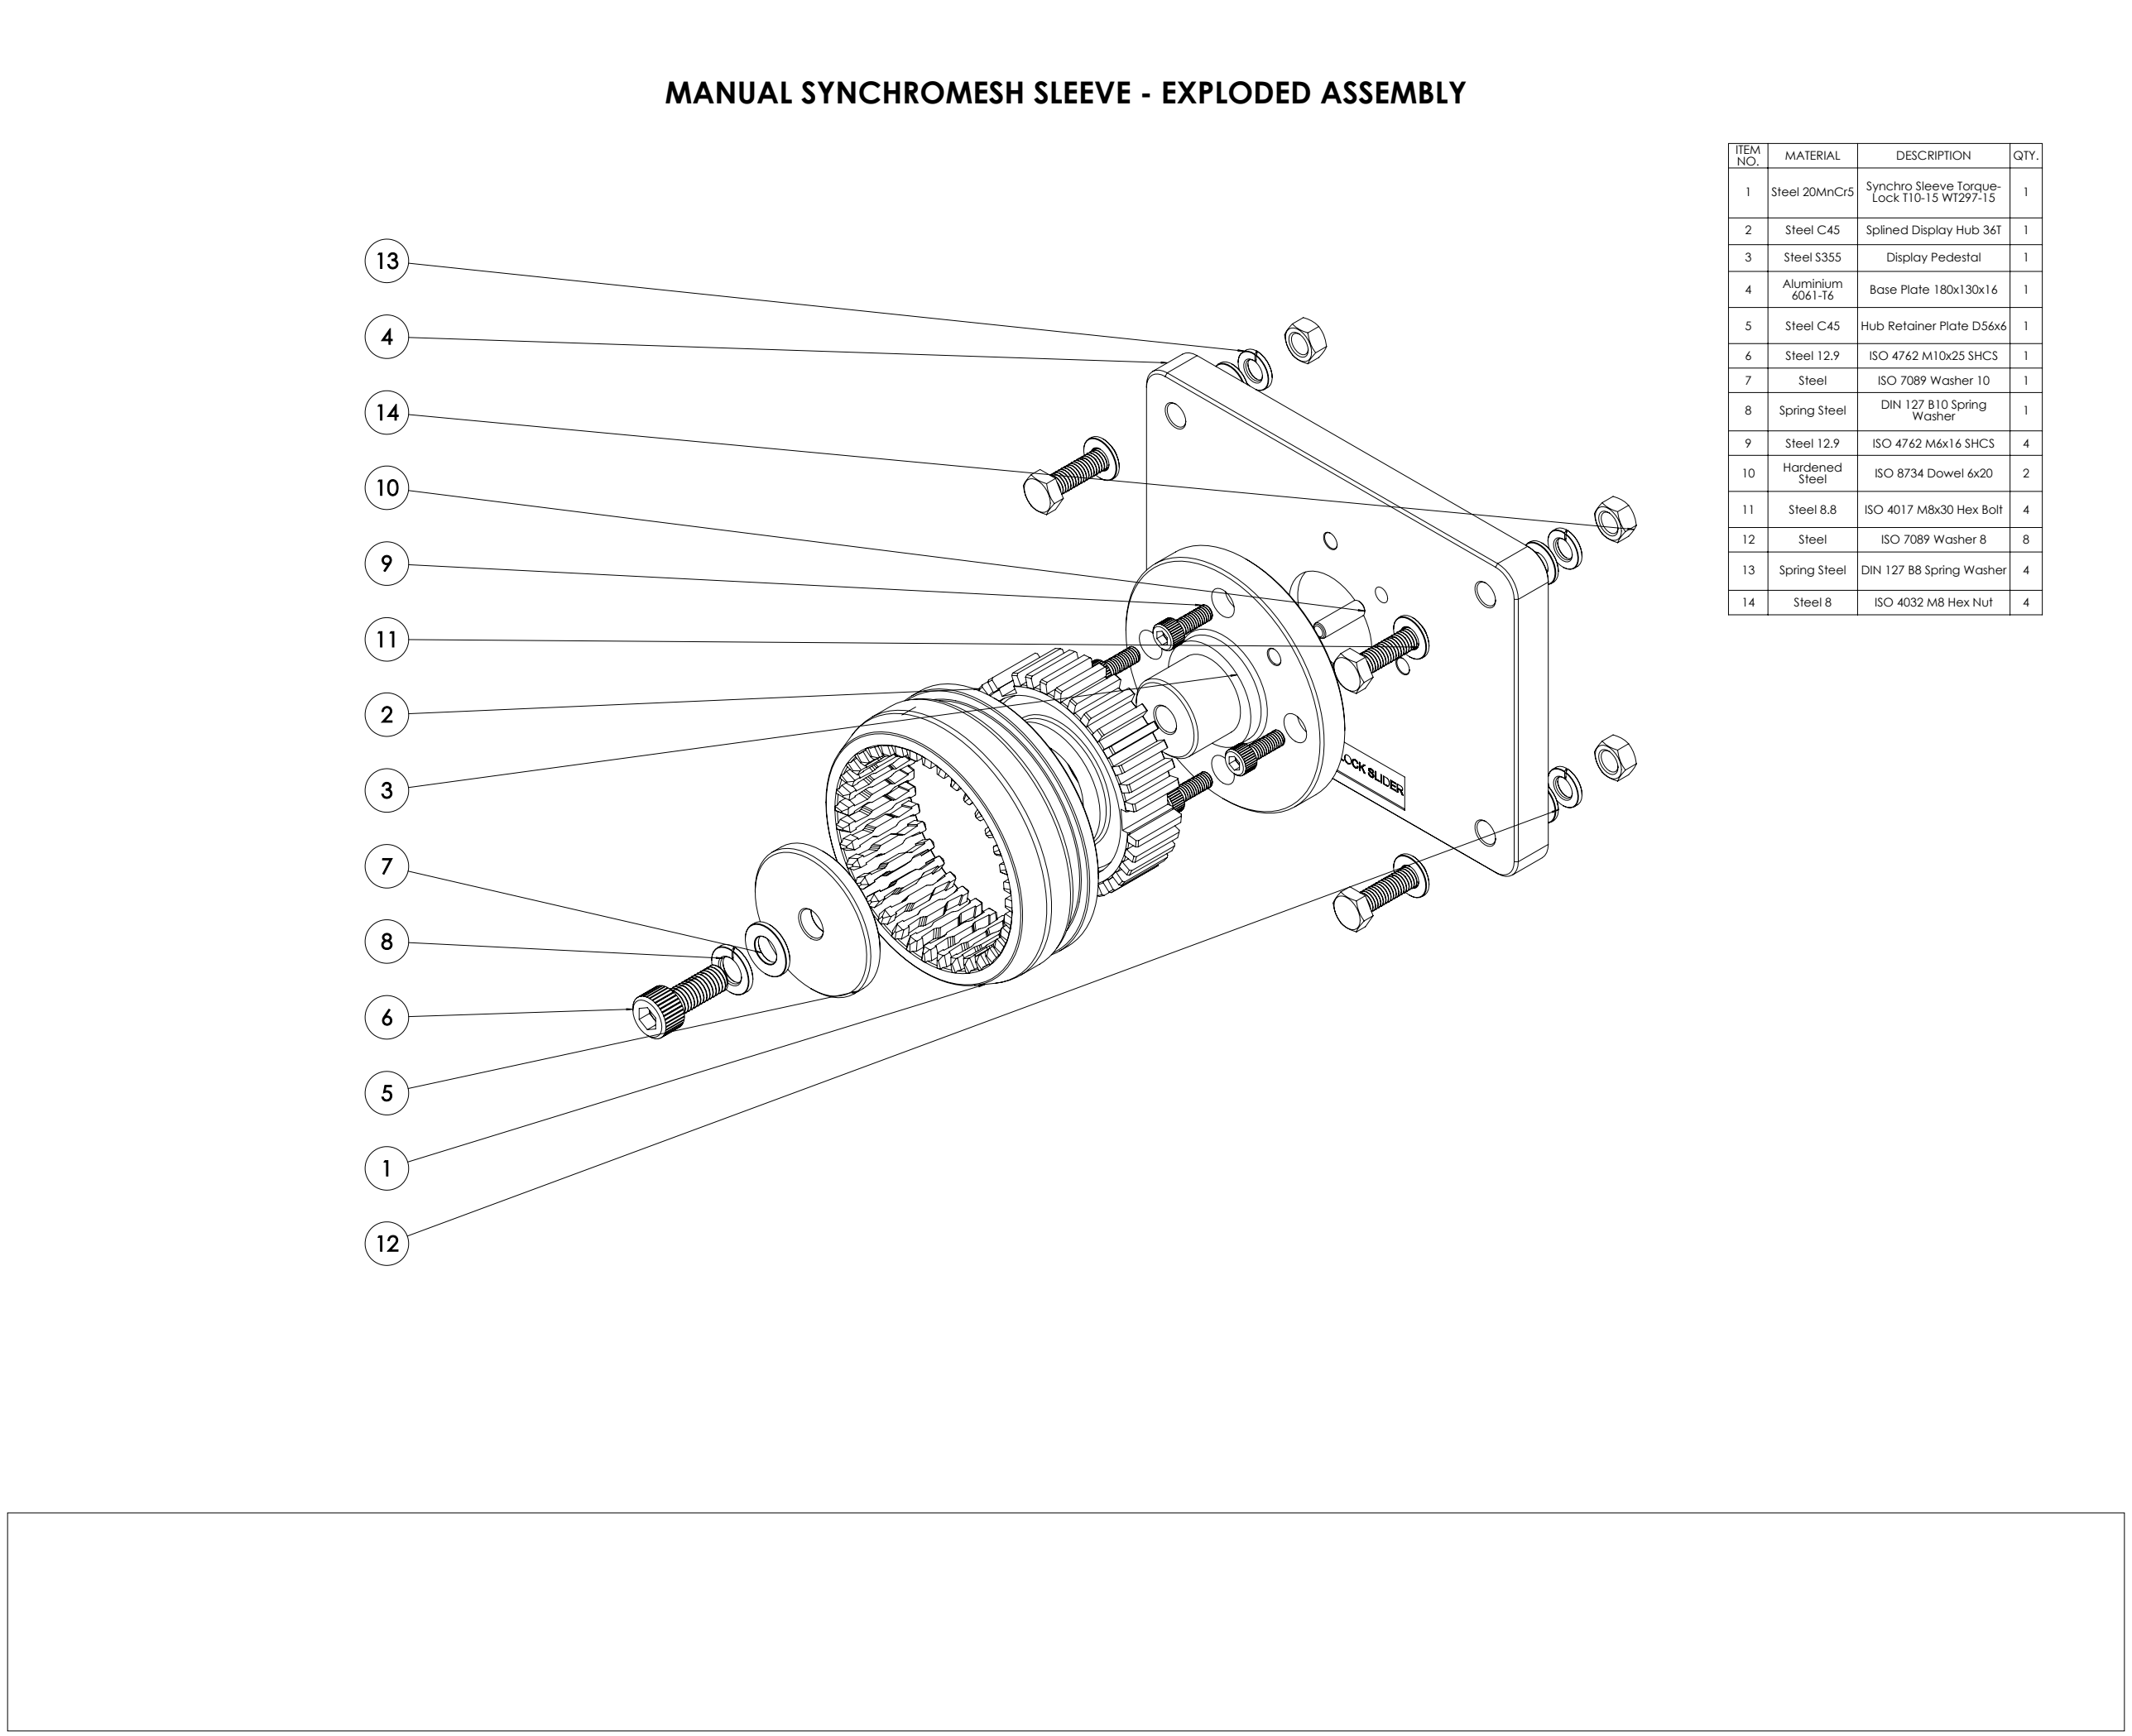
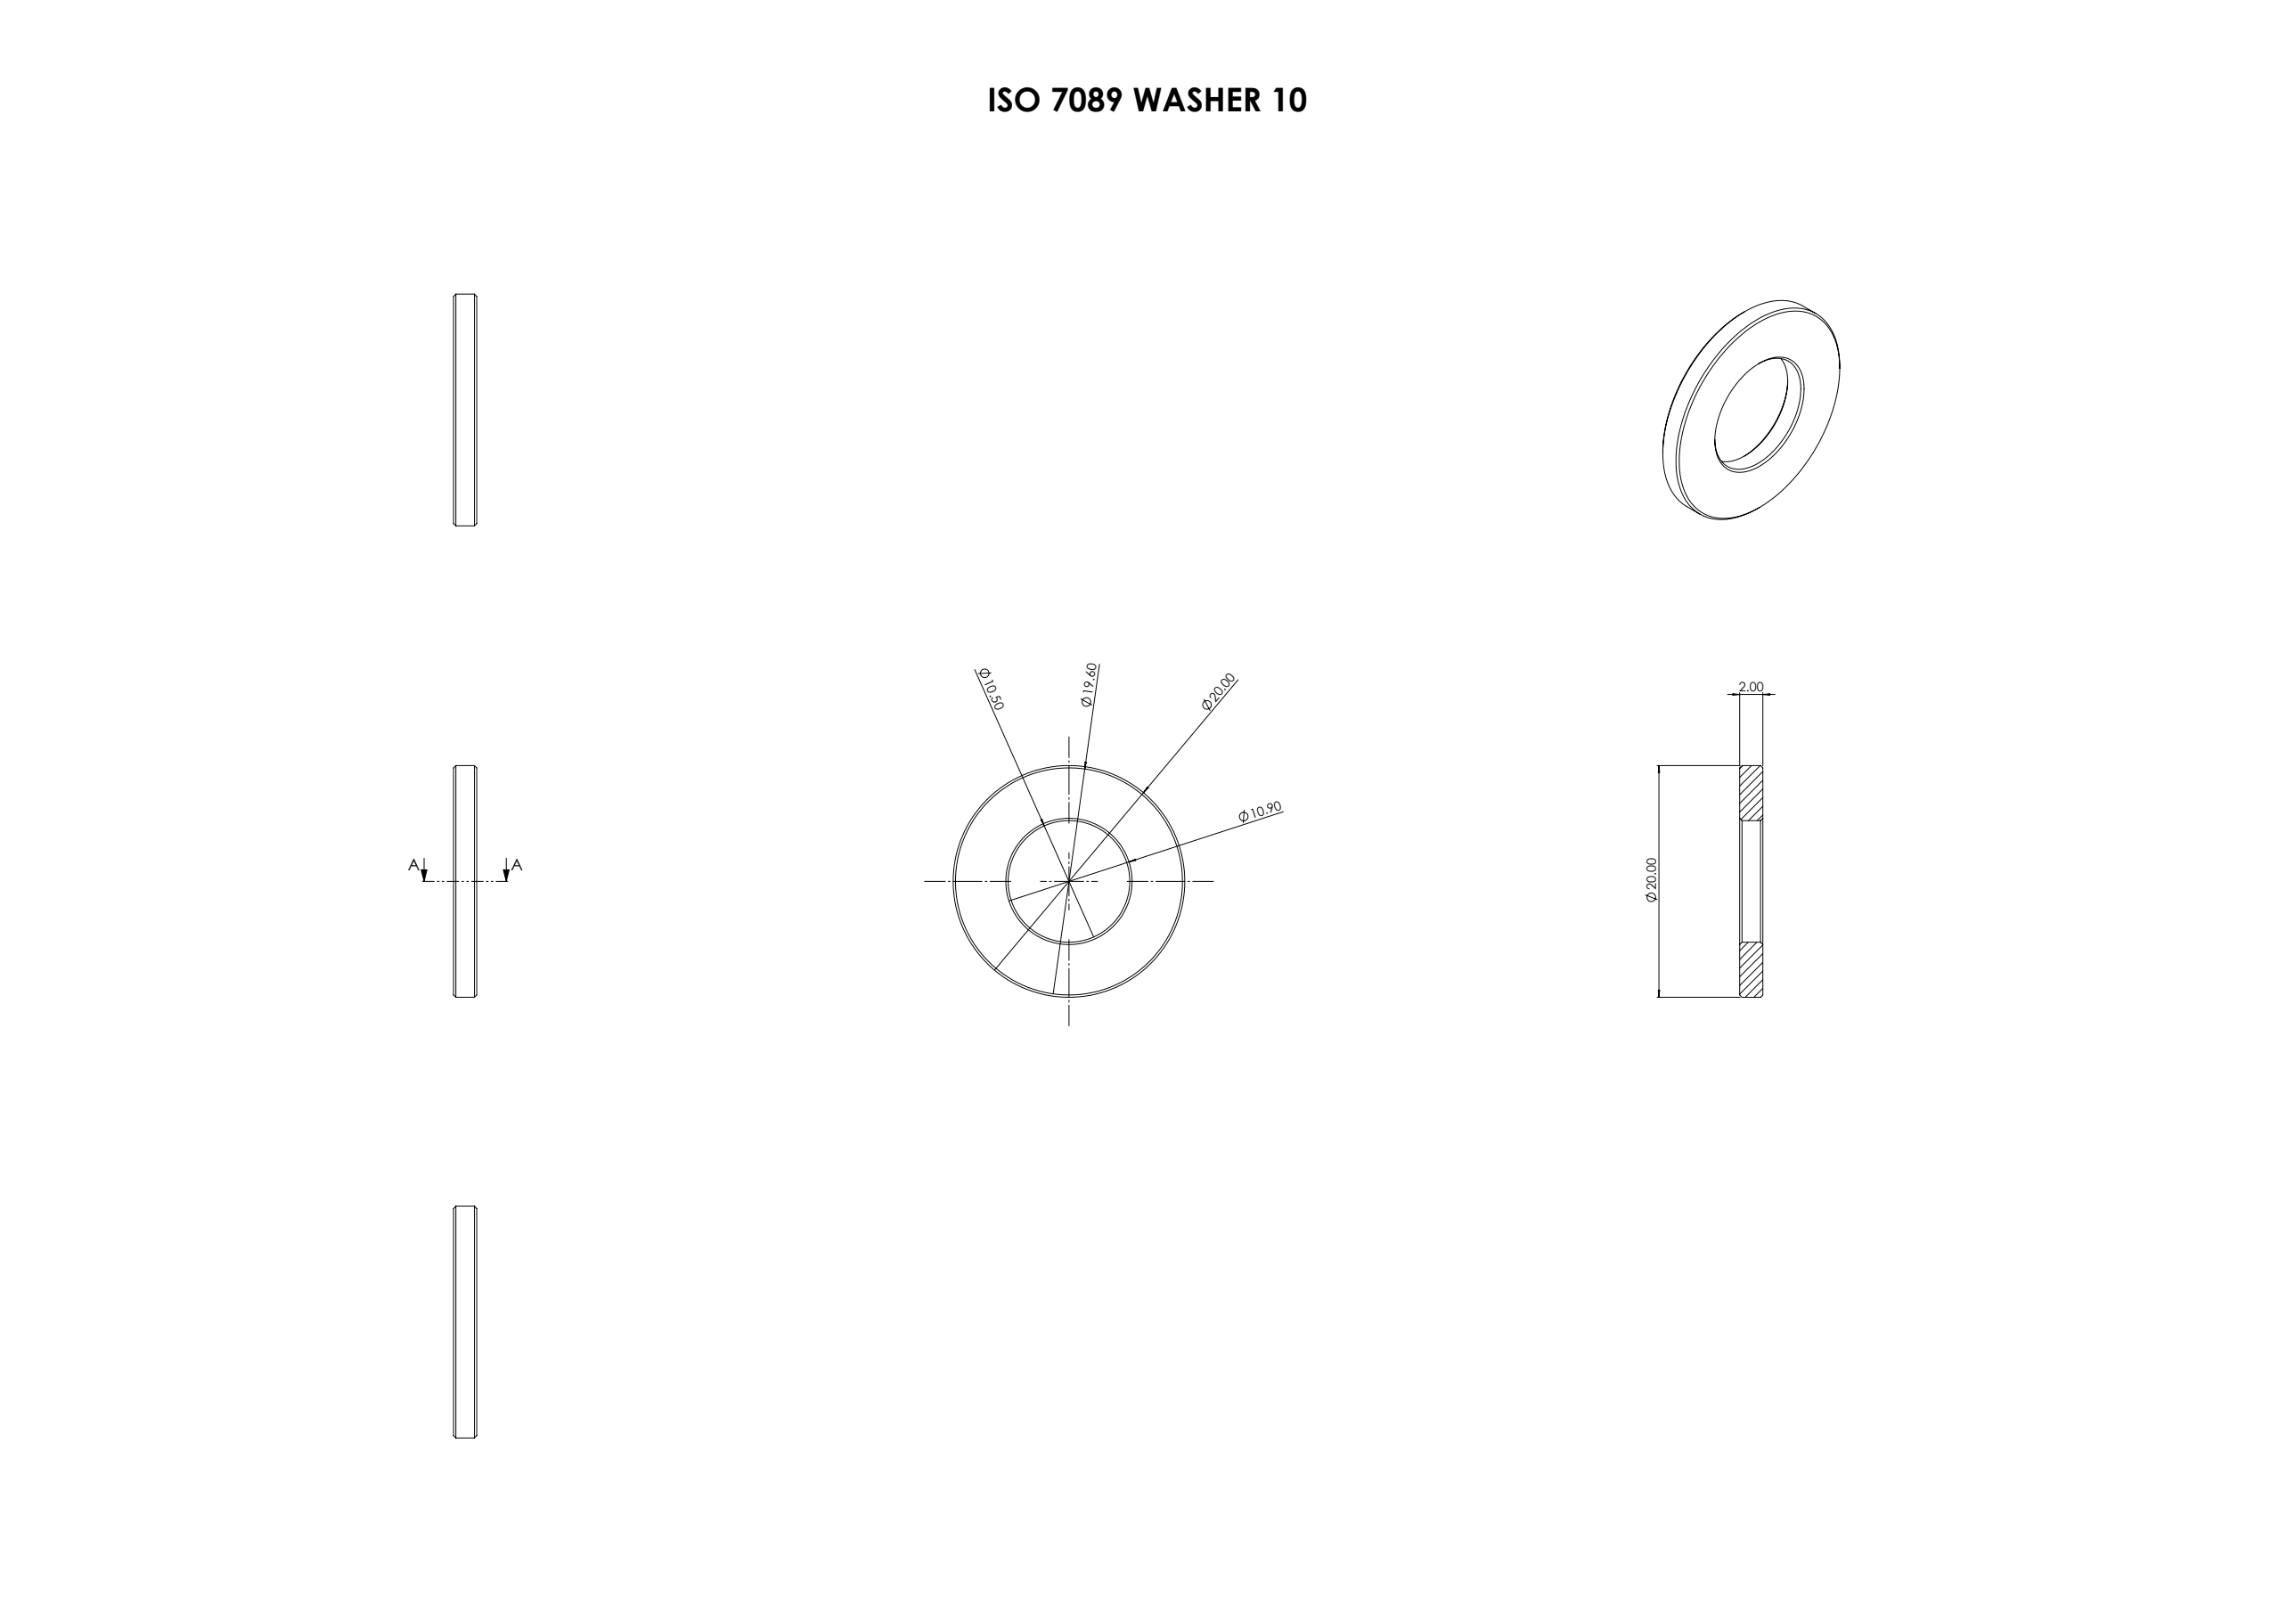
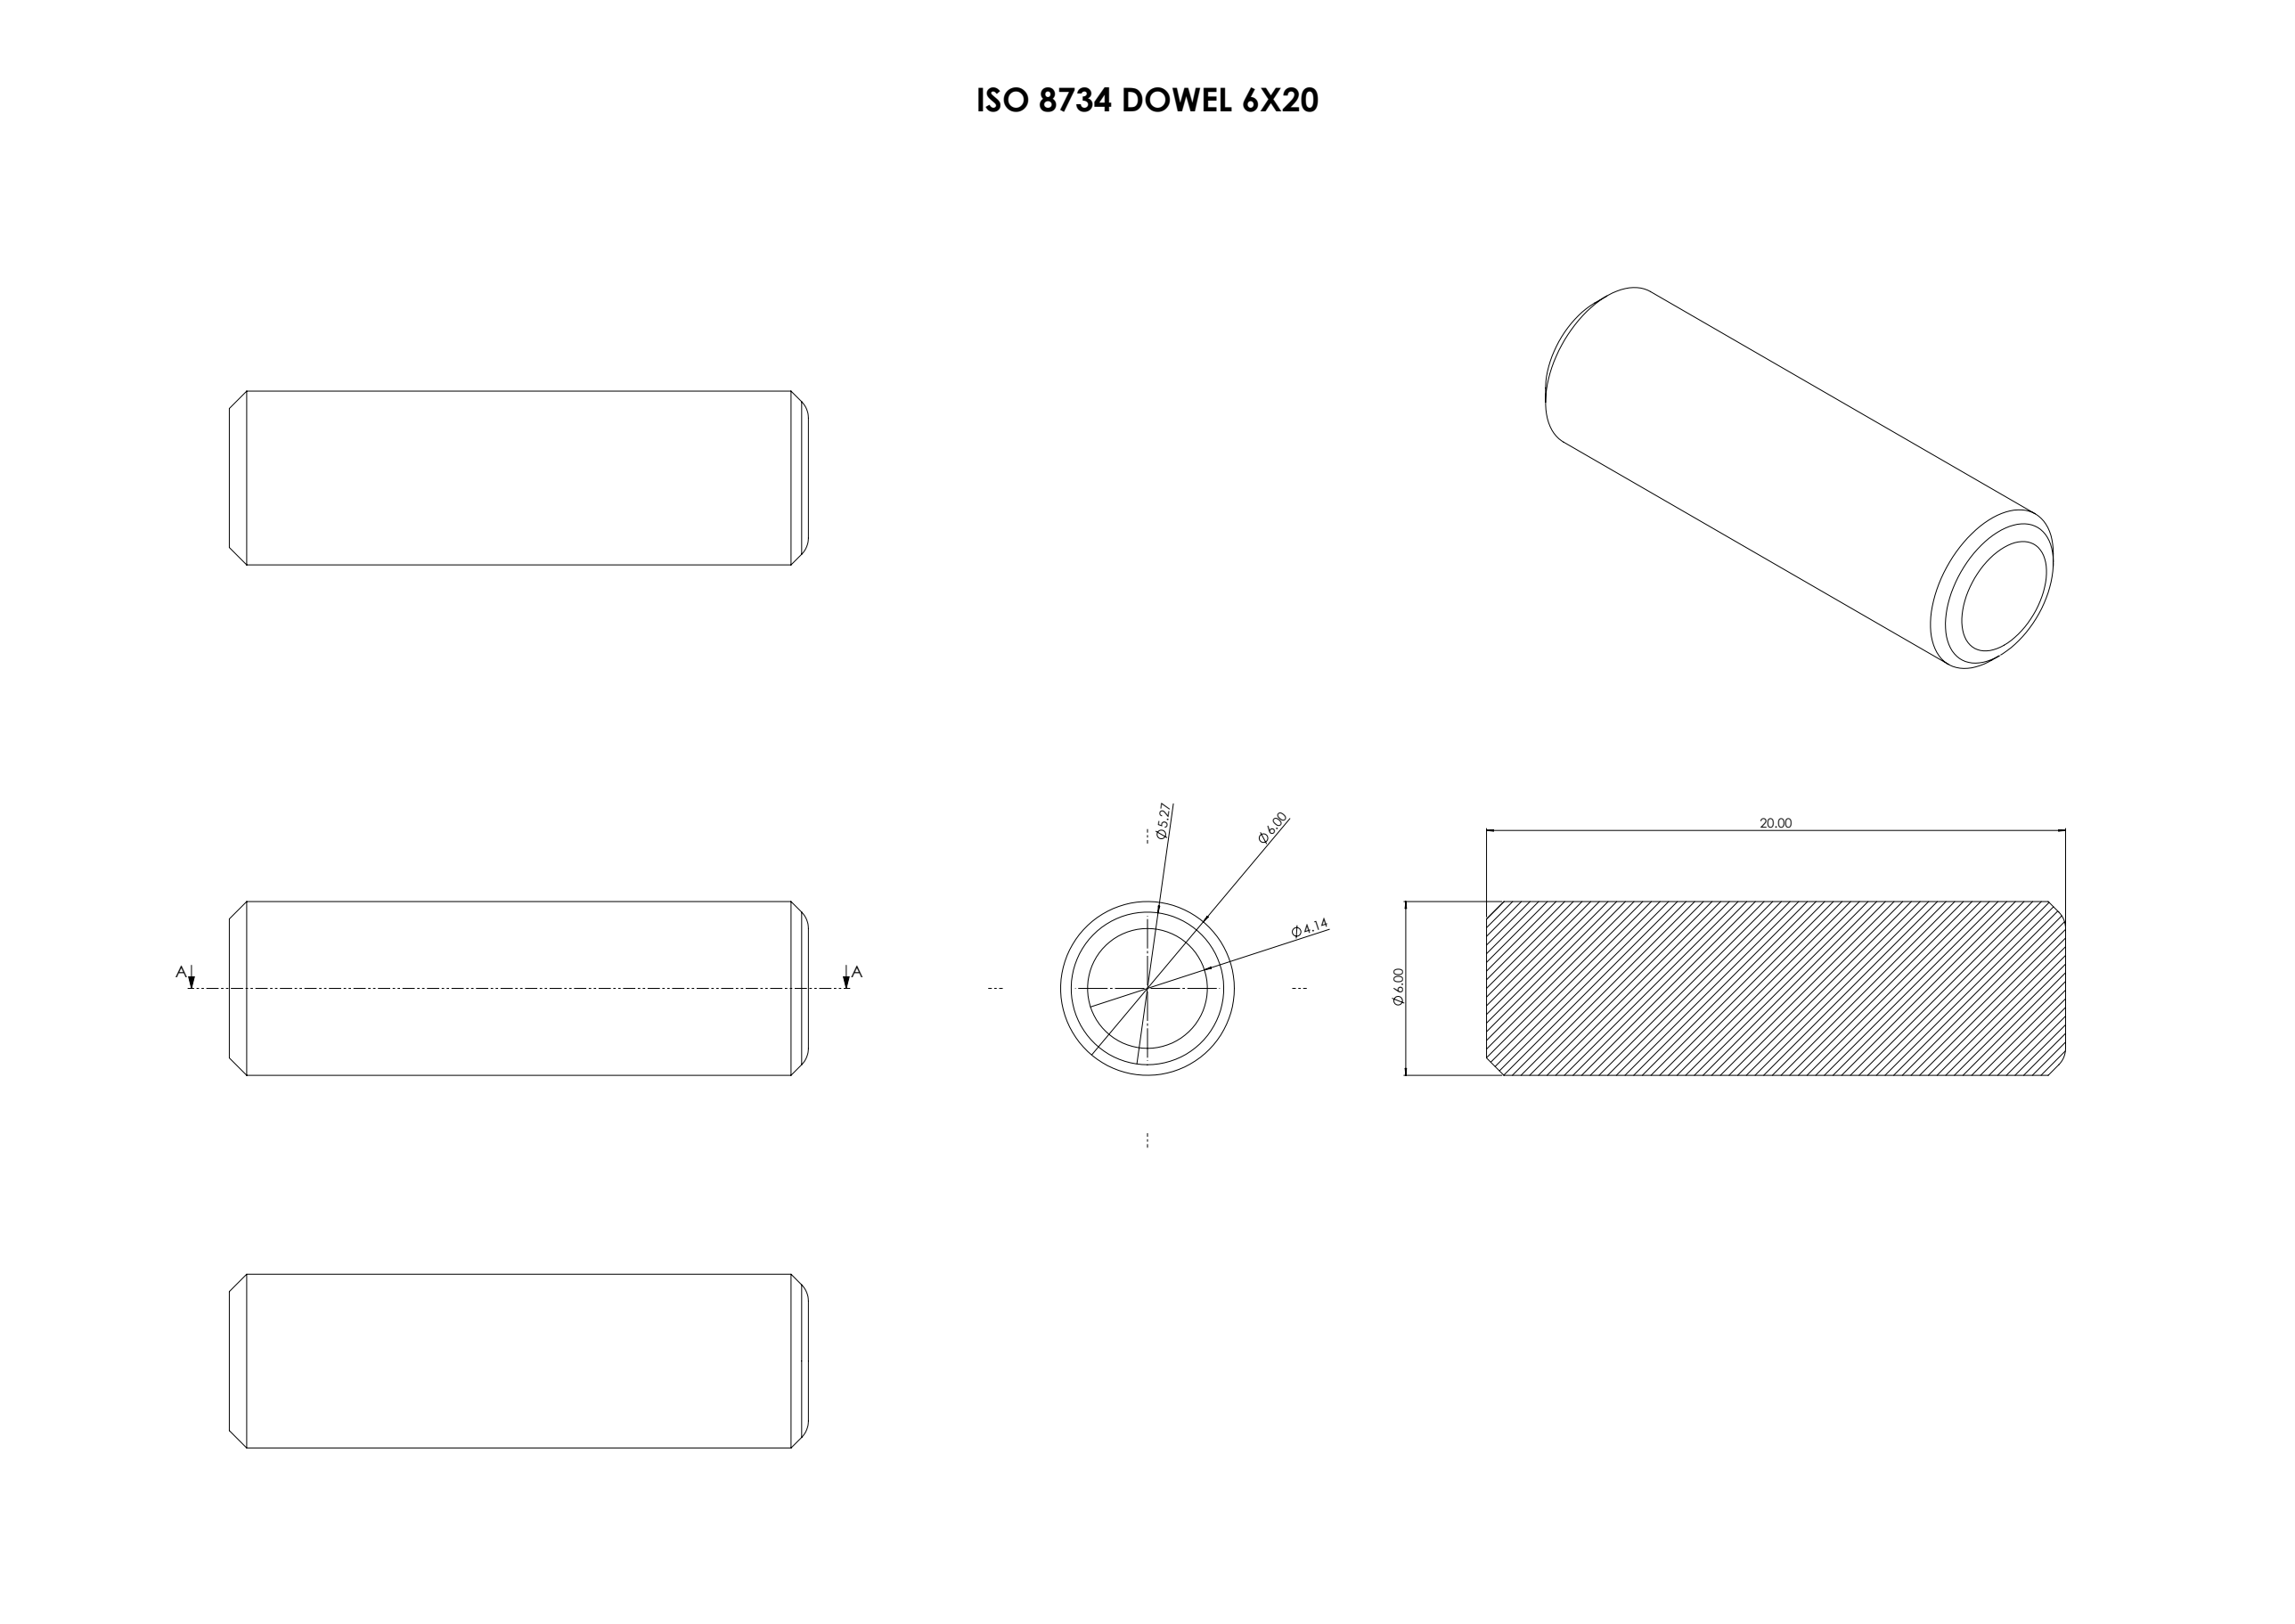
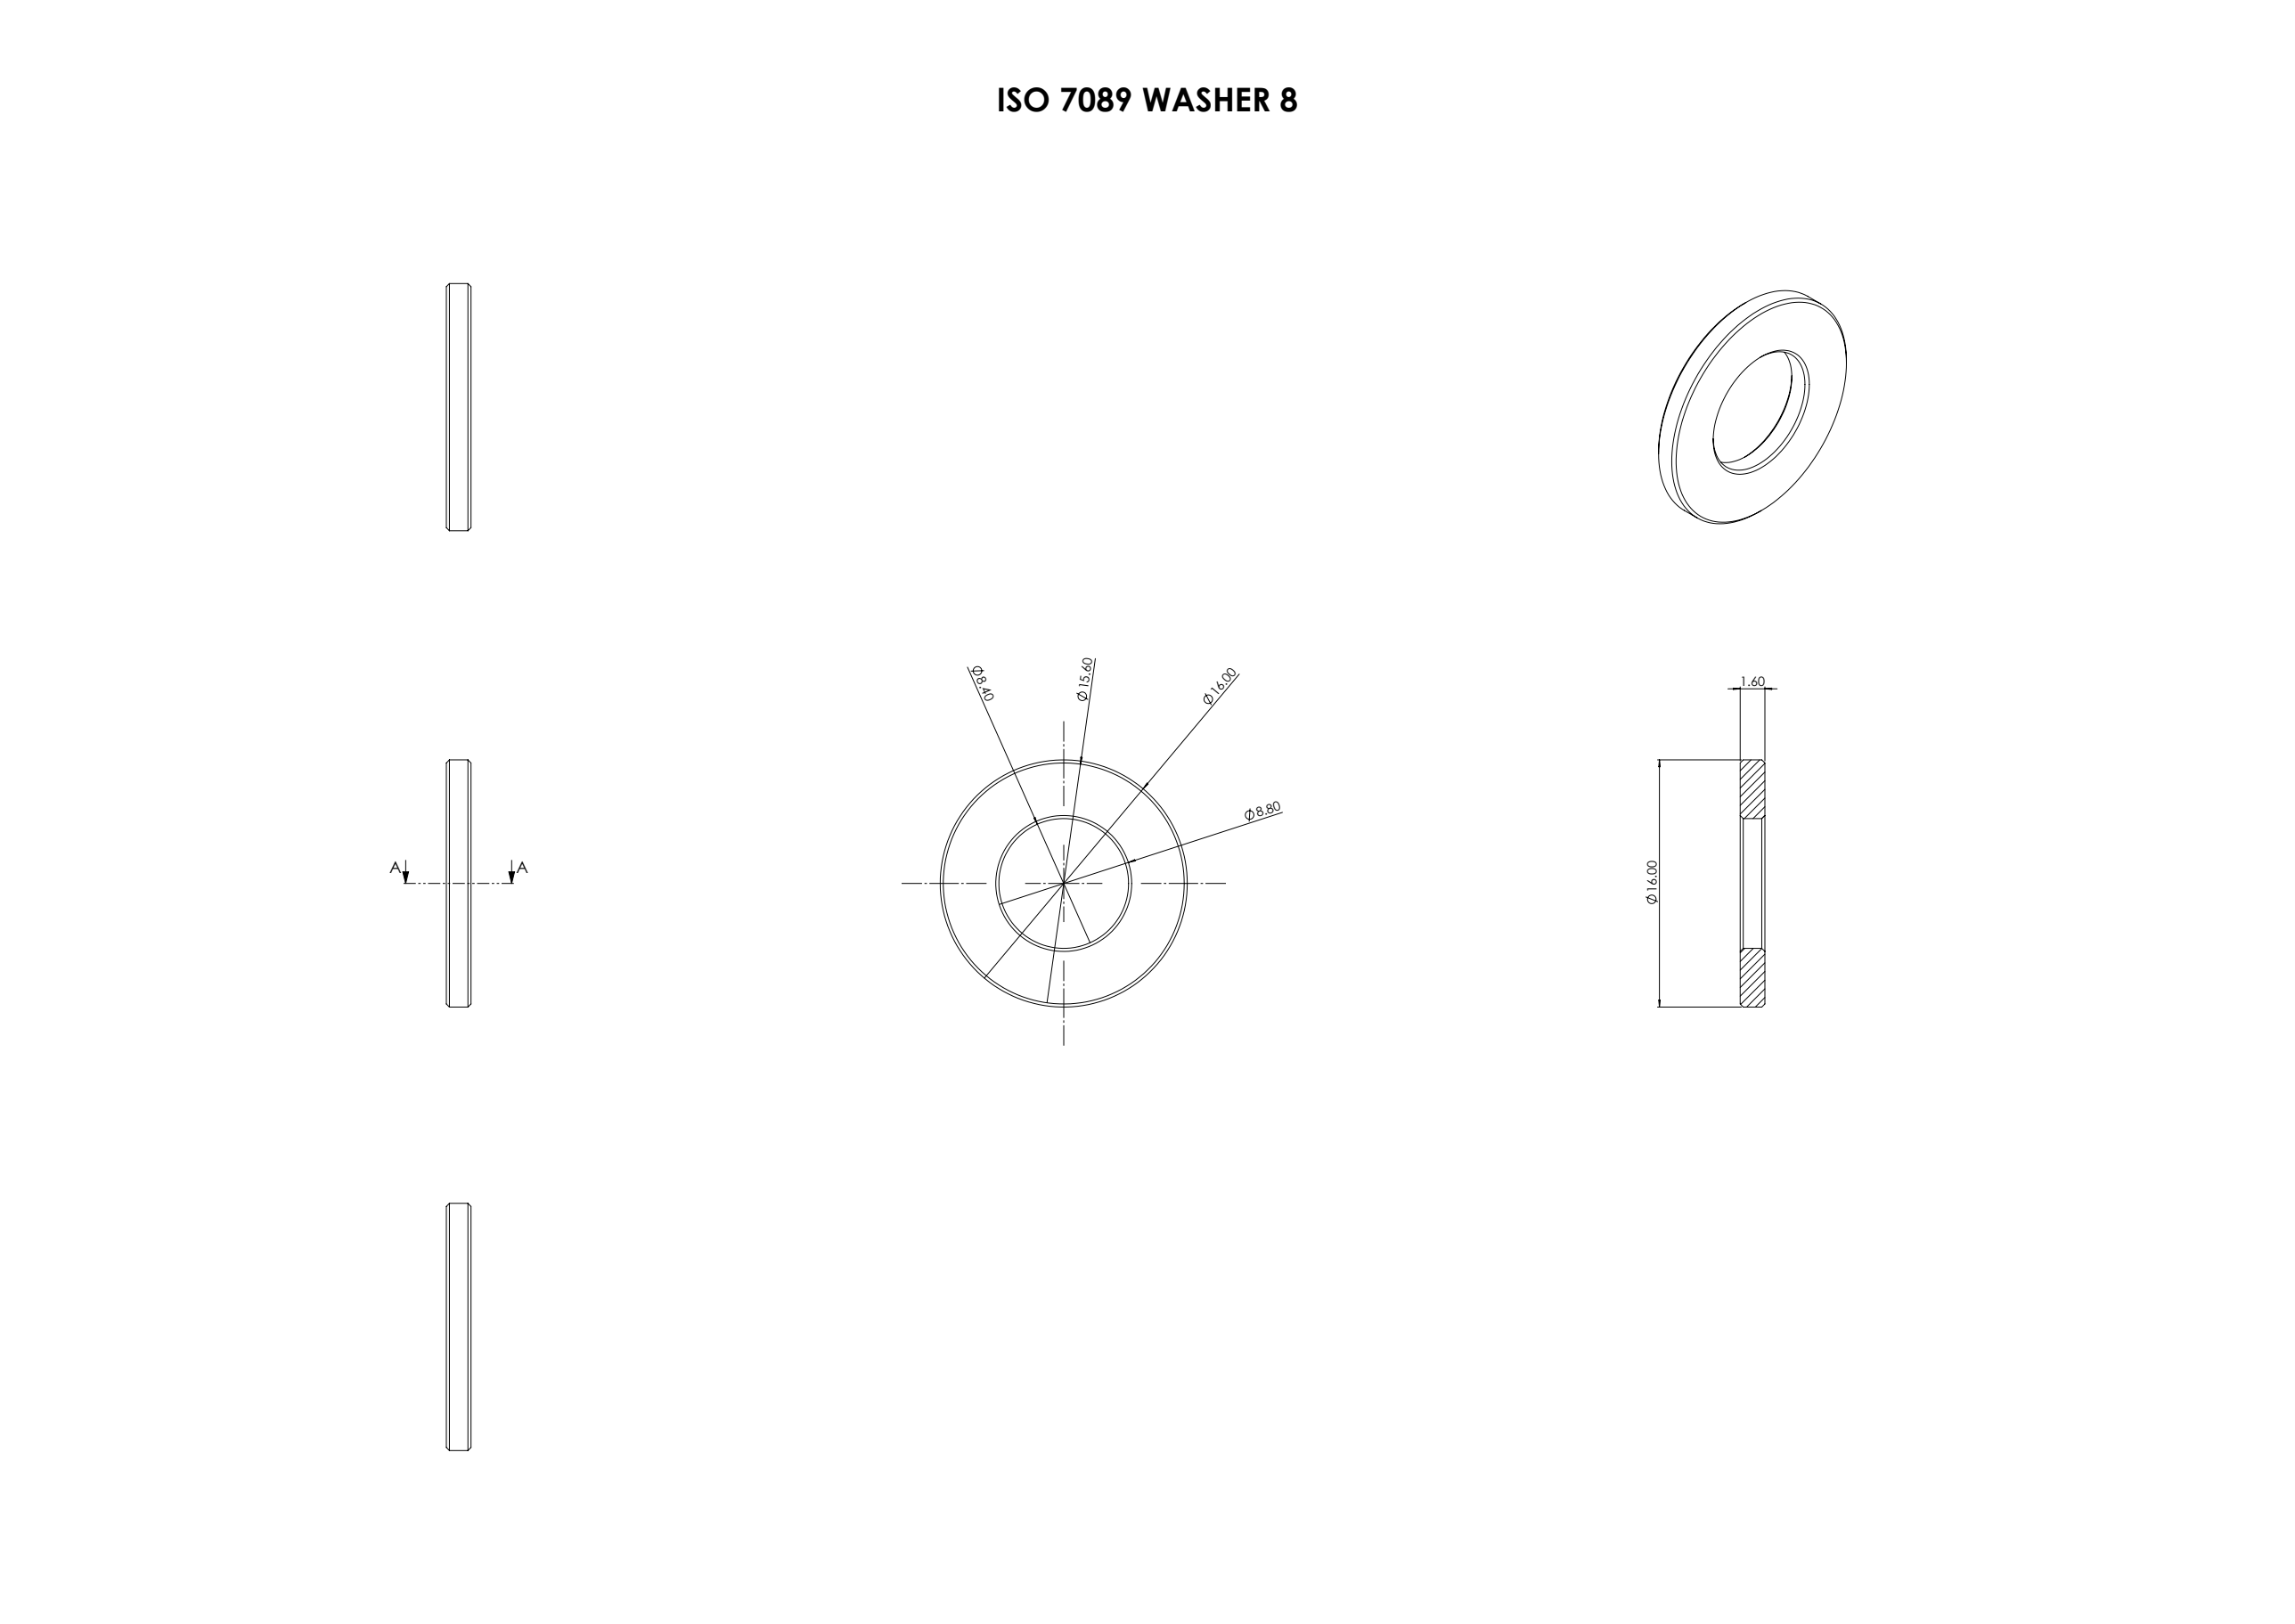
ISO-10303-21;
HEADER;
/* Generated by software containing ST-Developer
 * from STEP Tools, Inc. (www.steptools.com) 
 */

FILE_DESCRIPTION(
/* description */ (''),
/* implementation_level */ '2;1');

FILE_NAME(
/* name */ 'MAS-367',
/* time_stamp */ '2026-10-11T08:27:52-07:00',
/* author */ (''),
/* organization */ (''),
/* preprocessor_version */ 'ST-DEVELOPER v20.2',
/* originating_system */ 'Autodesk Translation Framework v15.15.0.0',
/* authorisation */ '');

FILE_SCHEMA (('AUTOMOTIVE_DESIGN { 1 0 10303 214 3 1 1 }'));
ENDSEC;

DATA;
#10=MECHANICAL_DESIGN_GEOMETRIC_PRESENTATION_REPRESENTATION('',(#919,#920,
#921,#922,#923,#924,#925,#926,#927,#928,#929,#930,#931,#932),#94301);
#11=ITEM_DEFINED_TRANSFORMATION($,$,#51188,#55334);
#12=ITEM_DEFINED_TRANSFORMATION($,$,#53608,#55335);
#13=ITEM_DEFINED_TRANSFORMATION($,$,#54142,#55336);
#14=ITEM_DEFINED_TRANSFORMATION($,$,#54216,#55337);
#15=ITEM_DEFINED_TRANSFORMATION($,$,#54474,#55338);
#16=ITEM_DEFINED_TRANSFORMATION($,$,#54491,#55339);
#17=ITEM_DEFINED_TRANSFORMATION($,$,#54812,#55340);
#18=ITEM_DEFINED_TRANSFORMATION($,$,#54829,#55341);
#19=ITEM_DEFINED_TRANSFORMATION($,$,#54858,#55342);
#20=ITEM_DEFINED_TRANSFORMATION($,$,#54858,#55343);
#21=ITEM_DEFINED_TRANSFORMATION($,$,#54858,#55344);
#22=ITEM_DEFINED_TRANSFORMATION($,$,#54858,#55345);
#23=ITEM_DEFINED_TRANSFORMATION($,$,#55178,#55346);
#24=ITEM_DEFINED_TRANSFORMATION($,$,#55178,#55347);
#25=ITEM_DEFINED_TRANSFORMATION($,$,#55192,#55348);
#26=ITEM_DEFINED_TRANSFORMATION($,$,#55192,#55349);
#27=ITEM_DEFINED_TRANSFORMATION($,$,#55192,#55350);
#28=ITEM_DEFINED_TRANSFORMATION($,$,#55192,#55351);
#29=ITEM_DEFINED_TRANSFORMATION($,$,#55271,#55352);
#30=ITEM_DEFINED_TRANSFORMATION($,$,#55271,#55353);
#31=ITEM_DEFINED_TRANSFORMATION($,$,#55271,#55354);
#32=ITEM_DEFINED_TRANSFORMATION($,$,#55271,#55355);
#33=ITEM_DEFINED_TRANSFORMATION($,$,#55271,#55356);
#34=ITEM_DEFINED_TRANSFORMATION($,$,#55271,#55357);
#35=ITEM_DEFINED_TRANSFORMATION($,$,#55271,#55358);
#36=ITEM_DEFINED_TRANSFORMATION($,$,#55271,#55359);
#37=ITEM_DEFINED_TRANSFORMATION($,$,#55288,#55360);
#38=ITEM_DEFINED_TRANSFORMATION($,$,#55288,#55361);
#39=ITEM_DEFINED_TRANSFORMATION($,$,#55288,#55362);
#40=ITEM_DEFINED_TRANSFORMATION($,$,#55288,#55363);
#41=ITEM_DEFINED_TRANSFORMATION($,$,#55314,#55364);
#42=ITEM_DEFINED_TRANSFORMATION($,$,#55314,#55365);
#43=ITEM_DEFINED_TRANSFORMATION($,$,#55314,#55366);
#44=ITEM_DEFINED_TRANSFORMATION($,$,#55314,#55367);
#45=(
REPRESENTATION_RELATIONSHIP($,$,#94371,#94370)
REPRESENTATION_RELATIONSHIP_WITH_TRANSFORMATION(#11)
SHAPE_REPRESENTATION_RELATIONSHIP()
);
#46=(
REPRESENTATION_RELATIONSHIP($,$,#94372,#94370)
REPRESENTATION_RELATIONSHIP_WITH_TRANSFORMATION(#12)
SHAPE_REPRESENTATION_RELATIONSHIP()
);
#47=(
REPRESENTATION_RELATIONSHIP($,$,#94373,#94370)
REPRESENTATION_RELATIONSHIP_WITH_TRANSFORMATION(#13)
SHAPE_REPRESENTATION_RELATIONSHIP()
);
#48=(
REPRESENTATION_RELATIONSHIP($,$,#94374,#94370)
REPRESENTATION_RELATIONSHIP_WITH_TRANSFORMATION(#14)
SHAPE_REPRESENTATION_RELATIONSHIP()
);
#49=(
REPRESENTATION_RELATIONSHIP($,$,#94375,#94370)
REPRESENTATION_RELATIONSHIP_WITH_TRANSFORMATION(#15)
SHAPE_REPRESENTATION_RELATIONSHIP()
);
#50=(
REPRESENTATION_RELATIONSHIP($,$,#94376,#94370)
REPRESENTATION_RELATIONSHIP_WITH_TRANSFORMATION(#16)
SHAPE_REPRESENTATION_RELATIONSHIP()
);
#51=(
REPRESENTATION_RELATIONSHIP($,$,#94377,#94370)
REPRESENTATION_RELATIONSHIP_WITH_TRANSFORMATION(#17)
SHAPE_REPRESENTATION_RELATIONSHIP()
);
#52=(
REPRESENTATION_RELATIONSHIP($,$,#94378,#94370)
REPRESENTATION_RELATIONSHIP_WITH_TRANSFORMATION(#18)
SHAPE_REPRESENTATION_RELATIONSHIP()
);
#53=(
REPRESENTATION_RELATIONSHIP($,$,#94379,#94370)
REPRESENTATION_RELATIONSHIP_WITH_TRANSFORMATION(#19)
SHAPE_REPRESENTATION_RELATIONSHIP()
);
#54=(
REPRESENTATION_RELATIONSHIP($,$,#94379,#94370)
REPRESENTATION_RELATIONSHIP_WITH_TRANSFORMATION(#20)
SHAPE_REPRESENTATION_RELATIONSHIP()
);
#55=(
REPRESENTATION_RELATIONSHIP($,$,#94379,#94370)
REPRESENTATION_RELATIONSHIP_WITH_TRANSFORMATION(#21)
SHAPE_REPRESENTATION_RELATIONSHIP()
);
#56=(
REPRESENTATION_RELATIONSHIP($,$,#94379,#94370)
REPRESENTATION_RELATIONSHIP_WITH_TRANSFORMATION(#22)
SHAPE_REPRESENTATION_RELATIONSHIP()
);
#57=(
REPRESENTATION_RELATIONSHIP($,$,#94380,#94370)
REPRESENTATION_RELATIONSHIP_WITH_TRANSFORMATION(#23)
SHAPE_REPRESENTATION_RELATIONSHIP()
);
#58=(
REPRESENTATION_RELATIONSHIP($,$,#94380,#94370)
REPRESENTATION_RELATIONSHIP_WITH_TRANSFORMATION(#24)
SHAPE_REPRESENTATION_RELATIONSHIP()
);
#59=(
REPRESENTATION_RELATIONSHIP($,$,#94381,#94370)
REPRESENTATION_RELATIONSHIP_WITH_TRANSFORMATION(#25)
SHAPE_REPRESENTATION_RELATIONSHIP()
);
#60=(
REPRESENTATION_RELATIONSHIP($,$,#94381,#94370)
REPRESENTATION_RELATIONSHIP_WITH_TRANSFORMATION(#26)
SHAPE_REPRESENTATION_RELATIONSHIP()
);
#61=(
REPRESENTATION_RELATIONSHIP($,$,#94381,#94370)
REPRESENTATION_RELATIONSHIP_WITH_TRANSFORMATION(#27)
SHAPE_REPRESENTATION_RELATIONSHIP()
);
#62=(
REPRESENTATION_RELATIONSHIP($,$,#94381,#94370)
REPRESENTATION_RELATIONSHIP_WITH_TRANSFORMATION(#28)
SHAPE_REPRESENTATION_RELATIONSHIP()
);
#63=(
REPRESENTATION_RELATIONSHIP($,$,#94382,#94370)
REPRESENTATION_RELATIONSHIP_WITH_TRANSFORMATION(#29)
SHAPE_REPRESENTATION_RELATIONSHIP()
);
#64=(
REPRESENTATION_RELATIONSHIP($,$,#94382,#94370)
REPRESENTATION_RELATIONSHIP_WITH_TRANSFORMATION(#30)
SHAPE_REPRESENTATION_RELATIONSHIP()
);
#65=(
REPRESENTATION_RELATIONSHIP($,$,#94382,#94370)
REPRESENTATION_RELATIONSHIP_WITH_TRANSFORMATION(#31)
SHAPE_REPRESENTATION_RELATIONSHIP()
);
#66=(
REPRESENTATION_RELATIONSHIP($,$,#94382,#94370)
REPRESENTATION_RELATIONSHIP_WITH_TRANSFORMATION(#32)
SHAPE_REPRESENTATION_RELATIONSHIP()
);
#67=(
REPRESENTATION_RELATIONSHIP($,$,#94382,#94370)
REPRESENTATION_RELATIONSHIP_WITH_TRANSFORMATION(#33)
SHAPE_REPRESENTATION_RELATIONSHIP()
);
#68=(
REPRESENTATION_RELATIONSHIP($,$,#94382,#94370)
REPRESENTATION_RELATIONSHIP_WITH_TRANSFORMATION(#34)
SHAPE_REPRESENTATION_RELATIONSHIP()
);
#69=(
REPRESENTATION_RELATIONSHIP($,$,#94382,#94370)
REPRESENTATION_RELATIONSHIP_WITH_TRANSFORMATION(#35)
SHAPE_REPRESENTATION_RELATIONSHIP()
);
#70=(
REPRESENTATION_RELATIONSHIP($,$,#94382,#94370)
REPRESENTATION_RELATIONSHIP_WITH_TRANSFORMATION(#36)
SHAPE_REPRESENTATION_RELATIONSHIP()
);
#71=(
REPRESENTATION_RELATIONSHIP($,$,#94383,#94370)
REPRESENTATION_RELATIONSHIP_WITH_TRANSFORMATION(#37)
SHAPE_REPRESENTATION_RELATIONSHIP()
);
#72=(
REPRESENTATION_RELATIONSHIP($,$,#94383,#94370)
REPRESENTATION_RELATIONSHIP_WITH_TRANSFORMATION(#38)
SHAPE_REPRESENTATION_RELATIONSHIP()
);
#73=(
REPRESENTATION_RELATIONSHIP($,$,#94383,#94370)
REPRESENTATION_RELATIONSHIP_WITH_TRANSFORMATION(#39)
SHAPE_REPRESENTATION_RELATIONSHIP()
);
#74=(
REPRESENTATION_RELATIONSHIP($,$,#94383,#94370)
REPRESENTATION_RELATIONSHIP_WITH_TRANSFORMATION(#40)
SHAPE_REPRESENTATION_RELATIONSHIP()
);
#75=(
REPRESENTATION_RELATIONSHIP($,$,#94384,#94370)
REPRESENTATION_RELATIONSHIP_WITH_TRANSFORMATION(#41)
SHAPE_REPRESENTATION_RELATIONSHIP()
);
#76=(
REPRESENTATION_RELATIONSHIP($,$,#94384,#94370)
REPRESENTATION_RELATIONSHIP_WITH_TRANSFORMATION(#42)
SHAPE_REPRESENTATION_RELATIONSHIP()
);
#77=(
REPRESENTATION_RELATIONSHIP($,$,#94384,#94370)
REPRESENTATION_RELATIONSHIP_WITH_TRANSFORMATION(#43)
SHAPE_REPRESENTATION_RELATIONSHIP()
);
#78=(
REPRESENTATION_RELATIONSHIP($,$,#94384,#94370)
REPRESENTATION_RELATIONSHIP_WITH_TRANSFORMATION(#44)
SHAPE_REPRESENTATION_RELATIONSHIP()
);
#79=CONTEXT_DEPENDENT_SHAPE_REPRESENTATION(#45,#94336);
#80=CONTEXT_DEPENDENT_SHAPE_REPRESENTATION(#46,#94337);
#81=CONTEXT_DEPENDENT_SHAPE_REPRESENTATION(#47,#94338);
#82=CONTEXT_DEPENDENT_SHAPE_REPRESENTATION(#48,#94339);
#83=CONTEXT_DEPENDENT_SHAPE_REPRESENTATION(#49,#94340);
#84=CONTEXT_DEPENDENT_SHAPE_REPRESENTATION(#50,#94341);
#85=CONTEXT_DEPENDENT_SHAPE_REPRESENTATION(#51,#94342);
#86=CONTEXT_DEPENDENT_SHAPE_REPRESENTATION(#52,#94343);
#87=CONTEXT_DEPENDENT_SHAPE_REPRESENTATION(#53,#94344);
#88=CONTEXT_DEPENDENT_SHAPE_REPRESENTATION(#54,#94345);
#89=CONTEXT_DEPENDENT_SHAPE_REPRESENTATION(#55,#94346);
#90=CONTEXT_DEPENDENT_SHAPE_REPRESENTATION(#56,#94347);
#91=CONTEXT_DEPENDENT_SHAPE_REPRESENTATION(#57,#94348);
#92=CONTEXT_DEPENDENT_SHAPE_REPRESENTATION(#58,#94349);
#93=CONTEXT_DEPENDENT_SHAPE_REPRESENTATION(#59,#94350);
#94=CONTEXT_DEPENDENT_SHAPE_REPRESENTATION(#60,#94351);
#95=CONTEXT_DEPENDENT_SHAPE_REPRESENTATION(#61,#94352);
#96=CONTEXT_DEPENDENT_SHAPE_REPRESENTATION(#62,#94353);
#97=CONTEXT_DEPENDENT_SHAPE_REPRESENTATION(#63,#94354);
#98=CONTEXT_DEPENDENT_SHAPE_REPRESENTATION(#64,#94355);
#99=CONTEXT_DEPENDENT_SHAPE_REPRESENTATION(#65,#94356);
#100=CONTEXT_DEPENDENT_SHAPE_REPRESENTATION(#66,#94357);
#101=CONTEXT_DEPENDENT_SHAPE_REPRESENTATION(#67,#94358);
#102=CONTEXT_DEPENDENT_SHAPE_REPRESENTATION(#68,#94359);
#103=CONTEXT_DEPENDENT_SHAPE_REPRESENTATION(#69,#94360);
#104=CONTEXT_DEPENDENT_SHAPE_REPRESENTATION(#70,#94361);
#105=CONTEXT_DEPENDENT_SHAPE_REPRESENTATION(#71,#94362);
#106=CONTEXT_DEPENDENT_SHAPE_REPRESENTATION(#72,#94363);
#107=CONTEXT_DEPENDENT_SHAPE_REPRESENTATION(#73,#94364);
#108=CONTEXT_DEPENDENT_SHAPE_REPRESENTATION(#74,#94365);
#109=CONTEXT_DEPENDENT_SHAPE_REPRESENTATION(#75,#94366);
#110=CONTEXT_DEPENDENT_SHAPE_REPRESENTATION(#76,#94367);
#111=CONTEXT_DEPENDENT_SHAPE_REPRESENTATION(#77,#94368);
#112=CONTEXT_DEPENDENT_SHAPE_REPRESENTATION(#78,#94369);
#113=NEXT_ASSEMBLY_USAGE_OCCURRENCE(
'01_Synchro_Sleeve_Torque-Lock_T10-15_WT297-15:2',
'01_Synchro_Sleeve_Torque-Lock_T10-15_WT297-15:2',
'01_Synchro_Sleeve_Torque-Lock_T10-15_WT297-15:2',#94386,#94387,
'01_Synchro_Sleeve_Torque-Lock_T10-15_WT297-15:2');
#114=NEXT_ASSEMBLY_USAGE_OCCURRENCE('02_Splined_Display_Hub_36T:2',
'02_Splined_Display_Hub_36T:2','02_Splined_Display_Hub_36T:2',#94386,#94388,
'02_Splined_Display_Hub_36T:2');
#115=NEXT_ASSEMBLY_USAGE_OCCURRENCE('03_Display_Pedestal:2',
'03_Display_Pedestal:2','03_Display_Pedestal:2',#94386,#94389,
'03_Display_Pedestal:2');
#116=NEXT_ASSEMBLY_USAGE_OCCURRENCE('04_Base_Plate_180x130x16:2',
'04_Base_Plate_180x130x16:2','04_Base_Plate_180x130x16:2',#94386,#94390,
'04_Base_Plate_180x130x16:2');
#117=NEXT_ASSEMBLY_USAGE_OCCURRENCE('05_Hub_Retainer_Plate_D56x6:2',
'05_Hub_Retainer_Plate_D56x6:2','05_Hub_Retainer_Plate_D56x6:2',#94386,
#94391,'05_Hub_Retainer_Plate_D56x6:2');
#118=NEXT_ASSEMBLY_USAGE_OCCURRENCE('06_ISO_4762_M10x25_SHCS:2',
'06_ISO_4762_M10x25_SHCS:2','06_ISO_4762_M10x25_SHCS:2',#94386,#94392,
'06_ISO_4762_M10x25_SHCS:2');
#119=NEXT_ASSEMBLY_USAGE_OCCURRENCE('07_ISO_7089_Washer_10:2',
'07_ISO_7089_Washer_10:2','07_ISO_7089_Washer_10:2',#94386,#94393,
'07_ISO_7089_Washer_10:2');
#120=NEXT_ASSEMBLY_USAGE_OCCURRENCE('08_DIN_127_B10_Spring_Washer:2',
'08_DIN_127_B10_Spring_Washer:2','08_DIN_127_B10_Spring_Washer:2',#94386,
#94394,'08_DIN_127_B10_Spring_Washer:2');
#121=NEXT_ASSEMBLY_USAGE_OCCURRENCE('09_ISO_4762_M6x16_SHCS:2',
'09_ISO_4762_M6x16_SHCS:2','09_ISO_4762_M6x16_SHCS:2',#94386,#94395,
'09_ISO_4762_M6x16_SHCS:2');
#122=NEXT_ASSEMBLY_USAGE_OCCURRENCE('09_ISO_4762_M6x16_SHCS:3',
'09_ISO_4762_M6x16_SHCS:3','09_ISO_4762_M6x16_SHCS:3',#94386,#94395,
'09_ISO_4762_M6x16_SHCS:3');
#123=NEXT_ASSEMBLY_USAGE_OCCURRENCE('09_ISO_4762_M6x16_SHCS:4',
'09_ISO_4762_M6x16_SHCS:4','09_ISO_4762_M6x16_SHCS:4',#94386,#94395,
'09_ISO_4762_M6x16_SHCS:4');
#124=NEXT_ASSEMBLY_USAGE_OCCURRENCE('09_ISO_4762_M6x16_SHCS:5',
'09_ISO_4762_M6x16_SHCS:5','09_ISO_4762_M6x16_SHCS:5',#94386,#94395,
'09_ISO_4762_M6x16_SHCS:5');
#125=NEXT_ASSEMBLY_USAGE_OCCURRENCE('10_ISO_8734_Dowel_6x20:2',
'10_ISO_8734_Dowel_6x20:2','10_ISO_8734_Dowel_6x20:2',#94386,#94396,
'10_ISO_8734_Dowel_6x20:2');
#126=NEXT_ASSEMBLY_USAGE_OCCURRENCE('10_ISO_8734_Dowel_6x20:3',
'10_ISO_8734_Dowel_6x20:3','10_ISO_8734_Dowel_6x20:3',#94386,#94396,
'10_ISO_8734_Dowel_6x20:3');
#127=NEXT_ASSEMBLY_USAGE_OCCURRENCE('11_ISO_4017_M8x30_Hex_Bolt:2',
'11_ISO_4017_M8x30_Hex_Bolt:2','11_ISO_4017_M8x30_Hex_Bolt:2',#94386,#94397,
'11_ISO_4017_M8x30_Hex_Bolt:2');
#128=NEXT_ASSEMBLY_USAGE_OCCURRENCE('11_ISO_4017_M8x30_Hex_Bolt:3',
'11_ISO_4017_M8x30_Hex_Bolt:3','11_ISO_4017_M8x30_Hex_Bolt:3',#94386,#94397,
'11_ISO_4017_M8x30_Hex_Bolt:3');
#129=NEXT_ASSEMBLY_USAGE_OCCURRENCE('11_ISO_4017_M8x30_Hex_Bolt:4',
'11_ISO_4017_M8x30_Hex_Bolt:4','11_ISO_4017_M8x30_Hex_Bolt:4',#94386,#94397,
'11_ISO_4017_M8x30_Hex_Bolt:4');
#130=NEXT_ASSEMBLY_USAGE_OCCURRENCE('11_ISO_4017_M8x30_Hex_Bolt:5',
'11_ISO_4017_M8x30_Hex_Bolt:5','11_ISO_4017_M8x30_Hex_Bolt:5',#94386,#94397,
'11_ISO_4017_M8x30_Hex_Bolt:5');
#131=NEXT_ASSEMBLY_USAGE_OCCURRENCE('12_ISO_7089_Washer_8:2',
'12_ISO_7089_Washer_8:2','12_ISO_7089_Washer_8:2',#94386,#94398,
'12_ISO_7089_Washer_8:2');
#132=NEXT_ASSEMBLY_USAGE_OCCURRENCE('12_ISO_7089_Washer_8:3',
'12_ISO_7089_Washer_8:3','12_ISO_7089_Washer_8:3',#94386,#94398,
'12_ISO_7089_Washer_8:3');
#133=NEXT_ASSEMBLY_USAGE_OCCURRENCE('12_ISO_7089_Washer_8:4',
'12_ISO_7089_Washer_8:4','12_ISO_7089_Washer_8:4',#94386,#94398,
'12_ISO_7089_Washer_8:4');
#134=NEXT_ASSEMBLY_USAGE_OCCURRENCE('12_ISO_7089_Washer_8:5',
'12_ISO_7089_Washer_8:5','12_ISO_7089_Washer_8:5',#94386,#94398,
'12_ISO_7089_Washer_8:5');
#135=NEXT_ASSEMBLY_USAGE_OCCURRENCE('12_ISO_7089_Washer_8:6',
'12_ISO_7089_Washer_8:6','12_ISO_7089_Washer_8:6',#94386,#94398,
'12_ISO_7089_Washer_8:6');
#136=NEXT_ASSEMBLY_USAGE_OCCURRENCE('12_ISO_7089_Washer_8:7',
'12_ISO_7089_Washer_8:7','12_ISO_7089_Washer_8:7',#94386,#94398,
'12_ISO_7089_Washer_8:7');
#137=NEXT_ASSEMBLY_USAGE_OCCURRENCE('12_ISO_7089_Washer_8:8',
'12_ISO_7089_Washer_8:8','12_ISO_7089_Washer_8:8',#94386,#94398,
'12_ISO_7089_Washer_8:8');
#138=NEXT_ASSEMBLY_USAGE_OCCURRENCE('12_ISO_7089_Washer_8:9',
'12_ISO_7089_Washer_8:9','12_ISO_7089_Washer_8:9',#94386,#94398,
'12_ISO_7089_Washer_8:9');
#139=NEXT_ASSEMBLY_USAGE_OCCURRENCE('13_DIN_127_B8_Spring_Washer:2',
'13_DIN_127_B8_Spring_Washer:2','13_DIN_127_B8_Spring_Washer:2',#94386,
#94399,'13_DIN_127_B8_Spring_Washer:2');
#140=NEXT_ASSEMBLY_USAGE_OCCURRENCE('13_DIN_127_B8_Spring_Washer:3',
'13_DIN_127_B8_Spring_Washer:3','13_DIN_127_B8_Spring_Washer:3',#94386,
#94399,'13_DIN_127_B8_Spring_Washer:3');
#141=NEXT_ASSEMBLY_USAGE_OCCURRENCE('13_DIN_127_B8_Spring_Washer:4',
'13_DIN_127_B8_Spring_Washer:4','13_DIN_127_B8_Spring_Washer:4',#94386,
#94399,'13_DIN_127_B8_Spring_Washer:4');
#142=NEXT_ASSEMBLY_USAGE_OCCURRENCE('13_DIN_127_B8_Spring_Washer:5',
'13_DIN_127_B8_Spring_Washer:5','13_DIN_127_B8_Spring_Washer:5',#94386,
#94399,'13_DIN_127_B8_Spring_Washer:5');
#143=NEXT_ASSEMBLY_USAGE_OCCURRENCE('14_ISO_4032_M8_Hex_Nut:2',
'14_ISO_4032_M8_Hex_Nut:2','14_ISO_4032_M8_Hex_Nut:2',#94386,#94400,
'14_ISO_4032_M8_Hex_Nut:2');
#144=NEXT_ASSEMBLY_USAGE_OCCURRENCE('14_ISO_4032_M8_Hex_Nut:3',
'14_ISO_4032_M8_Hex_Nut:3','14_ISO_4032_M8_Hex_Nut:3',#94386,#94400,
'14_ISO_4032_M8_Hex_Nut:3');
#145=NEXT_ASSEMBLY_USAGE_OCCURRENCE('14_ISO_4032_M8_Hex_Nut:4',
'14_ISO_4032_M8_Hex_Nut:4','14_ISO_4032_M8_Hex_Nut:4',#94386,#94400,
'14_ISO_4032_M8_Hex_Nut:4');
#146=NEXT_ASSEMBLY_USAGE_OCCURRENCE('14_ISO_4032_M8_Hex_Nut:5',
'14_ISO_4032_M8_Hex_Nut:5','14_ISO_4032_M8_Hex_Nut:5',#94386,#94400,
'14_ISO_4032_M8_Hex_Nut:5');
#147=B_SPLINE_CURVE_WITH_KNOTS('',2,(#80633,#80634,#80635),
 .UNSPECIFIED.,.F.,.F.,(3,3),(0.,1.),.UNSPECIFIED.);
#148=B_SPLINE_CURVE_WITH_KNOTS('',2,(#80639,#80640,#80641),
 .UNSPECIFIED.,.F.,.F.,(3,3),(0.,1.),.UNSPECIFIED.);
#149=B_SPLINE_CURVE_WITH_KNOTS('',2,(#80650,#80651,#80652),
 .UNSPECIFIED.,.F.,.F.,(3,3),(0.,1.),.UNSPECIFIED.);
#150=B_SPLINE_CURVE_WITH_KNOTS('',2,(#80655,#80656,#80657),
 .UNSPECIFIED.,.F.,.F.,(3,3),(0.,1.),.UNSPECIFIED.);
#151=B_SPLINE_CURVE_WITH_KNOTS('',2,(#80665,#80666,#80667),
 .UNSPECIFIED.,.F.,.F.,(3,3),(0.,1.),.UNSPECIFIED.);
#152=B_SPLINE_CURVE_WITH_KNOTS('',2,(#80670,#80671,#80672),
 .UNSPECIFIED.,.F.,.F.,(3,3),(0.,1.),.UNSPECIFIED.);
#153=B_SPLINE_CURVE_WITH_KNOTS('',2,(#80680,#80681,#80682),
 .UNSPECIFIED.,.F.,.F.,(3,3),(0.,1.),.UNSPECIFIED.);
#154=B_SPLINE_CURVE_WITH_KNOTS('',2,(#80685,#80686,#80687),
 .UNSPECIFIED.,.F.,.F.,(3,3),(0.,1.),.UNSPECIFIED.);
#155=B_SPLINE_CURVE_WITH_KNOTS('',2,(#80695,#80696,#80697),
 .UNSPECIFIED.,.F.,.F.,(3,3),(0.,1.),.UNSPECIFIED.);
#156=B_SPLINE_CURVE_WITH_KNOTS('',2,(#80700,#80701,#80702),
 .UNSPECIFIED.,.F.,.F.,(3,3),(0.,1.),.UNSPECIFIED.);
#157=B_SPLINE_CURVE_WITH_KNOTS('',2,(#80710,#80711,#80712),
 .UNSPECIFIED.,.F.,.F.,(3,3),(0.,1.),.UNSPECIFIED.);
#158=B_SPLINE_CURVE_WITH_KNOTS('',2,(#80715,#80716,#80717),
 .UNSPECIFIED.,.F.,.F.,(3,3),(0.,1.),.UNSPECIFIED.);
#159=B_SPLINE_CURVE_WITH_KNOTS('',2,(#80725,#80726,#80727),
 .UNSPECIFIED.,.F.,.F.,(3,3),(0.,1.),.UNSPECIFIED.);
#160=B_SPLINE_CURVE_WITH_KNOTS('',2,(#80730,#80731,#80732),
 .UNSPECIFIED.,.F.,.F.,(3,3),(0.,1.),.UNSPECIFIED.);
#161=B_SPLINE_CURVE_WITH_KNOTS('',2,(#80740,#80741,#80742),
 .UNSPECIFIED.,.F.,.F.,(3,3),(0.,1.),.UNSPECIFIED.);
#162=B_SPLINE_CURVE_WITH_KNOTS('',2,(#80745,#80746,#80747),
 .UNSPECIFIED.,.F.,.F.,(3,3),(0.,1.),.UNSPECIFIED.);
#163=B_SPLINE_CURVE_WITH_KNOTS('',2,(#80755,#80756,#80757),
 .UNSPECIFIED.,.F.,.F.,(3,3),(0.,1.),.UNSPECIFIED.);
#164=B_SPLINE_CURVE_WITH_KNOTS('',2,(#80760,#80761,#80762),
 .UNSPECIFIED.,.F.,.F.,(3,3),(0.,1.),.UNSPECIFIED.);
#165=B_SPLINE_CURVE_WITH_KNOTS('',2,(#80770,#80771,#80772),
 .UNSPECIFIED.,.F.,.F.,(3,3),(0.,1.),.UNSPECIFIED.);
#166=B_SPLINE_CURVE_WITH_KNOTS('',2,(#80775,#80776,#80777),
 .UNSPECIFIED.,.F.,.F.,(3,3),(0.,1.),.UNSPECIFIED.);
#167=B_SPLINE_CURVE_WITH_KNOTS('',2,(#80785,#80786,#80787),
 .UNSPECIFIED.,.F.,.F.,(3,3),(0.,1.),.UNSPECIFIED.);
#168=B_SPLINE_CURVE_WITH_KNOTS('',2,(#80790,#80791,#80792),
 .UNSPECIFIED.,.F.,.F.,(3,3),(0.,1.),.UNSPECIFIED.);
#169=B_SPLINE_CURVE_WITH_KNOTS('',2,(#80800,#80801,#80802),
 .UNSPECIFIED.,.F.,.F.,(3,3),(0.,1.),.UNSPECIFIED.);
#170=B_SPLINE_CURVE_WITH_KNOTS('',2,(#80805,#80806,#80807),
 .UNSPECIFIED.,.F.,.F.,(3,3),(0.,1.),.UNSPECIFIED.);
#171=B_SPLINE_CURVE_WITH_KNOTS('',2,(#80815,#80816,#80817),
 .UNSPECIFIED.,.F.,.F.,(3,3),(0.,1.),.UNSPECIFIED.);
#172=B_SPLINE_CURVE_WITH_KNOTS('',2,(#80820,#80821,#80822),
 .UNSPECIFIED.,.F.,.F.,(3,3),(0.,1.),.UNSPECIFIED.);
#173=B_SPLINE_CURVE_WITH_KNOTS('',2,(#80836,#80837,#80838),
 .UNSPECIFIED.,.F.,.F.,(3,3),(0.,1.),.UNSPECIFIED.);
#174=B_SPLINE_CURVE_WITH_KNOTS('',2,(#80841,#80842,#80843),
 .UNSPECIFIED.,.F.,.F.,(3,3),(0.,1.),.UNSPECIFIED.);
#175=B_SPLINE_CURVE_WITH_KNOTS('',2,(#80851,#80852,#80853),
 .UNSPECIFIED.,.F.,.F.,(3,3),(0.,1.),.UNSPECIFIED.);
#176=B_SPLINE_CURVE_WITH_KNOTS('',2,(#80856,#80857,#80858),
 .UNSPECIFIED.,.F.,.F.,(3,3),(0.,1.),.UNSPECIFIED.);
#177=B_SPLINE_CURVE_WITH_KNOTS('',2,(#80866,#80867,#80868),
 .UNSPECIFIED.,.F.,.F.,(3,3),(0.,1.),.UNSPECIFIED.);
#178=B_SPLINE_CURVE_WITH_KNOTS('',2,(#80871,#80872,#80873),
 .UNSPECIFIED.,.F.,.F.,(3,3),(0.,1.),.UNSPECIFIED.);
#179=B_SPLINE_CURVE_WITH_KNOTS('',2,(#80881,#80882,#80883),
 .UNSPECIFIED.,.F.,.F.,(3,3),(0.,1.),.UNSPECIFIED.);
#180=B_SPLINE_CURVE_WITH_KNOTS('',2,(#80886,#80887,#80888),
 .UNSPECIFIED.,.F.,.F.,(3,3),(0.,1.),.UNSPECIFIED.);
#181=B_SPLINE_CURVE_WITH_KNOTS('',2,(#80896,#80897,#80898),
 .UNSPECIFIED.,.F.,.F.,(3,3),(0.,1.),.UNSPECIFIED.);
#182=B_SPLINE_CURVE_WITH_KNOTS('',2,(#80901,#80902,#80903),
 .UNSPECIFIED.,.F.,.F.,(3,3),(0.,1.),.UNSPECIFIED.);
#183=B_SPLINE_CURVE_WITH_KNOTS('',2,(#80911,#80912,#80913),
 .UNSPECIFIED.,.F.,.F.,(3,3),(0.,1.),.UNSPECIFIED.);
#184=B_SPLINE_CURVE_WITH_KNOTS('',2,(#80916,#80917,#80918),
 .UNSPECIFIED.,.F.,.F.,(3,3),(0.,1.),.UNSPECIFIED.);
#185=B_SPLINE_CURVE_WITH_KNOTS('',2,(#80926,#80927,#80928),
 .UNSPECIFIED.,.F.,.F.,(3,3),(0.,1.),.UNSPECIFIED.);
#186=B_SPLINE_CURVE_WITH_KNOTS('',2,(#80931,#80932,#80933),
 .UNSPECIFIED.,.F.,.F.,(3,3),(0.,1.),.UNSPECIFIED.);
#187=B_SPLINE_CURVE_WITH_KNOTS('',2,(#80941,#80942,#80943),
 .UNSPECIFIED.,.F.,.F.,(3,3),(0.,1.),.UNSPECIFIED.);
#188=B_SPLINE_CURVE_WITH_KNOTS('',2,(#80946,#80947,#80948),
 .UNSPECIFIED.,.F.,.F.,(3,3),(0.,1.),.UNSPECIFIED.);
#189=B_SPLINE_CURVE_WITH_KNOTS('',2,(#80956,#80957,#80958),
 .UNSPECIFIED.,.F.,.F.,(3,3),(0.,1.),.UNSPECIFIED.);
#190=B_SPLINE_CURVE_WITH_KNOTS('',2,(#80961,#80962,#80963),
 .UNSPECIFIED.,.F.,.F.,(3,3),(0.,1.),.UNSPECIFIED.);
#191=B_SPLINE_CURVE_WITH_KNOTS('',2,(#80971,#80972,#80973),
 .UNSPECIFIED.,.F.,.F.,(3,3),(0.,1.),.UNSPECIFIED.);
#192=B_SPLINE_CURVE_WITH_KNOTS('',2,(#80976,#80977,#80978),
 .UNSPECIFIED.,.F.,.F.,(3,3),(0.,1.),.UNSPECIFIED.);
#193=B_SPLINE_CURVE_WITH_KNOTS('',2,(#80986,#80987,#80988),
 .UNSPECIFIED.,.F.,.F.,(3,3),(0.,1.),.UNSPECIFIED.);
#194=B_SPLINE_CURVE_WITH_KNOTS('',2,(#80991,#80992,#80993),
 .UNSPECIFIED.,.F.,.F.,(3,3),(0.,1.),.UNSPECIFIED.);
#195=B_SPLINE_CURVE_WITH_KNOTS('',2,(#81001,#81002,#81003),
 .UNSPECIFIED.,.F.,.F.,(3,3),(0.,1.),.UNSPECIFIED.);
#196=B_SPLINE_CURVE_WITH_KNOTS('',2,(#81006,#81007,#81008),
 .UNSPECIFIED.,.F.,.F.,(3,3),(0.,1.),.UNSPECIFIED.);
#197=B_SPLINE_CURVE_WITH_KNOTS('',2,(#81016,#81017,#81018),
 .UNSPECIFIED.,.F.,.F.,(3,3),(0.,1.),.UNSPECIFIED.);
#198=B_SPLINE_CURVE_WITH_KNOTS('',2,(#81021,#81022,#81023),
 .UNSPECIFIED.,.F.,.F.,(3,3),(0.,1.),.UNSPECIFIED.);
#199=B_SPLINE_CURVE_WITH_KNOTS('',2,(#81031,#81032,#81033),
 .UNSPECIFIED.,.F.,.F.,(3,3),(0.,1.),.UNSPECIFIED.);
#200=B_SPLINE_CURVE_WITH_KNOTS('',2,(#81036,#81037,#81038),
 .UNSPECIFIED.,.F.,.F.,(3,3),(0.,1.),.UNSPECIFIED.);
#201=B_SPLINE_CURVE_WITH_KNOTS('',2,(#81046,#81047,#81048),
 .UNSPECIFIED.,.F.,.F.,(3,3),(0.,1.),.UNSPECIFIED.);
#202=B_SPLINE_CURVE_WITH_KNOTS('',2,(#81051,#81052,#81053),
 .UNSPECIFIED.,.F.,.F.,(3,3),(0.,1.),.UNSPECIFIED.);
#203=B_SPLINE_CURVE_WITH_KNOTS('',2,(#81061,#81062,#81063),
 .UNSPECIFIED.,.F.,.F.,(3,3),(0.,1.),.UNSPECIFIED.);
#204=B_SPLINE_CURVE_WITH_KNOTS('',2,(#81066,#81067,#81068),
 .UNSPECIFIED.,.F.,.F.,(3,3),(0.,1.),.UNSPECIFIED.);
#205=B_SPLINE_CURVE_WITH_KNOTS('',2,(#81076,#81077,#81078),
 .UNSPECIFIED.,.F.,.F.,(3,3),(0.,1.),.UNSPECIFIED.);
#206=B_SPLINE_CURVE_WITH_KNOTS('',2,(#81081,#81082,#81083),
 .UNSPECIFIED.,.F.,.F.,(3,3),(0.,1.),.UNSPECIFIED.);
#207=B_SPLINE_CURVE_WITH_KNOTS('',2,(#81091,#81092,#81093),
 .UNSPECIFIED.,.F.,.F.,(3,3),(0.,1.),.UNSPECIFIED.);
#208=B_SPLINE_CURVE_WITH_KNOTS('',2,(#81096,#81097,#81098),
 .UNSPECIFIED.,.F.,.F.,(3,3),(0.,1.),.UNSPECIFIED.);
#209=B_SPLINE_CURVE_WITH_KNOTS('',2,(#81112,#81113,#81114),
 .UNSPECIFIED.,.F.,.F.,(3,3),(0.,1.),.UNSPECIFIED.);
#210=B_SPLINE_CURVE_WITH_KNOTS('',2,(#81117,#81118,#81119),
 .UNSPECIFIED.,.F.,.F.,(3,3),(0.,1.),.UNSPECIFIED.);
#211=B_SPLINE_CURVE_WITH_KNOTS('',2,(#81126,#81127,#81128),
 .UNSPECIFIED.,.F.,.F.,(3,3),(0.,1.),.UNSPECIFIED.);
#212=B_SPLINE_CURVE_WITH_KNOTS('',2,(#81129,#81130,#81131),
 .UNSPECIFIED.,.F.,.F.,(3,3),(0.,1.),.UNSPECIFIED.);
#213=B_SPLINE_CURVE_WITH_KNOTS('',2,(#81141,#81142,#81143),
 .UNSPECIFIED.,.F.,.F.,(3,3),(0.,1.),.UNSPECIFIED.);
#214=B_SPLINE_CURVE_WITH_KNOTS('',2,(#81147,#81148,#81149),
 .UNSPECIFIED.,.F.,.F.,(3,3),(0.,1.),.UNSPECIFIED.);
#215=B_SPLINE_CURVE_WITH_KNOTS('',2,(#81158,#81159,#81160),
 .UNSPECIFIED.,.F.,.F.,(3,3),(0.,1.),.UNSPECIFIED.);
#216=B_SPLINE_CURVE_WITH_KNOTS('',2,(#81163,#81164,#81165),
 .UNSPECIFIED.,.F.,.F.,(3,3),(0.,1.),.UNSPECIFIED.);
#217=B_SPLINE_CURVE_WITH_KNOTS('',2,(#81173,#81174,#81175),
 .UNSPECIFIED.,.F.,.F.,(3,3),(0.,1.),.UNSPECIFIED.);
#218=B_SPLINE_CURVE_WITH_KNOTS('',2,(#81178,#81179,#81180),
 .UNSPECIFIED.,.F.,.F.,(3,3),(0.,1.),.UNSPECIFIED.);
#219=B_SPLINE_CURVE_WITH_KNOTS('',2,(#81188,#81189,#81190),
 .UNSPECIFIED.,.F.,.F.,(3,3),(0.,1.),.UNSPECIFIED.);
#220=B_SPLINE_CURVE_WITH_KNOTS('',2,(#81193,#81194,#81195),
 .UNSPECIFIED.,.F.,.F.,(3,3),(0.,1.),.UNSPECIFIED.);
#221=B_SPLINE_CURVE_WITH_KNOTS('',2,(#81203,#81204,#81205),
 .UNSPECIFIED.,.F.,.F.,(3,3),(0.,1.),.UNSPECIFIED.);
#222=B_SPLINE_CURVE_WITH_KNOTS('',2,(#81208,#81209,#81210),
 .UNSPECIFIED.,.F.,.F.,(3,3),(0.,1.),.UNSPECIFIED.);
#223=B_SPLINE_CURVE_WITH_KNOTS('',2,(#81218,#81219,#81220),
 .UNSPECIFIED.,.F.,.F.,(3,3),(0.,1.),.UNSPECIFIED.);
#224=B_SPLINE_CURVE_WITH_KNOTS('',2,(#81223,#81224,#81225),
 .UNSPECIFIED.,.F.,.F.,(3,3),(0.,1.),.UNSPECIFIED.);
#225=B_SPLINE_CURVE_WITH_KNOTS('',2,(#81233,#81234,#81235),
 .UNSPECIFIED.,.F.,.F.,(3,3),(0.,1.),.UNSPECIFIED.);
#226=B_SPLINE_CURVE_WITH_KNOTS('',2,(#81238,#81239,#81240),
 .UNSPECIFIED.,.F.,.F.,(3,3),(0.,1.),.UNSPECIFIED.);
#227=B_SPLINE_CURVE_WITH_KNOTS('',2,(#81248,#81249,#81250),
 .UNSPECIFIED.,.F.,.F.,(3,3),(0.,1.),.UNSPECIFIED.);
#228=B_SPLINE_CURVE_WITH_KNOTS('',2,(#81253,#81254,#81255),
 .UNSPECIFIED.,.F.,.F.,(3,3),(0.,1.),.UNSPECIFIED.);
#229=B_SPLINE_CURVE_WITH_KNOTS('',2,(#81269,#81270,#81271),
 .UNSPECIFIED.,.F.,.F.,(3,3),(0.,1.),.UNSPECIFIED.);
#230=B_SPLINE_CURVE_WITH_KNOTS('',2,(#81274,#81275,#81276),
 .UNSPECIFIED.,.F.,.F.,(3,3),(0.,1.),.UNSPECIFIED.);
#231=B_SPLINE_CURVE_WITH_KNOTS('',2,(#81284,#81285,#81286),
 .UNSPECIFIED.,.F.,.F.,(3,3),(0.,1.),.UNSPECIFIED.);
#232=B_SPLINE_CURVE_WITH_KNOTS('',2,(#81289,#81290,#81291),
 .UNSPECIFIED.,.F.,.F.,(3,3),(0.,1.),.UNSPECIFIED.);
#233=B_SPLINE_CURVE_WITH_KNOTS('',2,(#81299,#81300,#81301),
 .UNSPECIFIED.,.F.,.F.,(3,3),(0.,1.),.UNSPECIFIED.);
#234=B_SPLINE_CURVE_WITH_KNOTS('',2,(#81304,#81305,#81306),
 .UNSPECIFIED.,.F.,.F.,(3,3),(0.,1.),.UNSPECIFIED.);
#235=B_SPLINE_CURVE_WITH_KNOTS('',2,(#81314,#81315,#81316),
 .UNSPECIFIED.,.F.,.F.,(3,3),(0.,1.),.UNSPECIFIED.);
#236=B_SPLINE_CURVE_WITH_KNOTS('',2,(#81319,#81320,#81321),
 .UNSPECIFIED.,.F.,.F.,(3,3),(0.,1.),.UNSPECIFIED.);
#237=B_SPLINE_CURVE_WITH_KNOTS('',2,(#81329,#81330,#81331),
 .UNSPECIFIED.,.F.,.F.,(3,3),(0.,1.),.UNSPECIFIED.);
#238=B_SPLINE_CURVE_WITH_KNOTS('',2,(#81334,#81335,#81336),
 .UNSPECIFIED.,.F.,.F.,(3,3),(0.,1.),.UNSPECIFIED.);
#239=B_SPLINE_CURVE_WITH_KNOTS('',2,(#81344,#81345,#81346),
 .UNSPECIFIED.,.F.,.F.,(3,3),(0.,1.),.UNSPECIFIED.);
#240=B_SPLINE_CURVE_WITH_KNOTS('',2,(#81349,#81350,#81351),
 .UNSPECIFIED.,.F.,.F.,(3,3),(0.,1.),.UNSPECIFIED.);
#241=B_SPLINE_CURVE_WITH_KNOTS('',2,(#81359,#81360,#81361),
 .UNSPECIFIED.,.F.,.F.,(3,3),(0.,1.),.UNSPECIFIED.);
#242=B_SPLINE_CURVE_WITH_KNOTS('',2,(#81364,#81365,#81366),
 .UNSPECIFIED.,.F.,.F.,(3,3),(0.,1.),.UNSPECIFIED.);
#243=B_SPLINE_CURVE_WITH_KNOTS('',2,(#81374,#81375,#81376),
 .UNSPECIFIED.,.F.,.F.,(3,3),(0.,1.),.UNSPECIFIED.);
#244=B_SPLINE_CURVE_WITH_KNOTS('',2,(#81379,#81380,#81381),
 .UNSPECIFIED.,.F.,.F.,(3,3),(0.,1.),.UNSPECIFIED.);
#245=B_SPLINE_CURVE_WITH_KNOTS('',2,(#81389,#81390,#81391),
 .UNSPECIFIED.,.F.,.F.,(3,3),(0.,1.),.UNSPECIFIED.);
#246=B_SPLINE_CURVE_WITH_KNOTS('',2,(#81394,#81395,#81396),
 .UNSPECIFIED.,.F.,.F.,(3,3),(0.,1.),.UNSPECIFIED.);
#247=B_SPLINE_CURVE_WITH_KNOTS('',2,(#81404,#81405,#81406),
 .UNSPECIFIED.,.F.,.F.,(3,3),(0.,1.),.UNSPECIFIED.);
#248=B_SPLINE_CURVE_WITH_KNOTS('',2,(#81409,#81410,#81411),
 .UNSPECIFIED.,.F.,.F.,(3,3),(0.,1.),.UNSPECIFIED.);
#249=B_SPLINE_CURVE_WITH_KNOTS('',2,(#81425,#81426,#81427),
 .UNSPECIFIED.,.F.,.F.,(3,3),(0.,1.),.UNSPECIFIED.);
#250=B_SPLINE_CURVE_WITH_KNOTS('',2,(#81430,#81431,#81432),
 .UNSPECIFIED.,.F.,.F.,(3,3),(0.,1.),.UNSPECIFIED.);
#251=B_SPLINE_CURVE_WITH_KNOTS('',2,(#81439,#81440,#81441),
 .UNSPECIFIED.,.F.,.F.,(3,3),(0.,1.),.UNSPECIFIED.);
#252=B_SPLINE_CURVE_WITH_KNOTS('',2,(#81442,#81443,#81444),
 .UNSPECIFIED.,.F.,.F.,(3,3),(0.,1.),.UNSPECIFIED.);
#253=B_SPLINE_CURVE_WITH_KNOTS('',2,(#81540,#81541,#81542),
 .UNSPECIFIED.,.F.,.F.,(3,3),(0.,1.),.UNSPECIFIED.);
#254=B_SPLINE_CURVE_WITH_KNOTS('',2,(#81546,#81547,#81548),
 .UNSPECIFIED.,.F.,.F.,(3,3),(0.,1.),.UNSPECIFIED.);
#255=B_SPLINE_CURVE_WITH_KNOTS('',2,(#81557,#81558,#81559),
 .UNSPECIFIED.,.F.,.F.,(3,3),(0.,1.),.UNSPECIFIED.);
#256=B_SPLINE_CURVE_WITH_KNOTS('',2,(#81562,#81563,#81564),
 .UNSPECIFIED.,.F.,.F.,(3,3),(0.,1.),.UNSPECIFIED.);
#257=B_SPLINE_CURVE_WITH_KNOTS('',2,(#81572,#81573,#81574),
 .UNSPECIFIED.,.F.,.F.,(3,3),(0.,1.),.UNSPECIFIED.);
#258=B_SPLINE_CURVE_WITH_KNOTS('',2,(#81577,#81578,#81579),
 .UNSPECIFIED.,.F.,.F.,(3,3),(0.,1.),.UNSPECIFIED.);
#259=B_SPLINE_CURVE_WITH_KNOTS('',2,(#81587,#81588,#81589),
 .UNSPECIFIED.,.F.,.F.,(3,3),(0.,1.),.UNSPECIFIED.);
#260=B_SPLINE_CURVE_WITH_KNOTS('',2,(#81592,#81593,#81594),
 .UNSPECIFIED.,.F.,.F.,(3,3),(0.,1.),.UNSPECIFIED.);
#261=B_SPLINE_CURVE_WITH_KNOTS('',2,(#81620,#81621,#81622),
 .UNSPECIFIED.,.F.,.F.,(3,3),(0.,1.),.UNSPECIFIED.);
#262=B_SPLINE_CURVE_WITH_KNOTS('',2,(#81625,#81626,#81627),
 .UNSPECIFIED.,.F.,.F.,(3,3),(0.,1.),.UNSPECIFIED.);
#263=B_SPLINE_CURVE_WITH_KNOTS('',2,(#81635,#81636,#81637),
 .UNSPECIFIED.,.F.,.F.,(3,3),(0.,1.),.UNSPECIFIED.);
#264=B_SPLINE_CURVE_WITH_KNOTS('',2,(#81640,#81641,#81642),
 .UNSPECIFIED.,.F.,.F.,(3,3),(0.,1.),.UNSPECIFIED.);
#265=B_SPLINE_CURVE_WITH_KNOTS('',2,(#81650,#81651,#81652),
 .UNSPECIFIED.,.F.,.F.,(3,3),(0.,1.),.UNSPECIFIED.);
#266=B_SPLINE_CURVE_WITH_KNOTS('',2,(#81655,#81656,#81657),
 .UNSPECIFIED.,.F.,.F.,(3,3),(0.,1.),.UNSPECIFIED.);
#267=B_SPLINE_CURVE_WITH_KNOTS('',2,(#81665,#81666,#81667),
 .UNSPECIFIED.,.F.,.F.,(3,3),(0.,1.),.UNSPECIFIED.);
#268=B_SPLINE_CURVE_WITH_KNOTS('',2,(#81670,#81671,#81672),
 .UNSPECIFIED.,.F.,.F.,(3,3),(0.,1.),.UNSPECIFIED.);
#269=B_SPLINE_CURVE_WITH_KNOTS('',2,(#81680,#81681,#81682),
 .UNSPECIFIED.,.F.,.F.,(3,3),(0.,1.),.UNSPECIFIED.);
#270=B_SPLINE_CURVE_WITH_KNOTS('',2,(#81685,#81686,#81687),
 .UNSPECIFIED.,.F.,.F.,(3,3),(0.,1.),.UNSPECIFIED.);
#271=B_SPLINE_CURVE_WITH_KNOTS('',2,(#81695,#81696,#81697),
 .UNSPECIFIED.,.F.,.F.,(3,3),(0.,1.),.UNSPECIFIED.);
#272=B_SPLINE_CURVE_WITH_KNOTS('',2,(#81700,#81701,#81702),
 .UNSPECIFIED.,.F.,.F.,(3,3),(0.,1.),.UNSPECIFIED.);
#273=B_SPLINE_CURVE_WITH_KNOTS('',2,(#81727,#81728,#81729),
 .UNSPECIFIED.,.F.,.F.,(3,3),(0.,1.),.UNSPECIFIED.);
#274=B_SPLINE_CURVE_WITH_KNOTS('',2,(#81730,#81731,#81732),
 .UNSPECIFIED.,.F.,.F.,(3,3),(0.,1.),.UNSPECIFIED.);
#275=B_SPLINE_CURVE_WITH_KNOTS('',2,(#81750,#81751,#81752),
 .UNSPECIFIED.,.F.,.F.,(3,3),(0.,1.),.UNSPECIFIED.);
#276=B_SPLINE_CURVE_WITH_KNOTS('',2,(#81755,#81756,#81757),
 .UNSPECIFIED.,.F.,.F.,(3,3),(0.,1.),.UNSPECIFIED.);
#277=B_SPLINE_CURVE_WITH_KNOTS('',2,(#81765,#81766,#81767),
 .UNSPECIFIED.,.F.,.F.,(3,3),(0.,1.),.UNSPECIFIED.);
#278=B_SPLINE_CURVE_WITH_KNOTS('',2,(#81770,#81771,#81772),
 .UNSPECIFIED.,.F.,.F.,(3,3),(0.,1.),.UNSPECIFIED.);
#279=B_SPLINE_CURVE_WITH_KNOTS('',2,(#81780,#81781,#81782),
 .UNSPECIFIED.,.F.,.F.,(3,3),(0.,1.),.UNSPECIFIED.);
#280=B_SPLINE_CURVE_WITH_KNOTS('',2,(#81785,#81786,#81787),
 .UNSPECIFIED.,.F.,.F.,(3,3),(0.,1.),.UNSPECIFIED.);
#281=B_SPLINE_CURVE_WITH_KNOTS('',2,(#81795,#81796,#81797),
 .UNSPECIFIED.,.F.,.F.,(3,3),(0.,1.),.UNSPECIFIED.);
#282=B_SPLINE_CURVE_WITH_KNOTS('',2,(#81800,#81801,#81802),
 .UNSPECIFIED.,.F.,.F.,(3,3),(0.,1.),.UNSPECIFIED.);
#283=B_SPLINE_CURVE_WITH_KNOTS('',2,(#81828,#81829,#81830),
 .UNSPECIFIED.,.F.,.F.,(3,3),(0.,1.),.UNSPECIFIED.);
#284=B_SPLINE_CURVE_WITH_KNOTS('',2,(#81833,#81834,#81835),
 .UNSPECIFIED.,.F.,.F.,(3,3),(0.,1.),.UNSPECIFIED.);
#285=B_SPLINE_CURVE_WITH_KNOTS('',2,(#81843,#81844,#81845),
 .UNSPECIFIED.,.F.,.F.,(3,3),(0.,1.),.UNSPECIFIED.);
#286=B_SPLINE_CURVE_WITH_KNOTS('',2,(#81848,#81849,#81850),
 .UNSPECIFIED.,.F.,.F.,(3,3),(0.,1.),.UNSPECIFIED.);
#287=B_SPLINE_CURVE_WITH_KNOTS('',2,(#81858,#81859,#81860),
 .UNSPECIFIED.,.F.,.F.,(3,3),(0.,1.),.UNSPECIFIED.);
#288=B_SPLINE_CURVE_WITH_KNOTS('',2,(#81863,#81864,#81865),
 .UNSPECIFIED.,.F.,.F.,(3,3),(0.,1.),.UNSPECIFIED.);
#289=B_SPLINE_CURVE_WITH_KNOTS('',2,(#81873,#81874,#81875),
 .UNSPECIFIED.,.F.,.F.,(3,3),(0.,1.),.UNSPECIFIED.);
#290=B_SPLINE_CURVE_WITH_KNOTS('',2,(#81878,#81879,#81880),
 .UNSPECIFIED.,.F.,.F.,(3,3),(0.,1.),.UNSPECIFIED.);
#291=B_SPLINE_CURVE_WITH_KNOTS('',2,(#81888,#81889,#81890),
 .UNSPECIFIED.,.F.,.F.,(3,3),(0.,1.),.UNSPECIFIED.);
#292=B_SPLINE_CURVE_WITH_KNOTS('',2,(#81893,#81894,#81895),
 .UNSPECIFIED.,.F.,.F.,(3,3),(0.,1.),.UNSPECIFIED.);
#293=B_SPLINE_CURVE_WITH_KNOTS('',2,(#81903,#81904,#81905),
 .UNSPECIFIED.,.F.,.F.,(3,3),(0.,1.),.UNSPECIFIED.);
#294=B_SPLINE_CURVE_WITH_KNOTS('',2,(#81908,#81909,#81910),
 .UNSPECIFIED.,.F.,.F.,(3,3),(0.,1.),.UNSPECIFIED.);
#295=B_SPLINE_CURVE_WITH_KNOTS('',2,(#81918,#81919,#81920),
 .UNSPECIFIED.,.F.,.F.,(3,3),(0.,1.),.UNSPECIFIED.);
#296=B_SPLINE_CURVE_WITH_KNOTS('',2,(#81923,#81924,#81925),
 .UNSPECIFIED.,.F.,.F.,(3,3),(0.,1.),.UNSPECIFIED.);
#297=B_SPLINE_CURVE_WITH_KNOTS('',2,(#82005,#82006,#82007),
 .UNSPECIFIED.,.F.,.F.,(3,3),(0.,1.),.UNSPECIFIED.);
#298=B_SPLINE_CURVE_WITH_KNOTS('',2,(#82011,#82012,#82013),
 .UNSPECIFIED.,.F.,.F.,(3,3),(0.,1.),.UNSPECIFIED.);
#299=B_SPLINE_CURVE_WITH_KNOTS('',2,(#82022,#82023,#82024),
 .UNSPECIFIED.,.F.,.F.,(3,3),(0.,1.),.UNSPECIFIED.);
#300=B_SPLINE_CURVE_WITH_KNOTS('',2,(#82027,#82028,#82029),
 .UNSPECIFIED.,.F.,.F.,(3,3),(0.,1.),.UNSPECIFIED.);
#301=B_SPLINE_CURVE_WITH_KNOTS('',2,(#82043,#82044,#82045),
 .UNSPECIFIED.,.F.,.F.,(3,3),(0.,1.),.UNSPECIFIED.);
#302=B_SPLINE_CURVE_WITH_KNOTS('',2,(#82048,#82049,#82050),
 .UNSPECIFIED.,.F.,.F.,(3,3),(0.,1.),.UNSPECIFIED.);
#303=B_SPLINE_CURVE_WITH_KNOTS('',2,(#82058,#82059,#82060),
 .UNSPECIFIED.,.F.,.F.,(3,3),(0.,1.),.UNSPECIFIED.);
#304=B_SPLINE_CURVE_WITH_KNOTS('',2,(#82063,#82064,#82065),
 .UNSPECIFIED.,.F.,.F.,(3,3),(0.,1.),.UNSPECIFIED.);
#305=B_SPLINE_CURVE_WITH_KNOTS('',2,(#82096,#82097,#82098),
 .UNSPECIFIED.,.F.,.F.,(3,3),(0.,1.),.UNSPECIFIED.);
#306=B_SPLINE_CURVE_WITH_KNOTS('',2,(#82102,#82103,#82104),
 .UNSPECIFIED.,.F.,.F.,(3,3),(0.,1.),.UNSPECIFIED.);
#307=B_SPLINE_CURVE_WITH_KNOTS('',2,(#82113,#82114,#82115),
 .UNSPECIFIED.,.F.,.F.,(3,3),(0.,1.),.UNSPECIFIED.);
#308=B_SPLINE_CURVE_WITH_KNOTS('',2,(#82118,#82119,#82120),
 .UNSPECIFIED.,.F.,.F.,(3,3),(0.,1.),.UNSPECIFIED.);
#309=B_SPLINE_CURVE_WITH_KNOTS('',2,(#82128,#82129,#82130),
 .UNSPECIFIED.,.F.,.F.,(3,3),(0.,1.),.UNSPECIFIED.);
#310=B_SPLINE_CURVE_WITH_KNOTS('',2,(#82133,#82134,#82135),
 .UNSPECIFIED.,.F.,.F.,(3,3),(0.,1.),.UNSPECIFIED.);
#311=B_SPLINE_CURVE_WITH_KNOTS('',2,(#82143,#82144,#82145),
 .UNSPECIFIED.,.F.,.F.,(3,3),(0.,1.),.UNSPECIFIED.);
#312=B_SPLINE_CURVE_WITH_KNOTS('',2,(#82148,#82149,#82150),
 .UNSPECIFIED.,.F.,.F.,(3,3),(0.,1.),.UNSPECIFIED.);
#313=B_SPLINE_CURVE_WITH_KNOTS('',2,(#82158,#82159,#82160),
 .UNSPECIFIED.,.F.,.F.,(3,3),(0.,1.),.UNSPECIFIED.);
#314=B_SPLINE_CURVE_WITH_KNOTS('',2,(#82163,#82164,#82165),
 .UNSPECIFIED.,.F.,.F.,(3,3),(0.,1.),.UNSPECIFIED.);
#315=B_SPLINE_CURVE_WITH_KNOTS('',2,(#82173,#82174,#82175),
 .UNSPECIFIED.,.F.,.F.,(3,3),(0.,1.),.UNSPECIFIED.);
#316=B_SPLINE_CURVE_WITH_KNOTS('',2,(#82178,#82179,#82180),
 .UNSPECIFIED.,.F.,.F.,(3,3),(0.,1.),.UNSPECIFIED.);
#317=B_SPLINE_CURVE_WITH_KNOTS('',2,(#82188,#82189,#82190),
 .UNSPECIFIED.,.F.,.F.,(3,3),(0.,1.),.UNSPECIFIED.);
#318=B_SPLINE_CURVE_WITH_KNOTS('',2,(#82193,#82194,#82195),
 .UNSPECIFIED.,.F.,.F.,(3,3),(0.,1.),.UNSPECIFIED.);
#319=B_SPLINE_CURVE_WITH_KNOTS('',2,(#82203,#82204,#82205),
 .UNSPECIFIED.,.F.,.F.,(3,3),(0.,1.),.UNSPECIFIED.);
#320=B_SPLINE_CURVE_WITH_KNOTS('',2,(#82208,#82209,#82210),
 .UNSPECIFIED.,.F.,.F.,(3,3),(0.,1.),.UNSPECIFIED.);
#321=B_SPLINE_CURVE_WITH_KNOTS('',2,(#82218,#82219,#82220),
 .UNSPECIFIED.,.F.,.F.,(3,3),(0.,1.),.UNSPECIFIED.);
#322=B_SPLINE_CURVE_WITH_KNOTS('',2,(#82223,#82224,#82225),
 .UNSPECIFIED.,.F.,.F.,(3,3),(0.,1.),.UNSPECIFIED.);
#323=B_SPLINE_CURVE_WITH_KNOTS('',2,(#82233,#82234,#82235),
 .UNSPECIFIED.,.F.,.F.,(3,3),(0.,1.),.UNSPECIFIED.);
#324=B_SPLINE_CURVE_WITH_KNOTS('',2,(#82238,#82239,#82240),
 .UNSPECIFIED.,.F.,.F.,(3,3),(0.,1.),.UNSPECIFIED.);
#325=B_SPLINE_CURVE_WITH_KNOTS('',2,(#82248,#82249,#82250),
 .UNSPECIFIED.,.F.,.F.,(3,3),(0.,1.),.UNSPECIFIED.);
#326=B_SPLINE_CURVE_WITH_KNOTS('',2,(#82253,#82254,#82255),
 .UNSPECIFIED.,.F.,.F.,(3,3),(0.,1.),.UNSPECIFIED.);
#327=B_SPLINE_CURVE_WITH_KNOTS('',2,(#82262,#82263,#82264),
 .UNSPECIFIED.,.F.,.F.,(3,3),(0.,1.),.UNSPECIFIED.);
#328=B_SPLINE_CURVE_WITH_KNOTS('',2,(#82265,#82266,#82267),
 .UNSPECIFIED.,.F.,.F.,(3,3),(0.,1.),.UNSPECIFIED.);
#329=B_SPLINE_CURVE_WITH_KNOTS('',2,(#82277,#82278,#82279),
 .UNSPECIFIED.,.F.,.F.,(3,3),(0.,1.),.UNSPECIFIED.);
#330=B_SPLINE_CURVE_WITH_KNOTS('',2,(#82283,#82284,#82285),
 .UNSPECIFIED.,.F.,.F.,(3,3),(0.,1.),.UNSPECIFIED.);
#331=B_SPLINE_CURVE_WITH_KNOTS('',2,(#82294,#82295,#82296),
 .UNSPECIFIED.,.F.,.F.,(3,3),(0.,1.),.UNSPECIFIED.);
#332=B_SPLINE_CURVE_WITH_KNOTS('',2,(#82299,#82300,#82301),
 .UNSPECIFIED.,.F.,.F.,(3,3),(0.,1.),.UNSPECIFIED.);
#333=B_SPLINE_CURVE_WITH_KNOTS('',2,(#82315,#82316,#82317),
 .UNSPECIFIED.,.F.,.F.,(3,3),(0.,1.),.UNSPECIFIED.);
#334=B_SPLINE_CURVE_WITH_KNOTS('',2,(#82320,#82321,#82322),
 .UNSPECIFIED.,.F.,.F.,(3,3),(0.,1.),.UNSPECIFIED.);
#335=B_SPLINE_CURVE_WITH_KNOTS('',2,(#82330,#82331,#82332),
 .UNSPECIFIED.,.F.,.F.,(3,3),(0.,1.),.UNSPECIFIED.);
#336=B_SPLINE_CURVE_WITH_KNOTS('',2,(#82335,#82336,#82337),
 .UNSPECIFIED.,.F.,.F.,(3,3),(0.,1.),.UNSPECIFIED.);
#337=B_SPLINE_CURVE_WITH_KNOTS('',2,(#82393,#82394,#82395),
 .UNSPECIFIED.,.F.,.F.,(3,3),(0.,1.),.UNSPECIFIED.);
#338=B_SPLINE_CURVE_WITH_KNOTS('',2,(#82399,#82400,#82401),
 .UNSPECIFIED.,.F.,.F.,(3,3),(0.,1.),.UNSPECIFIED.);
#339=B_SPLINE_CURVE_WITH_KNOTS('',2,(#82410,#82411,#82412),
 .UNSPECIFIED.,.F.,.F.,(3,3),(0.,1.),.UNSPECIFIED.);
#340=B_SPLINE_CURVE_WITH_KNOTS('',2,(#82415,#82416,#82417),
 .UNSPECIFIED.,.F.,.F.,(3,3),(0.,1.),.UNSPECIFIED.);
#341=B_SPLINE_CURVE_WITH_KNOTS('',2,(#82425,#82426,#82427),
 .UNSPECIFIED.,.F.,.F.,(3,3),(0.,1.),.UNSPECIFIED.);
#342=B_SPLINE_CURVE_WITH_KNOTS('',2,(#82430,#82431,#82432),
 .UNSPECIFIED.,.F.,.F.,(3,3),(0.,1.),.UNSPECIFIED.);
#343=B_SPLINE_CURVE_WITH_KNOTS('',2,(#82440,#82441,#82442),
 .UNSPECIFIED.,.F.,.F.,(3,3),(0.,1.),.UNSPECIFIED.);
#344=B_SPLINE_CURVE_WITH_KNOTS('',2,(#82445,#82446,#82447),
 .UNSPECIFIED.,.F.,.F.,(3,3),(0.,1.),.UNSPECIFIED.);
#345=B_SPLINE_CURVE_WITH_KNOTS('',2,(#82455,#82456,#82457),
 .UNSPECIFIED.,.F.,.F.,(3,3),(0.,1.),.UNSPECIFIED.);
#346=B_SPLINE_CURVE_WITH_KNOTS('',2,(#82460,#82461,#82462),
 .UNSPECIFIED.,.F.,.F.,(3,3),(0.,1.),.UNSPECIFIED.);
#347=B_SPLINE_CURVE_WITH_KNOTS('',2,(#82506,#82507,#82508),
 .UNSPECIFIED.,.F.,.F.,(3,3),(0.,1.),.UNSPECIFIED.);
#348=B_SPLINE_CURVE_WITH_KNOTS('',2,(#82511,#82512,#82513),
 .UNSPECIFIED.,.F.,.F.,(3,3),(0.,1.),.UNSPECIFIED.);
#349=B_SPLINE_CURVE_WITH_KNOTS('',2,(#82521,#82522,#82523),
 .UNSPECIFIED.,.F.,.F.,(3,3),(0.,1.),.UNSPECIFIED.);
#350=B_SPLINE_CURVE_WITH_KNOTS('',2,(#82526,#82527,#82528),
 .UNSPECIFIED.,.F.,.F.,(3,3),(0.,1.),.UNSPECIFIED.);
#351=B_SPLINE_CURVE_WITH_KNOTS('',2,(#82536,#82537,#82538),
 .UNSPECIFIED.,.F.,.F.,(3,3),(0.,1.),.UNSPECIFIED.);
#352=B_SPLINE_CURVE_WITH_KNOTS('',2,(#82541,#82542,#82543),
 .UNSPECIFIED.,.F.,.F.,(3,3),(0.,1.),.UNSPECIFIED.);
#353=B_SPLINE_CURVE_WITH_KNOTS('',2,(#82551,#82552,#82553),
 .UNSPECIFIED.,.F.,.F.,(3,3),(0.,1.),.UNSPECIFIED.);
#354=B_SPLINE_CURVE_WITH_KNOTS('',2,(#82556,#82557,#82558),
 .UNSPECIFIED.,.F.,.F.,(3,3),(0.,1.),.UNSPECIFIED.);
#355=B_SPLINE_CURVE_WITH_KNOTS('',2,(#82566,#82567,#82568),
 .UNSPECIFIED.,.F.,.F.,(3,3),(0.,1.),.UNSPECIFIED.);
#356=B_SPLINE_CURVE_WITH_KNOTS('',2,(#82571,#82572,#82573),
 .UNSPECIFIED.,.F.,.F.,(3,3),(0.,1.),.UNSPECIFIED.);
#357=B_SPLINE_CURVE_WITH_KNOTS('',2,(#82581,#82582,#82583),
 .UNSPECIFIED.,.F.,.F.,(3,3),(0.,1.),.UNSPECIFIED.);
#358=B_SPLINE_CURVE_WITH_KNOTS('',2,(#82586,#82587,#82588),
 .UNSPECIFIED.,.F.,.F.,(3,3),(0.,1.),.UNSPECIFIED.);
#359=B_SPLINE_CURVE_WITH_KNOTS('',2,(#82596,#82597,#82598),
 .UNSPECIFIED.,.F.,.F.,(3,3),(0.,1.),.UNSPECIFIED.);
#360=B_SPLINE_CURVE_WITH_KNOTS('',2,(#82601,#82602,#82603),
 .UNSPECIFIED.,.F.,.F.,(3,3),(0.,1.),.UNSPECIFIED.);
#361=B_SPLINE_CURVE_WITH_KNOTS('',2,(#82611,#82612,#82613),
 .UNSPECIFIED.,.F.,.F.,(3,3),(0.,1.),.UNSPECIFIED.);
#362=B_SPLINE_CURVE_WITH_KNOTS('',2,(#82616,#82617,#82618),
 .UNSPECIFIED.,.F.,.F.,(3,3),(0.,1.),.UNSPECIFIED.);
#363=B_SPLINE_CURVE_WITH_KNOTS('',2,(#82632,#82633,#82634),
 .UNSPECIFIED.,.F.,.F.,(3,3),(0.,1.),.UNSPECIFIED.);
#364=B_SPLINE_CURVE_WITH_KNOTS('',2,(#82637,#82638,#82639),
 .UNSPECIFIED.,.F.,.F.,(3,3),(0.,1.),.UNSPECIFIED.);
#365=B_SPLINE_CURVE_WITH_KNOTS('',2,(#82646,#82647,#82648),
 .UNSPECIFIED.,.F.,.F.,(3,3),(0.,1.),.UNSPECIFIED.);
#366=B_SPLINE_CURVE_WITH_KNOTS('',2,(#82649,#82650,#82651),
 .UNSPECIFIED.,.F.,.F.,(3,3),(0.,1.),.UNSPECIFIED.);
#367=B_SPLINE_CURVE_WITH_KNOTS('',2,(#82661,#82662,#82663),
 .UNSPECIFIED.,.F.,.F.,(3,3),(0.,1.),.UNSPECIFIED.);
#368=B_SPLINE_CURVE_WITH_KNOTS('',2,(#82667,#82668,#82669),
 .UNSPECIFIED.,.F.,.F.,(3,3),(0.,1.),.UNSPECIFIED.);
#369=B_SPLINE_CURVE_WITH_KNOTS('',2,(#82678,#82679,#82680),
 .UNSPECIFIED.,.F.,.F.,(3,3),(0.,1.),.UNSPECIFIED.);
#370=B_SPLINE_CURVE_WITH_KNOTS('',2,(#82683,#82684,#82685),
 .UNSPECIFIED.,.F.,.F.,(3,3),(0.,1.),.UNSPECIFIED.);
#371=B_SPLINE_CURVE_WITH_KNOTS('',2,(#82693,#82694,#82695),
 .UNSPECIFIED.,.F.,.F.,(3,3),(0.,1.),.UNSPECIFIED.);
#372=B_SPLINE_CURVE_WITH_KNOTS('',2,(#82698,#82699,#82700),
 .UNSPECIFIED.,.F.,.F.,(3,3),(0.,1.),.UNSPECIFIED.);
#373=B_SPLINE_CURVE_WITH_KNOTS('',2,(#82708,#82709,#82710),
 .UNSPECIFIED.,.F.,.F.,(3,3),(0.,1.),.UNSPECIFIED.);
#374=B_SPLINE_CURVE_WITH_KNOTS('',2,(#82713,#82714,#82715),
 .UNSPECIFIED.,.F.,.F.,(3,3),(0.,1.),.UNSPECIFIED.);
#375=B_SPLINE_CURVE_WITH_KNOTS('',2,(#82723,#82724,#82725),
 .UNSPECIFIED.,.F.,.F.,(3,3),(0.,1.),.UNSPECIFIED.);
#376=B_SPLINE_CURVE_WITH_KNOTS('',2,(#82728,#82729,#82730),
 .UNSPECIFIED.,.F.,.F.,(3,3),(0.,1.),.UNSPECIFIED.);
#377=B_SPLINE_CURVE_WITH_KNOTS('',2,(#82738,#82739,#82740),
 .UNSPECIFIED.,.F.,.F.,(3,3),(0.,1.),.UNSPECIFIED.);
#378=B_SPLINE_CURVE_WITH_KNOTS('',2,(#82743,#82744,#82745),
 .UNSPECIFIED.,.F.,.F.,(3,3),(0.,1.),.UNSPECIFIED.);
#379=B_SPLINE_CURVE_WITH_KNOTS('',2,(#82753,#82754,#82755),
 .UNSPECIFIED.,.F.,.F.,(3,3),(0.,1.),.UNSPECIFIED.);
#380=B_SPLINE_CURVE_WITH_KNOTS('',2,(#82758,#82759,#82760),
 .UNSPECIFIED.,.F.,.F.,(3,3),(0.,1.),.UNSPECIFIED.);
#381=B_SPLINE_CURVE_WITH_KNOTS('',2,(#82768,#82769,#82770),
 .UNSPECIFIED.,.F.,.F.,(3,3),(0.,1.),.UNSPECIFIED.);
#382=B_SPLINE_CURVE_WITH_KNOTS('',2,(#82773,#82774,#82775),
 .UNSPECIFIED.,.F.,.F.,(3,3),(0.,1.),.UNSPECIFIED.);
#383=B_SPLINE_CURVE_WITH_KNOTS('',2,(#82783,#82784,#82785),
 .UNSPECIFIED.,.F.,.F.,(3,3),(0.,1.),.UNSPECIFIED.);
#384=B_SPLINE_CURVE_WITH_KNOTS('',2,(#82788,#82789,#82790),
 .UNSPECIFIED.,.F.,.F.,(3,3),(0.,1.),.UNSPECIFIED.);
#385=B_SPLINE_CURVE_WITH_KNOTS('',2,(#82798,#82799,#82800),
 .UNSPECIFIED.,.F.,.F.,(3,3),(0.,1.),.UNSPECIFIED.);
#386=B_SPLINE_CURVE_WITH_KNOTS('',2,(#82803,#82804,#82805),
 .UNSPECIFIED.,.F.,.F.,(3,3),(0.,1.),.UNSPECIFIED.);
#387=B_SPLINE_CURVE_WITH_KNOTS('',2,(#82812,#82813,#82814),
 .UNSPECIFIED.,.F.,.F.,(3,3),(0.,1.),.UNSPECIFIED.);
#388=B_SPLINE_CURVE_WITH_KNOTS('',2,(#82815,#82816,#82817),
 .UNSPECIFIED.,.F.,.F.,(3,3),(0.,1.),.UNSPECIFIED.);
#389=B_SPLINE_CURVE_WITH_KNOTS('',2,(#82827,#82828,#82829),
 .UNSPECIFIED.,.F.,.F.,(3,3),(0.,1.),.UNSPECIFIED.);
#390=B_SPLINE_CURVE_WITH_KNOTS('',2,(#82833,#82834,#82835),
 .UNSPECIFIED.,.F.,.F.,(3,3),(0.,1.),.UNSPECIFIED.);
#391=B_SPLINE_CURVE_WITH_KNOTS('',2,(#82844,#82845,#82846),
 .UNSPECIFIED.,.F.,.F.,(3,3),(0.,1.),.UNSPECIFIED.);
#392=B_SPLINE_CURVE_WITH_KNOTS('',2,(#82849,#82850,#82851),
 .UNSPECIFIED.,.F.,.F.,(3,3),(0.,1.),.UNSPECIFIED.);
#393=B_SPLINE_CURVE_WITH_KNOTS('',2,(#82859,#82860,#82861),
 .UNSPECIFIED.,.F.,.F.,(3,3),(0.,1.),.UNSPECIFIED.);
#394=B_SPLINE_CURVE_WITH_KNOTS('',2,(#82864,#82865,#82866),
 .UNSPECIFIED.,.F.,.F.,(3,3),(0.,1.),.UNSPECIFIED.);
#395=B_SPLINE_CURVE_WITH_KNOTS('',2,(#82874,#82875,#82876),
 .UNSPECIFIED.,.F.,.F.,(3,3),(0.,1.),.UNSPECIFIED.);
#396=B_SPLINE_CURVE_WITH_KNOTS('',2,(#82879,#82880,#82881),
 .UNSPECIFIED.,.F.,.F.,(3,3),(0.,1.),.UNSPECIFIED.);
#397=B_SPLINE_CURVE_WITH_KNOTS('',2,(#82889,#82890,#82891),
 .UNSPECIFIED.,.F.,.F.,(3,3),(0.,1.),.UNSPECIFIED.);
#398=B_SPLINE_CURVE_WITH_KNOTS('',2,(#82894,#82895,#82896),
 .UNSPECIFIED.,.F.,.F.,(3,3),(0.,1.),.UNSPECIFIED.);
#399=B_SPLINE_CURVE_WITH_KNOTS('',2,(#82904,#82905,#82906),
 .UNSPECIFIED.,.F.,.F.,(3,3),(0.,1.),.UNSPECIFIED.);
#400=B_SPLINE_CURVE_WITH_KNOTS('',2,(#82909,#82910,#82911),
 .UNSPECIFIED.,.F.,.F.,(3,3),(0.,1.),.UNSPECIFIED.);
#401=B_SPLINE_CURVE_WITH_KNOTS('',2,(#82919,#82920,#82921),
 .UNSPECIFIED.,.F.,.F.,(3,3),(0.,1.),.UNSPECIFIED.);
#402=B_SPLINE_CURVE_WITH_KNOTS('',2,(#82924,#82925,#82926),
 .UNSPECIFIED.,.F.,.F.,(3,3),(0.,1.),.UNSPECIFIED.);
#403=B_SPLINE_CURVE_WITH_KNOTS('',2,(#82934,#82935,#82936),
 .UNSPECIFIED.,.F.,.F.,(3,3),(0.,1.),.UNSPECIFIED.);
#404=B_SPLINE_CURVE_WITH_KNOTS('',2,(#82939,#82940,#82941),
 .UNSPECIFIED.,.F.,.F.,(3,3),(0.,1.),.UNSPECIFIED.);
#405=B_SPLINE_CURVE_WITH_KNOTS('',2,(#82949,#82950,#82951),
 .UNSPECIFIED.,.F.,.F.,(3,3),(0.,1.),.UNSPECIFIED.);
#406=B_SPLINE_CURVE_WITH_KNOTS('',2,(#82954,#82955,#82956),
 .UNSPECIFIED.,.F.,.F.,(3,3),(0.,1.),.UNSPECIFIED.);
#407=B_SPLINE_CURVE_WITH_KNOTS('',2,(#82964,#82965,#82966),
 .UNSPECIFIED.,.F.,.F.,(3,3),(0.,1.),.UNSPECIFIED.);
#408=B_SPLINE_CURVE_WITH_KNOTS('',2,(#82969,#82970,#82971),
 .UNSPECIFIED.,.F.,.F.,(3,3),(0.,1.),.UNSPECIFIED.);
#409=B_SPLINE_CURVE_WITH_KNOTS('',2,(#82979,#82980,#82981),
 .UNSPECIFIED.,.F.,.F.,(3,3),(0.,1.),.UNSPECIFIED.);
#410=B_SPLINE_CURVE_WITH_KNOTS('',2,(#82984,#82985,#82986),
 .UNSPECIFIED.,.F.,.F.,(3,3),(0.,1.),.UNSPECIFIED.);
#411=B_SPLINE_CURVE_WITH_KNOTS('',2,(#83000,#83001,#83002),
 .UNSPECIFIED.,.F.,.F.,(3,3),(0.,1.),.UNSPECIFIED.);
#412=B_SPLINE_CURVE_WITH_KNOTS('',2,(#83005,#83006,#83007),
 .UNSPECIFIED.,.F.,.F.,(3,3),(0.,1.),.UNSPECIFIED.);
#413=B_SPLINE_CURVE_WITH_KNOTS('',2,(#83015,#83016,#83017),
 .UNSPECIFIED.,.F.,.F.,(3,3),(0.,1.),.UNSPECIFIED.);
#414=B_SPLINE_CURVE_WITH_KNOTS('',2,(#83020,#83021,#83022),
 .UNSPECIFIED.,.F.,.F.,(3,3),(0.,1.),.UNSPECIFIED.);
#415=B_SPLINE_CURVE_WITH_KNOTS('',2,(#83029,#83030,#83031),
 .UNSPECIFIED.,.F.,.F.,(3,3),(0.,1.),.UNSPECIFIED.);
#416=B_SPLINE_CURVE_WITH_KNOTS('',2,(#83032,#83033,#83034),
 .UNSPECIFIED.,.F.,.F.,(3,3),(0.,1.),.UNSPECIFIED.);
#417=B_SPLINE_CURVE_WITH_KNOTS('',2,(#83142,#83143,#83144),
 .UNSPECIFIED.,.F.,.F.,(3,3),(0.,1.),.UNSPECIFIED.);
#418=B_SPLINE_CURVE_WITH_KNOTS('',2,(#83148,#83149,#83150),
 .UNSPECIFIED.,.F.,.F.,(3,3),(0.,1.),.UNSPECIFIED.);
#419=B_SPLINE_CURVE_WITH_KNOTS('',2,(#83159,#83160,#83161),
 .UNSPECIFIED.,.F.,.F.,(3,3),(0.,1.),.UNSPECIFIED.);
#420=B_SPLINE_CURVE_WITH_KNOTS('',2,(#83164,#83165,#83166),
 .UNSPECIFIED.,.F.,.F.,(3,3),(0.,1.),.UNSPECIFIED.);
#421=B_SPLINE_CURVE_WITH_KNOTS('',2,(#83174,#83175,#83176),
 .UNSPECIFIED.,.F.,.F.,(3,3),(0.,1.),.UNSPECIFIED.);
#422=B_SPLINE_CURVE_WITH_KNOTS('',2,(#83179,#83180,#83181),
 .UNSPECIFIED.,.F.,.F.,(3,3),(0.,1.),.UNSPECIFIED.);
#423=B_SPLINE_CURVE_WITH_KNOTS('',2,(#83189,#83190,#83191),
 .UNSPECIFIED.,.F.,.F.,(3,3),(0.,1.),.UNSPECIFIED.);
#424=B_SPLINE_CURVE_WITH_KNOTS('',2,(#83194,#83195,#83196),
 .UNSPECIFIED.,.F.,.F.,(3,3),(0.,1.),.UNSPECIFIED.);
#425=B_SPLINE_CURVE_WITH_KNOTS('',2,(#83204,#83205,#83206),
 .UNSPECIFIED.,.F.,.F.,(3,3),(0.,1.),.UNSPECIFIED.);
#426=B_SPLINE_CURVE_WITH_KNOTS('',2,(#83209,#83210,#83211),
 .UNSPECIFIED.,.F.,.F.,(3,3),(0.,1.),.UNSPECIFIED.);
#427=B_SPLINE_CURVE_WITH_KNOTS('',2,(#83219,#83220,#83221),
 .UNSPECIFIED.,.F.,.F.,(3,3),(0.,1.),.UNSPECIFIED.);
#428=B_SPLINE_CURVE_WITH_KNOTS('',2,(#83224,#83225,#83226),
 .UNSPECIFIED.,.F.,.F.,(3,3),(0.,1.),.UNSPECIFIED.);
#429=B_SPLINE_CURVE_WITH_KNOTS('',2,(#83234,#83235,#83236),
 .UNSPECIFIED.,.F.,.F.,(3,3),(0.,1.),.UNSPECIFIED.);
#430=B_SPLINE_CURVE_WITH_KNOTS('',2,(#83239,#83240,#83241),
 .UNSPECIFIED.,.F.,.F.,(3,3),(0.,1.),.UNSPECIFIED.);
#431=B_SPLINE_CURVE_WITH_KNOTS('',2,(#83249,#83250,#83251),
 .UNSPECIFIED.,.F.,.F.,(3,3),(0.,1.),.UNSPECIFIED.);
#432=B_SPLINE_CURVE_WITH_KNOTS('',2,(#83254,#83255,#83256),
 .UNSPECIFIED.,.F.,.F.,(3,3),(0.,1.),.UNSPECIFIED.);
#433=B_SPLINE_CURVE_WITH_KNOTS('',2,(#83264,#83265,#83266),
 .UNSPECIFIED.,.F.,.F.,(3,3),(0.,1.),.UNSPECIFIED.);
#434=B_SPLINE_CURVE_WITH_KNOTS('',2,(#83269,#83270,#83271),
 .UNSPECIFIED.,.F.,.F.,(3,3),(0.,1.),.UNSPECIFIED.);
#435=B_SPLINE_CURVE_WITH_KNOTS('',2,(#83279,#83280,#83281),
 .UNSPECIFIED.,.F.,.F.,(3,3),(0.,1.),.UNSPECIFIED.);
#436=B_SPLINE_CURVE_WITH_KNOTS('',2,(#83284,#83285,#83286),
 .UNSPECIFIED.,.F.,.F.,(3,3),(0.,1.),.UNSPECIFIED.);
#437=B_SPLINE_CURVE_WITH_KNOTS('',2,(#83293,#83294,#83295),
 .UNSPECIFIED.,.F.,.F.,(3,3),(0.,1.),.UNSPECIFIED.);
#438=B_SPLINE_CURVE_WITH_KNOTS('',2,(#83296,#83297,#83298),
 .UNSPECIFIED.,.F.,.F.,(3,3),(0.,1.),.UNSPECIFIED.);
#439=B_SPLINE_CURVE_WITH_KNOTS('',2,(#83418,#83419,#83420),
 .UNSPECIFIED.,.F.,.F.,(3,3),(0.,1.),.UNSPECIFIED.);
#440=B_SPLINE_CURVE_WITH_KNOTS('',2,(#83424,#83425,#83426),
 .UNSPECIFIED.,.F.,.F.,(3,3),(0.,1.),.UNSPECIFIED.);
#441=B_SPLINE_CURVE_WITH_KNOTS('',2,(#83435,#83436,#83437),
 .UNSPECIFIED.,.F.,.F.,(3,3),(0.,1.),.UNSPECIFIED.);
#442=B_SPLINE_CURVE_WITH_KNOTS('',2,(#83440,#83441,#83442),
 .UNSPECIFIED.,.F.,.F.,(3,3),(0.,1.),.UNSPECIFIED.);
#443=B_SPLINE_CURVE_WITH_KNOTS('',2,(#83450,#83451,#83452),
 .UNSPECIFIED.,.F.,.F.,(3,3),(0.,1.),.UNSPECIFIED.);
#444=B_SPLINE_CURVE_WITH_KNOTS('',2,(#83455,#83456,#83457),
 .UNSPECIFIED.,.F.,.F.,(3,3),(0.,1.),.UNSPECIFIED.);
#445=B_SPLINE_CURVE_WITH_KNOTS('',2,(#83465,#83466,#83467),
 .UNSPECIFIED.,.F.,.F.,(3,3),(0.,1.),.UNSPECIFIED.);
#446=B_SPLINE_CURVE_WITH_KNOTS('',2,(#83470,#83471,#83472),
 .UNSPECIFIED.,.F.,.F.,(3,3),(0.,1.),.UNSPECIFIED.);
#447=B_SPLINE_CURVE_WITH_KNOTS('',2,(#83480,#83481,#83482),
 .UNSPECIFIED.,.F.,.F.,(3,3),(0.,1.),.UNSPECIFIED.);
#448=B_SPLINE_CURVE_WITH_KNOTS('',2,(#83485,#83486,#83487),
 .UNSPECIFIED.,.F.,.F.,(3,3),(0.,1.),.UNSPECIFIED.);
#449=B_SPLINE_CURVE_WITH_KNOTS('',2,(#83495,#83496,#83497),
 .UNSPECIFIED.,.F.,.F.,(3,3),(0.,1.),.UNSPECIFIED.);
#450=B_SPLINE_CURVE_WITH_KNOTS('',2,(#83500,#83501,#83502),
 .UNSPECIFIED.,.F.,.F.,(3,3),(0.,1.),.UNSPECIFIED.);
#451=B_SPLINE_CURVE_WITH_KNOTS('',2,(#83510,#83511,#83512),
 .UNSPECIFIED.,.F.,.F.,(3,3),(0.,1.),.UNSPECIFIED.);
#452=B_SPLINE_CURVE_WITH_KNOTS('',2,(#83515,#83516,#83517),
 .UNSPECIFIED.,.F.,.F.,(3,3),(0.,1.),.UNSPECIFIED.);
#453=B_SPLINE_CURVE_WITH_KNOTS('',2,(#83525,#83526,#83527),
 .UNSPECIFIED.,.F.,.F.,(3,3),(0.,1.),.UNSPECIFIED.);
#454=B_SPLINE_CURVE_WITH_KNOTS('',2,(#83530,#83531,#83532),
 .UNSPECIFIED.,.F.,.F.,(3,3),(0.,1.),.UNSPECIFIED.);
#455=B_SPLINE_CURVE_WITH_KNOTS('',2,(#83557,#83558,#83559),
 .UNSPECIFIED.,.F.,.F.,(3,3),(0.,1.),.UNSPECIFIED.);
#456=B_SPLINE_CURVE_WITH_KNOTS('',2,(#83560,#83561,#83562),
 .UNSPECIFIED.,.F.,.F.,(3,3),(0.,1.),.UNSPECIFIED.);
#457=B_SPLINE_CURVE_WITH_KNOTS('',2,(#83580,#83581,#83582),
 .UNSPECIFIED.,.F.,.F.,(3,3),(0.,1.),.UNSPECIFIED.);
#458=B_SPLINE_CURVE_WITH_KNOTS('',2,(#83585,#83586,#83587),
 .UNSPECIFIED.,.F.,.F.,(3,3),(0.,1.),.UNSPECIFIED.);
#459=B_SPLINE_CURVE_WITH_KNOTS('',2,(#83595,#83596,#83597),
 .UNSPECIFIED.,.F.,.F.,(3,3),(0.,1.),.UNSPECIFIED.);
#460=B_SPLINE_CURVE_WITH_KNOTS('',2,(#83600,#83601,#83602),
 .UNSPECIFIED.,.F.,.F.,(3,3),(0.,1.),.UNSPECIFIED.);
#461=B_SPLINE_CURVE_WITH_KNOTS('',2,(#83610,#83611,#83612),
 .UNSPECIFIED.,.F.,.F.,(3,3),(0.,1.),.UNSPECIFIED.);
#462=B_SPLINE_CURVE_WITH_KNOTS('',2,(#83615,#83616,#83617),
 .UNSPECIFIED.,.F.,.F.,(3,3),(0.,1.),.UNSPECIFIED.);
#463=B_SPLINE_CURVE_WITH_KNOTS('',2,(#83625,#83626,#83627),
 .UNSPECIFIED.,.F.,.F.,(3,3),(0.,1.),.UNSPECIFIED.);
#464=B_SPLINE_CURVE_WITH_KNOTS('',2,(#83630,#83631,#83632),
 .UNSPECIFIED.,.F.,.F.,(3,3),(0.,1.),.UNSPECIFIED.);
#465=B_SPLINE_CURVE_WITH_KNOTS('',2,(#83658,#83659,#83660),
 .UNSPECIFIED.,.F.,.F.,(3,3),(0.,1.),.UNSPECIFIED.);
#466=B_SPLINE_CURVE_WITH_KNOTS('',2,(#83663,#83664,#83665),
 .UNSPECIFIED.,.F.,.F.,(3,3),(0.,1.),.UNSPECIFIED.);
#467=B_SPLINE_CURVE_WITH_KNOTS('',2,(#83673,#83674,#83675),
 .UNSPECIFIED.,.F.,.F.,(3,3),(0.,1.),.UNSPECIFIED.);
#468=B_SPLINE_CURVE_WITH_KNOTS('',2,(#83678,#83679,#83680),
 .UNSPECIFIED.,.F.,.F.,(3,3),(0.,1.),.UNSPECIFIED.);
#469=B_SPLINE_CURVE_WITH_KNOTS('',2,(#83688,#83689,#83690),
 .UNSPECIFIED.,.F.,.F.,(3,3),(0.,1.),.UNSPECIFIED.);
#470=B_SPLINE_CURVE_WITH_KNOTS('',2,(#83693,#83694,#83695),
 .UNSPECIFIED.,.F.,.F.,(3,3),(0.,1.),.UNSPECIFIED.);
#471=B_SPLINE_CURVE_WITH_KNOTS('',2,(#83703,#83704,#83705),
 .UNSPECIFIED.,.F.,.F.,(3,3),(0.,1.),.UNSPECIFIED.);
#472=B_SPLINE_CURVE_WITH_KNOTS('',2,(#83708,#83709,#83710),
 .UNSPECIFIED.,.F.,.F.,(3,3),(0.,1.),.UNSPECIFIED.);
#473=B_SPLINE_CURVE_WITH_KNOTS('',2,(#83718,#83719,#83720),
 .UNSPECIFIED.,.F.,.F.,(3,3),(0.,1.),.UNSPECIFIED.);
#474=B_SPLINE_CURVE_WITH_KNOTS('',2,(#83723,#83724,#83725),
 .UNSPECIFIED.,.F.,.F.,(3,3),(0.,1.),.UNSPECIFIED.);
#475=B_SPLINE_CURVE_WITH_KNOTS('',2,(#83733,#83734,#83735),
 .UNSPECIFIED.,.F.,.F.,(3,3),(0.,1.),.UNSPECIFIED.);
#476=B_SPLINE_CURVE_WITH_KNOTS('',2,(#83738,#83739,#83740),
 .UNSPECIFIED.,.F.,.F.,(3,3),(0.,1.),.UNSPECIFIED.);
#477=B_SPLINE_CURVE_WITH_KNOTS('',2,(#83748,#83749,#83750),
 .UNSPECIFIED.,.F.,.F.,(3,3),(0.,1.),.UNSPECIFIED.);
#478=B_SPLINE_CURVE_WITH_KNOTS('',2,(#83753,#83754,#83755),
 .UNSPECIFIED.,.F.,.F.,(3,3),(0.,1.),.UNSPECIFIED.);
#479=B_SPLINE_CURVE_WITH_KNOTS('',3,(#84087,#84088,#84089,#84090,#84091,
#84092,#84093,#84094,#84095,#84096),.UNSPECIFIED.,.F.,.F.,(4,3,3,4),(-4.0932327200247,
-3.97004432054779,-2.97753324041084,-2.06652207565086),.UNSPECIFIED.);
#480=B_SPLINE_CURVE_WITH_KNOTS('',3,(#84099,#84100,#84101,#84102,#84103,
#84104,#84105,#84106,#84107,#84108),.UNSPECIFIED.,.F.,.F.,(4,3,3,4),(0.,
0.496255540068463,0.992511080136944,1.11488200921589),.UNSPECIFIED.);
#481=B_SPLINE_CURVE_WITH_KNOTS('',3,(#84113,#84114,#84115,#84116,#84117,
#84118,#84119,#84120,#84121,#84122,#84123,#84124,#84125,#84126,#84127,#84128,
#84129,#84130,#84131,#84132,#84133,#84134),.UNSPECIFIED.,.F.,.F.,(4,3,3,
3,3,3,3,4),(-10.3764180272043,-9.92511080136948,-8.93259972123253,-7.94008864109558,
-6.94757756095863,-5.95506648082169,-4.96255540068474,-4.0932327200247),
 .UNSPECIFIED.);
#482=B_SPLINE_CURVE_WITH_KNOTS('',3,(#84135,#84136,#84137,#84138,#84139,
#84140,#84141,#84142,#84143,#84144,#84145,#84146,#84147,#84148,#84149,#84150,
#84151,#84152,#84153,#84154,#84155,#84156),.UNSPECIFIED.,.F.,.F.,(4,3,3,
3,3,3,3,4),(1.11488200921589,1.98502216027389,2.97753324041084,3.97004432054779,
4.96255540068474,5.95506648082169,6.94757756095864,7.39806731639547),
 .UNSPECIFIED.);
#483=B_SPLINE_CURVE_WITH_KNOTS('',3,(#84161,#84162,#84163,#84164,#84165,
#84166,#84167,#84168,#84169,#84170,#84171,#84172,#84173,#84174,#84175,#84176,
#84177,#84178,#84179,#84180,#84181,#84182),.UNSPECIFIED.,.F.,.F.,(4,3,3,
3,3,3,3,4),(-16.6596033343839,-15.8801772821912,-14.8876662020542,-13.8951551219173,
-12.9026440417803,-11.9101329616434,-10.9176218815064,-10.3764180272043),
 .UNSPECIFIED.);
#484=B_SPLINE_CURVE_WITH_KNOTS('',3,(#84183,#84184,#84185,#84186,#84187,
#84188,#84189,#84190,#84191,#84192,#84193,#84194,#84195,#84196,#84197,#84198,
#84199,#84200,#84201,#84202,#84203,#84204),.UNSPECIFIED.,.F.,.F.,(4,3,3,
3,3,3,3,4),(7.39806731639547,7.94008864109559,8.93259972123253,9.92511080136948,
10.9176218815064,11.9101329616434,12.9026440417803,13.681252623575),
 .UNSPECIFIED.);
#485=B_SPLINE_CURVE_WITH_KNOTS('',3,(#84209,#84210,#84211,#84212,#84213,
#84214,#84215,#84216,#84217,#84218,#84219,#84220,#84221,#84222,#84223,#84224,
#84225,#84226,#84227,#84228,#84229,#84230,#84231,#84232,#84233),
 .UNSPECIFIED.,.F.,.F.,(4,3,3,3,3,3,3,3,4),(-22.9427886415635,-22.8277548431498,
-21.8352437630129,-20.8427326828759,-19.850221602739,-18.857710522602,-17.8651994424651,
-16.8726883623281,-16.6596033343839),.UNSPECIFIED.);
#486=B_SPLINE_CURVE_WITH_KNOTS('',3,(#84234,#84235,#84236,#84237,#84238,
#84239,#84240,#84241,#84242,#84243,#84244,#84245,#84246,#84247,#84248,#84249,
#84250,#84251,#84252,#84253,#84254,#84255,#84256,#84257,#84258),
 .UNSPECIFIED.,.F.,.F.,(4,3,3,3,3,3,3,3,4),(13.681252623575,13.8951551219173,
14.8876662020542,15.8801772821912,16.8726883623281,17.8651994424651,18.857710522602,
19.8502216027389,19.9644379307546),.UNSPECIFIED.);
#487=B_SPLINE_CURVE_WITH_KNOTS('',3,(#84263,#84264,#84265,#84266,#84267,
#84268,#84269,#84270,#84271,#84272,#84273,#84274,#84275,#84276,#84277,#84278,
#84279,#84280,#84281,#84282,#84283,#84284),.UNSPECIFIED.,.F.,.F.,(4,3,3,
3,3,3,3,4),(-29.225973948743,-28.7828213239715,-27.7903102438345,-26.7977991636976,
-25.8052880835606,-24.8127770034237,-23.8202659232867,-22.9427886415635),
 .UNSPECIFIED.);
#488=B_SPLINE_CURVE_WITH_KNOTS('',3,(#84285,#84286,#84287,#84288,#84289,
#84290,#84291,#84292,#84293,#84294,#84295,#84296,#84297,#84298,#84299,#84300,
#84301,#84302,#84303,#84304,#84305,#84306),.UNSPECIFIED.,.F.,.F.,(4,3,3,
3,3,3,3,4),(19.9644379307546,20.8427326828759,21.8352437630128,22.8277548431498,
23.8202659232867,24.8127770034237,25.8052880835606,26.2476232379342),
 .UNSPECIFIED.);
#489=B_SPLINE_CURVE_WITH_KNOTS('',3,(#84311,#84312,#84313,#84314,#84315,
#84316,#84317,#84318,#84319,#84320,#84321,#84322,#84323,#84324,#84325,#84326,
#84327,#84328,#84329,#84330,#84331,#84332),.UNSPECIFIED.,.F.,.F.,(4,3,3,
3,3,3,3,4),(-35.5091592559226,-34.7378878047932,-33.7453767246562,-32.7528656445193,
-31.7603545643823,-30.7678434842454,-29.7753324041084,-29.225973948743),
 .UNSPECIFIED.);
#490=B_SPLINE_CURVE_WITH_KNOTS('',3,(#84333,#84334,#84335,#84336,#84337,
#84338,#84339,#84340,#84341,#84342,#84343,#84344,#84345,#84346,#84347,#84348,
#84349,#84350,#84351,#84352,#84353,#84354),.UNSPECIFIED.,.F.,.F.,(4,3,3,
3,3,3,3,4),(26.2476232379342,26.7977991636976,27.7903102438345,28.7828213239715,
29.7753324041084,30.7678434842454,31.7603545643823,32.5308085451138),
 .UNSPECIFIED.);
#491=B_SPLINE_CURVE_WITH_KNOTS('',3,(#84359,#84360,#84361,#84362,#84363,
#84364,#84365,#84366,#84367,#84368,#84369,#84370,#84371,#84372,#84373,#84374,
#84375,#84376,#84377,#84378,#84379,#84380,#84381,#84382,#84383),
 .UNSPECIFIED.,.F.,.F.,(4,3,3,3,3,3,3,3,4),(-41.7923445631022,-41.6854653657518,
-40.6929542856149,-39.7004432054779,-38.707932125341,-37.715421045204,-36.7229099650671,
-35.7303988849301,-35.5091592559226),.UNSPECIFIED.);
#492=B_SPLINE_CURVE_WITH_KNOTS('',3,(#84384,#84385,#84386,#84387,#84388,
#84389,#84390,#84391,#84392,#84393,#84394,#84395,#84396,#84397,#84398,#84399,
#84400,#84401,#84402,#84403,#84404,#84405,#84406,#84407,#84408),
 .UNSPECIFIED.,.F.,.F.,(4,3,3,3,3,3,3,3,4),(32.5308085451138,32.7528656445192,
33.7453767246562,34.7378878047931,35.7303988849301,36.722909965067,37.715421045204,
38.7079321253409,38.8139938522934),.UNSPECIFIED.);
#493=B_SPLINE_CURVE_WITH_KNOTS('',3,(#84413,#84414,#84415,#84416,#84417,
#84418,#84419,#84420,#84421,#84422,#84423,#84424,#84425,#84426,#84427,#84428,
#84429,#84430,#84431,#84432,#84433,#84434),.UNSPECIFIED.,.F.,.F.,(4,3,3,
3,3,3,3,4),(-48.0755298702818,-47.6405318465735,-46.6480207664365,-45.6555096862996,
-44.6629986061626,-43.6704875260257,-42.6779764458888,-41.7923445631022),
 .UNSPECIFIED.);
#494=B_SPLINE_CURVE_WITH_KNOTS('',3,(#84435,#84436,#84437,#84438,#84439,
#84440,#84441,#84442,#84443,#84444,#84445,#84446,#84447,#84448,#84449,#84450,
#84451,#84452,#84453,#84454,#84455,#84456),.UNSPECIFIED.,.F.,.F.,(4,3,3,
3,3,3,3,4),(38.8139938522934,39.7004432054779,40.6929542856148,41.6854653657518,
42.6779764458887,43.6704875260257,44.6629986061626,45.097179159473),
 .UNSPECIFIED.);
#495=B_SPLINE_CURVE_WITH_KNOTS('',3,(#84461,#84462,#84463,#84464,#84465,
#84466,#84467,#84468,#84469,#84470,#84471,#84472,#84473,#84474,#84475,#84476,
#84477,#84478,#84479,#84480,#84481,#84482),.UNSPECIFIED.,.F.,.F.,(4,3,3,
3,3,3,3,4),(-54.3587151774614,-53.5955983273952,-52.6030872472582,-51.6105761671213,
-50.6180650869843,-49.6255540068474,-48.6330429267104,-48.0755298702818),
 .UNSPECIFIED.);
#496=B_SPLINE_CURVE_WITH_KNOTS('',3,(#84483,#84484,#84485,#84486,#84487,
#84488,#84489,#84490,#84491,#84492,#84493,#84494,#84495,#84496,#84497,#84498,
#84499,#84500,#84501,#84502,#84503,#84504),.UNSPECIFIED.,.F.,.F.,(4,3,3,
3,3,3,3,4),(45.097179159473,45.6555096862996,46.6480207664365,47.6405318465735,
48.6330429267104,49.6255540068474,50.6180650869843,51.3803644666526),
 .UNSPECIFIED.);
#497=B_SPLINE_CURVE_WITH_KNOTS('',3,(#84509,#84510,#84511,#84512,#84513,
#84514,#84515,#84516,#84517,#84518,#84519,#84520,#84521,#84522,#84523,#84524,
#84525,#84526,#84527,#84528,#84529,#84530,#84531,#84532,#84533),
 .UNSPECIFIED.,.F.,.F.,(4,3,3,3,3,3,3,3,4),(-60.641900484641,-60.5431758883538,
-59.5506648082169,-58.5581537280799,-57.565642647943,-56.573131567806,-55.5806204876691,
-54.5881094075321,-54.3587151774614),.UNSPECIFIED.);
#498=B_SPLINE_CURVE_WITH_KNOTS('',3,(#84534,#84535,#84536,#84537,#84538,
#84539,#84540,#84541,#84542,#84543,#84544,#84545,#84546,#84547,#84548,#84549,
#84550,#84551,#84552,#84553,#84554,#84555,#84556,#84557,#84558),
 .UNSPECIFIED.,.F.,.F.,(4,3,3,3,3,3,3,3,4),(51.3803644666526,51.6105761671213,
52.6030872472582,53.5955983273952,54.5881094075321,55.5806204876691,56.573131567806,
57.565642647943,57.6635497738322),.UNSPECIFIED.);
#499=B_SPLINE_CURVE_WITH_KNOTS('',3,(#84563,#84564,#84565,#84566,#84567,
#84568,#84569,#84570,#84571,#84572,#84573,#84574,#84575,#84576,#84577,#84578,
#84579,#84580,#84581,#84582,#84583,#84584),.UNSPECIFIED.,.F.,.F.,(4,3,3,
3,3,3,3,4),(-66.9250857918206,-66.4982423691755,-65.5057312890386,-64.5132202089016,
-63.5207091287647,-62.5281980486277,-61.5356869684908,-60.641900484641),
 .UNSPECIFIED.);
#500=B_SPLINE_CURVE_WITH_KNOTS('',3,(#84585,#84586,#84587,#84588,#84589,
#84590,#84591,#84592,#84593,#84594,#84595,#84596,#84597,#84598,#84599,#84600,
#84601,#84602,#84603,#84604,#84605,#84606),.UNSPECIFIED.,.F.,.F.,(4,3,3,
3,3,3,3,4),(57.6635497738322,58.5581537280799,59.5506648082169,60.5431758883538,
61.5356869684908,62.5281980486277,63.5207091287646,63.9467350810118),
 .UNSPECIFIED.);
#501=B_SPLINE_CURVE_WITH_KNOTS('',3,(#84611,#84612,#84613,#84614,#84615,
#84616,#84617,#84618,#84619,#84620,#84621,#84622,#84623,#84624,#84625,#84626,
#84627,#84628,#84629,#84630,#84631,#84632),.UNSPECIFIED.,.F.,.F.,(4,3,3,
3,3,3,3,4),(-73.2082710990002,-72.4533088499972,-71.4607977698602,-70.4682866897233,
-69.4757756095863,-68.4832645294494,-67.4907534493124,-66.9250857918206),
 .UNSPECIFIED.);
#502=B_SPLINE_CURVE_WITH_KNOTS('',3,(#84633,#84634,#84635,#84636,#84637,
#84638,#84639,#84640,#84641,#84642,#84643,#84644,#84645,#84646,#84647,#84648,
#84649,#84650,#84651,#84652,#84653,#84654),.UNSPECIFIED.,.F.,.F.,(4,3,3,
3,3,3,3,4),(63.9467350810118,64.5132202089016,65.5057312890385,66.4982423691755,
67.4907534493124,68.4832645294494,69.4757756095863,70.2299203881914),
 .UNSPECIFIED.);
#503=B_SPLINE_CURVE_WITH_KNOTS('',3,(#84659,#84660,#84661,#84662,#84663,
#84664,#84665,#84666,#84667,#84668,#84669,#84670,#84671,#84672,#84673,#84674,
#84675,#84676,#84677,#84678,#84679,#84680,#84681,#84682,#84683),
 .UNSPECIFIED.,.F.,.F.,(4,3,3,3,3,3,3,3,4),(-79.4914564061798,-79.4008864109558,
-78.4083753308189,-77.4158642506819,-76.423353170545,-75.430842090408,-74.4383310102711,
-73.4458199301341,-73.2082710990002),.UNSPECIFIED.);
#504=B_SPLINE_CURVE_WITH_KNOTS('',3,(#84684,#84685,#84686,#84687,#84688,
#84689,#84690,#84691,#84692,#84693,#84694,#84695,#84696,#84697,#84698,#84699,
#84700,#84701,#84702,#84703,#84704,#84705,#84706,#84707,#84708),
 .UNSPECIFIED.,.F.,.F.,(4,3,3,3,3,3,3,3,4),(70.2299203881914,70.4682866897233,
71.4607977698602,72.4533088499972,73.4458199301341,74.4383310102711,75.430842090408,
76.423353170545,76.513105695371),.UNSPECIFIED.);
#505=B_SPLINE_CURVE_WITH_KNOTS('',3,(#84713,#84714,#84715,#84716,#84717,
#84718,#84719,#84720,#84721,#84722,#84723,#84724,#84725,#84726,#84727,#84728,
#84729,#84730,#84731,#84732,#84733,#84734),.UNSPECIFIED.,.F.,.F.,(4,3,3,
3,3,3,3,4),(-85.7746417133594,-85.3559528917775,-84.3634418116406,-83.3709307315036,
-82.3784196513666,-81.3859085712297,-80.3933974910928,-79.4914564061798),
 .UNSPECIFIED.);
#506=B_SPLINE_CURVE_WITH_KNOTS('',3,(#84735,#84736,#84737,#84738,#84739,
#84740,#84741,#84742,#84743,#84744,#84745,#84746,#84747,#84748,#84749,#84750,
#84751,#84752,#84753,#84754,#84755,#84756),.UNSPECIFIED.,.F.,.F.,(4,3,3,
3,3,3,3,4),(76.513105695371,77.4158642506819,78.4083753308189,79.4008864109558,
80.3933974910927,81.3859085712297,82.3784196513666,82.7962910025506),
 .UNSPECIFIED.);
#507=B_SPLINE_CURVE_WITH_KNOTS('',3,(#84761,#84762,#84763,#84764,#84765,
#84766,#84767,#84768,#84769,#84770,#84771,#84772,#84773,#84774,#84775,#84776,
#84777,#84778,#84779,#84780,#84781,#84782),.UNSPECIFIED.,.F.,.F.,(4,3,3,
3,3,3,3,4),(-92.057827020539,-91.3110193725992,-90.3185082924622,-89.3259972123253,
-88.3334861321883,-87.3409750520514,-86.3484639719144,-85.7746417133594),
 .UNSPECIFIED.);
#508=B_SPLINE_CURVE_WITH_KNOTS('',3,(#84783,#84784,#84785,#84786,#84787,
#84788,#84789,#84790,#84791,#84792,#84793,#84794,#84795,#84796,#84797,#84798,
#84799,#84800,#84801,#84802,#84803,#84804),.UNSPECIFIED.,.F.,.F.,(4,3,3,
3,3,3,3,4),(82.7962910025506,83.3709307315036,84.3634418116405,85.3559528917775,
86.3484639719144,87.3409750520514,88.3334861321883,89.0794763097301),
 .UNSPECIFIED.);
#509=B_SPLINE_CURVE_WITH_KNOTS('',3,(#84809,#84810,#84811,#84812,#84813,
#84814,#84815,#84816,#84817,#84818,#84819,#84820,#84821,#84822,#84823,#84824,
#84825,#84826,#84827,#84828,#84829,#84830,#84831,#84832,#84833),
 .UNSPECIFIED.,.F.,.F.,(4,3,3,3,3,3,3,3,4),(-98.3410123277186,-98.2585969335579,
-97.2660858534209,-96.2735747732839,-95.281063693147,-94.28855261301,-93.2960415328731,
-92.3035304527361,-92.057827020539),.UNSPECIFIED.);
#510=B_SPLINE_CURVE_WITH_KNOTS('',3,(#84834,#84835,#84836,#84837,#84838,
#84839,#84840,#84841,#84842,#84843,#84844,#84845,#84846,#84847,#84848,#84849,
#84850,#84851,#84852,#84853,#84854,#84855,#84856,#84857,#84858),
 .UNSPECIFIED.,.F.,.F.,(4,3,3,3,3,3,3,3,4),(89.0794763097301,89.3259972123253,
90.3185082924622,91.3110193725992,92.3035304527361,93.2960415328731,94.28855261301,
95.2810636931469,95.3626616169097),.UNSPECIFIED.);
#511=B_SPLINE_CURVE_WITH_KNOTS('',3,(#84864,#84865,#84866,#84867),
 .UNSPECIFIED.,.F.,.F.,(4,4),(109.955742875643,110.784338646242),
 .UNSPECIFIED.);
#512=B_SPLINE_CURVE_WITH_KNOTS('',3,(#84873,#84874,#84875,#84876,#84877,
#84878,#84879,#84880,#84881,#84882,#84883),.UNSPECIFIED.,.F.,.F.,(4,1,1,
1,1,1,1,1,4),(103.672557568463,103.91826100066,104.910772080797,105.903283160934,
106.895794241071,107.888305321208,108.880816401345,109.873327481482,109.955742875643),
 .UNSPECIFIED.);
#513=B_SPLINE_CURVE_WITH_KNOTS('',3,(#84886,#84887,#84888,#84889,#84890,
#84891,#84892,#84893,#84894,#84895),.UNSPECIFIED.,.F.,.F.,(4,1,1,1,1,1,
1,4),(103.672557568463,104.583470724837,105.575981804974,106.568492885111,
107.561003965248,108.553515045385,109.049770585453,109.546026125522),
 .UNSPECIFIED.);
#514=B_SPLINE_CURVE_WITH_KNOTS('',3,(#84900,#84901,#84902,#84903,#84904,
#84905,#84906,#84907,#84908,#84909),.UNSPECIFIED.,.F.,.F.,(4,1,1,1,1,1,
1,4),(97.3893722612836,97.9631945198386,98.9557055999756,99.9482166801125,
100.940727760249,101.933238840386,102.925749920523,103.672557568463),
 .UNSPECIFIED.);
#515=B_SPLINE_CURVE_WITH_KNOTS('',3,(#84910,#84911,#84912,#84913,#84914,
#84915,#84916,#84917,#84918,#84919,#84920),.UNSPECIFIED.,.F.,.F.,(4,1,1,
1,1,1,1,1,4),(97.3893722612836,97.6358931638786,98.6284042440155,99.6209153241525,
100.613426404289,101.605937484426,102.598448564563,103.5909596447,103.672557568463),
 .UNSPECIFIED.);
#516=B_SPLINE_CURVE_WITH_KNOTS('',3,(#84925,#84926,#84927,#84928,#84929,
#84930,#84931,#84932,#84933,#84934),.UNSPECIFIED.,.F.,.F.,(4,1,1,1,1,1,
1,4),(91.106186954104,92.0081280390169,93.0006391191539,93.9931501992908,
94.9856612794278,95.9781723595647,96.9706834397017,97.3893722612836),
 .UNSPECIFIED.);
#517=B_SPLINE_CURVE_WITH_KNOTS('',3,(#84935,#84936,#84937,#84938,#84939,
#84940,#84941,#84942,#84943,#84944),.UNSPECIFIED.,.F.,.F.,(4,1,1,1,1,1,
1,4),(91.106186954104,91.6808266830569,92.6733377631939,93.6658488433308,
94.6583599234677,95.6508710036047,96.6433820837416,97.3893722612836),
 .UNSPECIFIED.);
#518=B_SPLINE_CURVE_WITH_KNOTS('',3,(#84949,#84950,#84951,#84952,#84953,
#84954,#84955,#84956,#84957,#84958,#84959),.UNSPECIFIED.,.F.,.F.,(4,1,1,
1,1,1,1,1,4),(84.8230016469244,85.0605504780583,86.0530615581953,87.0455726383322,
88.0380837184692,89.0305947986061,90.0231058787431,91.01561695888,91.106186954104),
 .UNSPECIFIED.);
#519=B_SPLINE_CURVE_WITH_KNOTS('',3,(#84960,#84961,#84962,#84963,#84964,
#84965,#84966,#84967,#84968,#84969),.UNSPECIFIED.,.F.,.F.,(4,1,1,1,1,1,
1,4),(84.8230016469244,85.7257602022352,86.7182712823722,87.7107823625091,
88.7032934426461,89.695804522783,90.68831560292,91.106186954104),
 .UNSPECIFIED.);
#520=B_SPLINE_CURVE_WITH_KNOTS('',3,(#84974,#84975,#84976,#84977,#84978,
#84979,#84980,#84981,#84982,#84983),.UNSPECIFIED.,.F.,.F.,(4,1,1,1,1,1,
1,4),(78.5398163397448,79.1054839972366,80.0979950773736,81.0905061575105,
82.0830172376475,83.0755283177844,84.0680393979214,84.8230016469244),
 .UNSPECIFIED.);
#521=B_SPLINE_CURVE_WITH_KNOTS('',3,(#84984,#84985,#84986,#84987,#84988,
#84989,#84990,#84991,#84992,#84993,#84994),.UNSPECIFIED.,.F.,.F.,(4,1,1,
1,1,1,1,1,4),(78.5398163397448,78.7781826412766,79.7706937214135,80.7632048015505,
81.7557158816874,82.7482269618244,83.7407380419613,84.7332491220983,84.8230016469244),
 .UNSPECIFIED.);
#522=B_SPLINE_CURVE_WITH_KNOTS('',3,(#84999,#85000,#85001,#85002,#85003,
#85004,#85005,#85006,#85007,#85008),.UNSPECIFIED.,.F.,.F.,(4,1,1,1,1,1,
1,4),(72.2566310325652,73.1504175164149,74.1429285965519,75.1354396766888,
76.1279507568258,77.1204618369627,78.1129729170997,78.5398163397448),
 .UNSPECIFIED.);
#523=B_SPLINE_CURVE_WITH_KNOTS('',3,(#85009,#85010,#85011,#85012,#85013,
#85014,#85015,#85016,#85017,#85018),.UNSPECIFIED.,.F.,.F.,(4,1,1,1,1,1,
1,4),(72.2566310325652,72.8231161604549,73.8156272405919,74.8081383207288,
75.8006494008658,76.7931604810027,77.7856715611396,78.5398163397448),
 .UNSPECIFIED.);
#524=B_SPLINE_CURVE_WITH_KNOTS('',3,(#85023,#85024,#85025,#85026,#85027,
#85028,#85029,#85030,#85031,#85032,#85033),.UNSPECIFIED.,.F.,.F.,(4,1,1,
1,1,1,1,1,4),(65.9734457253856,66.2028399554563,67.1953510355932,68.1878621157302,
69.1803731958671,70.1728842760041,71.165395356141,72.157906436278,72.2566310325652),
 .UNSPECIFIED.);
#525=B_SPLINE_CURVE_WITH_KNOTS('',3,(#85034,#85035,#85036,#85037,#85038,
#85039,#85040,#85041,#85042,#85043),.UNSPECIFIED.,.F.,.F.,(4,1,1,1,1,1,
1,4),(65.9734457253856,66.8680496796332,67.8605607597702,68.8530718399071,
69.8455829200441,70.838094000181,71.830605080318,72.2566310325652),
 .UNSPECIFIED.);
#526=B_SPLINE_CURVE_WITH_KNOTS('',3,(#85048,#85049,#85050,#85051,#85052,
#85053,#85054,#85055,#85056,#85057),.UNSPECIFIED.,.F.,.F.,(4,1,1,1,1,1,
1,4),(59.690260418206,60.2477734746346,61.2402845547716,62.2327956349085,
63.2253067150455,64.2178177951824,65.2103288753194,65.9734457253856),
 .UNSPECIFIED.);
#527=B_SPLINE_CURVE_WITH_KNOTS('',3,(#85058,#85059,#85060,#85061,#85062,
#85063,#85064,#85065,#85066,#85067,#85068),.UNSPECIFIED.,.F.,.F.,(4,1,1,
1,1,1,1,1,4),(59.690260418206,59.9204721186746,60.9129831988115,61.9054942789485,
62.8980053590854,63.8905164392224,64.8830275193593,65.8755385994963,65.9734457253856),
 .UNSPECIFIED.);
#528=B_SPLINE_CURVE_WITH_KNOTS('',3,(#85073,#85074,#85075,#85076,#85077,
#85078,#85079,#85080,#85081,#85082),.UNSPECIFIED.,.F.,.F.,(4,1,1,1,1,1,
1,4),(53.4070751110264,54.2927069938129,55.2852180739499,56.2777291540868,
57.2702402342238,58.2627513143607,59.2552623944977,59.690260418206),
 .UNSPECIFIED.);
#529=B_SPLINE_CURVE_WITH_KNOTS('',3,(#85083,#85084,#85085,#85086,#85087,
#85088,#85089,#85090,#85091,#85092),.UNSPECIFIED.,.F.,.F.,(4,1,1,1,1,1,
1,4),(53.4070751110264,53.9654056378529,54.9579167179898,55.9504277981268,
56.9429388782637,57.9354499584007,58.9279610385376,59.690260418206),
 .UNSPECIFIED.);
#530=B_SPLINE_CURVE_WITH_KNOTS('',3,(#85097,#85098,#85099,#85100,#85101,
#85102,#85103,#85104,#85105,#85106,#85107),.UNSPECIFIED.,.F.,.F.,(4,1,1,
1,1,1,1,1,4),(47.1238898038468,47.3451294328543,48.3376405129912,49.3301515931282,
50.3226626732651,51.3151737534021,52.307684833539,53.300195913676,53.4070751110264),
 .UNSPECIFIED.);
#531=B_SPLINE_CURVE_WITH_KNOTS('',3,(#85108,#85109,#85110,#85111,#85112,
#85113,#85114,#85115,#85116,#85117),.UNSPECIFIED.,.F.,.F.,(4,1,1,1,1,1,
1,4),(47.1238898038468,48.0103391570312,49.0028502371682,49.9953613173051,
50.9878723974421,51.980383477579,52.972894557716,53.4070751110264),
 .UNSPECIFIED.);
#532=B_SPLINE_CURVE_WITH_KNOTS('',3,(#85122,#85123,#85124,#85125,#85126,
#85127,#85128,#85129,#85130,#85131),.UNSPECIFIED.,.F.,.F.,(4,1,1,1,1,1,
1,4),(40.8407044966672,41.3900629520326,42.3825740321696,43.3750851123065,
44.3675961924435,45.3601072725804,46.3526183527174,47.1238898038468),
 .UNSPECIFIED.);
#533=B_SPLINE_CURVE_WITH_KNOTS('',3,(#85132,#85133,#85134,#85135,#85136,
#85137,#85138,#85139,#85140,#85141,#85142),.UNSPECIFIED.,.F.,.F.,(4,1,1,
1,1,1,1,1,4),(40.8407044966672,41.0627615960726,42.0552726762095,43.0477837563465,
44.0402948364834,45.0328059166204,46.0253169967573,47.0178280768943,47.1238898038468),
 .UNSPECIFIED.);
#534=B_SPLINE_CURVE_WITH_KNOTS('',3,(#85147,#85148,#85149,#85150,#85151,
#85152,#85153,#85154,#85155,#85156),.UNSPECIFIED.,.F.,.F.,(4,1,1,1,1,1,
1,4),(34.5575191894876,35.4349964712109,36.4275075513479,37.4200186314848,
38.4125297116218,39.4050407917587,40.3975518718957,40.8407044966672),
 .UNSPECIFIED.);
#535=B_SPLINE_CURVE_WITH_KNOTS('',3,(#85157,#85158,#85159,#85160,#85161,
#85162,#85163,#85164,#85165,#85166),.UNSPECIFIED.,.F.,.F.,(4,1,1,1,1,1,
1,4),(34.5575191894876,35.1076951152509,36.1002061953878,37.0927172755248,
38.0852283556617,39.0777394357987,40.0702505159356,40.8407044966672),
 .UNSPECIFIED.);
#536=B_SPLINE_CURVE_WITH_KNOTS('',3,(#85171,#85172,#85173,#85174,#85175,
#85176,#85177,#85178,#85179,#85180,#85181),.UNSPECIFIED.,.F.,.F.,(4,1,1,
1,1,1,1,1,4),(28.2743338823081,28.4874189102523,29.4799299903892,30.4724410705262,
31.4649521506631,32.4574632308001,33.449974310937,34.442485391074,34.5575191894876),
 .UNSPECIFIED.);
#537=B_SPLINE_CURVE_WITH_KNOTS('',3,(#85182,#85183,#85184,#85185,#85186,
#85187,#85188,#85189,#85190,#85191),.UNSPECIFIED.,.F.,.F.,(4,1,1,1,1,1,
1,4),(28.2743338823081,29.1526286344292,30.1451397145662,31.1376507947031,
32.1301618748401,33.122672954977,34.115184035114,34.5575191894876),
 .UNSPECIFIED.);
#538=B_SPLINE_CURVE_WITH_KNOTS('',3,(#85196,#85197,#85198,#85199,#85200,
#85201,#85202,#85203,#85204,#85205),.UNSPECIFIED.,.F.,.F.,(4,1,1,1,1,1,
1,4),(21.9911485751285,22.5323524294306,23.5248635095676,24.5173745897045,
25.5098856698415,26.5023967499784,27.4949078301153,28.2743338823081),
 .UNSPECIFIED.);
#539=B_SPLINE_CURVE_WITH_KNOTS('',3,(#85206,#85207,#85208,#85209,#85210,
#85211,#85212,#85213,#85214,#85215,#85216),.UNSPECIFIED.,.F.,.F.,(4,1,1,
1,1,1,1,1,4),(21.9911485751285,22.2050510734706,23.1975621536075,24.1900732337445,
25.1825843138814,26.1750953940184,27.1676064741553,28.1601175542923,28.2743338823081),
 .UNSPECIFIED.);
#540=B_SPLINE_CURVE_WITH_KNOTS('',3,(#85221,#85222,#85223,#85224,#85225,
#85226,#85227,#85228,#85229,#85230),.UNSPECIFIED.,.F.,.F.,(4,1,1,1,1,1,
1,4),(15.7079632679489,16.5772859486089,17.5697970287459,18.5623081088828,
19.5548191890198,20.5473302691567,21.5398413492937,21.9911485751285),
 .UNSPECIFIED.);
#541=B_SPLINE_CURVE_WITH_KNOTS('',3,(#85231,#85232,#85233,#85234,#85235,
#85236,#85237,#85238,#85239,#85240),.UNSPECIFIED.,.F.,.F.,(4,1,1,1,1,1,
1,4),(15.7079632679489,16.2499845926489,17.2424956727859,18.2350067529228,
19.2275178330597,20.2200289131967,21.2125399933336,21.9911485751285),
 .UNSPECIFIED.);
#542=B_SPLINE_CURVE_WITH_KNOTS('',3,(#85243,#85244,#85245,#85246,#85247,
#85248,#85249,#85250,#85251,#85252,#85253,#85254,#85255,#85256,#85257,#85258,
#85259,#85260,#85261,#85262,#85263,#85264,#85265,#85266,#85267,#85268,#85269,
#85270,#85271,#85272,#85273,#85274,#85275,#85276,#85277,#85278,#85279,#85280,
#85281,#85282,#85283,#85284,#85285,#85286,#85287,#85288,#85289,#85290,#85291,
#85292,#85293,#85294,#85295,#85296,#85297,#85298,#85299,#85300,#85301,#85302,
#85303,#85304,#85305,#85306,#85307,#85308,#85309,#85310,#85311,#85312,#85313,
#85314,#85315,#85316,#85317,#85318,#85319,#85320,#85321,#85322,#85323,#85324,
#85325,#85326,#85327,#85328,#85329,#85330,#85331,#85332,#85333,#85334,#85335,
#85336,#85337,#85338,#85339,#85340,#85341,#85342,#85343,#85344,#85345,#85346,
#85347,#85348),.UNSPECIFIED.,.F.,.F.,(4,3,3,3,3,3,3,3,3,3,3,3,3,3,3,3,3,
3,3,3,3,3,3,3,3,3,3,3,3,3,3,3,3,3,3,4),(-0.937740963081717,-0.904107646522432,
-0.866863955687421,-0.842197390067725,-0.832993449352449,-0.824789559002339,
-0.786675044092378,-0.747365526802366,-0.730167612987985,-0.721368607918277,
-0.713926887194103,-0.67422506805026,-0.633949893432139,-0.593512146517175,
-0.563183836330951,-0.549662025807026,-0.544150077215339,-0.502692185308048,
-0.472198905772281,-0.432024673306818,-0.391226520653541,-0.378538710027433,
-0.371922566564841,-0.366074525313514,-0.324929610892798,-0.282818014698314,
-0.241021666268101,-0.210893957984588,-0.197713085610552,-0.18926685442852,
-0.183259350799863,-0.140444090930293,-0.0970669920848681,-0.0537376549097892,
-0.0109807787802793,0.),.UNSPECIFIED.);
#543=B_SPLINE_CURVE_WITH_KNOTS('',3,(#85353,#85354,#85355,#85356,#85357,
#85358,#85359,#85360,#85361,#85362,#85363,#85364,#85365,#85366,#85367,#85368,
#85369,#85370,#85371,#85372,#85373,#85374,#85375,#85376,#85377,#85378,#85379,
#85380,#85381,#85382,#85383,#85384,#85385,#85386,#85387,#85388,#85389,#85390,
#85391,#85392,#85393,#85394,#85395,#85396,#85397,#85398,#85399,#85400,#85401,
#85402,#85403,#85404,#85405,#85406,#85407,#85408,#85409,#85410,#85411,#85412,
#85413,#85414,#85415,#85416,#85417,#85418,#85419,#85420,#85421,#85422,#85423,
#85424,#85425,#85426,#85427,#85428,#85429,#85430,#85431,#85432,#85433,#85434,
#85435,#85436,#85437,#85438,#85439,#85440,#85441,#85442,#85443,#85444,#85445,
#85446,#85447,#85448,#85449,#85450,#85451,#85452,#85453,#85454,#85455,#85456,
#85457,#85458),.UNSPECIFIED.,.F.,.F.,(4,3,3,3,3,3,3,3,3,3,3,3,3,3,3,3,3,
3,3,3,3,3,3,3,3,3,3,3,3,3,3,3,3,3,3,4),(-0.93397589402314,-0.893931319943522,
-0.850589364476838,-0.824132124098182,-0.808860826581905,-0.801881936601205,
-0.75913893284388,-0.717655756040688,-0.698300481629254,-0.686886922860203,
-0.681304646666429,-0.639280691781047,-0.597411580416329,-0.554877064916833,
-0.522976178292211,-0.510638772677517,-0.502211774582474,-0.496747396852542,
-0.456670538628237,-0.427273518418344,-0.386682137037577,-0.346195485729097,
-0.330880632953443,-0.325030908129725,-0.285554599290461,-0.246235559529426,
-0.208611124605633,-0.182534734029929,-0.16943344784353,-0.162203266198673,
-0.156994942118918,-0.117746206589189,-0.0795115062646132,-0.0397557531323066,
-0.00273238855256798,0.),.UNSPECIFIED.);
#544=B_SPLINE_CURVE_WITH_KNOTS('',3,(#85887,#85888,#85889,#85890,#85891,
#85892,#85893,#85894,#85895,#85896,#85897,#85898,#85899),.UNSPECIFIED.,
 .F.,.F.,(4,3,3,3,4),(95.3626616169097,96.2735747732839,97.2660858534208,
98.2585969335578,99.1696080983178),.UNSPECIFIED.);
#545=B_SPLINE_CURVE_WITH_KNOTS('',3,(#85901,#85902,#85903,#85904,#85905,
#85906,#85907,#85908,#85909,#85910,#85911,#85912,#85913,#85914,#85915,#85916,
#85917,#85918,#85919,#85920,#85921,#85922,#85923,#85924,#85925,#85926,#85927,
#85928,#85929,#85930,#85931,#85932,#85933,#85934,#85935,#85936,#85937,#85938,
#85939,#85940,#85941,#85942,#85943,#85944,#85945,#85946,#85947,#85948,#85949,
#85950,#85951,#85952,#85953,#85954,#85955,#85956,#85957,#85958,#85959,#85960,
#85961,#85962,#85963,#85964,#85965,#85966,#85967,#85968,#85969,#85970,#85971,
#85972,#85973,#85974,#85975,#85976,#85977,#85978,#85979,#85980,#85981,#85982,
#85983,#85984,#85985,#85986,#85987,#85988,#85989,#85990,#85991,#85992,#85993,
#85994,#85995,#85996,#85997,#85998,#85999,#86000,#86001,#86002,#86003,#86004,
#86005,#86006),.UNSPECIFIED.,.F.,.F.,(4,3,3,3,3,3,3,3,3,3,3,3,3,3,3,3,3,
3,3,3,3,3,3,3,3,3,3,3,3,3,3,3,3,3,3,4),(-0.93774096308178,-0.904107646522482,
-0.866863932192539,-0.842197368041274,-0.832993371681509,-0.824789553146923,
-0.786675013978796,-0.747365500452983,-0.730167588285441,-0.721368589124621,
-0.71392688849041,-0.674225052886835,-0.633949888794187,-0.593512143038715,
-0.563183833722111,-0.549662020429662,-0.544150075388719,-0.502692242333048,
-0.472198905772298,-0.432024869958226,-0.391226757969465,-0.378539422844806,
-0.371924656072871,-0.366074709533405,-0.324930003430011,-0.282818362179158,
-0.241021666268114,-0.210893957984599,-0.197713085610562,-0.189266835378695,
-0.183259344573423,-0.140443545162322,-0.0970662476713074,-0.0537369172547579,
-0.0109802554493726,0.),.UNSPECIFIED.);
#546=B_SPLINE_CURVE_WITH_KNOTS('',3,(#86007,#86008,#86009,#86010,#86011,
#86012,#86013,#86014,#86015),.UNSPECIFIED.,.F.,.F.,(4,1,1,1,1,1,4),(10.3764180272042,
11.2874291919642,12.2799402721011,13.2724513522381,14.264962432375,15.257473512512,
15.7079632679489),.UNSPECIFIED.);
#547=B_SPLINE_CURVE_WITH_KNOTS('',3,(#86021,#86022,#86023,#86024,#86025,
#86026,#86027,#86028,#86029,#86030,#86031,#86032,#86033,#86034,#86035,#86036,
#86037,#86038,#86039,#86040,#86041,#86042,#86043,#86044,#86045,#86046,#86047,
#86048,#86049,#86050,#86051,#86052,#86053,#86054,#86055,#86056,#86057,#86058,
#86059,#86060,#86061,#86062,#86063,#86064,#86065,#86066,#86067,#86068,#86069,
#86070,#86071,#86072,#86073,#86074,#86075,#86076,#86077,#86078,#86079,#86080,
#86081,#86082,#86083,#86084,#86085,#86086,#86087,#86088,#86089,#86090,#86091,
#86092,#86093,#86094,#86095,#86096,#86097,#86098,#86099,#86100,#86101,#86102,
#86103,#86104,#86105,#86106,#86107,#86108,#86109,#86110,#86111,#86112,#86113,
#86114,#86115,#86116,#86117,#86118,#86119,#86120,#86121,#86122,#86123,#86124,
#86125,#86126),.UNSPECIFIED.,.F.,.F.,(4,3,3,3,3,3,3,3,3,3,3,3,3,3,3,3,3,
3,3,3,3,3,3,3,3,3,3,3,3,3,3,3,3,3,3,4),(-0.933975894023116,-0.893931319943502,
-0.850589369822176,-0.824132129109434,-0.808860828934738,-0.801881933395027,
-0.7591389235175,-0.717655747880102,-0.698300462974381,-0.686886911899595,
-0.681304641078954,-0.639280632763917,-0.597411418690237,-0.554876943622257,
-0.522976087321272,-0.510638738070324,-0.502211740640668,-0.496747389660431,
-0.456670389952576,-0.427273518418318,-0.386682233223811,-0.346195805079578,
-0.330881843116922,-0.325030643604465,-0.285554427098605,-0.246235631641689,
-0.208611124605621,-0.182534734029918,-0.169433445615235,-0.162203295367182,
-0.156994995662412,-0.117746246746809,-0.079511462269274,-0.039755731134637,
-0.00273230733110789,0.),.UNSPECIFIED.);
#548=B_SPLINE_CURVE_WITH_KNOTS('',3,(#86129,#86130,#86131,#86132,#86133,
#86134,#86135,#86136,#86137),.UNSPECIFIED.,.F.,.F.,(4,1,1,1,1,1,4),(11.6147305479242,
12.1109860879927,12.6072416280611,13.5997527081981,14.592263788335,15.584774868472,
15.7079632679489),.UNSPECIFIED.);
#549=B_SPLINE_CURVE_WITH_KNOTS('',3,(#86566,#86567,#86568,#86569,#86570,
#86571,#86572,#86573,#86574,#86575,#86576,#86577,#86578),.UNSPECIFIED.,
 .F.,.F.,(4,3,3,3,4),(-101.236130173969,-100.7398746339,-100.243619093832,
-99.2511080136948,-98.3410123277186),.UNSPECIFIED.);
#550=B_SPLINE_CURVE_WITH_KNOTS('',3,(#87482,#87483,#87484,#87485,#87486,
#87487,#87488,#87489,#87490,#87491),.UNSPECIFIED.,.F.,.F.,(4,3,3,4),(-4.09293042013066,
-3.98462531944883,-2.98846898958662,-2.06863817490914),.UNSPECIFIED.);
#551=B_SPLINE_CURVE_WITH_KNOTS('',3,(#87494,#87495,#87496,#87497,#87498,
#87499,#87500),.UNSPECIFIED.,.F.,.F.,(4,3,4),(0.,0.996156329862199,1.11730040836818),
 .UNSPECIFIED.);
#552=B_SPLINE_CURVE_WITH_KNOTS('',3,(#87505,#87506,#87507,#87508,#87509,
#87510,#87511,#87512,#87513,#87514,#87515,#87516,#87517,#87518,#87519,#87520,
#87521,#87522,#87523,#87524,#87525,#87526),.UNSPECIFIED.,.F.,.F.,(4,3,3,
3,3,3,3,4),(-10.3761157273103,-9.96156329862207,-8.96540696875986,-7.96925063889766,
-6.97309430903545,-5.97693797917324,-4.98078164931104,-4.09293042013066),
 .UNSPECIFIED.);
#553=B_SPLINE_CURVE_WITH_KNOTS('',3,(#87527,#87528,#87529,#87530,#87531,
#87532,#87533,#87534,#87535,#87536,#87537,#87538,#87539,#87540,#87541,#87542,
#87543,#87544,#87545,#87546,#87547,#87548),.UNSPECIFIED.,.F.,.F.,(4,3,3,
3,3,3,3,4),(1.11730040836818,1.99231265972441,2.98846898958662,3.98462531944883,
4.98078164931103,5.97693797917324,6.97309430903544,7.40048571554775),
 .UNSPECIFIED.);
#554=B_SPLINE_CURVE_WITH_KNOTS('',3,(#87553,#87554,#87555,#87556,#87557,
#87558,#87559,#87560,#87561,#87562,#87563,#87564,#87565,#87566,#87567,#87568,
#87569,#87570,#87571,#87572,#87573,#87574),.UNSPECIFIED.,.F.,.F.,(4,3,3,
3,3,3,3,4),(-16.6593010344898,-15.9385012777953,-14.9423449479331,-13.9461886180709,
-12.9500322882087,-11.9538759583465,-10.9577196284843,-10.3761157273103),
 .UNSPECIFIED.);
#555=B_SPLINE_CURVE_WITH_KNOTS('',3,(#87575,#87576,#87577,#87578,#87579,
#87580,#87581,#87582,#87583,#87584,#87585,#87586,#87587,#87588,#87589,#87590,
#87591,#87592,#87593,#87594,#87595,#87596),.UNSPECIFIED.,.F.,.F.,(4,3,3,
3,3,3,3,4),(7.40048571554775,7.96925063889765,8.96540696875986,9.96156329862207,
10.9577196284843,11.9538759583465,12.9500322882087,13.6836710227273),
 .UNSPECIFIED.);
#556=B_SPLINE_CURVE_WITH_KNOTS('',3,(#87601,#87602,#87603,#87604,#87605,
#87606,#87607,#87608,#87609,#87610,#87611,#87612,#87613,#87614,#87615,#87616,
#87617,#87618,#87619,#87620,#87621,#87622,#87623,#87624,#87625),
 .UNSPECIFIED.,.F.,.F.,(4,3,3,3,3,3,3,3,4),(-22.9424863416694,-22.9115955868308,
-21.9154392569686,-20.9192829271063,-19.9231265972441,-18.9269702673819,
-17.9308139375197,-16.9346576076575,-16.6593010344898),.UNSPECIFIED.);
#557=B_SPLINE_CURVE_WITH_KNOTS('',3,(#87626,#87627,#87628,#87629,#87630,
#87631,#87632,#87633,#87634,#87635,#87636,#87637,#87638,#87639,#87640,#87641,
#87642,#87643,#87644,#87645,#87646,#87647,#87648,#87649,#87650),
 .UNSPECIFIED.,.F.,.F.,(4,3,3,3,3,3,3,3,4),(13.6836710227273,13.9461886180709,
14.9423449479331,15.9385012777953,16.9346576076575,17.9308139375197,18.9269702673819,
19.9231265972441,19.9668563299069),.UNSPECIFIED.);
#558=B_SPLINE_CURVE_WITH_KNOTS('',3,(#87655,#87656,#87657,#87658,#87659,
#87660,#87661,#87662,#87663,#87664,#87665,#87666,#87667,#87668,#87669,#87670,
#87671,#87672,#87673,#87674,#87675,#87676),.UNSPECIFIED.,.F.,.F.,(4,3,3,
3,3,3,3,4),(-29.225671648849,-28.888533566004,-27.8923772361418,-26.8962209062796,
-25.9000645764174,-24.9039082465552,-23.907751916693,-22.9424863416694),
 .UNSPECIFIED.);
#559=B_SPLINE_CURVE_WITH_KNOTS('',3,(#87677,#87678,#87679,#87680,#87681,
#87682,#87683,#87684,#87685,#87686,#87687,#87688,#87689,#87690,#87691,#87692,
#87693,#87694,#87695,#87696,#87697,#87698),.UNSPECIFIED.,.F.,.F.,(4,3,3,
3,3,3,3,4),(19.9668563299069,20.9192829271063,21.9154392569685,22.9115955868307,
23.907751916693,24.9039082465552,25.9000645764174,26.2500416370865),
 .UNSPECIFIED.);
#560=B_SPLINE_CURVE_WITH_KNOTS('',3,(#87703,#87704,#87705,#87706,#87707,
#87708,#87709,#87710,#87711,#87712,#87713,#87714,#87715,#87716,#87717,#87718,
#87719,#87720,#87721,#87722,#87723,#87724),.UNSPECIFIED.,.F.,.F.,(4,3,3,
3,3,3,3,4),(-35.5088569560286,-34.8654715451772,-33.869315215315,-32.8731588854528,
-31.8770025555906,-30.8808462257284,-29.8846898958662,-29.225671648849),
 .UNSPECIFIED.);
#561=B_SPLINE_CURVE_WITH_KNOTS('',3,(#87725,#87726,#87727,#87728,#87729,
#87730,#87731,#87732,#87733,#87734,#87735,#87736,#87737,#87738,#87739,#87740,
#87741,#87742,#87743,#87744,#87745,#87746),.UNSPECIFIED.,.F.,.F.,(4,3,3,
3,3,3,3,4),(26.2500416370865,26.8962209062796,27.8923772361418,28.888533566004,
29.8846898958662,30.8808462257284,31.8770025555906,32.5332269442661),
 .UNSPECIFIED.);
#562=B_SPLINE_CURVE_WITH_KNOTS('',3,(#87751,#87752,#87753,#87754,#87755,
#87756,#87757,#87758,#87759,#87760,#87761,#87762,#87763,#87764,#87765,#87766,
#87767,#87768,#87769,#87770,#87771,#87772),.UNSPECIFIED.,.F.,.F.,(4,3,3,
3,3,3,3,4),(-41.7920422632082,-40.8424095243505,-39.8462531944883,-38.8500968646261,
-37.8539405347639,-36.8577842049017,-35.8616278750394,-35.5088569560286),
 .UNSPECIFIED.);
#563=B_SPLINE_CURVE_WITH_KNOTS('',3,(#87773,#87774,#87775,#87776,#87777,
#87778,#87779,#87780,#87781,#87782,#87783,#87784,#87785,#87786,#87787,#87788,
#87789,#87790,#87791,#87792,#87793,#87794),.UNSPECIFIED.,.F.,.F.,(4,3,3,
3,3,3,3,4),(32.5332269442661,32.8731588854528,33.869315215315,34.8654715451772,
35.8616278750394,36.8577842049016,37.8539405347639,38.8164122514457),
 .UNSPECIFIED.);
#564=B_SPLINE_CURVE_WITH_KNOTS('',3,(#87799,#87800,#87801,#87802,#87803,
#87804,#87805,#87806,#87807,#87808,#87809,#87810,#87811,#87812,#87813,#87814,
#87815,#87816,#87817,#87818,#87819,#87820,#87821,#87822,#87823),
 .UNSPECIFIED.,.F.,.F.,(4,3,3,3,3,3,3,3,4),(-48.0752275703878,-47.8155038333859,
-46.8193475035237,-45.8231911736615,-44.8270348437993,-43.8308785139371,
-42.8347221840749,-41.8385658542127,-41.7920422632082),.UNSPECIFIED.);
#565=B_SPLINE_CURVE_WITH_KNOTS('',3,(#87824,#87825,#87826,#87827,#87828,
#87829,#87830,#87831,#87832,#87833,#87834,#87835,#87836,#87837,#87838,#87839,
#87840,#87841,#87842,#87843,#87844,#87845,#87846,#87847,#87848),
 .UNSPECIFIED.,.F.,.F.,(4,3,3,3,3,3,3,3,4),(38.8164122514457,38.8500968646261,
39.8462531944883,40.8424095243505,41.8385658542127,42.8347221840749,43.8308785139371,
44.8270348437993,45.0995975586253),.UNSPECIFIED.);
#566=B_SPLINE_CURVE_WITH_KNOTS('',3,(#87853,#87854,#87855,#87856,#87857,
#87858,#87859,#87860,#87861,#87862,#87863,#87864,#87865,#87866,#87867,#87868,
#87869,#87870,#87871,#87872,#87873,#87874),.UNSPECIFIED.,.F.,.F.,(4,3,3,
3,3,3,3,4),(-54.3584128775674,-53.7924418125592,-52.796285482697,-51.8001291528348,
-50.8039728229726,-49.8078164931104,-48.8116601632481,-48.0752275703878),
 .UNSPECIFIED.);
#567=B_SPLINE_CURVE_WITH_KNOTS('',3,(#87875,#87876,#87877,#87878,#87879,
#87880,#87881,#87882,#87883,#87884,#87885,#87886,#87887,#87888,#87889,#87890,
#87891,#87892,#87893,#87894,#87895,#87896),.UNSPECIFIED.,.F.,.F.,(4,3,3,
3,3,3,3,4),(45.0995975586253,45.8231911736615,46.8193475035237,47.8155038333859,
48.8116601632481,49.8078164931103,50.8039728229725,51.3827828658049),
 .UNSPECIFIED.);
#568=B_SPLINE_CURVE_WITH_KNOTS('',3,(#87901,#87902,#87903,#87904,#87905,
#87906,#87907,#87908,#87909,#87910,#87911,#87912,#87913,#87914,#87915,#87916,
#87917,#87918,#87919,#87920,#87921,#87922),.UNSPECIFIED.,.F.,.F.,(4,3,3,
3,3,3,3,4),(-60.641598184747,-59.7693797917324,-58.7732234618702,-57.777067132008,
-56.7809108021458,-55.7847544722836,-54.7885981424214,-54.3584128775674),
 .UNSPECIFIED.);
#569=B_SPLINE_CURVE_WITH_KNOTS('',3,(#87923,#87924,#87925,#87926,#87927,
#87928,#87929,#87930,#87931,#87932,#87933,#87934,#87935,#87936,#87937,#87938,
#87939,#87940,#87941,#87942,#87943,#87944),.UNSPECIFIED.,.F.,.F.,(4,3,3,
3,3,3,3,4),(51.3827828658049,51.8001291528347,52.796285482697,53.7924418125592,
54.7885981424214,55.7847544722836,56.7809108021458,57.6659681729845),
 .UNSPECIFIED.);
#570=B_SPLINE_CURVE_WITH_KNOTS('',3,(#87949,#87950,#87951,#87952,#87953,
#87954,#87955,#87956,#87957,#87958,#87959,#87960,#87961,#87962,#87963,#87964,
#87965,#87966,#87967,#87968,#87969,#87970,#87971,#87972,#87973),
 .UNSPECIFIED.,.F.,.F.,(4,3,3,3,3,3,3,3,4),(-66.9247834919266,-66.7424741007679,
-65.7463177709057,-64.7501614410435,-63.7540051111813,-62.757848781319,
-61.7616924514568,-60.7655361215946,-60.641598184747),.UNSPECIFIED.);
#571=B_SPLINE_CURVE_WITH_KNOTS('',3,(#87974,#87975,#87976,#87977,#87978,
#87979,#87980,#87981,#87982,#87983,#87984,#87985,#87986,#87987,#87988,#87989,
#87990,#87991,#87992,#87993,#87994,#87995,#87996,#87997,#87998),
 .UNSPECIFIED.,.F.,.F.,(4,3,3,3,3,3,3,3,4),(57.6659681729845,57.777067132008,
58.7732234618702,59.7693797917324,60.7655361215946,61.7616924514568,62.757848781319,
63.7540051111813,63.9491534801641),.UNSPECIFIED.);
#572=B_SPLINE_CURVE_WITH_KNOTS('',3,(#88003,#88004,#88005,#88006,#88007,
#88008,#88009,#88010,#88011,#88012,#88013,#88014,#88015,#88016,#88017,#88018,
#88019,#88020,#88021,#88022,#88023,#88024),.UNSPECIFIED.,.F.,.F.,(4,3,3,
3,3,3,3,4),(-73.2079687991062,-72.7194120799411,-71.7232557500789,-70.7270994202167,
-69.7309430903545,-68.7347867604923,-67.7386304306301,-66.9247834919266),
 .UNSPECIFIED.);
#573=B_SPLINE_CURVE_WITH_KNOTS('',3,(#88025,#88026,#88027,#88028,#88029,
#88030,#88031,#88032,#88033,#88034,#88035,#88036,#88037,#88038,#88039,#88040,
#88041,#88042,#88043,#88044,#88045,#88046),.UNSPECIFIED.,.F.,.F.,(4,3,3,
3,3,3,3,4),(63.9491534801641,64.7501614410435,65.7463177709057,66.7424741007679,
67.7386304306301,68.7347867604923,69.7309430903545,70.2323387873437),
 .UNSPECIFIED.);
#574=B_SPLINE_CURVE_WITH_KNOTS('',3,(#88051,#88052,#88053,#88054,#88055,
#88056,#88057,#88058,#88059,#88060,#88061,#88062,#88063,#88064,#88065,#88066,
#88067,#88068,#88069,#88070,#88071,#88072),.UNSPECIFIED.,.F.,.F.,(4,3,3,
3,3,3,3,4),(-79.4911541062857,-78.6963500591144,-77.7001937292521,-76.7040373993899,
-75.7078810695277,-74.7117247396655,-73.7155684098033,-73.2079687991062),
 .UNSPECIFIED.);
#575=B_SPLINE_CURVE_WITH_KNOTS('',3,(#88073,#88074,#88075,#88076,#88077,
#88078,#88079,#88080,#88081,#88082,#88083,#88084,#88085,#88086,#88087,#88088,
#88089,#88090,#88091,#88092,#88093,#88094),.UNSPECIFIED.,.F.,.F.,(4,3,3,
3,3,3,3,4),(70.2323387873437,70.7270994202167,71.7232557500789,72.7194120799411,
73.7155684098033,74.7117247396655,75.7078810695277,76.5155240945233),
 .UNSPECIFIED.);
#576=B_SPLINE_CURVE_WITH_KNOTS('',3,(#88099,#88100,#88101,#88102,#88103,
#88104,#88105,#88106,#88107,#88108,#88109,#88110,#88111,#88112,#88113,#88114,
#88115,#88116,#88117,#88118,#88119,#88120,#88121,#88122,#88123),
 .UNSPECIFIED.,.F.,.F.,(4,3,3,3,3,3,3,3,4),(-85.7743394134653,-85.6694443681498,
-84.6732880382876,-83.6771317084254,-82.6809753785632,-81.684819048701,
-80.6886627188388,-79.6925063889766,-79.4911541062857),.UNSPECIFIED.);
#577=B_SPLINE_CURVE_WITH_KNOTS('',3,(#88124,#88125,#88126,#88127,#88128,
#88129,#88130,#88131,#88132,#88133,#88134,#88135,#88136,#88137,#88138,#88139,
#88140,#88141,#88142,#88143,#88144,#88145,#88146,#88147,#88148),
 .UNSPECIFIED.,.F.,.F.,(4,3,3,3,3,3,3,3,4),(76.5155240945233,76.7040373993899,
77.7001937292521,78.6963500591143,79.6925063889765,80.6886627188388,81.684819048701,
82.6809753785631,82.7987094017029),.UNSPECIFIED.);
#578=B_SPLINE_CURVE_WITH_KNOTS('',3,(#88153,#88154,#88155,#88156,#88157,
#88158,#88159,#88160,#88161,#88162,#88163,#88164,#88165,#88166,#88167,#88168,
#88169,#88170,#88171,#88172,#88173,#88174),.UNSPECIFIED.,.F.,.F.,(4,3,3,
3,3,3,3,4),(-92.0575247206449,-91.646382347323,-90.6502260174608,-89.6540696875986,
-88.6579133577364,-87.6617570278742,-86.665600698012,-85.7743394134653),
 .UNSPECIFIED.);
#579=B_SPLINE_CURVE_WITH_KNOTS('',3,(#88175,#88176,#88177,#88178,#88179,
#88180,#88181,#88182,#88183,#88184,#88185,#88186,#88187,#88188,#88189,#88190,
#88191,#88192,#88193,#88194,#88195,#88196),.UNSPECIFIED.,.F.,.F.,(4,3,3,
3,3,3,3,4),(82.7987094017029,83.6771317084254,84.6732880382876,85.6694443681498,
86.665600698012,87.6617570278742,88.6579133577364,89.0818947088824),
 .UNSPECIFIED.);
#580=B_SPLINE_CURVE_WITH_KNOTS('',3,(#88203,#88204,#88205,#88206,#88207,
#88208,#88209,#88210,#88211,#88212,#88213,#88214,#88215,#88216,#88217,#88218,
#88219,#88220,#88221),.UNSPECIFIED.,.F.,.F.,(4,3,3,3,3,3,4),(-97.6233203264963,
-96.6271639966341,-95.6310076667719,-94.6348513369097,-93.6386950070474,
-92.6425386771852,-92.0575247206449),.UNSPECIFIED.);
#581=B_SPLINE_CURVE_WITH_KNOTS('',3,(#88222,#88223,#88224,#88225,#88226,
#88227,#88228,#88229,#88230,#88231,#88232,#88233,#88234,#88235,#88236,#88237,
#88238,#88239,#88240,#88241,#88242,#88243),.UNSPECIFIED.,.F.,.F.,(4,3,3,
3,3,3,3,4),(89.0818947088824,89.6540696875986,90.6502260174608,91.646382347323,
92.6425386771852,93.6386950070475,94.6348513369096,95.365080016062),
 .UNSPECIFIED.);
#582=B_SPLINE_CURVE_WITH_KNOTS('',3,(#88249,#88250,#88251,#88252,#88253,
#88254,#88255),.UNSPECIFIED.,.F.,.F.,(4,1,1,1,4),(103.672557568463,104.257571525003,
105.253727854866,106.249884184728,107.169714999405),.UNSPECIFIED.);
#583=B_SPLINE_CURVE_WITH_KNOTS('',3,(#88258,#88259,#88260,#88261,#88262,
#88263),.UNSPECIFIED.,.F.,.F.,(4,1,1,4),(103.672557568463,103.938485219173,
104.934641549035,105.930797878897),.UNSPECIFIED.);
#584=B_SPLINE_CURVE_WITH_KNOTS('',3,(#88268,#88269,#88270,#88271,#88272,
#88273,#88274,#88275,#88276,#88277),.UNSPECIFIED.,.F.,.F.,(4,1,1,1,1,1,
1,4),(97.3893722612836,98.2806335458302,99.2767898756924,100.272946205555,
101.269102535417,102.265258865279,103.261415195141,103.672557568463),
 .UNSPECIFIED.);
#585=B_SPLINE_CURVE_WITH_KNOTS('',3,(#88278,#88279,#88280,#88281,#88282,
#88283,#88284,#88285,#88286,#88287),.UNSPECIFIED.,.F.,.F.,(4,1,1,1,1,1,
1,4),(97.3893722612836,97.9615472399996,98.9577035698618,99.9538598997241,
100.950016229586,101.946172559448,102.942328889311,103.672557568463),
 .UNSPECIFIED.);
#586=B_SPLINE_CURVE_WITH_KNOTS('',3,(#88292,#88293,#88294,#88295,#88296,
#88297,#88298,#88299,#88300,#88301,#88302),.UNSPECIFIED.,.F.,.F.,(4,1,1,
1,1,1,1,1,4),(91.106186954104,91.3075392367948,92.303695566657,93.2998518965192,
94.2960082263814,95.2921645562436,96.2883208861058,97.284477215968,97.3893722612836),
 .UNSPECIFIED.);
#587=B_SPLINE_CURVE_WITH_KNOTS('',3,(#88303,#88304,#88305,#88306,#88307,
#88308,#88309,#88310,#88311,#88312),.UNSPECIFIED.,.F.,.F.,(4,1,1,1,1,1,
1,4),(91.106186954104,91.9846092608264,92.9807655906886,93.9769219205508,
94.973078250413,95.9692345802752,96.9653909101374,97.3893722612836),
 .UNSPECIFIED.);
#588=B_SPLINE_CURVE_WITH_KNOTS('',3,(#88317,#88318,#88319,#88320,#88321,
#88322,#88323,#88324,#88325,#88326),.UNSPECIFIED.,.F.,.F.,(4,1,1,1,1,1,
1,4),(84.8230016469244,85.3306012576215,86.3267575874837,87.322913917346,
88.3190702472082,89.3152265770704,90.3113829069326,91.106186954104),
 .UNSPECIFIED.);
#589=B_SPLINE_CURVE_WITH_KNOTS('',3,(#88327,#88328,#88329,#88330,#88331,
#88332,#88333,#88334,#88335,#88336,#88337),.UNSPECIFIED.,.F.,.F.,(4,1,1,
1,1,1,1,1,4),(84.8230016469244,85.0115149517909,86.0076712816532,87.0038276115154,
87.9999839413776,88.9961402712398,89.992296601102,90.9884529309642,91.106186954104),
 .UNSPECIFIED.);
#590=B_SPLINE_CURVE_WITH_KNOTS('',3,(#88342,#88343,#88344,#88345,#88346,
#88347,#88348,#88349,#88350,#88351),.UNSPECIFIED.,.F.,.F.,(4,1,1,1,1,1,
1,4),(78.5398163397448,79.3536632784483,80.3498196083105,81.3459759381727,
82.3421322680349,83.3382885978971,84.3344449277593,84.8230016469244),
 .UNSPECIFIED.);
#591=B_SPLINE_CURVE_WITH_KNOTS('',3,(#88352,#88353,#88354,#88355,#88356,
#88357,#88358,#88359,#88360,#88361),.UNSPECIFIED.,.F.,.F.,(4,1,1,1,1,1,
1,4),(78.5398163397448,79.0345769726177,80.0307333024799,81.0268896323421,
82.0230459622043,83.0192022920665,84.0153586219287,84.8230016469244),
 .UNSPECIFIED.);
#592=B_SPLINE_CURVE_WITH_KNOTS('',3,(#88366,#88367,#88368,#88369,#88370,
#88371,#88372,#88373,#88374,#88375,#88376),.UNSPECIFIED.,.F.,.F.,(4,1,1,
1,1,1,1,1,4),(72.2566310325652,72.3805689694128,73.3767252992751,74.3728816291373,
75.3690379589995,76.3651942888617,77.3613506187239,78.3575069485861,78.5398163397448),
 .UNSPECIFIED.);
#593=B_SPLINE_CURVE_WITH_KNOTS('',3,(#88377,#88378,#88379,#88380,#88381,
#88382,#88383,#88384,#88385,#88386),.UNSPECIFIED.,.F.,.F.,(4,1,1,1,1,1,
1,4),(72.2566310325652,73.0576389934445,74.0537953233067,75.0499516531689,
76.0461079830311,77.0422643128933,78.0384206427555,78.5398163397448),
 .UNSPECIFIED.);
#594=B_SPLINE_CURVE_WITH_KNOTS('',3,(#88391,#88392,#88393,#88394,#88395,
#88396,#88397,#88398,#88399,#88400),.UNSPECIFIED.,.F.,.F.,(4,1,1,1,1,1,
1,4),(65.9734457253856,66.4036309902396,67.3997873201018,68.395943649964,
69.3920999798262,70.3882563096884,71.3844126395506,72.2566310325652),
 .UNSPECIFIED.);
#595=B_SPLINE_CURVE_WITH_KNOTS('',3,(#88401,#88402,#88403,#88404,#88405,
#88406,#88407,#88408,#88409,#88410,#88411),.UNSPECIFIED.,.F.,.F.,(4,1,1,
1,1,1,1,1,4),(65.9734457253856,66.084544684409,67.0807010142712,68.0768573441334,
69.0730136739956,70.0691700038578,71.0653263337201,72.0614826635823,72.2566310325652),
 .UNSPECIFIED.);
#596=B_SPLINE_CURVE_WITH_KNOTS('',3,(#88416,#88417,#88418,#88419,#88420,
#88421,#88422,#88423,#88424,#88425),.UNSPECIFIED.,.F.,.F.,(4,1,1,1,1,1,
1,4),(59.690260418206,60.4266930110664,61.4228493409286,62.4190056707908,
63.415162000653,64.4113183305152,65.4074746603774,65.9734457253856),
 .UNSPECIFIED.);
#597=B_SPLINE_CURVE_WITH_KNOTS('',3,(#88426,#88427,#88428,#88429,#88430,
#88431,#88432,#88433,#88434,#88435),.UNSPECIFIED.,.F.,.F.,(4,1,1,1,1,1,
1,4),(59.690260418206,60.1076067052358,61.103763035098,62.0999193649602,
63.0960756948224,64.0922320246846,65.0883883545468,65.9734457253856),
 .UNSPECIFIED.);
#598=B_SPLINE_CURVE_WITH_KNOTS('',3,(#88440,#88441,#88442,#88443,#88444,
#88445,#88446,#88447,#88448,#88449,#88450),.UNSPECIFIED.,.F.,.F.,(4,1,1,
1,1,1,1,1,4),(53.4070751110264,53.4535987020309,54.4497550318931,55.4459113617553,
56.4420676916175,57.4382240214797,58.434380351342,59.4305366812042,59.690260418206),
 .UNSPECIFIED.);
#599=B_SPLINE_CURVE_WITH_KNOTS('',3,(#88451,#88452,#88453,#88454,#88455,
#88456,#88457,#88458,#88459,#88460),.UNSPECIFIED.,.F.,.F.,(4,1,1,1,1,1,
1,4),(53.4070751110264,54.1306687260625,55.1268250559247,56.122981385787,
57.1191377156492,58.1152940455114,59.1114503753736,59.690260418206),
 .UNSPECIFIED.);
#600=B_SPLINE_CURVE_WITH_KNOTS('',3,(#88465,#88466,#88467,#88468,#88469,
#88470,#88471,#88472,#88473,#88474),.UNSPECIFIED.,.F.,.F.,(4,1,1,1,1,1,
1,4),(47.1238898038468,47.4766607228577,48.4728170527199,49.4689733825821,
50.4651297124443,51.4612860423065,52.4574423721687,53.4070751110264),
 .UNSPECIFIED.);
#601=B_SPLINE_CURVE_WITH_KNOTS('',3,(#88475,#88476,#88477,#88478,#88479,
#88480,#88481,#88482,#88483,#88484,#88485),.UNSPECIFIED.,.F.,.F.,(4,1,1,
1,1,1,1,1,4),(47.1238898038468,47.1575744170271,48.1537307468893,49.1498870767515,
50.1460434066137,51.1421997364759,52.1383560663381,53.1345123962003,53.4070751110264),
 .UNSPECIFIED.);
#602=B_SPLINE_CURVE_WITH_KNOTS('',3,(#88490,#88491,#88492,#88493,#88494,
#88495,#88496,#88497,#88498,#88499),.UNSPECIFIED.,.F.,.F.,(4,1,1,1,1,1,
1,4),(40.8407044966673,41.4997227436844,42.4958790735466,43.4920354034088,
44.4881917332711,45.4843480631333,46.4805043929955,47.1238898038468),
 .UNSPECIFIED.);
#603=B_SPLINE_CURVE_WITH_KNOTS('',3,(#88500,#88501,#88502,#88503,#88504,
#88505,#88506,#88507,#88508,#88509),.UNSPECIFIED.,.F.,.F.,(4,1,1,1,1,1,
1,4),(40.8407044966672,41.1806364378538,42.1767927677161,43.1729490975783,
44.1691054274405,45.1652617573027,46.1614180871649,47.1238898038468),
 .UNSPECIFIED.);
#604=B_SPLINE_CURVE_WITH_KNOTS('',3,(#88514,#88515,#88516,#88517,#88518,
#88519,#88520,#88521,#88522,#88523),.UNSPECIFIED.,.F.,.F.,(4,1,1,1,1,1,
1,4),(34.5575191894877,35.5227847645112,36.5189410943734,37.5150974242356,
38.5112537540978,39.50741008396,40.5035664138222,40.8407044966673),
 .UNSPECIFIED.);
#605=B_SPLINE_CURVE_WITH_KNOTS('',3,(#88524,#88525,#88526,#88527,#88528,
#88529,#88530,#88531,#88532,#88533),.UNSPECIFIED.,.F.,.F.,(4,1,1,1,1,1,
1,4),(34.5575191894876,35.2036984586806,36.1998547885428,37.196011118405,
38.1921674482672,39.1883237781294,40.1844801079916,40.8407044966672),
 .UNSPECIFIED.);
#606=B_SPLINE_CURVE_WITH_KNOTS('',3,(#88538,#88539,#88540,#88541,#88542,
#88543,#88544,#88545,#88546,#88547,#88548),.UNSPECIFIED.,.F.,.F.,(4,1,1,
1,1,1,1,1,4),(28.2743338823081,28.5496904554757,29.545846785338,30.5420031152002,
31.5381594450624,32.5343157749246,33.5304721047868,34.526628434649,34.5575191894877),
 .UNSPECIFIED.);
#607=B_SPLINE_CURVE_WITH_KNOTS('',3,(#88549,#88550,#88551,#88552,#88553,
#88554,#88555,#88556,#88557,#88558),.UNSPECIFIED.,.F.,.F.,(4,1,1,1,1,1,
1,4),(28.2743338823081,29.2267604795074,30.2229168093696,31.2190731392318,
32.215229469094,33.2113857989562,34.2075421288184,34.5575191894876),
 .UNSPECIFIED.);
#608=B_SPLINE_CURVE_WITH_KNOTS('',3,(#88563,#88564,#88565,#88566,#88567,
#88568,#88569,#88570,#88571,#88572),.UNSPECIFIED.,.F.,.F.,(4,1,1,1,1,1,
1,4),(21.9911485751285,22.5727524763025,23.5689088061647,24.5650651360269,
25.5612214658891,26.5573777957513,27.5535341256135,28.2743338823081),
 .UNSPECIFIED.);
#609=B_SPLINE_CURVE_WITH_KNOTS('',3,(#88573,#88574,#88575,#88576,#88577,
#88578,#88579,#88580,#88581,#88582,#88583),.UNSPECIFIED.,.F.,.F.,(4,1,1,
1,1,1,1,1,4),(21.9911485751285,22.2536661704719,23.2498225003341,24.2459788301963,
25.2421351600585,26.2382914899207,27.234447819783,28.2306041496452,28.2743338823081),
 .UNSPECIFIED.);
#610=B_SPLINE_CURVE_WITH_KNOTS('',3,(#88588,#88589,#88590,#88591,#88592,
#88593,#88594,#88595,#88596,#88597),.UNSPECIFIED.,.F.,.F.,(4,1,1,1,1,1,
1,4),(15.7079632679489,16.5958144971293,17.5919708269915,18.5881271568537,
19.5842834867159,20.5804398165781,21.5765961464403,21.9911485751285),
 .UNSPECIFIED.);
#611=B_SPLINE_CURVE_WITH_KNOTS('',3,(#88598,#88599,#88600,#88601,#88602,
#88603,#88604,#88605,#88606,#88607),.UNSPECIFIED.,.F.,.F.,(4,1,1,1,1,1,
1,4),(15.7079632679489,16.2767281912987,17.2728845211609,18.2690408510231,
19.2651971808853,20.2613535107475,21.2575098406097,21.9911485751285),
 .UNSPECIFIED.);
#612=B_SPLINE_CURVE_WITH_KNOTS('',3,(#88609,#88610,#88611,#88612,#88613,
#88614,#88615,#88616,#88617,#88618,#88619,#88620,#88621,#88622,#88623,#88624,
#88625,#88626,#88627,#88628,#88629,#88630,#88631,#88632,#88633,#88634,#88635,
#88636,#88637,#88638,#88639,#88640,#88641,#88642,#88643,#88644,#88645,#88646,
#88647,#88648,#88649,#88650,#88651,#88652,#88653,#88654,#88655,#88656,#88657,
#88658,#88659,#88660,#88661,#88662,#88663,#88664,#88665,#88666,#88667,#88668,
#88669,#88670,#88671,#88672,#88673,#88674,#88675,#88676,#88677,#88678,#88679,
#88680,#88681,#88682,#88683,#88684,#88685,#88686,#88687,#88688,#88689,#88690,
#88691,#88692,#88693,#88694,#88695,#88696,#88697,#88698,#88699),
 .UNSPECIFIED.,.F.,.F.,(4,3,3,3,3,3,3,3,3,3,3,3,3,3,3,3,3,3,3,3,3,3,3,3,
3,3,3,3,3,3,4),(-0.555272788399387,-0.536878011109327,-0.51216130922638,
-0.497772596378623,-0.492151132384111,-0.487788613626176,-0.462008896459435,
-0.439500522359789,-0.428647464230627,-0.422031983310641,-0.395447331110844,
-0.367070974248699,-0.34578870660209,-0.329827005867133,-0.325388458044637,
-0.321109090061203,-0.293193723306362,-0.281941903662263,-0.254996262835833,
-0.227510620629366,-0.221955374106226,-0.217785459312042,-0.189854551496702,
-0.161379875371563,-0.132653453208679,-0.116071771557594,-0.111842840924105,
-0.082388957527505,-0.052837079875276,-0.0238339308196913,0.),
 .UNSPECIFIED.);
#613=B_SPLINE_CURVE_WITH_KNOTS('',3,(#88704,#88705,#88706,#88707,#88708,
#88709,#88710,#88711,#88712,#88713,#88714,#88715,#88716,#88717,#88718,#88719,
#88720,#88721,#88722,#88723,#88724,#88725,#88726,#88727,#88728,#88729,#88730,
#88731,#88732,#88733,#88734,#88735,#88736,#88737,#88738,#88739,#88740,#88741,
#88742,#88743,#88744,#88745,#88746,#88747,#88748,#88749,#88750,#88751,#88752,
#88753,#88754,#88755,#88756,#88757,#88758,#88759,#88760,#88761,#88762,#88763,
#88764,#88765,#88766,#88767,#88768,#88769,#88770,#88771,#88772,#88773,#88774,
#88775,#88776,#88777,#88778,#88779,#88780,#88781,#88782,#88783,#88784,#88785,
#88786,#88787,#88788,#88789,#88790,#88791,#88792,#88793,#88794,#88795,#88796,
#88797),.UNSPECIFIED.,.F.,.F.,(4,3,3,3,3,3,3,3,3,3,3,3,3,3,3,3,3,3,3,3,
3,3,3,3,3,3,3,3,3,3,3,4),(-0.552745378375053,-0.530338827917477,-0.500953818352793,
-0.485391213597782,-0.477022768561509,-0.471909598051007,-0.44285760577117,
-0.418994422833851,-0.408389712365122,-0.402041246675515,-0.397478427204802,
-0.369171225298371,-0.339866454541933,-0.31274605694021,-0.296909993024151,
-0.291443327397581,-0.264638986575274,-0.251952142272617,-0.224584144938619,
-0.196511126821292,-0.192477354107935,-0.188234651713186,-0.161595549194534,
-0.134996331746453,-0.108821820380775,-0.0998778564626278,-0.0942964343013907,
-0.0901979491855338,-0.0646528926729606,-0.0395090521317962,-0.0151488290738175,
0.),.UNSPECIFIED.);
#614=B_SPLINE_CURVE_WITH_KNOTS('',3,(#89202,#89203,#89204,#89205),
 .UNSPECIFIED.,.F.,.F.,(4,4),(95.365080016062,95.5546821515871),
 .UNSPECIFIED.);
#615=B_SPLINE_CURVE_WITH_KNOTS('',3,(#89207,#89208,#89209,#89210,#89211,
#89212,#89213,#89214,#89215,#89216,#89217,#89218,#89219,#89220,#89221,#89222,
#89223,#89224,#89225,#89226,#89227,#89228,#89229,#89230,#89231,#89232,#89233,
#89234,#89235,#89236,#89237,#89238,#89239,#89240,#89241,#89242,#89243,#89244,
#89245,#89246,#89247,#89248,#89249,#89250,#89251,#89252,#89253,#89254,#89255,
#89256,#89257,#89258,#89259,#89260,#89261,#89262,#89263,#89264,#89265,#89266,
#89267,#89268,#89269,#89270,#89271,#89272,#89273,#89274,#89275,#89276,#89277,
#89278,#89279,#89280,#89281,#89282,#89283,#89284,#89285,#89286,#89287,#89288,
#89289,#89290,#89291,#89292,#89293,#89294,#89295,#89296,#89297),
 .UNSPECIFIED.,.F.,.F.,(4,3,3,3,3,3,3,3,3,3,3,3,3,3,3,3,3,3,3,3,3,3,3,3,
3,3,3,3,3,3,4),(-0.555272788399382,-0.536878011109318,-0.512161326342915,
-0.497772612425373,-0.492151154968866,-0.487788650423359,-0.462008945431106,
-0.43950056521,-0.42864753175858,-0.422031972845274,-0.395447329416593,
-0.367070972978008,-0.34578870564907,-0.329827005152366,-0.325388447497642,
-0.3211090901766,-0.293193722617674,-0.281941903662254,-0.254996269333342,
-0.227510635185161,-0.221955302854236,-0.217785398797394,-0.189854497259803,
-0.161379828090615,-0.132653408275648,-0.116071732241192,-0.111842820088624,
-0.082388941995823,-0.0528370621263981,-0.0238338935438655,0.),
 .UNSPECIFIED.);
#616=B_SPLINE_CURVE_WITH_KNOTS('',3,(#89298,#89299,#89300,#89301,#89302,
#89303,#89304,#89305,#89306),.UNSPECIFIED.,.F.,.F.,(4,1,1,1,1,1,4),(10.3761157273101,
11.2959465419876,12.2921028718499,13.2882592017121,14.2844155315743,15.2805718614365,
15.7079632679489),.UNSPECIFIED.);
#617=B_SPLINE_CURVE_WITH_KNOTS('',3,(#89312,#89313,#89314,#89315,#89316,
#89317,#89318,#89319,#89320,#89321,#89322,#89323,#89324,#89325,#89326,#89327,
#89328,#89329,#89330,#89331,#89332,#89333,#89334,#89335,#89336,#89337,#89338,
#89339,#89340,#89341,#89342,#89343,#89344,#89345,#89346,#89347,#89348,#89349,
#89350,#89351,#89352,#89353,#89354,#89355,#89356,#89357,#89358,#89359,#89360,
#89361,#89362,#89363,#89364,#89365,#89366,#89367,#89368,#89369,#89370,#89371,
#89372,#89373,#89374,#89375,#89376,#89377,#89378,#89379,#89380,#89381,#89382,
#89383,#89384,#89385,#89386,#89387,#89388,#89389,#89390,#89391,#89392,#89393,
#89394,#89395,#89396,#89397,#89398,#89399,#89400,#89401,#89402,#89403,#89404,
#89405),.UNSPECIFIED.,.F.,.F.,(4,3,3,3,3,3,3,3,3,3,3,3,3,3,3,3,3,3,3,3,
3,3,3,3,3,3,3,3,3,3,3,4),(-0.552745378375037,-0.530338827917459,-0.500953817808515,
-0.485391213087521,-0.477022760402337,-0.471909587137758,-0.442857594671736,
-0.418994413121844,-0.408389707498453,-0.402041225045699,-0.397478412365188,
-0.36917120902983,-0.339866442340524,-0.312746024644426,-0.296909938382682,
-0.291443325001991,-0.264638969851884,-0.251952142272605,-0.224584135800549,
-0.19651111882548,-0.192477332906104,-0.188234649643676,-0.161595542748898,
-0.134996333495264,-0.108821841443691,-0.0998779134716403,-0.0942962236814242,
-0.0901979154241252,-0.0646528744752608,-0.0395090567028245,-0.0151488617676011,
0.),.UNSPECIFIED.);
#618=B_SPLINE_CURVE_WITH_KNOTS('',3,(#89408,#89409,#89410,#89411,#89412,
#89413,#89414,#89415),.UNSPECIFIED.,.F.,.F.,(4,1,1,1,1,4),(11.6150328478182,
12.6111891776804,13.6073455075426,14.6035018374048,15.5996581672671,15.7079632679489),
 .UNSPECIFIED.);
#619=B_SPLINE_CURVE_WITH_KNOTS('',3,(#90636,#90637,#90638,#90639,#90640,
#90641,#90642,#90643,#90644,#90645),.UNSPECIFIED.,.F.,.F.,(4,3,3,4),(-4.09274904019423,
-3.97736675155131,-2.98302506366348,-2.06120159751574),.UNSPECIFIED.);
#620=B_SPLINE_CURVE_WITH_KNOTS('',3,(#90648,#90649,#90650,#90651,#90652,
#90653,#90654),.UNSPECIFIED.,.F.,.F.,(4,3,4),(0.,0.994341687887822,1.11004521091126),
 .UNSPECIFIED.);
#621=B_SPLINE_CURVE_WITH_KNOTS('',3,(#90659,#90660,#90661,#90662,#90663,
#90664,#90665,#90666,#90667,#90668,#90669,#90670,#90671,#90672,#90673,#90674,
#90675,#90676,#90677,#90678,#90679,#90680),.UNSPECIFIED.,.F.,.F.,(4,3,3,
3,3,3,3,4),(-10.3759343473738,-9.94341687887826,-8.94907519099043,-7.95473350310261,
-6.96039181521478,-5.96605012732696,-4.97170843943913,-4.09274904019423),
 .UNSPECIFIED.);
#622=B_SPLINE_CURVE_WITH_KNOTS('',3,(#90681,#90682,#90683,#90684,#90685,
#90686,#90687,#90688,#90689,#90690,#90691,#90692,#90693,#90694,#90695,#90696,
#90697,#90698,#90699,#90700,#90701,#90702),.UNSPECIFIED.,.F.,.F.,(4,3,3,
3,3,3,3,4),(1.11004521091126,1.98868337577565,2.98302506366347,3.9773667515513,
4.97170843943912,5.96605012732695,6.96039181521477,7.39323051809085),
 .UNSPECIFIED.);
#623=B_SPLINE_CURVE_WITH_KNOTS('',3,(#90707,#90708,#90709,#90710,#90711,
#90712,#90713,#90714,#90715,#90716,#90717,#90718,#90719,#90720,#90721,#90722,
#90723,#90724,#90725,#90726,#90727,#90728),.UNSPECIFIED.,.F.,.F.,(4,3,3,
3,3,3,3,4),(-16.6591196545534,-15.9094670062052,-14.9151253183174,-13.9207836304296,
-12.9264419425417,-11.9321002546539,-10.9377585667661,-10.3759343473738),
 .UNSPECIFIED.);
#624=B_SPLINE_CURVE_WITH_KNOTS('',3,(#90729,#90730,#90731,#90732,#90733,
#90734,#90735,#90736,#90737,#90738,#90739,#90740,#90741,#90742,#90743,#90744,
#90745,#90746,#90747,#90748,#90749,#90750),.UNSPECIFIED.,.F.,.F.,(4,3,3,
3,3,3,3,4),(7.39323051809085,7.9547335031026,8.94907519099043,9.94341687887826,
10.9377585667661,11.9321002546539,12.9264419425418,13.6764158252704),
 .UNSPECIFIED.);
#625=B_SPLINE_CURVE_WITH_KNOTS('',3,(#90755,#90756,#90757,#90758,#90759,
#90760,#90761,#90762,#90763,#90764,#90765,#90766,#90767,#90768,#90769,#90770,
#90771,#90772,#90773,#90774,#90775,#90776,#90777,#90778,#90779),
 .UNSPECIFIED.,.F.,.F.,(4,3,3,3,3,3,3,3,4),(-22.942304961733,-22.86985882142,
-21.8755171335322,-20.8811754456444,-19.8868337577565,-18.8924920698687,
-17.8981503819809,-16.903808694093,-16.6591196545534),.UNSPECIFIED.);
#626=B_SPLINE_CURVE_WITH_KNOTS('',3,(#90780,#90781,#90782,#90783,#90784,
#90785,#90786,#90787,#90788,#90789,#90790,#90791,#90792,#90793,#90794,#90795,
#90796,#90797,#90798,#90799,#90800,#90801,#90802,#90803,#90804),
 .UNSPECIFIED.,.F.,.F.,(4,3,3,3,3,3,3,3,4),(13.6764158252704,13.9207836304296,
14.9151253183174,15.9094670062052,16.9038086940931,17.8981503819809,18.8924920698687,
19.8868337577565,19.95960113245),.UNSPECIFIED.);
#627=B_SPLINE_CURVE_WITH_KNOTS('',3,(#90809,#90810,#90811,#90812,#90813,
#90814,#90815,#90816,#90817,#90818,#90819,#90820,#90821,#90822,#90823,#90824,
#90825,#90826,#90827,#90828,#90829,#90830),.UNSPECIFIED.,.F.,.F.,(4,3,3,
3,3,3,3,4),(-29.2254902689126,-28.835908948747,-27.8415672608591,-26.8472255729713,
-25.8528838850835,-24.8585421971957,-23.8642005093078,-22.942304961733),
 .UNSPECIFIED.);
#628=B_SPLINE_CURVE_WITH_KNOTS('',3,(#90831,#90832,#90833,#90834,#90835,
#90836,#90837,#90838,#90839,#90840,#90841,#90842,#90843,#90844,#90845,#90846,
#90847,#90848,#90849,#90850,#90851,#90852),.UNSPECIFIED.,.F.,.F.,(4,3,3,
3,3,3,3,4),(19.95960113245,20.8811754456443,21.8755171335322,22.86985882142,
23.8642005093078,24.8585421971956,25.8528838850835,26.2427864396296),
 .UNSPECIFIED.);
#629=B_SPLINE_CURVE_WITH_KNOTS('',3,(#90857,#90858,#90859,#90860,#90861,
#90862,#90863,#90864,#90865,#90866,#90867,#90868,#90869,#90870,#90871,#90872,
#90873,#90874,#90875,#90876,#90877,#90878),.UNSPECIFIED.,.F.,.F.,(4,3,3,
3,3,3,3,4),(-35.5086755760922,-34.8019590760739,-33.8076173881861,-32.8132757002983,
-31.8189340124104,-30.8245923245226,-29.8302506366348,-29.2254902689126),
 .UNSPECIFIED.);
#630=B_SPLINE_CURVE_WITH_KNOTS('',3,(#90879,#90880,#90881,#90882,#90883,
#90884,#90885,#90886,#90887,#90888,#90889,#90890,#90891,#90892,#90893,#90894,
#90895,#90896,#90897,#90898,#90899,#90900),.UNSPECIFIED.,.F.,.F.,(4,3,3,
3,3,3,3,4),(26.2427864396296,26.8472255729713,27.8415672608591,28.8359089487469,
29.8302506366348,30.8245923245226,31.8189340124104,32.5259717468092),
 .UNSPECIFIED.);
#631=B_SPLINE_CURVE_WITH_KNOTS('',3,(#90905,#90906,#90907,#90908,#90909,
#90910,#90911,#90912,#90913,#90914,#90915,#90916,#90917,#90918,#90919,#90920,
#90921,#90922,#90923,#90924,#90925,#90926,#90927,#90928,#90929),
 .UNSPECIFIED.,.F.,.F.,(4,3,3,3,3,3,3,3,4),(-41.7918608832717,-41.7623508912887,
-40.7680092034009,-39.773667515513,-38.7793258276252,-37.7849841397374,
-36.7906424518496,-35.7963007639617,-35.5086755760922),.UNSPECIFIED.);
#632=B_SPLINE_CURVE_WITH_KNOTS('',3,(#90930,#90931,#90932,#90933,#90934,
#90935,#90936,#90937,#90938,#90939,#90940,#90941,#90942,#90943,#90944,#90945,
#90946,#90947,#90948,#90949,#90950,#90951,#90952,#90953,#90954),
 .UNSPECIFIED.,.F.,.F.,(4,3,3,3,3,3,3,3,4),(32.5259717468092,32.8132757002983,
33.8076173881861,34.8019590760739,35.7963007639617,36.7906424518496,37.7849841397374,
38.7793258276252,38.8091570539888),.UNSPECIFIED.);
#633=B_SPLINE_CURVE_WITH_KNOTS('',3,(#90959,#90960,#90961,#90962,#90963,
#90964,#90965,#90966,#90967,#90968,#90969,#90970,#90971,#90972,#90973,#90974,
#90975,#90976,#90977,#90978,#90979,#90980),.UNSPECIFIED.,.F.,.F.,(4,3,3,
3,3,3,3,4),(-48.0750461904514,-47.7284010186156,-46.7340593307278,-45.73971764284,
-44.7453759549522,-43.7510342670644,-42.7566925791765,-41.7918608832717),
 .UNSPECIFIED.);
#634=B_SPLINE_CURVE_WITH_KNOTS('',3,(#90981,#90982,#90983,#90984,#90985,
#90986,#90987,#90988,#90989,#90990,#90991,#90992,#90993,#90994,#90995,#90996,
#90997,#90998,#90999,#91000,#91001,#91002),.UNSPECIFIED.,.F.,.F.,(4,3,3,
3,3,3,3,4),(38.8091570539888,39.773667515513,40.7680092034009,41.7623508912887,
42.7566925791765,43.7510342670643,44.7453759549522,45.0923423611684),
 .UNSPECIFIED.);
#635=B_SPLINE_CURVE_WITH_KNOTS('',3,(#91007,#91008,#91009,#91010,#91011,
#91012,#91013,#91014,#91015,#91016,#91017,#91018,#91019,#91020,#91021,#91022,
#91023,#91024,#91025,#91026,#91027,#91028),.UNSPECIFIED.,.F.,.F.,(4,3,3,
3,3,3,3,4),(-54.3582314976309,-53.6944511459426,-52.7001094580548,-51.705767770167,
-50.7114260822791,-49.7170843943913,-48.7227427065035,-48.0750461904514),
 .UNSPECIFIED.);
#636=B_SPLINE_CURVE_WITH_KNOTS('',3,(#91029,#91030,#91031,#91032,#91033,
#91034,#91035,#91036,#91037,#91038,#91039,#91040,#91041,#91042,#91043,#91044,
#91045,#91046,#91047,#91048,#91049,#91050),.UNSPECIFIED.,.F.,.F.,(4,3,3,
3,3,3,3,4),(45.0923423611684,45.73971764284,46.7340593307278,47.7284010186156,
48.7227427065035,49.7170843943913,50.7114260822791,51.375527668348),
 .UNSPECIFIED.);
#637=B_SPLINE_CURVE_WITH_KNOTS('',3,(#91055,#91056,#91057,#91058,#91059,
#91060,#91061,#91062,#91063,#91064,#91065,#91066,#91067,#91068,#91069,#91070,
#91071,#91072,#91073,#91074,#91075,#91076),.UNSPECIFIED.,.F.,.F.,(4,3,3,
3,3,3,3,4),(-60.6414168048105,-59.6605012732696,-58.6661595853817,-57.6718178974939,
-56.6774762096061,-55.6831345217183,-54.6887928338304,-54.3582314976309),
 .UNSPECIFIED.);
#638=B_SPLINE_CURVE_WITH_KNOTS('',3,(#91077,#91078,#91079,#91080,#91081,
#91082,#91083,#91084,#91085,#91086,#91087,#91088,#91089,#91090,#91091,#91092,
#91093,#91094,#91095,#91096,#91097,#91098),.UNSPECIFIED.,.F.,.F.,(4,3,3,
3,3,3,3,4),(51.375527668348,51.705767770167,52.7001094580548,53.6944511459426,
54.6887928338304,55.6831345217183,56.6774762096061,57.6587129755276),
 .UNSPECIFIED.);
#639=B_SPLINE_CURVE_WITH_KNOTS('',3,(#91103,#91104,#91105,#91106,#91107,
#91108,#91109,#91110,#91111,#91112,#91113,#91114,#91115,#91116,#91117,#91118,
#91119,#91120,#91121,#91122,#91123,#91124,#91125,#91126,#91127),
 .UNSPECIFIED.,.F.,.F.,(4,3,3,3,3,3,3,3,4),(-66.9246021119901,-66.6208930884844,
-65.6265514005965,-64.6322097127087,-63.6378680248209,-62.643526336933,
-61.6491846490452,-60.6548429611574,-60.6414168048105),.UNSPECIFIED.);
#640=B_SPLINE_CURVE_WITH_KNOTS('',3,(#91128,#91129,#91130,#91131,#91132,
#91133,#91134,#91135,#91136,#91137,#91138,#91139,#91140,#91141,#91142,#91143,
#91144,#91145,#91146,#91147,#91148,#91149,#91150,#91151,#91152),
 .UNSPECIFIED.,.F.,.F.,(4,3,3,3,3,3,3,3,4),(57.6587129755276,57.6718178974939,
58.6661595853817,59.6605012732696,60.6548429611574,61.6491846490452,62.643526336933,
63.6378680248209,63.9418982827072),.UNSPECIFIED.);
#641=B_SPLINE_CURVE_WITH_KNOTS('',3,(#91157,#91158,#91159,#91160,#91161,
#91162,#91163,#91164,#91165,#91166,#91167,#91168,#91169,#91170,#91171,#91172,
#91173,#91174,#91175,#91176,#91177,#91178),.UNSPECIFIED.,.F.,.F.,(4,3,3,
3,3,3,3,4),(-73.2077874191697,-72.5869432158113,-71.5926015279235,-70.5982598400356,
-69.6039181521478,-68.60957646426,-67.6152347763722,-66.9246021119901),
 .UNSPECIFIED.);
#642=B_SPLINE_CURVE_WITH_KNOTS('',3,(#91179,#91180,#91181,#91182,#91183,
#91184,#91185,#91186,#91187,#91188,#91189,#91190,#91191,#91192,#91193,#91194,
#91195,#91196,#91197,#91198,#91199,#91200),.UNSPECIFIED.,.F.,.F.,(4,3,3,
3,3,3,3,4),(63.9418982827072,64.6322097127087,65.6265514005965,66.6208930884843,
67.6152347763722,68.60957646426,69.6039181521478,70.2250835898868),
 .UNSPECIFIED.);
#643=B_SPLINE_CURVE_WITH_KNOTS('',3,(#91205,#91206,#91207,#91208,#91209,
#91210,#91211,#91212,#91213,#91214,#91215,#91216,#91217,#91218,#91219,#91220,
#91221,#91222,#91223,#91224,#91225,#91226),.UNSPECIFIED.,.F.,.F.,(4,3,3,
3,3,3,3,4),(-79.4909727263493,-78.5529933431383,-77.5586516552504,-76.5643099673626,
-75.5699682794748,-74.575626591587,-73.5812849036991,-73.2077874191697),
 .UNSPECIFIED.);
#644=B_SPLINE_CURVE_WITH_KNOTS('',3,(#91227,#91228,#91229,#91230,#91231,
#91232,#91233,#91234,#91235,#91236,#91237,#91238,#91239,#91240,#91241,#91242,
#91243,#91244,#91245,#91246,#91247,#91248),.UNSPECIFIED.,.F.,.F.,(4,3,3,
3,3,3,3,4),(70.2250835898868,70.5982598400356,71.5926015279234,72.5869432158113,
73.5812849036991,74.5756265915869,75.5699682794748,76.5082688970663),
 .UNSPECIFIED.);
#645=B_SPLINE_CURVE_WITH_KNOTS('',3,(#91253,#91254,#91255,#91256,#91257,
#91258,#91259,#91260,#91261,#91262,#91263,#91264,#91265,#91266,#91267,#91268,
#91269,#91270,#91271,#91272,#91273,#91274,#91275,#91276,#91277),
 .UNSPECIFIED.,.F.,.F.,(4,3,3,3,3,3,3,3,4),(-85.7741580335289,-85.513385158353,
-84.5190434704652,-83.5247017825774,-82.5303600946896,-81.5360184068017,
-80.5416767189139,-79.5473350310261,-79.4909727263493),.UNSPECIFIED.);
#646=B_SPLINE_CURVE_WITH_KNOTS('',3,(#91278,#91279,#91280,#91281,#91282,
#91283,#91284,#91285,#91286,#91287,#91288,#91289,#91290,#91291,#91292,#91293,
#91294,#91295,#91296,#91297,#91298,#91299,#91300,#91301,#91302),
 .UNSPECIFIED.,.F.,.F.,(4,3,3,3,3,3,3,3,4),(76.5082688970663,76.5643099673626,
77.5586516552504,78.5529933431382,79.5473350310261,80.5416767189139,81.5360184068017,
82.5303600946895,82.7914542042459),.UNSPECIFIED.);
#647=B_SPLINE_CURVE_WITH_KNOTS('',3,(#91307,#91308,#91309,#91310,#91311,
#91312,#91313,#91314,#91315,#91316,#91317,#91318,#91319,#91320,#91321,#91322,
#91323,#91324,#91325,#91326,#91327,#91328),.UNSPECIFIED.,.F.,.F.,(4,3,3,
3,3,3,3,4),(-92.0573433407085,-91.47943528568,-90.4850935977922,-89.4907519099043,
-88.4964102220165,-87.5020685341287,-86.5077268462409,-85.7741580335289),
 .UNSPECIFIED.);
#648=B_SPLINE_CURVE_WITH_KNOTS('',3,(#91329,#91330,#91331,#91332,#91333,
#91334,#91335,#91336,#91337,#91338,#91339,#91340,#91341,#91342,#91343,#91344,
#91345,#91346,#91347,#91348,#91349,#91350),.UNSPECIFIED.,.F.,.F.,(4,3,3,
3,3,3,3,4),(82.7914542042459,83.5247017825774,84.5190434704652,85.513385158353,
86.5077268462408,87.5020685341287,88.4964102220165,89.0746395114255),
 .UNSPECIFIED.);
#649=B_SPLINE_CURVE_WITH_KNOTS('',3,(#91355,#91356,#91357,#91358,#91359,
#91360,#91361,#91362,#91363,#91364,#91365,#91366,#91367,#91368,#91369,#91370,
#91371,#91372,#91373,#91374,#91375,#91376),.UNSPECIFIED.,.F.,.F.,(4,3,3,
3,3,3,3,4),(-98.3405286478881,-97.4454854130069,-96.4511437251191,-95.4568020372313,
-94.4624603493435,-93.4681186614556,-92.4737769735678,-92.0573433407085),
 .UNSPECIFIED.);
#650=B_SPLINE_CURVE_WITH_KNOTS('',3,(#91377,#91378,#91379,#91380,#91381,
#91382,#91383,#91384,#91385,#91386,#91387,#91388,#91389,#91390,#91391,#91392,
#91393,#91394,#91395,#91396,#91397,#91398),.UNSPECIFIED.,.F.,.F.,(4,3,3,
3,3,3,3,4),(89.0746395114255,89.4907519099043,90.4850935977922,91.47943528568,
92.4737769735678,93.4681186614556,94.4624603493435,95.3578248186051),
 .UNSPECIFIED.);
#651=B_SPLINE_CURVE_WITH_KNOTS('',3,(#91403,#91404,#91405,#91406,#91407,
#91408,#91409,#91410,#91411,#91412,#91413,#91414,#91415,#91416,#91417,#91418,
#91419,#91420,#91421,#91422,#91423,#91424,#91425,#91426,#91427),
 .UNSPECIFIED.,.F.,.F.,(4,3,3,3,3,3,3,3,4),(-104.623713955068,-104.405877228222,
-103.411535540334,-102.417193852446,-101.422852164558,-100.42851047667,
-99.4341687887826,-98.4398271008948,-98.3405286478881),.UNSPECIFIED.);
#652=B_SPLINE_CURVE_WITH_KNOTS('',3,(#91428,#91429,#91430,#91431,#91432,
#91433,#91434,#91435,#91436,#91437,#91438,#91439,#91440,#91441,#91442,#91443,
#91444,#91445,#91446,#91447,#91448,#91449,#91450,#91451,#91452),
 .UNSPECIFIED.,.F.,.F.,(4,3,3,3,3,3,3,3,4),(95.3578248186051,95.4568020372313,
96.4511437251191,97.4454854130069,98.4398271008948,99.4341687887826,100.42851047667,
101.422852164558,101.641010125785),.UNSPECIFIED.);
#653=B_SPLINE_CURVE_WITH_KNOTS('',3,(#91457,#91458,#91459,#91460,#91461,
#91462,#91463,#91464,#91465,#91466,#91467,#91468,#91469,#91470,#91471,#91472,
#91473,#91474,#91475,#91476,#91477,#91478),.UNSPECIFIED.,.F.,.F.,(4,3,3,
3,3,3,3,4),(-110.906899262247,-110.371927355549,-109.377585667661,-108.383243979773,
-107.388902291885,-106.394560603997,-105.40021891611,-104.623713955068),
 .UNSPECIFIED.);
#654=B_SPLINE_CURVE_WITH_KNOTS('',3,(#91479,#91480,#91481,#91482,#91483,
#91484,#91485,#91486,#91487,#91488,#91489,#91490,#91491,#91492,#91493,#91494,
#91495,#91496,#91497,#91498,#91499,#91500),.UNSPECIFIED.,.F.,.F.,(4,3,3,
3,3,3,3,4),(101.641010125785,102.417193852446,103.411535540334,104.405877228222,
105.40021891611,106.394560603997,107.388902291885,107.924195432964),
 .UNSPECIFIED.);
#655=B_SPLINE_CURVE_WITH_KNOTS('',3,(#91505,#91506,#91507,#91508,#91509,
#91510,#91511,#91512,#91513,#91514,#91515,#91516,#91517,#91518,#91519,#91520,
#91521,#91522,#91523,#91524,#91525,#91526),.UNSPECIFIED.,.F.,.F.,(4,3,3,
3,3,3,3,4),(-117.190084569427,-116.337977482876,-115.343635794988,-114.3492941071,
-113.354952419212,-112.360610731324,-111.366269043437,-110.906899262247),
 .UNSPECIFIED.);
#656=B_SPLINE_CURVE_WITH_KNOTS('',3,(#91527,#91528,#91529,#91530,#91531,
#91532,#91533,#91534,#91535,#91536,#91537,#91538,#91539,#91540,#91541,#91542,
#91543,#91544,#91545,#91546,#91547,#91548),.UNSPECIFIED.,.F.,.F.,(4,3,3,
3,3,3,3,4),(107.924195432964,108.383243979773,109.377585667661,110.371927355549,
111.366269043437,112.360610731324,113.354952419212,114.207380740144),
 .UNSPECIFIED.);
#657=B_SPLINE_CURVE_WITH_KNOTS('',3,(#91553,#91554,#91555,#91556,#91557,
#91558,#91559,#91560,#91561,#91562,#91563,#91564,#91565,#91566,#91567,#91568,
#91569,#91570,#91571,#91572,#91573,#91574,#91575,#91576,#91577),
 .UNSPECIFIED.,.F.,.F.,(4,3,3,3,3,3,3,3,4),(-123.473269876606,-123.29836929809,
-122.304027610203,-121.309685922315,-120.315344234427,-119.321002546539,
-118.326660858651,-117.332319170763,-117.190084569427),.UNSPECIFIED.);
#658=B_SPLINE_CURVE_WITH_KNOTS('',3,(#91578,#91579,#91580,#91581,#91582,
#91583,#91584,#91585,#91586,#91587,#91588,#91589,#91590,#91591,#91592,#91593,
#91594,#91595,#91596,#91597,#91598,#91599,#91600,#91601,#91602),
 .UNSPECIFIED.,.F.,.F.,(4,3,3,3,3,3,3,3,4),(114.207380740144,114.3492941071,
115.343635794988,116.337977482876,117.332319170763,118.326660858651,119.321002546539,
120.315344234427,120.490566047323),.UNSPECIFIED.);
#659=B_SPLINE_CURVE_WITH_KNOTS('',3,(#91607,#91608,#91609,#91610,#91611,
#91612,#91613,#91614,#91615,#91616,#91617,#91618,#91619,#91620,#91621,#91622,
#91623,#91624,#91625,#91626,#91627,#91628),.UNSPECIFIED.,.F.,.F.,(4,3,3,
3,3,3,3,4),(-129.756455183786,-129.264419425417,-128.27007773753,-127.275736049642,
-126.281394361754,-125.287052673866,-124.292710985978,-123.473269876606),
 .UNSPECIFIED.);
#660=B_SPLINE_CURVE_WITH_KNOTS('',3,(#91629,#91630,#91631,#91632,#91633,
#91634,#91635,#91636,#91637,#91638,#91639,#91640,#91641,#91642,#91643,#91644,
#91645,#91646,#91647,#91648,#91649,#91650),.UNSPECIFIED.,.F.,.F.,(4,3,3,
3,3,3,3,4),(120.490566047323,121.309685922315,122.304027610203,123.29836929809,
124.292710985978,125.287052673866,126.281394361754,126.773751354503),
 .UNSPECIFIED.);
#661=B_SPLINE_CURVE_WITH_KNOTS('',3,(#91655,#91656,#91657,#91658,#91659,
#91660,#91661,#91662,#91663,#91664,#91665,#91666,#91667,#91668,#91669,#91670,
#91671,#91672,#91673,#91674,#91675,#91676),.UNSPECIFIED.,.F.,.F.,(4,3,3,
3,3,3,3,4),(-136.039640490966,-135.230469552744,-134.236127864856,-133.241786176969,
-132.247444489081,-131.253102801193,-130.258761113305,-129.756455183786),
 .UNSPECIFIED.);
#662=B_SPLINE_CURVE_WITH_KNOTS('',3,(#91677,#91678,#91679,#91680,#91681,
#91682,#91683,#91684,#91685,#91686,#91687,#91688,#91689,#91690,#91691,#91692,
#91693,#91694,#91695,#91696,#91697,#91698),.UNSPECIFIED.,.F.,.F.,(4,3,3,
3,3,3,3,4),(126.773751354503,127.275736049642,128.27007773753,129.264419425417,
130.258761113305,131.253102801193,132.247444489081,133.056936661683),
 .UNSPECIFIED.);
#663=B_SPLINE_CURVE_WITH_KNOTS('',3,(#91703,#91704,#91705,#91706,#91707,
#91708,#91709,#91710,#91711,#91712,#91713,#91714,#91715,#91716,#91717,#91718,
#91719,#91720,#91721,#91722,#91723,#91724,#91725,#91726,#91727),
 .UNSPECIFIED.,.F.,.F.,(4,3,3,3,3,3,3,3,4),(-142.322825798145,-142.190861367959,
-141.196519680071,-140.202177992183,-139.207836304296,-138.213494616408,
-137.21915292852,-136.224811240632,-136.039640490966),.UNSPECIFIED.);
#664=B_SPLINE_CURVE_WITH_KNOTS('',3,(#91728,#91729,#91730,#91731,#91732,
#91733,#91734,#91735,#91736,#91737,#91738,#91739,#91740,#91741,#91742,#91743,
#91744,#91745,#91746,#91747,#91748,#91749,#91750,#91751,#91752),
 .UNSPECIFIED.,.F.,.F.,(4,3,3,3,3,3,3,3,4),(133.056936661683,133.241786176969,
134.236127864857,135.230469552744,136.224811240632,137.21915292852,138.213494616408,
139.207836304296,139.340121968862),.UNSPECIFIED.);
#665=B_SPLINE_CURVE_WITH_KNOTS('',3,(#91758,#91759,#91760,#91761,#91762,
#91763),.UNSPECIFIED.,.F.,.F.,(4,1,1,4),(153.9380400259,154.800417283602,
155.79475897149,156.716582437637),.UNSPECIFIED.);
#666=B_SPLINE_CURVE_WITH_KNOTS('',3,(#91766,#91767,#91768,#91769,#91770),
 .UNSPECIFIED.,.F.,.F.,(4,1,4),(153.9380400259,154.482960869368,155.477302557256),
 .UNSPECIFIED.);
#667=B_SPLINE_CURVE_WITH_KNOTS('',3,(#91775,#91776,#91777,#91778,#91779,
#91780,#91781,#91782,#91783,#91784,#91785),.UNSPECIFIED.,.F.,.F.,(4,1,1,
1,1,1,1,1,4),(147.65485471872,147.840025468387,148.834367156275,149.828708844163,
150.82305053205,151.817392219938,152.811733907826,153.806075595714,153.9380400259),
 .UNSPECIFIED.);
#668=B_SPLINE_CURVE_WITH_KNOTS('',3,(#91786,#91787,#91788,#91789,#91790,
#91791,#91792,#91793,#91794,#91795),.UNSPECIFIED.,.F.,.F.,(4,1,1,1,1,1,
1,4),(147.65485471872,148.516910742041,149.511252429929,150.505594117817,
151.499935805705,152.494277493593,153.488619181481,153.9380400259),
 .UNSPECIFIED.);
#669=B_SPLINE_CURVE_WITH_KNOTS('',3,(#91800,#91801,#91802,#91803,#91804,
#91805,#91806,#91807,#91808,#91809),.UNSPECIFIED.,.F.,.F.,(4,1,1,1,1,1,
1,4),(141.371669411541,141.87397534106,142.868317028948,143.862658716836,
144.857000404723,145.851342092611,146.845683780499,147.65485471872),
 .UNSPECIFIED.);
#670=B_SPLINE_CURVE_WITH_KNOTS('',3,(#91810,#91811,#91812,#91813,#91814,
#91815,#91816,#91817,#91818,#91819,#91820),.UNSPECIFIED.,.F.,.F.,(4,1,1,
1,1,1,1,1,4),(141.371669411541,141.556518926827,142.550860614715,143.545202302602,
144.53954399049,145.533885678378,146.528227366266,147.522569054154,147.65485471872),
 .UNSPECIFIED.);
#671=B_SPLINE_CURVE_WITH_KNOTS('',3,(#91825,#91826,#91827,#91828,#91829,
#91830,#91831,#91832,#91833,#91834),.UNSPECIFIED.,.F.,.F.,(4,1,1,1,1,1,
1,4),(135.088484104361,135.907925213733,136.902266901621,137.896608589509,
138.890950277396,139.885291965284,140.879633653172,141.371669411541),
 .UNSPECIFIED.);
#672=B_SPLINE_CURVE_WITH_KNOTS('',3,(#91835,#91836,#91837,#91838,#91839,
#91840,#91841,#91842,#91843,#91844),.UNSPECIFIED.,.F.,.F.,(4,1,1,1,1,1,
1,4),(135.088484104361,135.5904687995,136.584810487388,137.579152175275,
138.573493863163,139.567835551051,140.562177238939,141.371669411541),
 .UNSPECIFIED.);
#673=B_SPLINE_CURVE_WITH_KNOTS('',3,(#91849,#91850,#91851,#91852,#91853,
#91854,#91855,#91856,#91857,#91858,#91859),.UNSPECIFIED.,.F.,.F.,(4,1,1,
1,1,1,1,1,4),(128.805298797182,128.947533398518,129.941875086406,130.936216774294,
131.930558462182,132.92490015007,133.919241837957,134.913583525845,135.088484104361),
 .UNSPECIFIED.);
#674=B_SPLINE_CURVE_WITH_KNOTS('',3,(#91860,#91861,#91862,#91863,#91864,
#91865,#91866,#91867,#91868,#91869),.UNSPECIFIED.,.F.,.F.,(4,1,1,1,1,1,
1,4),(128.805298797182,129.624418672173,130.618760360061,131.613102047948,
132.607443735836,133.601785423724,134.596127111612,135.088484104361),
 .UNSPECIFIED.);
#675=B_SPLINE_CURVE_WITH_KNOTS('',3,(#91874,#91875,#91876,#91877,#91878,
#91879,#91880,#91881,#91882,#91883),.UNSPECIFIED.,.F.,.F.,(4,1,1,1,1,1,
1,4),(122.522113490002,122.981483271191,123.975824959079,124.970166646967,
125.964508334855,126.958850022743,127.95319171063,128.805298797182),
 .UNSPECIFIED.);
#676=B_SPLINE_CURVE_WITH_KNOTS('',3,(#91884,#91885,#91886,#91887,#91888,
#91889,#91890,#91891,#91892,#91893,#91894),.UNSPECIFIED.,.F.,.F.,(4,1,1,
1,1,1,1,1,4),(122.522113490002,122.664026856958,123.658368544846,124.652710232734,
125.647051920622,126.641393608509,127.635735296397,128.630076984285,128.805298797182),
 .UNSPECIFIED.);
#677=B_SPLINE_CURVE_WITH_KNOTS('',3,(#91899,#91900,#91901,#91902,#91903,
#91904,#91905,#91906,#91907,#91908),.UNSPECIFIED.,.F.,.F.,(4,1,1,1,1,1,
1,4),(116.238928182822,117.015433143864,118.009774831752,119.00411651964,
119.998458207528,120.992799895416,121.987141583303,122.522113490002),
 .UNSPECIFIED.);
#678=B_SPLINE_CURVE_WITH_KNOTS('',3,(#91909,#91910,#91911,#91912,#91913,
#91914,#91915,#91916,#91917,#91918),.UNSPECIFIED.,.F.,.F.,(4,1,1,1,1,1,
1,4),(116.238928182822,116.697976729631,117.692318417519,118.686660105407,
119.681001793295,120.675343481182,121.66968516907,122.522113490002),
 .UNSPECIFIED.);
#679=B_SPLINE_CURVE_WITH_KNOTS('',3,(#91923,#91924,#91925,#91926,#91927,
#91928,#91929,#91930,#91931,#91932,#91933),.UNSPECIFIED.,.F.,.F.,(4,1,1,
1,1,1,1,1,4),(109.955742875643,110.05504132865,111.049383016537,112.043724704425,
113.038066392313,114.032408080201,115.026749768089,116.021091455976,116.238928182822),
 .UNSPECIFIED.);
#680=B_SPLINE_CURVE_WITH_KNOTS('',3,(#91934,#91935,#91936,#91937,#91938,
#91939,#91940,#91941,#91942,#91943),.UNSPECIFIED.,.F.,.F.,(4,1,1,1,1,1,
1,4),(109.955742875643,110.731926602304,111.726268290192,112.72060997808,
113.714951665968,114.709293353855,115.703635041743,116.238928182822),
 .UNSPECIFIED.);
#681=B_SPLINE_CURVE_WITH_KNOTS('',3,(#91948,#91949,#91950,#91951,#91952,
#91953,#91954,#91955,#91956,#91957),.UNSPECIFIED.,.F.,.F.,(4,1,1,1,1,1,
1,4),(103.672557568463,104.088991201323,105.08333288921,106.077674577098,
107.072016264986,108.066357952874,109.060699640762,109.955742875643),
 .UNSPECIFIED.);
#682=B_SPLINE_CURVE_WITH_KNOTS('',3,(#91958,#91959,#91960,#91961,#91962,
#91963,#91964,#91965,#91966,#91967,#91968),.UNSPECIFIED.,.F.,.F.,(4,1,1,
1,1,1,1,1,4),(103.672557568463,103.771534787089,104.765876474977,105.760218162865,
106.754559850753,107.748901538641,108.743243226528,109.737584914416,109.955742875643),
 .UNSPECIFIED.);
#683=B_SPLINE_CURVE_WITH_KNOTS('',3,(#91973,#91974,#91975,#91976,#91977,
#91978,#91979,#91980,#91981,#91982),.UNSPECIFIED.,.F.,.F.,(4,1,1,1,1,1,
1,4),(97.3893722612836,98.1229410739956,99.1172827618834,100.111624449771,
101.105966137659,102.100307825547,103.094649513435,103.672557568463),
 .UNSPECIFIED.);
#684=B_SPLINE_CURVE_WITH_KNOTS('',3,(#91983,#91984,#91985,#91986,#91987,
#91988,#91989,#91990,#91991,#91992),.UNSPECIFIED.,.F.,.F.,(4,1,1,1,1,1,
1,4),(97.3893722612836,97.8054846597624,98.7998263476502,99.794168035538,
100.788509723426,101.782851411314,102.777193099202,103.672557568463),
 .UNSPECIFIED.);
#685=B_SPLINE_CURVE_WITH_KNOTS('',3,(#91997,#91998,#91999,#92000,#92001,
#92002,#92003,#92004,#92005,#92006,#92007),.UNSPECIFIED.,.F.,.F.,(4,1,1,
1,1,1,1,1,4),(91.106186954104,91.1625492587808,92.1568909466686,93.1512326345565,
94.1455743224443,95.1399160103321,96.13425769822,97.1285993861078,97.3893722612836),
 .UNSPECIFIED.);
#686=B_SPLINE_CURVE_WITH_KNOTS('',3,(#92008,#92009,#92010,#92011,#92012,
#92013,#92014,#92015,#92016,#92017),.UNSPECIFIED.,.F.,.F.,(4,1,1,1,1,1,
1,4),(91.106186954104,91.8394345324354,92.8337762203232,93.8281179082111,
94.8224595960989,95.8168012839867,96.8111429718745,97.3893722612836),
 .UNSPECIFIED.);
#687=B_SPLINE_CURVE_WITH_KNOTS('',3,(#92022,#92023,#92024,#92025,#92026,
#92027,#92028,#92029,#92030,#92031),.UNSPECIFIED.,.F.,.F.,(4,1,1,1,1,1,
1,4),(84.8230016469244,85.1964991314539,86.1908408193417,87.1851825072295,
88.1795241951173,89.1738658830052,90.168207570893,91.106186954104),
 .UNSPECIFIED.);
#688=B_SPLINE_CURVE_WITH_KNOTS('',3,(#92032,#92033,#92034,#92035,#92036,
#92037,#92038,#92039,#92040,#92041,#92042),.UNSPECIFIED.,.F.,.F.,(4,1,1,
1,1,1,1,1,4),(84.8230016469244,84.8790427172206,85.8733844051085,86.8677260929963,
87.8620677808841,88.8564094687719,89.8507511566598,90.8450928445476,91.106186954104),
 .UNSPECIFIED.);
#689=B_SPLINE_CURVE_WITH_KNOTS('',3,(#92047,#92048,#92049,#92050,#92051,
#92052,#92053,#92054,#92055,#92056),.UNSPECIFIED.,.F.,.F.,(4,1,1,1,1,1,
1,4),(78.5398163397448,79.2304490041269,80.2247906920147,81.2191323799026,
82.2134740677904,83.2078157556782,84.202157443566,84.8230016469244),
 .UNSPECIFIED.);
#690=B_SPLINE_CURVE_WITH_KNOTS('',3,(#92057,#92058,#92059,#92060,#92061,
#92062,#92063,#92064,#92065,#92066),.UNSPECIFIED.,.F.,.F.,(4,1,1,1,1,1,
1,4),(78.5398163397448,78.9129925898937,79.9073342777815,80.9016759656693,
81.8960176535572,82.890359341445,83.8847010293328,84.8230016469244),
 .UNSPECIFIED.);
#691=B_SPLINE_CURVE_WITH_KNOTS('',3,(#92071,#92072,#92073,#92074,#92075,
#92076,#92077,#92078,#92079,#92080,#92081),.UNSPECIFIED.,.F.,.F.,(4,1,1,
1,1,1,1,1,4),(72.2566310325653,72.2700571889121,73.2643988768,74.2587405646878,
75.2530822525756,76.2474239404634,77.2417656283513,78.2361073162391,78.5398163397448),
 .UNSPECIFIED.);
#692=B_SPLINE_CURVE_WITH_KNOTS('',3,(#92082,#92083,#92084,#92085,#92086,
#92087,#92088,#92089,#92090,#92091),.UNSPECIFIED.,.F.,.F.,(4,1,1,1,1,1,
1,4),(72.2566310325653,72.9469424625667,73.9412841504546,74.9356258383424,
75.9299675262302,76.924309214118,77.9186509020059,78.5398163397448),
 .UNSPECIFIED.);
#693=B_SPLINE_CURVE_WITH_KNOTS('',3,(#92096,#92097,#92098,#92099,#92100,
#92101,#92102,#92103,#92104,#92105),.UNSPECIFIED.,.F.,.F.,(4,1,1,1,1,1,
1,4),(65.9734457253856,66.3040070615852,67.298348749473,68.2926904373608,
69.2870321252486,70.2813738131365,71.2757155010243,72.2566310325653),
 .UNSPECIFIED.);
#694=B_SPLINE_CURVE_WITH_KNOTS('',3,(#92106,#92107,#92108,#92109,#92110,
#92111,#92112,#92113,#92114,#92115,#92116),.UNSPECIFIED.,.F.,.F.,(4,1,1,
1,1,1,1,1,4),(65.9734457253856,65.9865506473519,66.9808923352398,67.9752340231276,
68.9695757110154,69.9639173989032,70.9582590867911,71.9526007746789,72.2566310325653),
 .UNSPECIFIED.);
#695=B_SPLINE_CURVE_WITH_KNOTS('',3,(#92121,#92122,#92123,#92124,#92125,
#92126,#92127,#92128,#92129,#92130),.UNSPECIFIED.,.F.,.F.,(4,1,1,1,1,1,
1,4),(59.6902604182061,60.3379569342582,61.332298622146,62.3266403100339,
63.3209819979217,64.3153236858095,65.3096653736973,65.9734457253856),
 .UNSPECIFIED.);
#696=B_SPLINE_CURVE_WITH_KNOTS('',3,(#92131,#92132,#92133,#92134,#92135,
#92136,#92137,#92138,#92139,#92140),.UNSPECIFIED.,.F.,.F.,(4,1,1,1,1,1,
1,4),(59.6902604182061,60.020500520025,61.0148422079128,62.0091838958006,
63.0035255836885,63.9978672715763,64.9922089594641,65.9734457253856),
 .UNSPECIFIED.);
#697=B_SPLINE_CURVE_WITH_KNOTS('',3,(#92145,#92146,#92147,#92148,#92149,
#92150,#92151,#92152,#92153,#92154),.UNSPECIFIED.,.F.,.F.,(4,1,1,1,1,1,
1,4),(53.4070751110265,54.3719068069313,55.3662484948191,56.3605901827069,
57.3549318705947,58.3492735584826,59.3436152463704,59.6902604182061),
 .UNSPECIFIED.);
#698=B_SPLINE_CURVE_WITH_KNOTS('',3,(#92155,#92156,#92157,#92158,#92159,
#92160,#92161,#92162,#92163,#92164),.UNSPECIFIED.,.F.,.F.,(4,1,1,1,1,1,
1,4),(53.4070751110265,54.054450392698,55.0487920805859,56.0431337684737,
57.0374754563615,58.0318171442493,59.0261588321372,59.6902604182061),
 .UNSPECIFIED.);
#699=B_SPLINE_CURVE_WITH_KNOTS('',3,(#92169,#92170,#92171,#92172,#92173,
#92174,#92175,#92176,#92177,#92178,#92179),.UNSPECIFIED.,.F.,.F.,(4,1,1,
1,1,1,1,1,4),(47.1238898038469,47.4115149917165,48.4058566796043,49.4001983674921,
50.3945400553799,51.3888817432678,52.3832234311556,53.3775651190434,53.4070751110265),
 .UNSPECIFIED.);
#700=B_SPLINE_CURVE_WITH_KNOTS('',3,(#92180,#92181,#92182,#92183,#92184,
#92185,#92186,#92187,#92188,#92189),.UNSPECIFIED.,.F.,.F.,(4,1,1,1,1,1,
1,4),(47.1238898038469,48.0884002653711,49.0827419532589,50.0770836411467,
51.0714253290346,52.0657670169224,53.0601087048102,53.4070751110265),
 .UNSPECIFIED.);
#701=B_SPLINE_CURVE_WITH_KNOTS('',3,(#92194,#92195,#92196,#92197,#92198,
#92199,#92200,#92201,#92202,#92203),.UNSPECIFIED.,.F.,.F.,(4,1,1,1,1,1,
1,4),(40.8407044966673,41.4454648643895,42.4398065522773,43.4341482401652,
44.428489928053,45.4228316159408,46.4171733038286,47.1238898038469),
 .UNSPECIFIED.);
#702=B_SPLINE_CURVE_WITH_KNOTS('',3,(#92204,#92205,#92206,#92207,#92208,
#92209,#92210,#92211,#92212,#92213,#92214),.UNSPECIFIED.,.F.,.F.,(4,1,1,
1,1,1,1,1,4),(40.8407044966673,41.1280084501563,42.1223501380441,43.116691825932,
44.1110335138198,45.1053752017076,46.0997168895954,47.0940585774833,47.1238898038469),
 .UNSPECIFIED.);
#703=B_SPLINE_CURVE_WITH_KNOTS('',3,(#92219,#92220,#92221,#92222,#92223,
#92224,#92225,#92226,#92227,#92228),.UNSPECIFIED.,.F.,.F.,(4,1,1,1,1,1,
1,4),(34.5575191894877,35.4794147370626,36.4737564249504,37.4680981128382,
38.462439800726,39.4567814886139,40.4511231765017,40.8407044966673),
 .UNSPECIFIED.);
#704=B_SPLINE_CURVE_WITH_KNOTS('',3,(#92229,#92230,#92231,#92232,#92233,
#92234,#92235,#92236,#92237,#92238),.UNSPECIFIED.,.F.,.F.,(4,1,1,1,1,1,
1,4),(34.5575191894877,35.1619583228293,36.1563000107172,37.150641698605,
38.1449833864928,39.1393250743807,40.1336667622685,40.8407044966673),
 .UNSPECIFIED.);
#705=B_SPLINE_CURVE_WITH_KNOTS('',3,(#92243,#92244,#92245,#92246,#92247,
#92248,#92249,#92250,#92251,#92252,#92253),.UNSPECIFIED.,.F.,.F.,(4,1,1,
1,1,1,1,1,4),(28.2743338823081,28.5190229218478,29.5133646097356,30.5077062976234,
31.5020479855113,32.4963896733991,33.4907313612869,34.4850730491747,34.5575191894877),
 .UNSPECIFIED.);
#706=B_SPLINE_CURVE_WITH_KNOTS('',3,(#92254,#92255,#92256,#92257,#92258,
#92259,#92260,#92261,#92262,#92263),.UNSPECIFIED.,.F.,.F.,(4,1,1,1,1,1,
1,4),(28.2743338823081,29.1959081955024,30.1902498833902,31.184591571278,
32.1789332591659,33.1732749470537,34.1676166349415,34.5575191894877),
 .UNSPECIFIED.);
#707=B_SPLINE_CURVE_WITH_KNOTS('',3,(#92268,#92269,#92270,#92271,#92272,
#92273,#92274,#92275,#92276,#92277),.UNSPECIFIED.,.F.,.F.,(4,1,1,1,1,1,
1,4),(21.9911485751285,22.5529727945208,23.5473144824086,24.5416561702965,
25.5359978581843,26.5303395460721,27.52468123396,28.2743338823081),
 .UNSPECIFIED.);
#708=B_SPLINE_CURVE_WITH_KNOTS('',3,(#92278,#92279,#92280,#92281,#92282,
#92283,#92284,#92285,#92286,#92287,#92288),.UNSPECIFIED.,.F.,.F.,(4,1,1,
1,1,1,1,1,4),(21.9911485751285,22.2355163802876,23.2298580681754,24.2241997560633,
25.2185414439511,26.2128831318389,27.2072248197267,28.2015665076146,28.2743338823081),
 .UNSPECIFIED.);
#709=B_SPLINE_CURVE_WITH_KNOTS('',3,(#92293,#92294,#92295,#92296,#92297,
#92298,#92299,#92300,#92301,#92302),.UNSPECIFIED.,.F.,.F.,(4,1,1,1,1,1,
1,4),(15.7079632679489,16.5869226671939,17.5812643550817,18.5756060429695,
19.5699477308573,20.5642894187452,21.558631106633,21.9911485751285),
 .UNSPECIFIED.);
#710=B_SPLINE_CURVE_WITH_KNOTS('',3,(#92303,#92304,#92305,#92306,#92307,
#92308,#92309,#92310,#92311,#92312),.UNSPECIFIED.,.F.,.F.,(4,1,1,1,1,1,
1,4),(15.7079632679489,16.2694662529607,17.2638079408485,18.2581496287363,
19.2524913166241,20.246833004512,21.2411746923998,21.9911485751285),
 .UNSPECIFIED.);
#711=B_SPLINE_CURVE_WITH_KNOTS('',3,(#92315,#92316,#92317,#92318,#92319,
#92320,#92321,#92322,#92323,#92324,#92325,#92326,#92327,#92328,#92329,#92330,
#92331,#92332,#92333,#92334,#92335,#92336,#92337,#92338,#92339,#92340,#92341,
#92342,#92343,#92344,#92345,#92346,#92347,#92348,#92349,#92350,#92351,#92352,
#92353,#92354,#92355,#92356,#92357,#92358,#92359,#92360,#92361,#92362,#92363,
#92364,#92365,#92366,#92367,#92368,#92369,#92370,#92371,#92372,#92373,#92374,
#92375,#92376,#92377,#92378,#92379,#92380,#92381,#92382,#92383,#92384,#92385,
#92386,#92387,#92388,#92389,#92390,#92391,#92392,#92393,#92394,#92395,#92396,
#92397,#92398,#92399,#92400,#92401,#92402,#92403,#92404,#92405,#92406,#92407,
#92408,#92409,#92410,#92411),.UNSPECIFIED.,.F.,.F.,(4,3,3,3,3,3,3,3,3,3,
3,3,3,3,3,3,3,3,3,3,3,3,3,3,3,3,3,3,3,3,3,3,4),(-0.744397949170625,-0.720695733926605,
-0.689559276510196,-0.670036103351393,-0.659844114683856,-0.653655602764569,
-0.621646994773415,-0.591089683672906,-0.577510322236719,-0.571672000985749,
-0.566558200256387,-0.533181563358221,-0.499287246195234,-0.465487035108622,
-0.443412402823803,-0.436945256166294,-0.431748865628828,-0.396836613409468,
-0.377188505969346,-0.343448059020756,-0.309075827600796,-0.297163948119586,
-0.292811939195563,-0.258415064258314,-0.222910728343378,-0.187071424676623,
-0.163687496592045,-0.150656708009009,-0.145666602593747,-0.108928864805471,
-0.0721282795251585,-0.0360213506839708,0.),.UNSPECIFIED.);
#712=B_SPLINE_CURVE_WITH_KNOTS('',3,(#92416,#92417,#92418,#92419,#92420,
#92421,#92422,#92423,#92424,#92425,#92426,#92427,#92428,#92429,#92430,#92431,
#92432,#92433,#92434,#92435,#92436,#92437,#92438,#92439,#92440,#92441,#92442,
#92443,#92444,#92445,#92446,#92447,#92448,#92449,#92450,#92451,#92452,#92453,
#92454,#92455,#92456,#92457,#92458,#92459,#92460,#92461,#92462,#92463,#92464,
#92465,#92466,#92467,#92468,#92469,#92470,#92471,#92472,#92473,#92474,#92475,
#92476,#92477,#92478,#92479,#92480,#92481,#92482,#92483,#92484,#92485,#92486,
#92487,#92488,#92489,#92490,#92491,#92492,#92493,#92494,#92495,#92496,#92497,
#92498,#92499,#92500,#92501,#92502,#92503,#92504,#92505,#92506,#92507,#92508,
#92509,#92510,#92511,#92512),.UNSPECIFIED.,.F.,.F.,(4,3,3,3,3,3,3,3,3,3,
3,3,3,3,3,3,3,3,3,3,3,3,3,3,3,3,3,3,3,3,3,3,4),(-0.741270768406274,-0.712807950605837,
-0.676238641188094,-0.655219890693859,-0.642041516507432,-0.635990628203364,
-0.598984128837985,-0.566603441893278,-0.552436891354969,-0.544103215434064,
-0.537640090039063,-0.502240448549675,-0.467092661838385,-0.432981215367342,
-0.409720569845589,-0.402357089590634,-0.397540473388326,-0.363890224767345,
-0.339938633280332,-0.305661805073138,-0.27125659544551,-0.263740502835797,
-0.257191774771573,-0.223767368565723,-0.190306650667009,-0.157253142518131,
-0.137596499703365,-0.128270421992769,-0.123230695487105,-0.0910288793094783,
-0.0592786340288667,-0.0285032472800834,0.),.UNSPECIFIED.);
#713=B_SPLINE_CURVE_WITH_KNOTS('',3,(#93117,#93118,#93119,#93120,#93121,
#93122,#93123,#93124,#93125,#93126,#93127,#93128,#93129,#93130,#93131,#93132,
#93133,#93134,#93135),.UNSPECIFIED.,.F.,.F.,(4,3,3,3,3,3,4),(139.340121968862,
140.202177992183,141.196519680071,142.190861367959,143.185203055847,144.179544743735,
145.101368209882),.UNSPECIFIED.);
#714=B_SPLINE_CURVE_WITH_KNOTS('',3,(#93137,#93138,#93139,#93140,#93141,
#93142,#93143,#93144,#93145,#93146,#93147,#93148,#93149,#93150,#93151,#93152,
#93153,#93154,#93155,#93156,#93157,#93158,#93159,#93160,#93161,#93162,#93163,
#93164,#93165,#93166,#93167,#93168,#93169,#93170,#93171,#93172,#93173,#93174,
#93175,#93176,#93177,#93178,#93179,#93180,#93181,#93182,#93183,#93184,#93185,
#93186,#93187,#93188,#93189,#93190,#93191,#93192,#93193,#93194,#93195,#93196,
#93197,#93198,#93199,#93200,#93201,#93202,#93203,#93204,#93205,#93206,#93207,
#93208,#93209,#93210,#93211,#93212,#93213,#93214,#93215,#93216,#93217,#93218,
#93219,#93220,#93221,#93222,#93223,#93224,#93225,#93226,#93227,#93228,#93229,
#93230,#93231,#93232,#93233),.UNSPECIFIED.,.F.,.F.,(4,3,3,3,3,3,3,3,3,3,
3,3,3,3,3,3,3,3,3,3,3,3,3,3,3,3,3,3,3,3,3,3,4),(-0.744397949170602,-0.720695733926586,
-0.6895592934692,-0.670036119250459,-0.659844170884589,-0.653655608554017,
-0.621647015639673,-0.591089701930882,-0.577510352001926,-0.571671825159275,
-0.566558171753553,-0.533181542619665,-0.499287226983445,-0.465487016280342,
-0.443412388702592,-0.436945445960127,-0.431748880838135,-0.39683662780105,
-0.377188505969343,-0.343448066421773,-0.309075843625405,-0.297163975261819,
-0.292811966402081,-0.258415099070131,-0.222910772035957,-0.187071472120164,
-0.163687538105144,-0.150656788140358,-0.145666622445593,-0.108928889508498,
-0.072128300796967,-0.0360213509544539,0.),.UNSPECIFIED.);
#715=B_SPLINE_CURVE_WITH_KNOTS('',3,(#93234,#93235,#93236,#93237,#93238,
#93239,#93240,#93241,#93242),.UNSPECIFIED.,.F.,.F.,(4,1,1,1,1,1,4),(10.3759343473738,
11.2977578135215,12.2920995014094,13.2864411892972,14.280782877185,15.2751245650728,
15.7079632679489),.UNSPECIFIED.);
#716=B_SPLINE_CURVE_WITH_KNOTS('',3,(#93248,#93249,#93250,#93251,#93252,
#93253,#93254,#93255,#93256,#93257,#93258,#93259,#93260,#93261,#93262,#93263,
#93264,#93265,#93266,#93267,#93268,#93269,#93270,#93271,#93272,#93273,#93274,
#93275,#93276,#93277,#93278,#93279,#93280,#93281,#93282,#93283,#93284,#93285,
#93286,#93287,#93288,#93289,#93290,#93291,#93292,#93293,#93294,#93295,#93296,
#93297,#93298,#93299,#93300,#93301,#93302,#93303,#93304,#93305,#93306,#93307,
#93308,#93309,#93310,#93311,#93312,#93313,#93314,#93315,#93316,#93317,#93318,
#93319,#93320,#93321,#93322,#93323,#93324,#93325,#93326,#93327,#93328,#93329,
#93330,#93331,#93332,#93333,#93334,#93335,#93336,#93337,#93338,#93339,#93340,
#93341,#93342,#93343,#93344),.UNSPECIFIED.,.F.,.F.,(4,3,3,3,3,3,3,3,3,3,
3,3,3,3,3,3,3,3,3,3,3,3,3,3,3,3,3,3,3,3,3,3,4),(-0.741270768406348,-0.712807950605888,
-0.676238640305255,-0.655219889866198,-0.642041511505912,-0.635990623215072,
-0.598984124473231,-0.566603438074119,-0.552436887774508,-0.544103204743418,
-0.537640086026196,-0.50224044348667,-0.467092649849235,-0.432981184709489,
-0.409720546852202,-0.402357044665001,-0.397540380185969,-0.36389011877745,
-0.33993863328034,-0.305661795379487,-0.271256588274296,-0.263740488713404,
-0.2571917764368,-0.223767364341805,-0.190306652230719,-0.15725316132804,
-0.137596516162035,-0.128270487710825,-0.123230703086563,-0.091028901639038,
-0.0592786783268478,-0.0285033201413548,0.),.UNSPECIFIED.);
#717=B_SPLINE_CURVE_WITH_KNOTS('',3,(#93347,#93348,#93349,#93350,#93351,
#93352,#93353,#93354),.UNSPECIFIED.,.F.,.F.,(4,1,1,1,1,4),(11.6152142277547,
12.6095559156426,13.6038976035304,14.5982392914182,15.592580979306,15.7079632679489),
 .UNSPECIFIED.);
#718=B_SPLINE_CURVE_WITH_KNOTS('',3,(#93959,#93960,#93961,#93962,#93963,
#93964,#93965,#93966,#93967,#93968,#93969,#93970,#93971,#93972,#93973,#93974),
 .UNSPECIFIED.,.F.,.F.,(4,3,3,3,3,4),(-147.162569807398,-146.16822811951,
-145.173886431623,-144.179544743735,-143.185203055847,-142.322825798145),
 .UNSPECIFIED.);
#719=B_SPLINE_SURFACE_WITH_KNOTS('',2,1,((#80625,#80626),(#80627,#80628),
(#80629,#80630)),.UNSPECIFIED.,.F.,.F.,.F.,(3,3),(2,2),(0.,1.),(0.,0.03),
 .UNSPECIFIED.);
#720=B_SPLINE_SURFACE_WITH_KNOTS('',2,1,((#80643,#80644),(#80645,#80646),
(#80647,#80648)),.UNSPECIFIED.,.F.,.F.,.F.,(3,3),(2,2),(0.,1.),(0.,0.03),
 .UNSPECIFIED.);
#721=B_SPLINE_SURFACE_WITH_KNOTS('',2,1,((#80658,#80659),(#80660,#80661),
(#80662,#80663)),.UNSPECIFIED.,.F.,.F.,.F.,(3,3),(2,2),(0.,1.),(0.,0.03),
 .UNSPECIFIED.);
#722=B_SPLINE_SURFACE_WITH_KNOTS('',2,1,((#80673,#80674),(#80675,#80676),
(#80677,#80678)),.UNSPECIFIED.,.F.,.F.,.F.,(3,3),(2,2),(0.,1.),(0.,0.03),
 .UNSPECIFIED.);
#723=B_SPLINE_SURFACE_WITH_KNOTS('',2,1,((#80688,#80689),(#80690,#80691),
(#80692,#80693)),.UNSPECIFIED.,.F.,.F.,.F.,(3,3),(2,2),(0.,1.),(0.,0.03),
 .UNSPECIFIED.);
#724=B_SPLINE_SURFACE_WITH_KNOTS('',2,1,((#80703,#80704),(#80705,#80706),
(#80707,#80708)),.UNSPECIFIED.,.F.,.F.,.F.,(3,3),(2,2),(0.,1.),(0.,0.03),
 .UNSPECIFIED.);
#725=B_SPLINE_SURFACE_WITH_KNOTS('',2,1,((#80718,#80719),(#80720,#80721),
(#80722,#80723)),.UNSPECIFIED.,.F.,.F.,.F.,(3,3),(2,2),(0.,1.),(0.,0.03),
 .UNSPECIFIED.);
#726=B_SPLINE_SURFACE_WITH_KNOTS('',2,1,((#80733,#80734),(#80735,#80736),
(#80737,#80738)),.UNSPECIFIED.,.F.,.F.,.F.,(3,3),(2,2),(0.,1.),(0.,0.03),
 .UNSPECIFIED.);
#727=B_SPLINE_SURFACE_WITH_KNOTS('',2,1,((#80748,#80749),(#80750,#80751),
(#80752,#80753)),.UNSPECIFIED.,.F.,.F.,.F.,(3,3),(2,2),(0.,1.),(0.,0.03),
 .UNSPECIFIED.);
#728=B_SPLINE_SURFACE_WITH_KNOTS('',2,1,((#80763,#80764),(#80765,#80766),
(#80767,#80768)),.UNSPECIFIED.,.F.,.F.,.F.,(3,3),(2,2),(0.,1.),(0.,0.03),
 .UNSPECIFIED.);
#729=B_SPLINE_SURFACE_WITH_KNOTS('',2,1,((#80778,#80779),(#80780,#80781),
(#80782,#80783)),.UNSPECIFIED.,.F.,.F.,.F.,(3,3),(2,2),(0.,1.),(0.,0.03),
 .UNSPECIFIED.);
#730=B_SPLINE_SURFACE_WITH_KNOTS('',2,1,((#80793,#80794),(#80795,#80796),
(#80797,#80798)),.UNSPECIFIED.,.F.,.F.,.F.,(3,3),(2,2),(0.,1.),(0.,0.03),
 .UNSPECIFIED.);
#731=B_SPLINE_SURFACE_WITH_KNOTS('',2,1,((#80808,#80809),(#80810,#80811),
(#80812,#80813)),.UNSPECIFIED.,.F.,.F.,.F.,(3,3),(2,2),(0.,1.),(0.,0.03),
 .UNSPECIFIED.);
#732=B_SPLINE_SURFACE_WITH_KNOTS('',2,1,((#80829,#80830),(#80831,#80832),
(#80833,#80834)),.UNSPECIFIED.,.F.,.F.,.F.,(3,3),(2,2),(0.,1.),(0.,0.03),
 .UNSPECIFIED.);
#733=B_SPLINE_SURFACE_WITH_KNOTS('',2,1,((#80844,#80845),(#80846,#80847),
(#80848,#80849)),.UNSPECIFIED.,.F.,.F.,.F.,(3,3),(2,2),(0.,1.),(0.,0.03),
 .UNSPECIFIED.);
#734=B_SPLINE_SURFACE_WITH_KNOTS('',2,1,((#80859,#80860),(#80861,#80862),
(#80863,#80864)),.UNSPECIFIED.,.F.,.F.,.F.,(3,3),(2,2),(0.,1.),(0.,0.03),
 .UNSPECIFIED.);
#735=B_SPLINE_SURFACE_WITH_KNOTS('',2,1,((#80874,#80875),(#80876,#80877),
(#80878,#80879)),.UNSPECIFIED.,.F.,.F.,.F.,(3,3),(2,2),(0.,1.),(0.,0.03),
 .UNSPECIFIED.);
#736=B_SPLINE_SURFACE_WITH_KNOTS('',2,1,((#80889,#80890),(#80891,#80892),
(#80893,#80894)),.UNSPECIFIED.,.F.,.F.,.F.,(3,3),(2,2),(0.,1.),(0.,0.03),
 .UNSPECIFIED.);
#737=B_SPLINE_SURFACE_WITH_KNOTS('',2,1,((#80904,#80905),(#80906,#80907),
(#80908,#80909)),.UNSPECIFIED.,.F.,.F.,.F.,(3,3),(2,2),(0.,1.),(0.,0.03),
 .UNSPECIFIED.);
#738=B_SPLINE_SURFACE_WITH_KNOTS('',2,1,((#80919,#80920),(#80921,#80922),
(#80923,#80924)),.UNSPECIFIED.,.F.,.F.,.F.,(3,3),(2,2),(0.,1.),(0.,0.03),
 .UNSPECIFIED.);
#739=B_SPLINE_SURFACE_WITH_KNOTS('',2,1,((#80934,#80935),(#80936,#80937),
(#80938,#80939)),.UNSPECIFIED.,.F.,.F.,.F.,(3,3),(2,2),(0.,1.),(0.,0.03),
 .UNSPECIFIED.);
#740=B_SPLINE_SURFACE_WITH_KNOTS('',2,1,((#80949,#80950),(#80951,#80952),
(#80953,#80954)),.UNSPECIFIED.,.F.,.F.,.F.,(3,3),(2,2),(0.,1.),(0.,0.03),
 .UNSPECIFIED.);
#741=B_SPLINE_SURFACE_WITH_KNOTS('',2,1,((#80964,#80965),(#80966,#80967),
(#80968,#80969)),.UNSPECIFIED.,.F.,.F.,.F.,(3,3),(2,2),(0.,1.),(0.,0.03),
 .UNSPECIFIED.);
#742=B_SPLINE_SURFACE_WITH_KNOTS('',2,1,((#80979,#80980),(#80981,#80982),
(#80983,#80984)),.UNSPECIFIED.,.F.,.F.,.F.,(3,3),(2,2),(0.,1.),(0.,0.03),
 .UNSPECIFIED.);
#743=B_SPLINE_SURFACE_WITH_KNOTS('',2,1,((#80994,#80995),(#80996,#80997),
(#80998,#80999)),.UNSPECIFIED.,.F.,.F.,.F.,(3,3),(2,2),(0.,1.),(0.,0.03),
 .UNSPECIFIED.);
#744=B_SPLINE_SURFACE_WITH_KNOTS('',2,1,((#81009,#81010),(#81011,#81012),
(#81013,#81014)),.UNSPECIFIED.,.F.,.F.,.F.,(3,3),(2,2),(0.,1.),(0.,0.03),
 .UNSPECIFIED.);
#745=B_SPLINE_SURFACE_WITH_KNOTS('',2,1,((#81024,#81025),(#81026,#81027),
(#81028,#81029)),.UNSPECIFIED.,.F.,.F.,.F.,(3,3),(2,2),(0.,1.),(0.,0.03),
 .UNSPECIFIED.);
#746=B_SPLINE_SURFACE_WITH_KNOTS('',2,1,((#81039,#81040),(#81041,#81042),
(#81043,#81044)),.UNSPECIFIED.,.F.,.F.,.F.,(3,3),(2,2),(0.,1.),(0.,0.03),
 .UNSPECIFIED.);
#747=B_SPLINE_SURFACE_WITH_KNOTS('',2,1,((#81054,#81055),(#81056,#81057),
(#81058,#81059)),.UNSPECIFIED.,.F.,.F.,.F.,(3,3),(2,2),(0.,1.),(0.,0.03),
 .UNSPECIFIED.);
#748=B_SPLINE_SURFACE_WITH_KNOTS('',2,1,((#81069,#81070),(#81071,#81072),
(#81073,#81074)),.UNSPECIFIED.,.F.,.F.,.F.,(3,3),(2,2),(0.,1.),(0.,0.03),
 .UNSPECIFIED.);
#749=B_SPLINE_SURFACE_WITH_KNOTS('',2,1,((#81084,#81085),(#81086,#81087),
(#81088,#81089)),.UNSPECIFIED.,.F.,.F.,.F.,(3,3),(2,2),(0.,1.),(0.,0.03),
 .UNSPECIFIED.);
#750=B_SPLINE_SURFACE_WITH_KNOTS('',2,1,((#81105,#81106),(#81107,#81108),
(#81109,#81110)),.UNSPECIFIED.,.F.,.F.,.F.,(3,3),(2,2),(0.,1.),(0.,0.03),
 .UNSPECIFIED.);
#751=B_SPLINE_SURFACE_WITH_KNOTS('',2,1,((#81120,#81121),(#81122,#81123),
(#81124,#81125)),.UNSPECIFIED.,.F.,.F.,.F.,(3,3),(2,2),(0.,1.),(0.,0.03),
 .UNSPECIFIED.);
#752=B_SPLINE_SURFACE_WITH_KNOTS('',2,1,((#81133,#81134),(#81135,#81136),
(#81137,#81138)),.UNSPECIFIED.,.F.,.F.,.F.,(3,3),(2,2),(0.,1.),(0.,0.03),
 .UNSPECIFIED.);
#753=B_SPLINE_SURFACE_WITH_KNOTS('',2,1,((#81151,#81152),(#81153,#81154),
(#81155,#81156)),.UNSPECIFIED.,.F.,.F.,.F.,(3,3),(2,2),(0.,1.),(0.,0.03),
 .UNSPECIFIED.);
#754=B_SPLINE_SURFACE_WITH_KNOTS('',2,1,((#81166,#81167),(#81168,#81169),
(#81170,#81171)),.UNSPECIFIED.,.F.,.F.,.F.,(3,3),(2,2),(0.,1.),(0.,0.03),
 .UNSPECIFIED.);
#755=B_SPLINE_SURFACE_WITH_KNOTS('',2,1,((#81181,#81182),(#81183,#81184),
(#81185,#81186)),.UNSPECIFIED.,.F.,.F.,.F.,(3,3),(2,2),(0.,1.),(0.,0.03),
 .UNSPECIFIED.);
#756=B_SPLINE_SURFACE_WITH_KNOTS('',2,1,((#81196,#81197),(#81198,#81199),
(#81200,#81201)),.UNSPECIFIED.,.F.,.F.,.F.,(3,3),(2,2),(0.,1.),(0.,0.03),
 .UNSPECIFIED.);
#757=B_SPLINE_SURFACE_WITH_KNOTS('',2,1,((#81211,#81212),(#81213,#81214),
(#81215,#81216)),.UNSPECIFIED.,.F.,.F.,.F.,(3,3),(2,2),(0.,1.),(0.,0.03),
 .UNSPECIFIED.);
#758=B_SPLINE_SURFACE_WITH_KNOTS('',2,1,((#81226,#81227),(#81228,#81229),
(#81230,#81231)),.UNSPECIFIED.,.F.,.F.,.F.,(3,3),(2,2),(0.,1.),(0.,0.03),
 .UNSPECIFIED.);
#759=B_SPLINE_SURFACE_WITH_KNOTS('',2,1,((#81241,#81242),(#81243,#81244),
(#81245,#81246)),.UNSPECIFIED.,.F.,.F.,.F.,(3,3),(2,2),(0.,1.),(0.,0.03),
 .UNSPECIFIED.);
#760=B_SPLINE_SURFACE_WITH_KNOTS('',2,1,((#81262,#81263),(#81264,#81265),
(#81266,#81267)),.UNSPECIFIED.,.F.,.F.,.F.,(3,3),(2,2),(0.,1.),(0.,0.03),
 .UNSPECIFIED.);
#761=B_SPLINE_SURFACE_WITH_KNOTS('',2,1,((#81277,#81278),(#81279,#81280),
(#81281,#81282)),.UNSPECIFIED.,.F.,.F.,.F.,(3,3),(2,2),(0.,1.),(0.,0.03),
 .UNSPECIFIED.);
#762=B_SPLINE_SURFACE_WITH_KNOTS('',2,1,((#81292,#81293),(#81294,#81295),
(#81296,#81297)),.UNSPECIFIED.,.F.,.F.,.F.,(3,3),(2,2),(0.,1.),(0.,0.03),
 .UNSPECIFIED.);
#763=B_SPLINE_SURFACE_WITH_KNOTS('',2,1,((#81307,#81308),(#81309,#81310),
(#81311,#81312)),.UNSPECIFIED.,.F.,.F.,.F.,(3,3),(2,2),(0.,1.),(0.,0.03),
 .UNSPECIFIED.);
#764=B_SPLINE_SURFACE_WITH_KNOTS('',2,1,((#81322,#81323),(#81324,#81325),
(#81326,#81327)),.UNSPECIFIED.,.F.,.F.,.F.,(3,3),(2,2),(0.,1.),(0.,0.03),
 .UNSPECIFIED.);
#765=B_SPLINE_SURFACE_WITH_KNOTS('',2,1,((#81337,#81338),(#81339,#81340),
(#81341,#81342)),.UNSPECIFIED.,.F.,.F.,.F.,(3,3),(2,2),(0.,1.),(0.,0.03),
 .UNSPECIFIED.);
#766=B_SPLINE_SURFACE_WITH_KNOTS('',2,1,((#81352,#81353),(#81354,#81355),
(#81356,#81357)),.UNSPECIFIED.,.F.,.F.,.F.,(3,3),(2,2),(0.,1.),(0.,0.03),
 .UNSPECIFIED.);
#767=B_SPLINE_SURFACE_WITH_KNOTS('',2,1,((#81367,#81368),(#81369,#81370),
(#81371,#81372)),.UNSPECIFIED.,.F.,.F.,.F.,(3,3),(2,2),(0.,1.),(0.,0.03),
 .UNSPECIFIED.);
#768=B_SPLINE_SURFACE_WITH_KNOTS('',2,1,((#81382,#81383),(#81384,#81385),
(#81386,#81387)),.UNSPECIFIED.,.F.,.F.,.F.,(3,3),(2,2),(0.,1.),(0.,0.03),
 .UNSPECIFIED.);
#769=B_SPLINE_SURFACE_WITH_KNOTS('',2,1,((#81397,#81398),(#81399,#81400),
(#81401,#81402)),.UNSPECIFIED.,.F.,.F.,.F.,(3,3),(2,2),(0.,1.),(0.,0.03),
 .UNSPECIFIED.);
#770=B_SPLINE_SURFACE_WITH_KNOTS('',2,1,((#81418,#81419),(#81420,#81421),
(#81422,#81423)),.UNSPECIFIED.,.F.,.F.,.F.,(3,3),(2,2),(0.,1.),(0.,0.03),
 .UNSPECIFIED.);
#771=B_SPLINE_SURFACE_WITH_KNOTS('',2,1,((#81433,#81434),(#81435,#81436),
(#81437,#81438)),.UNSPECIFIED.,.F.,.F.,.F.,(3,3),(2,2),(0.,1.),(0.,0.03),
 .UNSPECIFIED.);
#772=B_SPLINE_SURFACE_WITH_KNOTS('',2,1,((#81532,#81533),(#81534,#81535),
(#81536,#81537)),.UNSPECIFIED.,.F.,.F.,.F.,(3,3),(2,2),(0.,1.),(0.,0.03),
 .UNSPECIFIED.);
#773=B_SPLINE_SURFACE_WITH_KNOTS('',2,1,((#81550,#81551),(#81552,#81553),
(#81554,#81555)),.UNSPECIFIED.,.F.,.F.,.F.,(3,3),(2,2),(0.,1.),(0.,0.03),
 .UNSPECIFIED.);
#774=B_SPLINE_SURFACE_WITH_KNOTS('',2,1,((#81565,#81566),(#81567,#81568),
(#81569,#81570)),.UNSPECIFIED.,.F.,.F.,.F.,(3,3),(2,2),(0.,1.),(0.,0.03),
 .UNSPECIFIED.);
#775=B_SPLINE_SURFACE_WITH_KNOTS('',2,1,((#81580,#81581),(#81582,#81583),
(#81584,#81585)),.UNSPECIFIED.,.F.,.F.,.F.,(3,3),(2,2),(0.,1.),(0.,0.03),
 .UNSPECIFIED.);
#776=B_SPLINE_SURFACE_WITH_KNOTS('',2,1,((#81613,#81614),(#81615,#81616),
(#81617,#81618)),.UNSPECIFIED.,.F.,.F.,.F.,(3,3),(2,2),(0.,1.),(0.,0.03),
 .UNSPECIFIED.);
#777=B_SPLINE_SURFACE_WITH_KNOTS('',2,1,((#81628,#81629),(#81630,#81631),
(#81632,#81633)),.UNSPECIFIED.,.F.,.F.,.F.,(3,3),(2,2),(0.,1.),(0.,0.03),
 .UNSPECIFIED.);
#778=B_SPLINE_SURFACE_WITH_KNOTS('',2,1,((#81643,#81644),(#81645,#81646),
(#81647,#81648)),.UNSPECIFIED.,.F.,.F.,.F.,(3,3),(2,2),(0.,1.),(0.,0.03),
 .UNSPECIFIED.);
#779=B_SPLINE_SURFACE_WITH_KNOTS('',2,1,((#81658,#81659),(#81660,#81661),
(#81662,#81663)),.UNSPECIFIED.,.F.,.F.,.F.,(3,3),(2,2),(0.,1.),(0.,0.03),
 .UNSPECIFIED.);
#780=B_SPLINE_SURFACE_WITH_KNOTS('',2,1,((#81673,#81674),(#81675,#81676),
(#81677,#81678)),.UNSPECIFIED.,.F.,.F.,.F.,(3,3),(2,2),(0.,1.),(0.,0.03),
 .UNSPECIFIED.);
#781=B_SPLINE_SURFACE_WITH_KNOTS('',2,1,((#81688,#81689),(#81690,#81691),
(#81692,#81693)),.UNSPECIFIED.,.F.,.F.,.F.,(3,3),(2,2),(0.,1.),(0.,0.03),
 .UNSPECIFIED.);
#782=B_SPLINE_SURFACE_WITH_KNOTS('',2,1,((#81721,#81722),(#81723,#81724),
(#81725,#81726)),.UNSPECIFIED.,.F.,.F.,.F.,(3,3),(2,2),(0.,1.),(0.,0.03),
 .UNSPECIFIED.);
#783=B_SPLINE_SURFACE_WITH_KNOTS('',2,1,((#81743,#81744),(#81745,#81746),
(#81747,#81748)),.UNSPECIFIED.,.F.,.F.,.F.,(3,3),(2,2),(0.,1.),(0.,0.03),
 .UNSPECIFIED.);
#784=B_SPLINE_SURFACE_WITH_KNOTS('',2,1,((#81758,#81759),(#81760,#81761),
(#81762,#81763)),.UNSPECIFIED.,.F.,.F.,.F.,(3,3),(2,2),(0.,1.),(0.,0.03),
 .UNSPECIFIED.);
#785=B_SPLINE_SURFACE_WITH_KNOTS('',2,1,((#81773,#81774),(#81775,#81776),
(#81777,#81778)),.UNSPECIFIED.,.F.,.F.,.F.,(3,3),(2,2),(0.,1.),(0.,0.03),
 .UNSPECIFIED.);
#786=B_SPLINE_SURFACE_WITH_KNOTS('',2,1,((#81788,#81789),(#81790,#81791),
(#81792,#81793)),.UNSPECIFIED.,.F.,.F.,.F.,(3,3),(2,2),(0.,1.),(0.,0.03),
 .UNSPECIFIED.);
#787=B_SPLINE_SURFACE_WITH_KNOTS('',2,1,((#81821,#81822),(#81823,#81824),
(#81825,#81826)),.UNSPECIFIED.,.F.,.F.,.F.,(3,3),(2,2),(0.,1.),(0.,0.03),
 .UNSPECIFIED.);
#788=B_SPLINE_SURFACE_WITH_KNOTS('',2,1,((#81836,#81837),(#81838,#81839),
(#81840,#81841)),.UNSPECIFIED.,.F.,.F.,.F.,(3,3),(2,2),(0.,1.),(0.,0.03),
 .UNSPECIFIED.);
#789=B_SPLINE_SURFACE_WITH_KNOTS('',2,1,((#81851,#81852),(#81853,#81854),
(#81855,#81856)),.UNSPECIFIED.,.F.,.F.,.F.,(3,3),(2,2),(0.,1.),(0.,0.03),
 .UNSPECIFIED.);
#790=B_SPLINE_SURFACE_WITH_KNOTS('',2,1,((#81866,#81867),(#81868,#81869),
(#81870,#81871)),.UNSPECIFIED.,.F.,.F.,.F.,(3,3),(2,2),(0.,1.),(0.,0.03),
 .UNSPECIFIED.);
#791=B_SPLINE_SURFACE_WITH_KNOTS('',2,1,((#81881,#81882),(#81883,#81884),
(#81885,#81886)),.UNSPECIFIED.,.F.,.F.,.F.,(3,3),(2,2),(0.,1.),(0.,0.03),
 .UNSPECIFIED.);
#792=B_SPLINE_SURFACE_WITH_KNOTS('',2,1,((#81896,#81897),(#81898,#81899),
(#81900,#81901)),.UNSPECIFIED.,.F.,.F.,.F.,(3,3),(2,2),(0.,1.),(0.,0.03),
 .UNSPECIFIED.);
#793=B_SPLINE_SURFACE_WITH_KNOTS('',2,1,((#81911,#81912),(#81913,#81914),
(#81915,#81916)),.UNSPECIFIED.,.F.,.F.,.F.,(3,3),(2,2),(0.,1.),(0.,0.03),
 .UNSPECIFIED.);
#794=B_SPLINE_SURFACE_WITH_KNOTS('',2,1,((#81997,#81998),(#81999,#82000),
(#82001,#82002)),.UNSPECIFIED.,.F.,.F.,.F.,(3,3),(2,2),(0.,1.),(0.,0.03),
 .UNSPECIFIED.);
#795=B_SPLINE_SURFACE_WITH_KNOTS('',2,1,((#82015,#82016),(#82017,#82018),
(#82019,#82020)),.UNSPECIFIED.,.F.,.F.,.F.,(3,3),(2,2),(0.,1.),(0.,0.03),
 .UNSPECIFIED.);
#796=B_SPLINE_SURFACE_WITH_KNOTS('',2,1,((#82036,#82037),(#82038,#82039),
(#82040,#82041)),.UNSPECIFIED.,.F.,.F.,.F.,(3,3),(2,2),(0.,1.),(0.,0.03),
 .UNSPECIFIED.);
#797=B_SPLINE_SURFACE_WITH_KNOTS('',2,1,((#82051,#82052),(#82053,#82054),
(#82055,#82056)),.UNSPECIFIED.,.F.,.F.,.F.,(3,3),(2,2),(0.,1.),(0.,0.03),
 .UNSPECIFIED.);
#798=B_SPLINE_SURFACE_WITH_KNOTS('',2,1,((#82088,#82089),(#82090,#82091),
(#82092,#82093)),.UNSPECIFIED.,.F.,.F.,.F.,(3,3),(2,2),(0.,1.),(0.,0.03),
 .UNSPECIFIED.);
#799=B_SPLINE_SURFACE_WITH_KNOTS('',2,1,((#82106,#82107),(#82108,#82109),
(#82110,#82111)),.UNSPECIFIED.,.F.,.F.,.F.,(3,3),(2,2),(0.,1.),(0.,0.03),
 .UNSPECIFIED.);
#800=B_SPLINE_SURFACE_WITH_KNOTS('',2,1,((#82121,#82122),(#82123,#82124),
(#82125,#82126)),.UNSPECIFIED.,.F.,.F.,.F.,(3,3),(2,2),(0.,1.),(0.,0.03),
 .UNSPECIFIED.);
#801=B_SPLINE_SURFACE_WITH_KNOTS('',2,1,((#82136,#82137),(#82138,#82139),
(#82140,#82141)),.UNSPECIFIED.,.F.,.F.,.F.,(3,3),(2,2),(0.,1.),(0.,0.03),
 .UNSPECIFIED.);
#802=B_SPLINE_SURFACE_WITH_KNOTS('',2,1,((#82151,#82152),(#82153,#82154),
(#82155,#82156)),.UNSPECIFIED.,.F.,.F.,.F.,(3,3),(2,2),(0.,1.),(0.,0.03),
 .UNSPECIFIED.);
#803=B_SPLINE_SURFACE_WITH_KNOTS('',2,1,((#82166,#82167),(#82168,#82169),
(#82170,#82171)),.UNSPECIFIED.,.F.,.F.,.F.,(3,3),(2,2),(0.,1.),(0.,0.03),
 .UNSPECIFIED.);
#804=B_SPLINE_SURFACE_WITH_KNOTS('',2,1,((#82181,#82182),(#82183,#82184),
(#82185,#82186)),.UNSPECIFIED.,.F.,.F.,.F.,(3,3),(2,2),(0.,1.),(0.,0.03),
 .UNSPECIFIED.);
#805=B_SPLINE_SURFACE_WITH_KNOTS('',2,1,((#82196,#82197),(#82198,#82199),
(#82200,#82201)),.UNSPECIFIED.,.F.,.F.,.F.,(3,3),(2,2),(0.,1.),(0.,0.03),
 .UNSPECIFIED.);
#806=B_SPLINE_SURFACE_WITH_KNOTS('',2,1,((#82211,#82212),(#82213,#82214),
(#82215,#82216)),.UNSPECIFIED.,.F.,.F.,.F.,(3,3),(2,2),(0.,1.),(0.,0.03),
 .UNSPECIFIED.);
#807=B_SPLINE_SURFACE_WITH_KNOTS('',2,1,((#82226,#82227),(#82228,#82229),
(#82230,#82231)),.UNSPECIFIED.,.F.,.F.,.F.,(3,3),(2,2),(0.,1.),(0.,0.03),
 .UNSPECIFIED.);
#808=B_SPLINE_SURFACE_WITH_KNOTS('',2,1,((#82241,#82242),(#82243,#82244),
(#82245,#82246)),.UNSPECIFIED.,.F.,.F.,.F.,(3,3),(2,2),(0.,1.),(0.,0.03),
 .UNSPECIFIED.);
#809=B_SPLINE_SURFACE_WITH_KNOTS('',2,1,((#82256,#82257),(#82258,#82259),
(#82260,#82261)),.UNSPECIFIED.,.F.,.F.,.F.,(3,3),(2,2),(0.,1.),(0.,0.03),
 .UNSPECIFIED.);
#810=B_SPLINE_SURFACE_WITH_KNOTS('',2,1,((#82269,#82270),(#82271,#82272),
(#82273,#82274)),.UNSPECIFIED.,.F.,.F.,.F.,(3,3),(2,2),(0.,1.),(0.,0.03),
 .UNSPECIFIED.);
#811=B_SPLINE_SURFACE_WITH_KNOTS('',2,1,((#82287,#82288),(#82289,#82290),
(#82291,#82292)),.UNSPECIFIED.,.F.,.F.,.F.,(3,3),(2,2),(0.,1.),(0.,0.03),
 .UNSPECIFIED.);
#812=B_SPLINE_SURFACE_WITH_KNOTS('',2,1,((#82308,#82309),(#82310,#82311),
(#82312,#82313)),.UNSPECIFIED.,.F.,.F.,.F.,(3,3),(2,2),(0.,1.),(0.,0.03),
 .UNSPECIFIED.);
#813=B_SPLINE_SURFACE_WITH_KNOTS('',2,1,((#82323,#82324),(#82325,#82326),
(#82327,#82328)),.UNSPECIFIED.,.F.,.F.,.F.,(3,3),(2,2),(0.,1.),(0.,0.03),
 .UNSPECIFIED.);
#814=B_SPLINE_SURFACE_WITH_KNOTS('',2,1,((#82385,#82386),(#82387,#82388),
(#82389,#82390)),.UNSPECIFIED.,.F.,.F.,.F.,(3,3),(2,2),(0.,1.),(0.,0.03),
 .UNSPECIFIED.);
#815=B_SPLINE_SURFACE_WITH_KNOTS('',2,1,((#82403,#82404),(#82405,#82406),
(#82407,#82408)),.UNSPECIFIED.,.F.,.F.,.F.,(3,3),(2,2),(0.,1.),(0.,0.03),
 .UNSPECIFIED.);
#816=B_SPLINE_SURFACE_WITH_KNOTS('',2,1,((#82418,#82419),(#82420,#82421),
(#82422,#82423)),.UNSPECIFIED.,.F.,.F.,.F.,(3,3),(2,2),(0.,1.),(0.,0.03),
 .UNSPECIFIED.);
#817=B_SPLINE_SURFACE_WITH_KNOTS('',2,1,((#82433,#82434),(#82435,#82436),
(#82437,#82438)),.UNSPECIFIED.,.F.,.F.,.F.,(3,3),(2,2),(0.,1.),(0.,0.03),
 .UNSPECIFIED.);
#818=B_SPLINE_SURFACE_WITH_KNOTS('',2,1,((#82448,#82449),(#82450,#82451),
(#82452,#82453)),.UNSPECIFIED.,.F.,.F.,.F.,(3,3),(2,2),(0.,1.),(0.,0.03),
 .UNSPECIFIED.);
#819=B_SPLINE_SURFACE_WITH_KNOTS('',2,1,((#82499,#82500),(#82501,#82502),
(#82503,#82504)),.UNSPECIFIED.,.F.,.F.,.F.,(3,3),(2,2),(0.,1.),(0.,0.03),
 .UNSPECIFIED.);
#820=B_SPLINE_SURFACE_WITH_KNOTS('',2,1,((#82514,#82515),(#82516,#82517),
(#82518,#82519)),.UNSPECIFIED.,.F.,.F.,.F.,(3,3),(2,2),(0.,1.),(0.,0.03),
 .UNSPECIFIED.);
#821=B_SPLINE_SURFACE_WITH_KNOTS('',2,1,((#82529,#82530),(#82531,#82532),
(#82533,#82534)),.UNSPECIFIED.,.F.,.F.,.F.,(3,3),(2,2),(0.,1.),(0.,0.03),
 .UNSPECIFIED.);
#822=B_SPLINE_SURFACE_WITH_KNOTS('',2,1,((#82544,#82545),(#82546,#82547),
(#82548,#82549)),.UNSPECIFIED.,.F.,.F.,.F.,(3,3),(2,2),(0.,1.),(0.,0.03),
 .UNSPECIFIED.);
#823=B_SPLINE_SURFACE_WITH_KNOTS('',2,1,((#82559,#82560),(#82561,#82562),
(#82563,#82564)),.UNSPECIFIED.,.F.,.F.,.F.,(3,3),(2,2),(0.,1.),(0.,0.03),
 .UNSPECIFIED.);
#824=B_SPLINE_SURFACE_WITH_KNOTS('',2,1,((#82574,#82575),(#82576,#82577),
(#82578,#82579)),.UNSPECIFIED.,.F.,.F.,.F.,(3,3),(2,2),(0.,1.),(0.,0.03),
 .UNSPECIFIED.);
#825=B_SPLINE_SURFACE_WITH_KNOTS('',2,1,((#82589,#82590),(#82591,#82592),
(#82593,#82594)),.UNSPECIFIED.,.F.,.F.,.F.,(3,3),(2,2),(0.,1.),(0.,0.03),
 .UNSPECIFIED.);
#826=B_SPLINE_SURFACE_WITH_KNOTS('',2,1,((#82604,#82605),(#82606,#82607),
(#82608,#82609)),.UNSPECIFIED.,.F.,.F.,.F.,(3,3),(2,2),(0.,1.),(0.,0.03),
 .UNSPECIFIED.);
#827=B_SPLINE_SURFACE_WITH_KNOTS('',2,1,((#82625,#82626),(#82627,#82628),
(#82629,#82630)),.UNSPECIFIED.,.F.,.F.,.F.,(3,3),(2,2),(0.,1.),(0.,0.03),
 .UNSPECIFIED.);
#828=B_SPLINE_SURFACE_WITH_KNOTS('',2,1,((#82640,#82641),(#82642,#82643),
(#82644,#82645)),.UNSPECIFIED.,.F.,.F.,.F.,(3,3),(2,2),(0.,1.),(0.,0.03),
 .UNSPECIFIED.);
#829=B_SPLINE_SURFACE_WITH_KNOTS('',2,1,((#82653,#82654),(#82655,#82656),
(#82657,#82658)),.UNSPECIFIED.,.F.,.F.,.F.,(3,3),(2,2),(0.,1.),(0.,0.03),
 .UNSPECIFIED.);
#830=B_SPLINE_SURFACE_WITH_KNOTS('',2,1,((#82671,#82672),(#82673,#82674),
(#82675,#82676)),.UNSPECIFIED.,.F.,.F.,.F.,(3,3),(2,2),(0.,1.),(0.,0.03),
 .UNSPECIFIED.);
#831=B_SPLINE_SURFACE_WITH_KNOTS('',2,1,((#82686,#82687),(#82688,#82689),
(#82690,#82691)),.UNSPECIFIED.,.F.,.F.,.F.,(3,3),(2,2),(0.,1.),(0.,0.03),
 .UNSPECIFIED.);
#832=B_SPLINE_SURFACE_WITH_KNOTS('',2,1,((#82701,#82702),(#82703,#82704),
(#82705,#82706)),.UNSPECIFIED.,.F.,.F.,.F.,(3,3),(2,2),(0.,1.),(0.,0.03),
 .UNSPECIFIED.);
#833=B_SPLINE_SURFACE_WITH_KNOTS('',2,1,((#82716,#82717),(#82718,#82719),
(#82720,#82721)),.UNSPECIFIED.,.F.,.F.,.F.,(3,3),(2,2),(0.,1.),(0.,0.03),
 .UNSPECIFIED.);
#834=B_SPLINE_SURFACE_WITH_KNOTS('',2,1,((#82731,#82732),(#82733,#82734),
(#82735,#82736)),.UNSPECIFIED.,.F.,.F.,.F.,(3,3),(2,2),(0.,1.),(0.,0.03),
 .UNSPECIFIED.);
#835=B_SPLINE_SURFACE_WITH_KNOTS('',2,1,((#82746,#82747),(#82748,#82749),
(#82750,#82751)),.UNSPECIFIED.,.F.,.F.,.F.,(3,3),(2,2),(0.,1.),(0.,0.03),
 .UNSPECIFIED.);
#836=B_SPLINE_SURFACE_WITH_KNOTS('',2,1,((#82761,#82762),(#82763,#82764),
(#82765,#82766)),.UNSPECIFIED.,.F.,.F.,.F.,(3,3),(2,2),(0.,1.),(0.,0.03),
 .UNSPECIFIED.);
#837=B_SPLINE_SURFACE_WITH_KNOTS('',2,1,((#82776,#82777),(#82778,#82779),
(#82780,#82781)),.UNSPECIFIED.,.F.,.F.,.F.,(3,3),(2,2),(0.,1.),(0.,0.03),
 .UNSPECIFIED.);
#838=B_SPLINE_SURFACE_WITH_KNOTS('',2,1,((#82791,#82792),(#82793,#82794),
(#82795,#82796)),.UNSPECIFIED.,.F.,.F.,.F.,(3,3),(2,2),(0.,1.),(0.,0.03),
 .UNSPECIFIED.);
#839=B_SPLINE_SURFACE_WITH_KNOTS('',2,1,((#82806,#82807),(#82808,#82809),
(#82810,#82811)),.UNSPECIFIED.,.F.,.F.,.F.,(3,3),(2,2),(0.,1.),(0.,0.03),
 .UNSPECIFIED.);
#840=B_SPLINE_SURFACE_WITH_KNOTS('',2,1,((#82819,#82820),(#82821,#82822),
(#82823,#82824)),.UNSPECIFIED.,.F.,.F.,.F.,(3,3),(2,2),(0.,1.),(0.,0.03),
 .UNSPECIFIED.);
#841=B_SPLINE_SURFACE_WITH_KNOTS('',2,1,((#82837,#82838),(#82839,#82840),
(#82841,#82842)),.UNSPECIFIED.,.F.,.F.,.F.,(3,3),(2,2),(0.,1.),(0.,0.03),
 .UNSPECIFIED.);
#842=B_SPLINE_SURFACE_WITH_KNOTS('',2,1,((#82852,#82853),(#82854,#82855),
(#82856,#82857)),.UNSPECIFIED.,.F.,.F.,.F.,(3,3),(2,2),(0.,1.),(0.,0.03),
 .UNSPECIFIED.);
#843=B_SPLINE_SURFACE_WITH_KNOTS('',2,1,((#82867,#82868),(#82869,#82870),
(#82871,#82872)),.UNSPECIFIED.,.F.,.F.,.F.,(3,3),(2,2),(0.,1.),(0.,0.03),
 .UNSPECIFIED.);
#844=B_SPLINE_SURFACE_WITH_KNOTS('',2,1,((#82882,#82883),(#82884,#82885),
(#82886,#82887)),.UNSPECIFIED.,.F.,.F.,.F.,(3,3),(2,2),(0.,1.),(0.,0.03),
 .UNSPECIFIED.);
#845=B_SPLINE_SURFACE_WITH_KNOTS('',2,1,((#82897,#82898),(#82899,#82900),
(#82901,#82902)),.UNSPECIFIED.,.F.,.F.,.F.,(3,3),(2,2),(0.,1.),(0.,0.03),
 .UNSPECIFIED.);
#846=B_SPLINE_SURFACE_WITH_KNOTS('',2,1,((#82912,#82913),(#82914,#82915),
(#82916,#82917)),.UNSPECIFIED.,.F.,.F.,.F.,(3,3),(2,2),(0.,1.),(0.,0.03),
 .UNSPECIFIED.);
#847=B_SPLINE_SURFACE_WITH_KNOTS('',2,1,((#82927,#82928),(#82929,#82930),
(#82931,#82932)),.UNSPECIFIED.,.F.,.F.,.F.,(3,3),(2,2),(0.,1.),(0.,0.03),
 .UNSPECIFIED.);
#848=B_SPLINE_SURFACE_WITH_KNOTS('',2,1,((#82942,#82943),(#82944,#82945),
(#82946,#82947)),.UNSPECIFIED.,.F.,.F.,.F.,(3,3),(2,2),(0.,1.),(0.,0.03),
 .UNSPECIFIED.);
#849=B_SPLINE_SURFACE_WITH_KNOTS('',2,1,((#82957,#82958),(#82959,#82960),
(#82961,#82962)),.UNSPECIFIED.,.F.,.F.,.F.,(3,3),(2,2),(0.,1.),(0.,0.03),
 .UNSPECIFIED.);
#850=B_SPLINE_SURFACE_WITH_KNOTS('',2,1,((#82972,#82973),(#82974,#82975),
(#82976,#82977)),.UNSPECIFIED.,.F.,.F.,.F.,(3,3),(2,2),(0.,1.),(0.,0.03),
 .UNSPECIFIED.);
#851=B_SPLINE_SURFACE_WITH_KNOTS('',2,1,((#82993,#82994),(#82995,#82996),
(#82997,#82998)),.UNSPECIFIED.,.F.,.F.,.F.,(3,3),(2,2),(0.,1.),(0.,0.03),
 .UNSPECIFIED.);
#852=B_SPLINE_SURFACE_WITH_KNOTS('',2,1,((#83008,#83009),(#83010,#83011),
(#83012,#83013)),.UNSPECIFIED.,.F.,.F.,.F.,(3,3),(2,2),(0.,1.),(0.,0.03),
 .UNSPECIFIED.);
#853=B_SPLINE_SURFACE_WITH_KNOTS('',2,1,((#83023,#83024),(#83025,#83026),
(#83027,#83028)),.UNSPECIFIED.,.F.,.F.,.F.,(3,3),(2,2),(0.,1.),(0.,0.03),
 .UNSPECIFIED.);
#854=B_SPLINE_SURFACE_WITH_KNOTS('',2,1,((#83134,#83135),(#83136,#83137),
(#83138,#83139)),.UNSPECIFIED.,.F.,.F.,.F.,(3,3),(2,2),(0.,1.),(0.,0.03),
 .UNSPECIFIED.);
#855=B_SPLINE_SURFACE_WITH_KNOTS('',2,1,((#83152,#83153),(#83154,#83155),
(#83156,#83157)),.UNSPECIFIED.,.F.,.F.,.F.,(3,3),(2,2),(0.,1.),(0.,0.03),
 .UNSPECIFIED.);
#856=B_SPLINE_SURFACE_WITH_KNOTS('',2,1,((#83167,#83168),(#83169,#83170),
(#83171,#83172)),.UNSPECIFIED.,.F.,.F.,.F.,(3,3),(2,2),(0.,1.),(0.,0.03),
 .UNSPECIFIED.);
#857=B_SPLINE_SURFACE_WITH_KNOTS('',2,1,((#83182,#83183),(#83184,#83185),
(#83186,#83187)),.UNSPECIFIED.,.F.,.F.,.F.,(3,3),(2,2),(0.,1.),(0.,0.03),
 .UNSPECIFIED.);
#858=B_SPLINE_SURFACE_WITH_KNOTS('',2,1,((#83197,#83198),(#83199,#83200),
(#83201,#83202)),.UNSPECIFIED.,.F.,.F.,.F.,(3,3),(2,2),(0.,1.),(0.,0.03),
 .UNSPECIFIED.);
#859=B_SPLINE_SURFACE_WITH_KNOTS('',2,1,((#83212,#83213),(#83214,#83215),
(#83216,#83217)),.UNSPECIFIED.,.F.,.F.,.F.,(3,3),(2,2),(0.,1.),(0.,0.03),
 .UNSPECIFIED.);
#860=B_SPLINE_SURFACE_WITH_KNOTS('',2,1,((#83227,#83228),(#83229,#83230),
(#83231,#83232)),.UNSPECIFIED.,.F.,.F.,.F.,(3,3),(2,2),(0.,1.),(0.,0.03),
 .UNSPECIFIED.);
#861=B_SPLINE_SURFACE_WITH_KNOTS('',2,1,((#83242,#83243),(#83244,#83245),
(#83246,#83247)),.UNSPECIFIED.,.F.,.F.,.F.,(3,3),(2,2),(0.,1.),(0.,0.03),
 .UNSPECIFIED.);
#862=B_SPLINE_SURFACE_WITH_KNOTS('',2,1,((#83257,#83258),(#83259,#83260),
(#83261,#83262)),.UNSPECIFIED.,.F.,.F.,.F.,(3,3),(2,2),(0.,1.),(0.,0.03),
 .UNSPECIFIED.);
#863=B_SPLINE_SURFACE_WITH_KNOTS('',2,1,((#83272,#83273),(#83274,#83275),
(#83276,#83277)),.UNSPECIFIED.,.F.,.F.,.F.,(3,3),(2,2),(0.,1.),(0.,0.03),
 .UNSPECIFIED.);
#864=B_SPLINE_SURFACE_WITH_KNOTS('',2,1,((#83287,#83288),(#83289,#83290),
(#83291,#83292)),.UNSPECIFIED.,.F.,.F.,.F.,(3,3),(2,2),(0.,1.),(0.,0.03),
 .UNSPECIFIED.);
#865=B_SPLINE_SURFACE_WITH_KNOTS('',2,1,((#83410,#83411),(#83412,#83413),
(#83414,#83415)),.UNSPECIFIED.,.F.,.F.,.F.,(3,3),(2,2),(0.,1.),(0.,0.03),
 .UNSPECIFIED.);
#866=B_SPLINE_SURFACE_WITH_KNOTS('',2,1,((#83428,#83429),(#83430,#83431),
(#83432,#83433)),.UNSPECIFIED.,.F.,.F.,.F.,(3,3),(2,2),(0.,1.),(0.,0.03),
 .UNSPECIFIED.);
#867=B_SPLINE_SURFACE_WITH_KNOTS('',2,1,((#83443,#83444),(#83445,#83446),
(#83447,#83448)),.UNSPECIFIED.,.F.,.F.,.F.,(3,3),(2,2),(0.,1.),(0.,0.03),
 .UNSPECIFIED.);
#868=B_SPLINE_SURFACE_WITH_KNOTS('',2,1,((#83458,#83459),(#83460,#83461),
(#83462,#83463)),.UNSPECIFIED.,.F.,.F.,.F.,(3,3),(2,2),(0.,1.),(0.,0.03),
 .UNSPECIFIED.);
#869=B_SPLINE_SURFACE_WITH_KNOTS('',2,1,((#83473,#83474),(#83475,#83476),
(#83477,#83478)),.UNSPECIFIED.,.F.,.F.,.F.,(3,3),(2,2),(0.,1.),(0.,0.03),
 .UNSPECIFIED.);
#870=B_SPLINE_SURFACE_WITH_KNOTS('',2,1,((#83488,#83489),(#83490,#83491),
(#83492,#83493)),.UNSPECIFIED.,.F.,.F.,.F.,(3,3),(2,2),(0.,1.),(0.,0.03),
 .UNSPECIFIED.);
#871=B_SPLINE_SURFACE_WITH_KNOTS('',2,1,((#83503,#83504),(#83505,#83506),
(#83507,#83508)),.UNSPECIFIED.,.F.,.F.,.F.,(3,3),(2,2),(0.,1.),(0.,0.03),
 .UNSPECIFIED.);
#872=B_SPLINE_SURFACE_WITH_KNOTS('',2,1,((#83518,#83519),(#83520,#83521),
(#83522,#83523)),.UNSPECIFIED.,.F.,.F.,.F.,(3,3),(2,2),(0.,1.),(0.,0.03),
 .UNSPECIFIED.);
#873=B_SPLINE_SURFACE_WITH_KNOTS('',2,1,((#83551,#83552),(#83553,#83554),
(#83555,#83556)),.UNSPECIFIED.,.F.,.F.,.F.,(3,3),(2,2),(0.,1.),(0.,0.03),
 .UNSPECIFIED.);
#874=B_SPLINE_SURFACE_WITH_KNOTS('',2,1,((#83573,#83574),(#83575,#83576),
(#83577,#83578)),.UNSPECIFIED.,.F.,.F.,.F.,(3,3),(2,2),(0.,1.),(0.,0.03),
 .UNSPECIFIED.);
#875=B_SPLINE_SURFACE_WITH_KNOTS('',2,1,((#83588,#83589),(#83590,#83591),
(#83592,#83593)),.UNSPECIFIED.,.F.,.F.,.F.,(3,3),(2,2),(0.,1.),(0.,0.03),
 .UNSPECIFIED.);
#876=B_SPLINE_SURFACE_WITH_KNOTS('',2,1,((#83603,#83604),(#83605,#83606),
(#83607,#83608)),.UNSPECIFIED.,.F.,.F.,.F.,(3,3),(2,2),(0.,1.),(0.,0.03),
 .UNSPECIFIED.);
#877=B_SPLINE_SURFACE_WITH_KNOTS('',2,1,((#83618,#83619),(#83620,#83621),
(#83622,#83623)),.UNSPECIFIED.,.F.,.F.,.F.,(3,3),(2,2),(0.,1.),(0.,0.03),
 .UNSPECIFIED.);
#878=B_SPLINE_SURFACE_WITH_KNOTS('',2,1,((#83651,#83652),(#83653,#83654),
(#83655,#83656)),.UNSPECIFIED.,.F.,.F.,.F.,(3,3),(2,2),(0.,1.),(0.,0.03),
 .UNSPECIFIED.);
#879=B_SPLINE_SURFACE_WITH_KNOTS('',2,1,((#83666,#83667),(#83668,#83669),
(#83670,#83671)),.UNSPECIFIED.,.F.,.F.,.F.,(3,3),(2,2),(0.,1.),(0.,0.03),
 .UNSPECIFIED.);
#880=B_SPLINE_SURFACE_WITH_KNOTS('',2,1,((#83681,#83682),(#83683,#83684),
(#83685,#83686)),.UNSPECIFIED.,.F.,.F.,.F.,(3,3),(2,2),(0.,1.),(0.,0.03),
 .UNSPECIFIED.);
#881=B_SPLINE_SURFACE_WITH_KNOTS('',2,1,((#83696,#83697),(#83698,#83699),
(#83700,#83701)),.UNSPECIFIED.,.F.,.F.,.F.,(3,3),(2,2),(0.,1.),(0.,0.03),
 .UNSPECIFIED.);
#882=B_SPLINE_SURFACE_WITH_KNOTS('',2,1,((#83711,#83712),(#83713,#83714),
(#83715,#83716)),.UNSPECIFIED.,.F.,.F.,.F.,(3,3),(2,2),(0.,1.),(0.,0.03),
 .UNSPECIFIED.);
#883=B_SPLINE_SURFACE_WITH_KNOTS('',2,1,((#83726,#83727),(#83728,#83729),
(#83730,#83731)),.UNSPECIFIED.,.F.,.F.,.F.,(3,3),(2,2),(0.,1.),(0.,0.03),
 .UNSPECIFIED.);
#884=B_SPLINE_SURFACE_WITH_KNOTS('',2,1,((#83741,#83742),(#83743,#83744),
(#83745,#83746)),.UNSPECIFIED.,.F.,.F.,.F.,(3,3),(2,2),(0.,1.),(0.,0.03),
 .UNSPECIFIED.);
#885=B_SPLINE_SURFACE_WITH_KNOTS('',3,3,((#85459,#85460,#85461,#85462,#85463,
#85464,#85465,#85466,#85467,#85468,#85469,#85470,#85471,#85472,#85473,#85474,
#85475,#85476,#85477,#85478,#85479,#85480,#85481,#85482,#85483,#85484,#85485,
#85486,#85487,#85488,#85489,#85490,#85491,#85492,#85493,#85494,#85495,#85496,
#85497,#85498,#85499,#85500,#85501,#85502,#85503,#85504,#85505,#85506,#85507,
#85508,#85509,#85510,#85511,#85512,#85513,#85514,#85515,#85516,#85517,#85518,
#85519,#85520,#85521,#85522,#85523,#85524,#85525,#85526,#85527,#85528,#85529,
#85530,#85531,#85532,#85533,#85534,#85535,#85536,#85537,#85538,#85539,#85540,
#85541,#85542,#85543,#85544,#85545,#85546,#85547,#85548,#85549,#85550,#85551,
#85552,#85553,#85554,#85555,#85556,#85557,#85558,#85559,#85560,#85561,#85562,
#85563,#85564,#85565),(#85566,#85567,#85568,#85569,#85570,#85571,#85572,
#85573,#85574,#85575,#85576,#85577,#85578,#85579,#85580,#85581,#85582,#85583,
#85584,#85585,#85586,#85587,#85588,#85589,#85590,#85591,#85592,#85593,#85594,
#85595,#85596,#85597,#85598,#85599,#85600,#85601,#85602,#85603,#85604,#85605,
#85606,#85607,#85608,#85609,#85610,#85611,#85612,#85613,#85614,#85615,#85616,
#85617,#85618,#85619,#85620,#85621,#85622,#85623,#85624,#85625,#85626,#85627,
#85628,#85629,#85630,#85631,#85632,#85633,#85634,#85635,#85636,#85637,#85638,
#85639,#85640,#85641,#85642,#85643,#85644,#85645,#85646,#85647,#85648,#85649,
#85650,#85651,#85652,#85653,#85654,#85655,#85656,#85657,#85658,#85659,#85660,
#85661,#85662,#85663,#85664,#85665,#85666,#85667,#85668,#85669,#85670,#85671,
#85672),(#85673,#85674,#85675,#85676,#85677,#85678,#85679,#85680,#85681,
#85682,#85683,#85684,#85685,#85686,#85687,#85688,#85689,#85690,#85691,#85692,
#85693,#85694,#85695,#85696,#85697,#85698,#85699,#85700,#85701,#85702,#85703,
#85704,#85705,#85706,#85707,#85708,#85709,#85710,#85711,#85712,#85713,#85714,
#85715,#85716,#85717,#85718,#85719,#85720,#85721,#85722,#85723,#85724,#85725,
#85726,#85727,#85728,#85729,#85730,#85731,#85732,#85733,#85734,#85735,#85736,
#85737,#85738,#85739,#85740,#85741,#85742,#85743,#85744,#85745,#85746,#85747,
#85748,#85749,#85750,#85751,#85752,#85753,#85754,#85755,#85756,#85757,#85758,
#85759,#85760,#85761,#85762,#85763,#85764,#85765,#85766,#85767,#85768,#85769,
#85770,#85771,#85772,#85773,#85774,#85775,#85776,#85777,#85778,#85779),
(#85780,#85781,#85782,#85783,#85784,#85785,#85786,#85787,#85788,#85789,
#85790,#85791,#85792,#85793,#85794,#85795,#85796,#85797,#85798,#85799,#85800,
#85801,#85802,#85803,#85804,#85805,#85806,#85807,#85808,#85809,#85810,#85811,
#85812,#85813,#85814,#85815,#85816,#85817,#85818,#85819,#85820,#85821,#85822,
#85823,#85824,#85825,#85826,#85827,#85828,#85829,#85830,#85831,#85832,#85833,
#85834,#85835,#85836,#85837,#85838,#85839,#85840,#85841,#85842,#85843,#85844,
#85845,#85846,#85847,#85848,#85849,#85850,#85851,#85852,#85853,#85854,#85855,
#85856,#85857,#85858,#85859,#85860,#85861,#85862,#85863,#85864,#85865,#85866,
#85867,#85868,#85869,#85870,#85871,#85872,#85873,#85874,#85875,#85876,#85877,
#85878,#85879,#85880,#85881,#85882,#85883,#85884,#85885,#85886)),
 .UNSPECIFIED.,.F.,.F.,.F.,(4,4),(4,1,1,1,1,1,1,1,1,1,1,1,1,1,1,1,1,1,1,
1,1,1,1,1,1,1,1,1,1,1,1,1,1,1,1,1,1,1,1,1,1,1,1,1,1,1,1,1,1,1,1,1,1,1,1,
1,1,1,1,1,1,1,1,1,1,1,1,1,1,1,1,1,1,1,1,1,1,1,1,1,1,1,1,1,1,1,1,1,1,1,1,
1,1,1,1,1,1,1,1,1,1,1,1,1,4),(0.,0.0986691610045069),(8.30989595155332,
8.8061514916218,9.30240703169027,10.2949181118272,11.2874291919642,12.2799402721011,
13.2724513522381,14.264962432375,15.257473512512,16.2499845926489,17.2424956727859,
18.2350067529228,19.2275178330597,20.2200289131967,21.2125399933336,22.2050510734706,
23.1975621536075,24.1900732337445,25.1825843138814,26.1750953940184,27.1676064741553,
28.1601175542923,29.1526286344292,30.1451397145662,31.1376507947031,32.1301618748401,
33.122672954977,34.115184035114,35.1076951152509,36.1002061953878,37.0927172755248,
38.0852283556617,39.0777394357987,40.0702505159356,41.0627615960726,42.0552726762095,
43.0477837563465,44.0402948364834,45.0328059166204,46.0253169967573,47.0178280768943,
48.0103391570312,49.0028502371682,49.9953613173051,50.9878723974421,51.980383477579,
52.972894557716,53.9654056378529,54.9579167179898,55.9504277981268,56.9429388782637,
57.9354499584007,58.9279610385376,59.9204721186746,60.9129831988115,61.9054942789485,
62.8980053590854,63.8905164392224,64.8830275193593,65.8755385994963,66.8680496796332,
67.8605607597702,68.8530718399071,69.8455829200441,70.838094000181,71.830605080318,
72.8231161604549,73.8156272405919,74.8081383207288,75.8006494008658,76.7931604810027,
77.7856715611396,78.7781826412766,79.7706937214135,80.7632048015505,81.7557158816874,
82.7482269618244,83.7407380419613,84.7332491220983,85.7257602022352,86.7182712823722,
87.7107823625091,88.7032934426461,89.695804522783,90.68831560292,91.6808266830569,
92.6733377631939,93.6658488433308,94.6583599234677,95.6508710036047,96.6433820837416,
97.6358931638786,98.6284042440155,99.6209153241525,100.613426404289,101.605937484426,
102.598448564563,103.5909596447,104.583470724837,105.575981804974,106.568492885111,
107.561003965248,108.553515045385,109.049770585453,109.546026125522),
 .UNSPECIFIED.);
#886=B_SPLINE_SURFACE_WITH_KNOTS('',3,3,((#86138,#86139,#86140,#86141,#86142,
#86143,#86144,#86145,#86146,#86147,#86148,#86149,#86150,#86151,#86152,#86153,
#86154,#86155,#86156,#86157,#86158,#86159,#86160,#86161,#86162,#86163,#86164,
#86165,#86166,#86167,#86168,#86169,#86170,#86171,#86172,#86173,#86174,#86175,
#86176,#86177,#86178,#86179,#86180,#86181,#86182,#86183,#86184,#86185,#86186,
#86187,#86188,#86189,#86190,#86191,#86192,#86193,#86194,#86195,#86196,#86197,
#86198,#86199,#86200,#86201,#86202,#86203,#86204,#86205,#86206,#86207,#86208,
#86209,#86210,#86211,#86212,#86213,#86214,#86215,#86216,#86217,#86218,#86219,
#86220,#86221,#86222,#86223,#86224,#86225,#86226,#86227,#86228,#86229,#86230,
#86231,#86232,#86233,#86234,#86235,#86236,#86237,#86238,#86239,#86240,#86241,
#86242,#86243,#86244),(#86245,#86246,#86247,#86248,#86249,#86250,#86251,
#86252,#86253,#86254,#86255,#86256,#86257,#86258,#86259,#86260,#86261,#86262,
#86263,#86264,#86265,#86266,#86267,#86268,#86269,#86270,#86271,#86272,#86273,
#86274,#86275,#86276,#86277,#86278,#86279,#86280,#86281,#86282,#86283,#86284,
#86285,#86286,#86287,#86288,#86289,#86290,#86291,#86292,#86293,#86294,#86295,
#86296,#86297,#86298,#86299,#86300,#86301,#86302,#86303,#86304,#86305,#86306,
#86307,#86308,#86309,#86310,#86311,#86312,#86313,#86314,#86315,#86316,#86317,
#86318,#86319,#86320,#86321,#86322,#86323,#86324,#86325,#86326,#86327,#86328,
#86329,#86330,#86331,#86332,#86333,#86334,#86335,#86336,#86337,#86338,#86339,
#86340,#86341,#86342,#86343,#86344,#86345,#86346,#86347,#86348,#86349,#86350,
#86351),(#86352,#86353,#86354,#86355,#86356,#86357,#86358,#86359,#86360,
#86361,#86362,#86363,#86364,#86365,#86366,#86367,#86368,#86369,#86370,#86371,
#86372,#86373,#86374,#86375,#86376,#86377,#86378,#86379,#86380,#86381,#86382,
#86383,#86384,#86385,#86386,#86387,#86388,#86389,#86390,#86391,#86392,#86393,
#86394,#86395,#86396,#86397,#86398,#86399,#86400,#86401,#86402,#86403,#86404,
#86405,#86406,#86407,#86408,#86409,#86410,#86411,#86412,#86413,#86414,#86415,
#86416,#86417,#86418,#86419,#86420,#86421,#86422,#86423,#86424,#86425,#86426,
#86427,#86428,#86429,#86430,#86431,#86432,#86433,#86434,#86435,#86436,#86437,
#86438,#86439,#86440,#86441,#86442,#86443,#86444,#86445,#86446,#86447,#86448,
#86449,#86450,#86451,#86452,#86453,#86454,#86455,#86456,#86457,#86458),
(#86459,#86460,#86461,#86462,#86463,#86464,#86465,#86466,#86467,#86468,
#86469,#86470,#86471,#86472,#86473,#86474,#86475,#86476,#86477,#86478,#86479,
#86480,#86481,#86482,#86483,#86484,#86485,#86486,#86487,#86488,#86489,#86490,
#86491,#86492,#86493,#86494,#86495,#86496,#86497,#86498,#86499,#86500,#86501,
#86502,#86503,#86504,#86505,#86506,#86507,#86508,#86509,#86510,#86511,#86512,
#86513,#86514,#86515,#86516,#86517,#86518,#86519,#86520,#86521,#86522,#86523,
#86524,#86525,#86526,#86527,#86528,#86529,#86530,#86531,#86532,#86533,#86534,
#86535,#86536,#86537,#86538,#86539,#86540,#86541,#86542,#86543,#86544,#86545,
#86546,#86547,#86548,#86549,#86550,#86551,#86552,#86553,#86554,#86555,#86556,
#86557,#86558,#86559,#86560,#86561,#86562,#86563,#86564,#86565)),
 .UNSPECIFIED.,.F.,.F.,.F.,(4,4),(4,1,1,1,1,1,1,1,1,1,1,1,1,1,1,1,1,1,1,
1,1,1,1,1,1,1,1,1,1,1,1,1,1,1,1,1,1,1,1,1,1,1,1,1,1,1,1,1,1,1,1,1,1,1,1,
1,1,1,1,1,1,1,1,1,1,1,1,1,1,1,1,1,1,1,1,1,1,1,1,1,1,1,1,1,1,1,1,1,1,1,1,
1,1,1,1,1,1,1,1,1,1,1,1,1,4),(0.,0.0986691610045069),(11.6147305479242,
12.1109860879927,12.6072416280611,13.5997527081981,14.592263788335,15.584774868472,
16.5772859486089,17.5697970287459,18.5623081088828,19.5548191890198,20.5473302691567,
21.5398413492937,22.5323524294306,23.5248635095676,24.5173745897045,25.5098856698415,
26.5023967499784,27.4949078301153,28.4874189102523,29.4799299903892,30.4724410705262,
31.4649521506631,32.4574632308001,33.449974310937,34.442485391074,35.4349964712109,
36.4275075513479,37.4200186314848,38.4125297116218,39.4050407917587,40.3975518718957,
41.3900629520326,42.3825740321696,43.3750851123065,44.3675961924435,45.3601072725804,
46.3526183527174,47.3451294328543,48.3376405129912,49.3301515931282,50.3226626732651,
51.3151737534021,52.307684833539,53.300195913676,54.2927069938129,55.2852180739499,
56.2777291540868,57.2702402342238,58.2627513143607,59.2552623944977,60.2477734746346,
61.2402845547716,62.2327956349085,63.2253067150455,64.2178177951824,65.2103288753194,
66.2028399554563,67.1953510355932,68.1878621157302,69.1803731958671,70.1728842760041,
71.165395356141,72.157906436278,73.1504175164149,74.1429285965519,75.1354396766888,
76.1279507568258,77.1204618369627,78.1129729170997,79.1054839972366,80.0979950773736,
81.0905061575105,82.0830172376475,83.0755283177844,84.0680393979214,85.0605504780583,
86.0530615581953,87.0455726383322,88.0380837184692,89.0305947986061,90.0231058787431,
91.01561695888,92.0081280390169,93.0006391191539,93.9931501992908,94.9856612794278,
95.9781723595647,96.9706834397017,97.9631945198386,98.9557055999756,99.9482166801125,
100.940727760249,101.933238840386,102.925749920523,103.91826100066,104.910772080797,
105.903283160934,106.895794241071,107.888305321208,108.880816401345,109.873327481482,
110.865838561619,111.858349641756,112.354605181824,112.850860721893),
 .UNSPECIFIED.);
#887=B_SPLINE_SURFACE_WITH_KNOTS('',3,3,((#88798,#88799,#88800,#88801,#88802,
#88803,#88804,#88805,#88806,#88807,#88808,#88809,#88810,#88811,#88812,#88813,
#88814,#88815,#88816,#88817,#88818,#88819,#88820,#88821,#88822,#88823,#88824,
#88825,#88826,#88827,#88828,#88829,#88830,#88831,#88832,#88833,#88834,#88835,
#88836,#88837,#88838,#88839,#88840,#88841,#88842,#88843,#88844,#88845,#88846,
#88847,#88848,#88849,#88850,#88851,#88852,#88853,#88854,#88855,#88856,#88857,
#88858,#88859,#88860,#88861,#88862,#88863,#88864,#88865,#88866,#88867,#88868,
#88869,#88870,#88871,#88872,#88873,#88874,#88875,#88876,#88877,#88878,#88879,
#88880,#88881,#88882,#88883,#88884,#88885,#88886,#88887,#88888,#88889,#88890,
#88891,#88892,#88893,#88894,#88895,#88896,#88897,#88898),(#88899,#88900,
#88901,#88902,#88903,#88904,#88905,#88906,#88907,#88908,#88909,#88910,#88911,
#88912,#88913,#88914,#88915,#88916,#88917,#88918,#88919,#88920,#88921,#88922,
#88923,#88924,#88925,#88926,#88927,#88928,#88929,#88930,#88931,#88932,#88933,
#88934,#88935,#88936,#88937,#88938,#88939,#88940,#88941,#88942,#88943,#88944,
#88945,#88946,#88947,#88948,#88949,#88950,#88951,#88952,#88953,#88954,#88955,
#88956,#88957,#88958,#88959,#88960,#88961,#88962,#88963,#88964,#88965,#88966,
#88967,#88968,#88969,#88970,#88971,#88972,#88973,#88974,#88975,#88976,#88977,
#88978,#88979,#88980,#88981,#88982,#88983,#88984,#88985,#88986,#88987,#88988,
#88989,#88990,#88991,#88992,#88993,#88994,#88995,#88996,#88997,#88998,#88999),
(#89000,#89001,#89002,#89003,#89004,#89005,#89006,#89007,#89008,#89009,
#89010,#89011,#89012,#89013,#89014,#89015,#89016,#89017,#89018,#89019,#89020,
#89021,#89022,#89023,#89024,#89025,#89026,#89027,#89028,#89029,#89030,#89031,
#89032,#89033,#89034,#89035,#89036,#89037,#89038,#89039,#89040,#89041,#89042,
#89043,#89044,#89045,#89046,#89047,#89048,#89049,#89050,#89051,#89052,#89053,
#89054,#89055,#89056,#89057,#89058,#89059,#89060,#89061,#89062,#89063,#89064,
#89065,#89066,#89067,#89068,#89069,#89070,#89071,#89072,#89073,#89074,#89075,
#89076,#89077,#89078,#89079,#89080,#89081,#89082,#89083,#89084,#89085,#89086,
#89087,#89088,#89089,#89090,#89091,#89092,#89093,#89094,#89095,#89096,#89097,
#89098,#89099,#89100),(#89101,#89102,#89103,#89104,#89105,#89106,#89107,
#89108,#89109,#89110,#89111,#89112,#89113,#89114,#89115,#89116,#89117,#89118,
#89119,#89120,#89121,#89122,#89123,#89124,#89125,#89126,#89127,#89128,#89129,
#89130,#89131,#89132,#89133,#89134,#89135,#89136,#89137,#89138,#89139,#89140,
#89141,#89142,#89143,#89144,#89145,#89146,#89147,#89148,#89149,#89150,#89151,
#89152,#89153,#89154,#89155,#89156,#89157,#89158,#89159,#89160,#89161,#89162,
#89163,#89164,#89165,#89166,#89167,#89168,#89169,#89170,#89171,#89172,#89173,
#89174,#89175,#89176,#89177,#89178,#89179,#89180,#89181,#89182,#89183,#89184,
#89185,#89186,#89187,#89188,#89189,#89190,#89191,#89192,#89193,#89194,#89195,
#89196,#89197,#89198,#89199,#89200,#89201)),.UNSPECIFIED.,.F.,.F.,.F.,(4,
4),(4,1,1,1,1,1,1,1,1,1,1,1,1,1,1,1,1,1,1,1,1,1,1,1,1,1,1,1,1,1,1,1,1,1,
1,1,1,1,1,1,1,1,1,1,1,1,1,1,1,1,1,1,1,1,1,1,1,1,1,1,1,1,1,1,1,1,1,1,1,1,
1,1,1,1,1,1,1,1,1,1,1,1,1,1,1,1,1,1,1,1,1,1,1,1,1,1,1,1,4),(0.,0.0658467982010768),
(8.30747755240103,9.30363388226323,10.2997902121254,11.2959465419876,12.2921028718499,
13.2882592017121,14.2844155315743,15.2805718614365,16.2767281912987,17.2728845211609,
18.2690408510231,19.2651971808853,20.2613535107475,21.2575098406097,22.2536661704719,
23.2498225003341,24.2459788301963,25.2421351600585,26.2382914899207,27.234447819783,
28.2306041496452,29.2267604795074,30.2229168093696,31.2190731392318,32.215229469094,
33.2113857989562,34.2075421288184,35.2036984586806,36.1998547885428,37.196011118405,
38.1921674482672,39.1883237781294,40.1844801079916,41.1806364378538,42.1767927677161,
43.1729490975783,44.1691054274405,45.1652617573027,46.1614180871649,47.1575744170271,
48.1537307468893,49.1498870767515,50.1460434066137,51.1421997364759,52.1383560663381,
53.1345123962003,54.1306687260625,55.1268250559247,56.122981385787,57.1191377156492,
58.1152940455114,59.1114503753736,60.1076067052358,61.103763035098,62.0999193649602,
63.0960756948224,64.0922320246846,65.0883883545468,66.084544684409,67.0807010142712,
68.0768573441334,69.0730136739956,70.0691700038578,71.0653263337201,72.0614826635823,
73.0576389934445,74.0537953233067,75.0499516531689,76.0461079830311,77.0422643128933,
78.0384206427555,79.0345769726177,80.0307333024799,81.0268896323421,82.0230459622043,
83.0192022920665,84.0153586219287,85.0115149517909,86.0076712816532,87.0038276115154,
87.9999839413776,88.9961402712398,89.992296601102,90.9884529309642,91.9846092608264,
92.9807655906886,93.9769219205508,94.973078250413,95.9692345802752,96.9653909101374,
97.9615472399996,98.9577035698618,99.9538598997241,100.950016229586,101.946172559448,
102.942328889311,103.938485219173,104.934641549035,105.930797878897),
 .UNSPECIFIED.);
#888=B_SPLINE_SURFACE_WITH_KNOTS('',3,3,((#89416,#89417,#89418,#89419,#89420,
#89421,#89422,#89423,#89424,#89425,#89426,#89427,#89428,#89429,#89430,#89431,
#89432,#89433,#89434,#89435,#89436,#89437,#89438,#89439,#89440,#89441,#89442,
#89443,#89444,#89445,#89446,#89447,#89448,#89449,#89450,#89451,#89452,#89453,
#89454,#89455,#89456,#89457,#89458,#89459,#89460,#89461,#89462,#89463,#89464,
#89465,#89466,#89467,#89468,#89469,#89470,#89471,#89472,#89473,#89474,#89475,
#89476,#89477,#89478,#89479,#89480,#89481,#89482,#89483,#89484,#89485,#89486,
#89487,#89488,#89489,#89490,#89491,#89492,#89493,#89494,#89495,#89496,#89497,
#89498,#89499,#89500,#89501,#89502,#89503,#89504,#89505,#89506,#89507,#89508,
#89509,#89510,#89511,#89512,#89513,#89514,#89515,#89516),(#89517,#89518,
#89519,#89520,#89521,#89522,#89523,#89524,#89525,#89526,#89527,#89528,#89529,
#89530,#89531,#89532,#89533,#89534,#89535,#89536,#89537,#89538,#89539,#89540,
#89541,#89542,#89543,#89544,#89545,#89546,#89547,#89548,#89549,#89550,#89551,
#89552,#89553,#89554,#89555,#89556,#89557,#89558,#89559,#89560,#89561,#89562,
#89563,#89564,#89565,#89566,#89567,#89568,#89569,#89570,#89571,#89572,#89573,
#89574,#89575,#89576,#89577,#89578,#89579,#89580,#89581,#89582,#89583,#89584,
#89585,#89586,#89587,#89588,#89589,#89590,#89591,#89592,#89593,#89594,#89595,
#89596,#89597,#89598,#89599,#89600,#89601,#89602,#89603,#89604,#89605,#89606,
#89607,#89608,#89609,#89610,#89611,#89612,#89613,#89614,#89615,#89616,#89617),
(#89618,#89619,#89620,#89621,#89622,#89623,#89624,#89625,#89626,#89627,
#89628,#89629,#89630,#89631,#89632,#89633,#89634,#89635,#89636,#89637,#89638,
#89639,#89640,#89641,#89642,#89643,#89644,#89645,#89646,#89647,#89648,#89649,
#89650,#89651,#89652,#89653,#89654,#89655,#89656,#89657,#89658,#89659,#89660,
#89661,#89662,#89663,#89664,#89665,#89666,#89667,#89668,#89669,#89670,#89671,
#89672,#89673,#89674,#89675,#89676,#89677,#89678,#89679,#89680,#89681,#89682,
#89683,#89684,#89685,#89686,#89687,#89688,#89689,#89690,#89691,#89692,#89693,
#89694,#89695,#89696,#89697,#89698,#89699,#89700,#89701,#89702,#89703,#89704,
#89705,#89706,#89707,#89708,#89709,#89710,#89711,#89712,#89713,#89714,#89715,
#89716,#89717,#89718),(#89719,#89720,#89721,#89722,#89723,#89724,#89725,
#89726,#89727,#89728,#89729,#89730,#89731,#89732,#89733,#89734,#89735,#89736,
#89737,#89738,#89739,#89740,#89741,#89742,#89743,#89744,#89745,#89746,#89747,
#89748,#89749,#89750,#89751,#89752,#89753,#89754,#89755,#89756,#89757,#89758,
#89759,#89760,#89761,#89762,#89763,#89764,#89765,#89766,#89767,#89768,#89769,
#89770,#89771,#89772,#89773,#89774,#89775,#89776,#89777,#89778,#89779,#89780,
#89781,#89782,#89783,#89784,#89785,#89786,#89787,#89788,#89789,#89790,#89791,
#89792,#89793,#89794,#89795,#89796,#89797,#89798,#89799,#89800,#89801,#89802,
#89803,#89804,#89805,#89806,#89807,#89808,#89809,#89810,#89811,#89812,#89813,
#89814,#89815,#89816,#89817,#89818,#89819)),.UNSPECIFIED.,.F.,.F.,.F.,(4,
4),(4,1,1,1,1,1,1,1,1,1,1,1,1,1,1,1,1,1,1,1,1,1,1,1,1,1,1,1,1,1,1,1,1,1,
1,1,1,1,1,1,1,1,1,1,1,1,1,1,1,1,1,1,1,1,1,1,1,1,1,1,1,1,1,1,1,1,1,1,1,1,
1,1,1,1,1,1,1,1,1,1,1,1,1,1,1,1,1,1,1,1,1,1,1,1,1,1,1,1,4),(0.,0.0658467982010768),
(11.6150328478182,12.6111891776804,13.6073455075426,14.6035018374048,15.5996581672671,
16.5958144971293,17.5919708269915,18.5881271568537,19.5842834867159,20.5804398165781,
21.5765961464403,22.5727524763025,23.5689088061647,24.5650651360269,25.5612214658891,
26.5573777957513,27.5535341256135,28.5496904554757,29.545846785338,30.5420031152002,
31.5381594450624,32.5343157749246,33.5304721047868,34.526628434649,35.5227847645112,
36.5189410943734,37.5150974242356,38.5112537540978,39.50741008396,40.5035664138222,
41.4997227436844,42.4958790735466,43.4920354034088,44.4881917332711,45.4843480631333,
46.4805043929955,47.4766607228577,48.4728170527199,49.4689733825821,50.4651297124443,
51.4612860423065,52.4574423721687,53.4535987020309,54.4497550318931,55.4459113617553,
56.4420676916175,57.4382240214797,58.434380351342,59.4305366812042,60.4266930110664,
61.4228493409286,62.4190056707908,63.415162000653,64.4113183305152,65.4074746603774,
66.4036309902396,67.3997873201018,68.395943649964,69.3920999798262,70.3882563096884,
71.3844126395506,72.3805689694128,73.3767252992751,74.3728816291373,75.3690379589995,
76.3651942888617,77.3613506187239,78.3575069485861,79.3536632784483,80.3498196083105,
81.3459759381727,82.3421322680349,83.3382885978971,84.3344449277593,85.3306012576215,
86.3267575874837,87.322913917346,88.3190702472082,89.3152265770704,90.3113829069326,
91.3075392367948,92.303695566657,93.2998518965192,94.2960082263814,95.2921645562436,
96.2883208861058,97.284477215968,98.2806335458302,99.2767898756924,100.272946205555,
101.269102535417,102.265258865279,103.261415195141,104.257571525003,105.253727854866,
106.249884184728,107.24604051459,108.242196844452,109.238353174315),
 .UNSPECIFIED.);
#889=B_SPLINE_SURFACE_WITH_KNOTS('',3,3,((#92513,#92514,#92515,#92516,#92517,
#92518,#92519,#92520,#92521,#92522,#92523,#92524,#92525,#92526,#92527,#92528,
#92529,#92530,#92531,#92532,#92533,#92534,#92535,#92536,#92537,#92538,#92539,
#92540,#92541,#92542,#92543,#92544,#92545,#92546,#92547,#92548,#92549,#92550,
#92551,#92552,#92553,#92554,#92555,#92556,#92557,#92558,#92559,#92560,#92561,
#92562,#92563,#92564,#92565,#92566,#92567,#92568,#92569,#92570,#92571,#92572,
#92573,#92574,#92575,#92576,#92577,#92578,#92579,#92580,#92581,#92582,#92583,
#92584,#92585,#92586,#92587,#92588,#92589,#92590,#92591,#92592,#92593,#92594,
#92595,#92596,#92597,#92598,#92599,#92600,#92601,#92602,#92603,#92604,#92605,
#92606,#92607,#92608,#92609,#92610,#92611,#92612,#92613,#92614,#92615,#92616,
#92617,#92618,#92619,#92620,#92621,#92622,#92623,#92624,#92625,#92626,#92627,
#92628,#92629,#92630,#92631,#92632,#92633,#92634,#92635,#92636,#92637,#92638,
#92639,#92640,#92641,#92642,#92643,#92644,#92645,#92646,#92647,#92648,#92649,
#92650,#92651,#92652,#92653,#92654,#92655,#92656,#92657,#92658,#92659,#92660,
#92661,#92662,#92663),(#92664,#92665,#92666,#92667,#92668,#92669,#92670,
#92671,#92672,#92673,#92674,#92675,#92676,#92677,#92678,#92679,#92680,#92681,
#92682,#92683,#92684,#92685,#92686,#92687,#92688,#92689,#92690,#92691,#92692,
#92693,#92694,#92695,#92696,#92697,#92698,#92699,#92700,#92701,#92702,#92703,
#92704,#92705,#92706,#92707,#92708,#92709,#92710,#92711,#92712,#92713,#92714,
#92715,#92716,#92717,#92718,#92719,#92720,#92721,#92722,#92723,#92724,#92725,
#92726,#92727,#92728,#92729,#92730,#92731,#92732,#92733,#92734,#92735,#92736,
#92737,#92738,#92739,#92740,#92741,#92742,#92743,#92744,#92745,#92746,#92747,
#92748,#92749,#92750,#92751,#92752,#92753,#92754,#92755,#92756,#92757,#92758,
#92759,#92760,#92761,#92762,#92763,#92764,#92765,#92766,#92767,#92768,#92769,
#92770,#92771,#92772,#92773,#92774,#92775,#92776,#92777,#92778,#92779,#92780,
#92781,#92782,#92783,#92784,#92785,#92786,#92787,#92788,#92789,#92790,#92791,
#92792,#92793,#92794,#92795,#92796,#92797,#92798,#92799,#92800,#92801,#92802,
#92803,#92804,#92805,#92806,#92807,#92808,#92809,#92810,#92811,#92812,#92813,
#92814),(#92815,#92816,#92817,#92818,#92819,#92820,#92821,#92822,#92823,
#92824,#92825,#92826,#92827,#92828,#92829,#92830,#92831,#92832,#92833,#92834,
#92835,#92836,#92837,#92838,#92839,#92840,#92841,#92842,#92843,#92844,#92845,
#92846,#92847,#92848,#92849,#92850,#92851,#92852,#92853,#92854,#92855,#92856,
#92857,#92858,#92859,#92860,#92861,#92862,#92863,#92864,#92865,#92866,#92867,
#92868,#92869,#92870,#92871,#92872,#92873,#92874,#92875,#92876,#92877,#92878,
#92879,#92880,#92881,#92882,#92883,#92884,#92885,#92886,#92887,#92888,#92889,
#92890,#92891,#92892,#92893,#92894,#92895,#92896,#92897,#92898,#92899,#92900,
#92901,#92902,#92903,#92904,#92905,#92906,#92907,#92908,#92909,#92910,#92911,
#92912,#92913,#92914,#92915,#92916,#92917,#92918,#92919,#92920,#92921,#92922,
#92923,#92924,#92925,#92926,#92927,#92928,#92929,#92930,#92931,#92932,#92933,
#92934,#92935,#92936,#92937,#92938,#92939,#92940,#92941,#92942,#92943,#92944,
#92945,#92946,#92947,#92948,#92949,#92950,#92951,#92952,#92953,#92954,#92955,
#92956,#92957,#92958,#92959,#92960,#92961,#92962,#92963,#92964,#92965),
(#92966,#92967,#92968,#92969,#92970,#92971,#92972,#92973,#92974,#92975,
#92976,#92977,#92978,#92979,#92980,#92981,#92982,#92983,#92984,#92985,#92986,
#92987,#92988,#92989,#92990,#92991,#92992,#92993,#92994,#92995,#92996,#92997,
#92998,#92999,#93000,#93001,#93002,#93003,#93004,#93005,#93006,#93007,#93008,
#93009,#93010,#93011,#93012,#93013,#93014,#93015,#93016,#93017,#93018,#93019,
#93020,#93021,#93022,#93023,#93024,#93025,#93026,#93027,#93028,#93029,#93030,
#93031,#93032,#93033,#93034,#93035,#93036,#93037,#93038,#93039,#93040,#93041,
#93042,#93043,#93044,#93045,#93046,#93047,#93048,#93049,#93050,#93051,#93052,
#93053,#93054,#93055,#93056,#93057,#93058,#93059,#93060,#93061,#93062,#93063,
#93064,#93065,#93066,#93067,#93068,#93069,#93070,#93071,#93072,#93073,#93074,
#93075,#93076,#93077,#93078,#93079,#93080,#93081,#93082,#93083,#93084,#93085,
#93086,#93087,#93088,#93089,#93090,#93091,#93092,#93093,#93094,#93095,#93096,
#93097,#93098,#93099,#93100,#93101,#93102,#93103,#93104,#93105,#93106,#93107,
#93108,#93109,#93110,#93111,#93112,#93113,#93114,#93115,#93116)),
 .UNSPECIFIED.,.F.,.F.,.F.,(4,4),(4,1,1,1,1,1,1,1,1,1,1,1,1,1,1,1,1,1,1,
1,1,1,1,1,1,1,1,1,1,1,1,1,1,1,1,1,1,1,1,1,1,1,1,1,1,1,1,1,1,1,1,1,1,1,1,
1,1,1,1,1,1,1,1,1,1,1,1,1,1,1,1,1,1,1,1,1,1,1,1,1,1,1,1,1,1,1,1,1,1,1,1,
1,1,1,1,1,1,1,1,1,1,1,1,1,1,1,1,1,1,1,1,1,1,1,1,1,1,1,1,1,1,1,1,1,1,1,1,
1,1,1,1,1,1,1,1,1,1,1,1,1,1,1,1,1,1,1,1,1,4),(0.,0.0820126057383863),(8.31473274985805,
9.30907443774587,10.3034161256337,11.2977578135215,12.2920995014094,13.2864411892972,
14.280782877185,15.2751245650728,16.2694662529607,17.2638079408485,18.2581496287363,
19.2524913166241,20.246833004512,21.2411746923998,22.2355163802876,23.2298580681754,
24.2241997560633,25.2185414439511,26.2128831318389,27.2072248197267,28.2015665076146,
29.1959081955024,30.1902498833902,31.184591571278,32.1789332591659,33.1732749470537,
34.1676166349415,35.1619583228293,36.1563000107172,37.150641698605,38.1449833864928,
39.1393250743807,40.1336667622685,41.1280084501563,42.1223501380441,43.116691825932,
44.1110335138198,45.1053752017076,46.0997168895954,47.0940585774833,48.0884002653711,
49.0827419532589,50.0770836411467,51.0714253290346,52.0657670169224,53.0601087048102,
54.054450392698,55.0487920805859,56.0431337684737,57.0374754563615,58.0318171442493,
59.0261588321372,60.020500520025,61.0148422079128,62.0091838958006,63.0035255836885,
63.9978672715763,64.9922089594641,65.9865506473519,66.9808923352398,67.9752340231276,
68.9695757110154,69.9639173989032,70.9582590867911,71.9526007746789,72.9469424625667,
73.9412841504546,74.9356258383424,75.9299675262302,76.924309214118,77.9186509020059,
78.9129925898937,79.9073342777815,80.9016759656693,81.8960176535572,82.890359341445,
83.8847010293328,84.8790427172206,85.8733844051085,86.8677260929963,87.8620677808841,
88.8564094687719,89.8507511566598,90.8450928445476,91.8394345324354,92.8337762203232,
93.8281179082111,94.8224595960989,95.8168012839867,96.8111429718745,97.8054846597624,
98.7998263476502,99.794168035538,100.788509723426,101.782851411314,102.777193099202,
103.771534787089,104.765876474977,105.760218162865,106.754559850753,107.748901538641,
108.743243226528,109.737584914416,110.731926602304,111.726268290192,112.72060997808,
113.714951665968,114.709293353855,115.703635041743,116.697976729631,117.692318417519,
118.686660105407,119.681001793295,120.675343481182,121.66968516907,122.664026856958,
123.658368544846,124.652710232734,125.647051920622,126.641393608509,127.635735296397,
128.630076984285,129.624418672173,130.618760360061,131.613102047948,132.607443735836,
133.601785423724,134.596127111612,135.5904687995,136.584810487388,137.579152175275,
138.573493863163,139.567835551051,140.562177238939,141.556518926827,142.550860614715,
143.545202302602,144.53954399049,145.533885678378,146.528227366266,147.522569054154,
148.516910742041,149.511252429929,150.505594117817,151.499935805705,152.494277493593,
153.488619181481,154.482960869368,155.477302557256),.UNSPECIFIED.);
#890=B_SPLINE_SURFACE_WITH_KNOTS('',3,3,((#93355,#93356,#93357,#93358,#93359,
#93360,#93361,#93362,#93363,#93364,#93365,#93366,#93367,#93368,#93369,#93370,
#93371,#93372,#93373,#93374,#93375,#93376,#93377,#93378,#93379,#93380,#93381,
#93382,#93383,#93384,#93385,#93386,#93387,#93388,#93389,#93390,#93391,#93392,
#93393,#93394,#93395,#93396,#93397,#93398,#93399,#93400,#93401,#93402,#93403,
#93404,#93405,#93406,#93407,#93408,#93409,#93410,#93411,#93412,#93413,#93414,
#93415,#93416,#93417,#93418,#93419,#93420,#93421,#93422,#93423,#93424,#93425,
#93426,#93427,#93428,#93429,#93430,#93431,#93432,#93433,#93434,#93435,#93436,
#93437,#93438,#93439,#93440,#93441,#93442,#93443,#93444,#93445,#93446,#93447,
#93448,#93449,#93450,#93451,#93452,#93453,#93454,#93455,#93456,#93457,#93458,
#93459,#93460,#93461,#93462,#93463,#93464,#93465,#93466,#93467,#93468,#93469,
#93470,#93471,#93472,#93473,#93474,#93475,#93476,#93477,#93478,#93479,#93480,
#93481,#93482,#93483,#93484,#93485,#93486,#93487,#93488,#93489,#93490,#93491,
#93492,#93493,#93494,#93495,#93496,#93497,#93498,#93499,#93500,#93501,#93502,
#93503,#93504,#93505),(#93506,#93507,#93508,#93509,#93510,#93511,#93512,
#93513,#93514,#93515,#93516,#93517,#93518,#93519,#93520,#93521,#93522,#93523,
#93524,#93525,#93526,#93527,#93528,#93529,#93530,#93531,#93532,#93533,#93534,
#93535,#93536,#93537,#93538,#93539,#93540,#93541,#93542,#93543,#93544,#93545,
#93546,#93547,#93548,#93549,#93550,#93551,#93552,#93553,#93554,#93555,#93556,
#93557,#93558,#93559,#93560,#93561,#93562,#93563,#93564,#93565,#93566,#93567,
#93568,#93569,#93570,#93571,#93572,#93573,#93574,#93575,#93576,#93577,#93578,
#93579,#93580,#93581,#93582,#93583,#93584,#93585,#93586,#93587,#93588,#93589,
#93590,#93591,#93592,#93593,#93594,#93595,#93596,#93597,#93598,#93599,#93600,
#93601,#93602,#93603,#93604,#93605,#93606,#93607,#93608,#93609,#93610,#93611,
#93612,#93613,#93614,#93615,#93616,#93617,#93618,#93619,#93620,#93621,#93622,
#93623,#93624,#93625,#93626,#93627,#93628,#93629,#93630,#93631,#93632,#93633,
#93634,#93635,#93636,#93637,#93638,#93639,#93640,#93641,#93642,#93643,#93644,
#93645,#93646,#93647,#93648,#93649,#93650,#93651,#93652,#93653,#93654,#93655,
#93656),(#93657,#93658,#93659,#93660,#93661,#93662,#93663,#93664,#93665,
#93666,#93667,#93668,#93669,#93670,#93671,#93672,#93673,#93674,#93675,#93676,
#93677,#93678,#93679,#93680,#93681,#93682,#93683,#93684,#93685,#93686,#93687,
#93688,#93689,#93690,#93691,#93692,#93693,#93694,#93695,#93696,#93697,#93698,
#93699,#93700,#93701,#93702,#93703,#93704,#93705,#93706,#93707,#93708,#93709,
#93710,#93711,#93712,#93713,#93714,#93715,#93716,#93717,#93718,#93719,#93720,
#93721,#93722,#93723,#93724,#93725,#93726,#93727,#93728,#93729,#93730,#93731,
#93732,#93733,#93734,#93735,#93736,#93737,#93738,#93739,#93740,#93741,#93742,
#93743,#93744,#93745,#93746,#93747,#93748,#93749,#93750,#93751,#93752,#93753,
#93754,#93755,#93756,#93757,#93758,#93759,#93760,#93761,#93762,#93763,#93764,
#93765,#93766,#93767,#93768,#93769,#93770,#93771,#93772,#93773,#93774,#93775,
#93776,#93777,#93778,#93779,#93780,#93781,#93782,#93783,#93784,#93785,#93786,
#93787,#93788,#93789,#93790,#93791,#93792,#93793,#93794,#93795,#93796,#93797,
#93798,#93799,#93800,#93801,#93802,#93803,#93804,#93805,#93806,#93807),
(#93808,#93809,#93810,#93811,#93812,#93813,#93814,#93815,#93816,#93817,
#93818,#93819,#93820,#93821,#93822,#93823,#93824,#93825,#93826,#93827,#93828,
#93829,#93830,#93831,#93832,#93833,#93834,#93835,#93836,#93837,#93838,#93839,
#93840,#93841,#93842,#93843,#93844,#93845,#93846,#93847,#93848,#93849,#93850,
#93851,#93852,#93853,#93854,#93855,#93856,#93857,#93858,#93859,#93860,#93861,
#93862,#93863,#93864,#93865,#93866,#93867,#93868,#93869,#93870,#93871,#93872,
#93873,#93874,#93875,#93876,#93877,#93878,#93879,#93880,#93881,#93882,#93883,
#93884,#93885,#93886,#93887,#93888,#93889,#93890,#93891,#93892,#93893,#93894,
#93895,#93896,#93897,#93898,#93899,#93900,#93901,#93902,#93903,#93904,#93905,
#93906,#93907,#93908,#93909,#93910,#93911,#93912,#93913,#93914,#93915,#93916,
#93917,#93918,#93919,#93920,#93921,#93922,#93923,#93924,#93925,#93926,#93927,
#93928,#93929,#93930,#93931,#93932,#93933,#93934,#93935,#93936,#93937,#93938,
#93939,#93940,#93941,#93942,#93943,#93944,#93945,#93946,#93947,#93948,#93949,
#93950,#93951,#93952,#93953,#93954,#93955,#93956,#93957,#93958)),
 .UNSPECIFIED.,.F.,.F.,.F.,(4,4),(4,1,1,1,1,1,1,1,1,1,1,1,1,1,1,1,1,1,1,
1,1,1,1,1,1,1,1,1,1,1,1,1,1,1,1,1,1,1,1,1,1,1,1,1,1,1,1,1,1,1,1,1,1,1,1,
1,1,1,1,1,1,1,1,1,1,1,1,1,1,1,1,1,1,1,1,1,1,1,1,1,1,1,1,1,1,1,1,1,1,1,1,
1,1,1,1,1,1,1,1,1,1,1,1,1,1,1,1,1,1,1,1,1,1,1,1,1,1,1,1,1,1,1,1,1,1,1,1,
1,1,1,1,1,1,1,1,1,1,1,1,1,1,1,1,1,1,1,1,1,4),(0.,0.0820126057383863),(11.6152142277547,
12.6095559156426,13.6038976035304,14.5982392914182,15.592580979306,16.5869226671939,
17.5812643550817,18.5756060429695,19.5699477308573,20.5642894187452,21.558631106633,
22.5529727945208,23.5473144824086,24.5416561702965,25.5359978581843,26.5303395460721,
27.52468123396,28.5190229218478,29.5133646097356,30.5077062976234,31.5020479855113,
32.4963896733991,33.4907313612869,34.4850730491747,35.4794147370626,36.4737564249504,
37.4680981128382,38.462439800726,39.4567814886139,40.4511231765017,41.4454648643895,
42.4398065522773,43.4341482401652,44.428489928053,45.4228316159408,46.4171733038286,
47.4115149917165,48.4058566796043,49.4001983674921,50.3945400553799,51.3888817432678,
52.3832234311556,53.3775651190434,54.3719068069313,55.3662484948191,56.3605901827069,
57.3549318705947,58.3492735584826,59.3436152463704,60.3379569342582,61.332298622146,
62.3266403100339,63.3209819979217,64.3153236858095,65.3096653736973,66.3040070615852,
67.298348749473,68.2926904373608,69.2870321252486,70.2813738131365,71.2757155010243,
72.2700571889121,73.2643988768,74.2587405646878,75.2530822525756,76.2474239404634,
77.2417656283513,78.2361073162391,79.2304490041269,80.2247906920147,81.2191323799026,
82.2134740677904,83.2078157556782,84.202157443566,85.1964991314539,86.1908408193417,
87.1851825072295,88.1795241951173,89.1738658830052,90.168207570893,91.1625492587808,
92.1568909466686,93.1512326345565,94.1455743224443,95.1399160103321,96.13425769822,
97.1285993861078,98.1229410739956,99.1172827618834,100.111624449771,101.105966137659,
102.100307825547,103.094649513435,104.088991201323,105.08333288921,106.077674577098,
107.072016264986,108.066357952874,109.060699640762,110.05504132865,111.049383016537,
112.043724704425,113.038066392313,114.032408080201,115.026749768089,116.021091455976,
117.015433143864,118.009774831752,119.00411651964,119.998458207528,120.992799895416,
121.987141583303,122.981483271191,123.975824959079,124.970166646967,125.964508334855,
126.958850022743,127.95319171063,128.947533398518,129.941875086406,130.936216774294,
131.930558462182,132.92490015007,133.919241837957,134.913583525845,135.907925213733,
136.902266901621,137.896608589509,138.890950277396,139.885291965284,140.879633653172,
141.87397534106,142.868317028948,143.862658716836,144.857000404723,145.851342092611,
146.845683780499,147.840025468387,148.834367156275,149.828708844163,150.82305053205,
151.817392219938,152.811733907826,153.806075595714,154.800417283602,155.79475897149,
156.789100659377,157.783442347265,158.777784035153),.UNSPECIFIED.);
#891=SHAPE_REPRESENTATION_RELATIONSHIP('SRR','None',#94371,#905);
#892=SHAPE_REPRESENTATION_RELATIONSHIP('SRR','None',#94372,#906);
#893=SHAPE_REPRESENTATION_RELATIONSHIP('SRR','None',#94373,#907);
#894=SHAPE_REPRESENTATION_RELATIONSHIP('SRR','None',#94374,#908);
#895=SHAPE_REPRESENTATION_RELATIONSHIP('SRR','None',#94375,#909);
#896=SHAPE_REPRESENTATION_RELATIONSHIP('SRR','None',#94376,#910);
#897=SHAPE_REPRESENTATION_RELATIONSHIP('SRR','None',#94377,#911);
#898=SHAPE_REPRESENTATION_RELATIONSHIP('SRR','None',#94378,#912);
#899=SHAPE_REPRESENTATION_RELATIONSHIP('SRR','None',#94379,#913);
#900=SHAPE_REPRESENTATION_RELATIONSHIP('SRR','None',#94380,#914);
#901=SHAPE_REPRESENTATION_RELATIONSHIP('SRR','None',#94381,#915);
#902=SHAPE_REPRESENTATION_RELATIONSHIP('SRR','None',#94382,#916);
#903=SHAPE_REPRESENTATION_RELATIONSHIP('SRR','None',#94383,#917);
#904=SHAPE_REPRESENTATION_RELATIONSHIP('SRR','None',#94384,#918);
#905=ADVANCED_BREP_SHAPE_REPRESENTATION('',(#933),#94287);
#906=ADVANCED_BREP_SHAPE_REPRESENTATION('',(#934),#94288);
#907=ADVANCED_BREP_SHAPE_REPRESENTATION('',(#935),#94289);
#908=ADVANCED_BREP_SHAPE_REPRESENTATION('',(#936),#94290);
#909=ADVANCED_BREP_SHAPE_REPRESENTATION('',(#937),#94291);
#910=ADVANCED_BREP_SHAPE_REPRESENTATION('',(#938),#94292);
#911=ADVANCED_BREP_SHAPE_REPRESENTATION('',(#939),#94293);
#912=ADVANCED_BREP_SHAPE_REPRESENTATION('',(#940),#94294);
#913=ADVANCED_BREP_SHAPE_REPRESENTATION('',(#941),#94295);
#914=ADVANCED_BREP_SHAPE_REPRESENTATION('',(#942),#94296);
#915=ADVANCED_BREP_SHAPE_REPRESENTATION('',(#943),#94297);
#916=ADVANCED_BREP_SHAPE_REPRESENTATION('',(#944),#94298);
#917=ADVANCED_BREP_SHAPE_REPRESENTATION('',(#945),#94299);
#918=ADVANCED_BREP_SHAPE_REPRESENTATION('',(#946),#94300);
#919=STYLED_ITEM('',(#94567),#933);
#920=STYLED_ITEM('',(#94595),#934);
#921=STYLED_ITEM('',(#94574),#935);
#922=STYLED_ITEM('',(#94560),#936);
#923=STYLED_ITEM('',(#94574),#937);
#924=STYLED_ITEM('',(#94588),#938);
#925=STYLED_ITEM('',(#94588),#939);
#926=STYLED_ITEM('',(#94588),#940);
#927=STYLED_ITEM('',(#94588),#941);
#928=STYLED_ITEM('',(#94595),#942);
#929=STYLED_ITEM('',(#94588),#943);
#930=STYLED_ITEM('',(#94588),#944);
#931=STYLED_ITEM('',(#94588),#945);
#932=STYLED_ITEM('',(#94588),#946);
#933=MANIFOLD_SOLID_BREP('Body1',#51018);
#934=MANIFOLD_SOLID_BREP('Body1',#51019);
#935=MANIFOLD_SOLID_BREP('Body1',#51020);
#936=MANIFOLD_SOLID_BREP('Body1',#51021);
#937=MANIFOLD_SOLID_BREP('Body1',#51022);
#938=MANIFOLD_SOLID_BREP('Body1',#51023);
#939=MANIFOLD_SOLID_BREP('Body1',#51024);
#940=MANIFOLD_SOLID_BREP('Body1',#51025);
#941=MANIFOLD_SOLID_BREP('Body1',#51026);
#942=MANIFOLD_SOLID_BREP('Body1',#51027);
#943=MANIFOLD_SOLID_BREP('Body1',#51028);
#944=MANIFOLD_SOLID_BREP('Body1',#51029);
#945=MANIFOLD_SOLID_BREP('Body1',#51030);
#946=MANIFOLD_SOLID_BREP('Body1',#51031);
#947=TOROIDAL_SURFACE('',#53576,45.,6.);
#948=TOROIDAL_SURFACE('',#53582,46.9,0.4);
#949=TOROIDAL_SURFACE('',#53592,46.9,0.4);
#950=TOROIDAL_SURFACE('',#54103,33.,1.);
#951=TOROIDAL_SURFACE('',#54112,33.,1.);
#952=TOROIDAL_SURFACE('',#54120,25.,1.);
#953=TOROIDAL_SURFACE('',#54126,25.,1.);
#954=TOROIDAL_SURFACE('',#54190,21.5,1.5);
#955=TOROIDAL_SURFACE('',#54535,5.325,0.4);
#956=TOROIDAL_SURFACE('',#54901,3.192,0.25);
#957=TOROIDAL_SURFACE('',#55179,2.06862915010152,0.8);
#958=TOROIDAL_SURFACE('',#55249,4.333,0.4);
#959=FACE_BOUND('',#17303,.T.);
#960=FACE_BOUND('',#17309,.T.);
#961=FACE_BOUND('',#17312,.T.);
#962=FACE_BOUND('',#17315,.T.);
#963=FACE_BOUND('',#17327,.T.);
#964=FACE_BOUND('',#17673,.T.);
#965=FACE_BOUND('',#17677,.T.);
#966=FACE_BOUND('',#17686,.T.);
#967=FACE_BOUND('',#17688,.T.);
#968=FACE_BOUND('',#17690,.T.);
#969=FACE_BOUND('',#17694,.T.);
#970=FACE_BOUND('',#17695,.T.);
#971=FACE_BOUND('',#17696,.T.);
#972=FACE_BOUND('',#17697,.T.);
#973=FACE_BOUND('',#17698,.T.);
#974=FACE_BOUND('',#17699,.T.);
#975=FACE_BOUND('',#17700,.T.);
#976=FACE_BOUND('',#17710,.T.);
#977=FACE_BOUND('',#17713,.T.);
#978=FACE_BOUND('',#17716,.T.);
#979=FACE_BOUND('',#17719,.T.);
#980=FACE_BOUND('',#17729,.T.);
#981=FACE_BOUND('',#17730,.T.);
#982=FACE_BOUND('',#17731,.T.);
#983=FACE_BOUND('',#17732,.T.);
#984=FACE_BOUND('',#17733,.T.);
#985=FACE_BOUND('',#17734,.T.);
#986=FACE_BOUND('',#17735,.T.);
#987=FACE_BOUND('',#17740,.T.);
#988=FACE_BOUND('',#17744,.T.);
#989=FACE_BOUND('',#18062,.T.);
#990=FACE_BOUND('',#18063,.T.);
#991=FACE_BOUND('',#18064,.T.);
#992=FACE_BOUND('',#18065,.T.);
#993=FACE_BOUND('',#18066,.T.);
#994=FACE_BOUND('',#18067,.T.);
#995=FACE_BOUND('',#18068,.T.);
#996=FACE_BOUND('',#18069,.T.);
#997=FACE_BOUND('',#18070,.T.);
#998=FACE_BOUND('',#18071,.T.);
#999=FACE_BOUND('',#18072,.T.);
#1000=FACE_BOUND('',#18073,.T.);
#1001=FACE_BOUND('',#18074,.T.);
#1002=FACE_BOUND('',#18075,.T.);
#1003=FACE_BOUND('',#18076,.T.);
#1004=FACE_BOUND('',#18077,.T.);
#1005=FACE_BOUND('',#18078,.T.);
#1006=FACE_BOUND('',#18079,.T.);
#1007=FACE_BOUND('',#18080,.T.);
#1008=FACE_BOUND('',#18081,.T.);
#1009=FACE_BOUND('',#18082,.T.);
#1010=FACE_BOUND('',#18083,.T.);
#1011=FACE_BOUND('',#18084,.T.);
#1012=FACE_BOUND('',#18088,.T.);
#1013=FACE_BOUND('',#18089,.T.);
#1014=FACE_BOUND('',#18090,.T.);
#1015=FACE_BOUND('',#18091,.T.);
#1016=FACE_BOUND('',#18092,.T.);
#1017=FACE_BOUND('',#18093,.T.);
#1018=FACE_BOUND('',#18094,.T.);
#1019=FACE_BOUND('',#18095,.T.);
#1020=FACE_BOUND('',#18096,.T.);
#1021=FACE_BOUND('',#18097,.T.);
#1022=FACE_BOUND('',#18098,.T.);
#1023=FACE_BOUND('',#18099,.T.);
#1024=FACE_BOUND('',#18102,.T.);
#1025=FACE_BOUND('',#18103,.T.);
#1026=FACE_BOUND('',#18104,.T.);
#1027=FACE_BOUND('',#18105,.T.);
#1028=FACE_BOUND('',#18160,.T.);
#1029=FACE_BOUND('',#18165,.T.);
#1030=FACE_BOUND('',#18207,.T.);
#1031=FACE_BOUND('',#18360,.T.);
#1032=FACE_BOUND('',#18366,.T.);
#1033=FACE_BOUND('',#18371,.T.);
#1034=FACE_BOUND('',#18376,.T.);
#1035=FACE_BOUND('',#18428,.T.);
#1036=FACE_BOUND('',#18581,.T.);
#1037=FACE_BOUND('',#18587,.T.);
#1038=FACE_BOUND('',#18648,.T.);
#1039=FACE_BOUND('',#18661,.T.);
#1040=FACE_BOUND('',#18666,.T.);
#1041=FACE_BOUND('',#18671,.T.);
#1042=FACE_BOUND('',#18695,.T.);
#1043=FACE_BOUND('',#18697,.T.);
#1044=CYLINDRICAL_SURFACE('',#51779,42.3);
#1045=CYLINDRICAL_SURFACE('',#51830,42.3);
#1046=CYLINDRICAL_SURFACE('',#51881,42.3);
#1047=CYLINDRICAL_SURFACE('',#51932,42.3);
#1048=CYLINDRICAL_SURFACE('',#51983,42.3);
#1049=CYLINDRICAL_SURFACE('',#52034,42.3);
#1050=CYLINDRICAL_SURFACE('',#52085,42.3);
#1051=CYLINDRICAL_SURFACE('',#52136,42.3);
#1052=CYLINDRICAL_SURFACE('',#52187,42.3);
#1053=CYLINDRICAL_SURFACE('',#52238,42.3);
#1054=CYLINDRICAL_SURFACE('',#52289,42.3);
#1055=CYLINDRICAL_SURFACE('',#52340,42.3);
#1056=CYLINDRICAL_SURFACE('',#52391,42.3);
#1057=CYLINDRICAL_SURFACE('',#52442,42.3);
#1058=CYLINDRICAL_SURFACE('',#52493,42.3);
#1059=CYLINDRICAL_SURFACE('',#52544,42.3);
#1060=CYLINDRICAL_SURFACE('',#52595,42.3);
#1061=CYLINDRICAL_SURFACE('',#52646,42.3);
#1062=CYLINDRICAL_SURFACE('',#52697,42.3);
#1063=CYLINDRICAL_SURFACE('',#52748,42.3);
#1064=CYLINDRICAL_SURFACE('',#52799,42.3);
#1065=CYLINDRICAL_SURFACE('',#52850,42.3);
#1066=CYLINDRICAL_SURFACE('',#52901,42.3);
#1067=CYLINDRICAL_SURFACE('',#52952,42.3);
#1068=CYLINDRICAL_SURFACE('',#53003,42.3);
#1069=CYLINDRICAL_SURFACE('',#53054,42.3);
#1070=CYLINDRICAL_SURFACE('',#53105,42.3);
#1071=CYLINDRICAL_SURFACE('',#53156,42.3);
#1072=CYLINDRICAL_SURFACE('',#53207,42.3);
#1073=CYLINDRICAL_SURFACE('',#53258,42.3);
#1074=CYLINDRICAL_SURFACE('',#53309,42.3);
#1075=CYLINDRICAL_SURFACE('',#53360,42.3);
#1076=CYLINDRICAL_SURFACE('',#53411,42.3);
#1077=CYLINDRICAL_SURFACE('',#53462,42.3);
#1078=CYLINDRICAL_SURFACE('',#53513,42.3);
#1079=CYLINDRICAL_SURFACE('',#53580,51.);
#1080=CYLINDRICAL_SURFACE('',#53587,46.5);
#1081=CYLINDRICAL_SURFACE('',#53597,42.3);
#1082=CYLINDRICAL_SURFACE('',#53602,50.5);
#1083=CYLINDRICAL_SURFACE('',#53605,50.4);
#1084=CYLINDRICAL_SURFACE('',#53612,37.8);
#1085=CYLINDRICAL_SURFACE('',#53689,37.8);
#1086=CYLINDRICAL_SURFACE('',#53706,37.8);
#1087=CYLINDRICAL_SURFACE('',#53942,37.8);
#1088=CYLINDRICAL_SURFACE('',#53943,37.8);
#1089=CYLINDRICAL_SURFACE('',#53948,37.8);
#1090=CYLINDRICAL_SURFACE('',#53953,37.8);
#1091=CYLINDRICAL_SURFACE('',#53958,37.8);
#1092=CYLINDRICAL_SURFACE('',#53963,37.8);
#1093=CYLINDRICAL_SURFACE('',#53968,37.8);
#1094=CYLINDRICAL_SURFACE('',#53973,37.8);
#1095=CYLINDRICAL_SURFACE('',#53978,37.8);
#1096=CYLINDRICAL_SURFACE('',#53983,37.8);
#1097=CYLINDRICAL_SURFACE('',#53988,37.8);
#1098=CYLINDRICAL_SURFACE('',#53993,37.8);
#1099=CYLINDRICAL_SURFACE('',#53998,37.8);
#1100=CYLINDRICAL_SURFACE('',#54003,37.8);
#1101=CYLINDRICAL_SURFACE('',#54008,37.8);
#1102=CYLINDRICAL_SURFACE('',#54013,37.8);
#1103=CYLINDRICAL_SURFACE('',#54018,37.8);
#1104=CYLINDRICAL_SURFACE('',#54023,37.8);
#1105=CYLINDRICAL_SURFACE('',#54028,37.8);
#1106=CYLINDRICAL_SURFACE('',#54033,37.8);
#1107=CYLINDRICAL_SURFACE('',#54038,37.8);
#1108=CYLINDRICAL_SURFACE('',#54043,37.8);
#1109=CYLINDRICAL_SURFACE('',#54048,37.8);
#1110=CYLINDRICAL_SURFACE('',#54053,37.8);
#1111=CYLINDRICAL_SURFACE('',#54058,37.8);
#1112=CYLINDRICAL_SURFACE('',#54063,37.8);
#1113=CYLINDRICAL_SURFACE('',#54068,37.8);
#1114=CYLINDRICAL_SURFACE('',#54073,37.8);
#1115=CYLINDRICAL_SURFACE('',#54078,37.8);
#1116=CYLINDRICAL_SURFACE('',#54083,37.8);
#1117=CYLINDRICAL_SURFACE('',#54088,37.8);
#1118=CYLINDRICAL_SURFACE('',#54093,37.8);
#1119=CYLINDRICAL_SURFACE('',#54098,37.8);
#1120=CYLINDRICAL_SURFACE('',#54110,34.);
#1121=CYLINDRICAL_SURFACE('',#54119,34.);
#1122=CYLINDRICAL_SURFACE('',#54124,24.);
#1123=CYLINDRICAL_SURFACE('',#54130,24.);
#1124=CYLINDRICAL_SURFACE('',#54132,15.01);
#1125=CYLINDRICAL_SURFACE('',#54154,3.);
#1126=CYLINDRICAL_SURFACE('',#54158,3.);
#1127=CYLINDRICAL_SURFACE('',#54160,3.3);
#1128=CYLINDRICAL_SURFACE('',#54163,3.3);
#1129=CYLINDRICAL_SURFACE('',#54166,3.3);
#1130=CYLINDRICAL_SURFACE('',#54169,3.3);
#1131=CYLINDRICAL_SURFACE('',#54172,5.5);
#1132=CYLINDRICAL_SURFACE('',#54175,5.5);
#1133=CYLINDRICAL_SURFACE('',#54178,5.5);
#1134=CYLINDRICAL_SURFACE('',#54181,5.5);
#1135=CYLINDRICAL_SURFACE('',#54186,5.05);
#1136=CYLINDRICAL_SURFACE('',#54194,20.);
#1137=CYLINDRICAL_SURFACE('',#54200,20.);
#1138=CYLINDRICAL_SURFACE('',#54206,48.);
#1139=CYLINDRICAL_SURFACE('',#54211,14.995);
#1140=CYLINDRICAL_SURFACE('',#54371,4.5);
#1141=CYLINDRICAL_SURFACE('',#54400,4.5);
#1142=CYLINDRICAL_SURFACE('',#54405,4.5);
#1143=CYLINDRICAL_SURFACE('',#54410,4.5);
#1144=CYLINDRICAL_SURFACE('',#54415,3.);
#1145=CYLINDRICAL_SURFACE('',#54418,3.);
#1146=CYLINDRICAL_SURFACE('',#54423,3.05);
#1147=CYLINDRICAL_SURFACE('',#54428,3.05);
#1148=CYLINDRICAL_SURFACE('',#54433,3.05);
#1149=CYLINDRICAL_SURFACE('',#54438,3.05);
#1150=CYLINDRICAL_SURFACE('',#54439,20.025);
#1151=CYLINDRICAL_SURFACE('',#54455,10.);
#1152=CYLINDRICAL_SURFACE('',#54458,10.);
#1153=CYLINDRICAL_SURFACE('',#54470,10.);
#1154=CYLINDRICAL_SURFACE('',#54472,10.);
#1155=CYLINDRICAL_SURFACE('',#54475,5.5);
#1156=CYLINDRICAL_SURFACE('',#54484,28.);
#1157=CYLINDRICAL_SURFACE('',#54492,4.925);
#1158=CYLINDRICAL_SURFACE('',#54494,4.925);
#1159=CYLINDRICAL_SURFACE('',#54495,4.925);
#1160=CYLINDRICAL_SURFACE('',#54496,4.925);
#1161=CYLINDRICAL_SURFACE('',#54497,4.925);
#1162=CYLINDRICAL_SURFACE('',#54498,4.925);
#1163=CYLINDRICAL_SURFACE('',#54499,4.925);
#1164=CYLINDRICAL_SURFACE('',#54500,4.925);
#1165=CYLINDRICAL_SURFACE('',#54501,4.925);
#1166=CYLINDRICAL_SURFACE('',#54502,4.925);
#1167=CYLINDRICAL_SURFACE('',#54503,4.925);
#1168=CYLINDRICAL_SURFACE('',#54504,4.925);
#1169=CYLINDRICAL_SURFACE('',#54505,4.925);
#1170=CYLINDRICAL_SURFACE('',#54506,4.925);
#1171=CYLINDRICAL_SURFACE('',#54507,4.925);
#1172=CYLINDRICAL_SURFACE('',#54508,4.925);
#1173=CYLINDRICAL_SURFACE('',#54509,4.0705);
#1174=CYLINDRICAL_SURFACE('',#54511,4.0705);
#1175=CYLINDRICAL_SURFACE('',#54513,4.0705);
#1176=CYLINDRICAL_SURFACE('',#54514,4.0705);
#1177=CYLINDRICAL_SURFACE('',#54515,4.0705);
#1178=CYLINDRICAL_SURFACE('',#54516,4.0705);
#1179=CYLINDRICAL_SURFACE('',#54517,4.0705);
#1180=CYLINDRICAL_SURFACE('',#54518,4.0705);
#1181=CYLINDRICAL_SURFACE('',#54519,4.0705);
#1182=CYLINDRICAL_SURFACE('',#54520,4.0705);
#1183=CYLINDRICAL_SURFACE('',#54521,4.0705);
#1184=CYLINDRICAL_SURFACE('',#54522,4.0705);
#1185=CYLINDRICAL_SURFACE('',#54523,4.0705);
#1186=CYLINDRICAL_SURFACE('',#54524,4.0705);
#1187=CYLINDRICAL_SURFACE('',#54525,4.0705);
#1188=CYLINDRICAL_SURFACE('',#54526,4.0705);
#1189=CYLINDRICAL_SURFACE('',#54534,4.0705);
#1190=CYLINDRICAL_SURFACE('',#54539,4.925);
#1191=CYLINDRICAL_SURFACE('',#54772,8.);
#1192=CYLINDRICAL_SURFACE('',#54816,10.);
#1193=CYLINDRICAL_SURFACE('',#54824,5.25);
#1194=CYLINDRICAL_SURFACE('',#54830,5.1);
#1195=CYLINDRICAL_SURFACE('',#54834,9.05);
#1196=CYLINDRICAL_SURFACE('',#54845,9.05);
#1197=CYLINDRICAL_SURFACE('',#54853,5.1);
#1198=CYLINDRICAL_SURFACE('',#54859,2.942);
#1199=CYLINDRICAL_SURFACE('',#54861,2.942);
#1200=CYLINDRICAL_SURFACE('',#54862,2.942);
#1201=CYLINDRICAL_SURFACE('',#54863,2.942);
#1202=CYLINDRICAL_SURFACE('',#54864,2.942);
#1203=CYLINDRICAL_SURFACE('',#54865,2.942);
#1204=CYLINDRICAL_SURFACE('',#54866,2.942);
#1205=CYLINDRICAL_SURFACE('',#54867,2.942);
#1206=CYLINDRICAL_SURFACE('',#54868,2.942);
#1207=CYLINDRICAL_SURFACE('',#54869,2.942);
#1208=CYLINDRICAL_SURFACE('',#54870,2.942);
#1209=CYLINDRICAL_SURFACE('',#54871,2.942);
#1210=CYLINDRICAL_SURFACE('',#54872,2.942);
#1211=CYLINDRICAL_SURFACE('',#54873,2.942);
#1212=CYLINDRICAL_SURFACE('',#54874,2.942);
#1213=CYLINDRICAL_SURFACE('',#54875,2.942);
#1214=CYLINDRICAL_SURFACE('',#54877,2.37175);
#1215=CYLINDRICAL_SURFACE('',#54879,2.37175);
#1216=CYLINDRICAL_SURFACE('',#54880,2.37175);
#1217=CYLINDRICAL_SURFACE('',#54881,2.37175);
#1218=CYLINDRICAL_SURFACE('',#54882,2.37175);
#1219=CYLINDRICAL_SURFACE('',#54883,2.37175);
#1220=CYLINDRICAL_SURFACE('',#54884,2.37175);
#1221=CYLINDRICAL_SURFACE('',#54885,2.37175);
#1222=CYLINDRICAL_SURFACE('',#54886,2.37175);
#1223=CYLINDRICAL_SURFACE('',#54887,2.37175);
#1224=CYLINDRICAL_SURFACE('',#54888,2.37175);
#1225=CYLINDRICAL_SURFACE('',#54889,2.37175);
#1226=CYLINDRICAL_SURFACE('',#54890,2.37175);
#1227=CYLINDRICAL_SURFACE('',#54891,2.37175);
#1228=CYLINDRICAL_SURFACE('',#54892,2.37175);
#1229=CYLINDRICAL_SURFACE('',#54900,2.37175);
#1230=CYLINDRICAL_SURFACE('',#54905,2.942);
#1231=CYLINDRICAL_SURFACE('',#55138,5.);
#1232=CYLINDRICAL_SURFACE('',#55191,3.);
#1233=CYLINDRICAL_SURFACE('',#55193,3.933);
#1234=CYLINDRICAL_SURFACE('',#55195,3.933);
#1235=CYLINDRICAL_SURFACE('',#55196,3.933);
#1236=CYLINDRICAL_SURFACE('',#55197,3.933);
#1237=CYLINDRICAL_SURFACE('',#55198,3.933);
#1238=CYLINDRICAL_SURFACE('',#55199,3.933);
#1239=CYLINDRICAL_SURFACE('',#55200,3.933);
#1240=CYLINDRICAL_SURFACE('',#55201,3.933);
#1241=CYLINDRICAL_SURFACE('',#55202,3.933);
#1242=CYLINDRICAL_SURFACE('',#55203,3.933);
#1243=CYLINDRICAL_SURFACE('',#55204,3.933);
#1244=CYLINDRICAL_SURFACE('',#55205,3.933);
#1245=CYLINDRICAL_SURFACE('',#55206,3.933);
#1246=CYLINDRICAL_SURFACE('',#55207,3.933);
#1247=CYLINDRICAL_SURFACE('',#55208,3.933);
#1248=CYLINDRICAL_SURFACE('',#55209,3.933);
#1249=CYLINDRICAL_SURFACE('',#55210,3.933);
#1250=CYLINDRICAL_SURFACE('',#55211,3.933);
#1251=CYLINDRICAL_SURFACE('',#55212,3.933);
#1252=CYLINDRICAL_SURFACE('',#55213,3.933);
#1253=CYLINDRICAL_SURFACE('',#55214,3.933);
#1254=CYLINDRICAL_SURFACE('',#55215,3.933);
#1255=CYLINDRICAL_SURFACE('',#55216,3.933);
#1256=CYLINDRICAL_SURFACE('',#55217,3.22275);
#1257=CYLINDRICAL_SURFACE('',#55219,3.22275);
#1258=CYLINDRICAL_SURFACE('',#55220,3.22275);
#1259=CYLINDRICAL_SURFACE('',#55221,3.22275);
#1260=CYLINDRICAL_SURFACE('',#55222,3.22275);
#1261=CYLINDRICAL_SURFACE('',#55223,3.22275);
#1262=CYLINDRICAL_SURFACE('',#55224,3.22275);
#1263=CYLINDRICAL_SURFACE('',#55225,3.22275);
#1264=CYLINDRICAL_SURFACE('',#55226,3.22275);
#1265=CYLINDRICAL_SURFACE('',#55227,3.22275);
#1266=CYLINDRICAL_SURFACE('',#55228,3.22275);
#1267=CYLINDRICAL_SURFACE('',#55229,3.22275);
#1268=CYLINDRICAL_SURFACE('',#55230,3.22275);
#1269=CYLINDRICAL_SURFACE('',#55231,3.22275);
#1270=CYLINDRICAL_SURFACE('',#55232,3.22275);
#1271=CYLINDRICAL_SURFACE('',#55233,3.22275);
#1272=CYLINDRICAL_SURFACE('',#55234,3.22275);
#1273=CYLINDRICAL_SURFACE('',#55235,3.22275);
#1274=CYLINDRICAL_SURFACE('',#55236,3.22275);
#1275=CYLINDRICAL_SURFACE('',#55237,3.22275);
#1276=CYLINDRICAL_SURFACE('',#55238,3.22275);
#1277=CYLINDRICAL_SURFACE('',#55239,3.22275);
#1278=CYLINDRICAL_SURFACE('',#55240,3.22275);
#1279=CYLINDRICAL_SURFACE('',#55248,3.22275);
#1280=CYLINDRICAL_SURFACE('',#55253,3.933);
#1281=CYLINDRICAL_SURFACE('',#55261,5.8);
#1282=CYLINDRICAL_SURFACE('',#55275,8.);
#1283=CYLINDRICAL_SURFACE('',#55283,4.2);
#1284=CYLINDRICAL_SURFACE('',#55289,7.4);
#1285=CYLINDRICAL_SURFACE('',#55301,7.4);
#1286=CYLINDRICAL_SURFACE('',#55309,4.05);
#1287=CYLINDRICAL_SURFACE('',#55318,4.05);
#1288=ELLIPSE('',#51263,65.1465238200804,42.3);
#1289=ELLIPSE('',#51266,65.1465238200804,42.3);
#1290=ELLIPSE('',#51269,65.1465238200804,42.3);
#1291=ELLIPSE('',#51272,65.1465238200804,42.3);
#1292=ELLIPSE('',#51275,65.1465238200804,42.3);
#1293=ELLIPSE('',#51278,65.1465238200804,42.3);
#1294=ELLIPSE('',#51281,65.1465238200804,42.3);
#1295=ELLIPSE('',#51284,65.1465238200804,42.3);
#1296=ELLIPSE('',#51287,65.1465238200804,42.3);
#1297=ELLIPSE('',#51290,65.1465238200804,42.3);
#1298=ELLIPSE('',#51293,65.1465238200804,42.3);
#1299=ELLIPSE('',#51296,65.1465238200804,42.3);
#1300=ELLIPSE('',#51299,65.1465238200804,42.3);
#1301=ELLIPSE('',#51302,65.1465238200804,42.3);
#1302=ELLIPSE('',#51305,65.1465238200804,42.3);
#1303=ELLIPSE('',#51308,65.1465238200804,42.3);
#1304=ELLIPSE('',#51311,65.1465238200804,42.3);
#1305=ELLIPSE('',#51314,65.1465238200804,42.3);
#1306=ELLIPSE('',#51317,65.1465238200804,42.3);
#1307=ELLIPSE('',#51320,65.1465238200804,42.3);
#1308=ELLIPSE('',#51323,65.1465238200804,42.3);
#1309=ELLIPSE('',#51326,65.1465238200804,42.3);
#1310=ELLIPSE('',#51329,65.1465238200804,42.3);
#1311=ELLIPSE('',#51332,65.1465238200804,42.3);
#1312=ELLIPSE('',#51335,65.1465238200804,42.3);
#1313=ELLIPSE('',#51338,65.1465238200804,42.3);
#1314=ELLIPSE('',#51341,65.1465238200804,42.3);
#1315=ELLIPSE('',#51344,65.1465238200804,42.3);
#1316=ELLIPSE('',#51347,65.1465238200804,42.3);
#1317=ELLIPSE('',#51350,65.1465238200804,42.3);
#1318=ELLIPSE('',#51353,65.1465238200804,42.3);
#1319=ELLIPSE('',#51356,65.1465238200804,42.3);
#1320=ELLIPSE('',#51359,65.1465238200804,42.3);
#1321=ELLIPSE('',#51362,65.1465238200804,42.3);
#1322=ELLIPSE('',#51365,65.1465238200804,42.3);
#1323=ELLIPSE('',#51368,65.1465238200804,42.3);
#1324=ELLIPSE('',#51442,65.1465238200804,42.3);
#1325=ELLIPSE('',#51444,65.1465238200804,42.3);
#1326=ELLIPSE('',#51446,65.1465238200804,42.3);
#1327=ELLIPSE('',#51448,65.1465238200804,42.3);
#1328=ELLIPSE('',#51450,65.1465238200804,42.3);
#1329=ELLIPSE('',#51452,65.1465238200804,42.3);
#1330=ELLIPSE('',#51454,65.1465238200804,42.3);
#1331=ELLIPSE('',#51456,65.1465238200804,42.3);
#1332=ELLIPSE('',#51458,65.1465238200804,42.3);
#1333=ELLIPSE('',#51460,65.1465238200804,42.3);
#1334=ELLIPSE('',#51462,65.1465238200804,42.3);
#1335=ELLIPSE('',#51464,65.1465238200804,42.3);
#1336=ELLIPSE('',#51466,65.1465238200804,42.3);
#1337=ELLIPSE('',#51468,65.1465238200804,42.3);
#1338=ELLIPSE('',#51470,65.1465238200804,42.3);
#1339=ELLIPSE('',#51472,65.1465238200804,42.3);
#1340=ELLIPSE('',#51474,65.1465238200804,42.3);
#1341=ELLIPSE('',#51476,65.1465238200804,42.3);
#1342=ELLIPSE('',#51478,65.1465238200804,42.3);
#1343=ELLIPSE('',#51480,65.1465238200804,42.3);
#1344=ELLIPSE('',#51482,65.1465238200804,42.3);
#1345=ELLIPSE('',#51484,65.1465238200804,42.3);
#1346=ELLIPSE('',#51486,65.1465238200804,42.3);
#1347=ELLIPSE('',#51488,65.1465238200804,42.3);
#1348=ELLIPSE('',#51490,65.1465238200804,42.3);
#1349=ELLIPSE('',#51492,65.1465238200804,42.3);
#1350=ELLIPSE('',#51494,65.1465238200804,42.3);
#1351=ELLIPSE('',#51496,65.1465238200804,42.3);
#1352=ELLIPSE('',#51498,65.1465238200804,42.3);
#1353=ELLIPSE('',#51500,65.1465238200804,42.3);
#1354=ELLIPSE('',#51502,65.1465238200804,42.3);
#1355=ELLIPSE('',#51504,65.1465238200804,42.3);
#1356=ELLIPSE('',#51506,65.1465238200804,42.3);
#1357=ELLIPSE('',#51508,65.1465238200804,42.3);
#1358=ELLIPSE('',#51510,65.1465238200804,42.3);
#1359=ELLIPSE('',#51512,65.1465238200804,42.3);
#1360=ELLIPSE('',#51550,65.1465238200804,42.3);
#1361=ELLIPSE('',#51552,65.1465238200804,42.3);
#1362=ELLIPSE('',#51554,65.1465238200804,42.3);
#1363=ELLIPSE('',#51556,65.1465238200804,42.3);
#1364=ELLIPSE('',#51558,65.1465238200804,42.3);
#1365=ELLIPSE('',#51560,65.1465238200804,42.3);
#1366=ELLIPSE('',#51562,65.1465238200804,42.3);
#1367=ELLIPSE('',#51564,65.1465238200804,42.3);
#1368=ELLIPSE('',#51566,65.1465238200804,42.3);
#1369=ELLIPSE('',#51568,65.1465238200804,42.3);
#1370=ELLIPSE('',#51570,65.1465238200804,42.3);
#1371=ELLIPSE('',#51572,65.1465238200804,42.3);
#1372=ELLIPSE('',#51574,65.1465238200804,42.3);
#1373=ELLIPSE('',#51576,65.1465238200804,42.3);
#1374=ELLIPSE('',#51578,65.1465238200804,42.3);
#1375=ELLIPSE('',#51580,65.1465238200804,42.3);
#1376=ELLIPSE('',#51582,65.1465238200804,42.3);
#1377=ELLIPSE('',#51584,65.1465238200804,42.3);
#1378=ELLIPSE('',#51586,65.1465238200804,42.3);
#1379=ELLIPSE('',#51588,65.1465238200804,42.3);
#1380=ELLIPSE('',#51590,65.1465238200804,42.3);
#1381=ELLIPSE('',#51592,65.1465238200804,42.3);
#1382=ELLIPSE('',#51594,65.1465238200804,42.3);
#1383=ELLIPSE('',#51596,65.1465238200804,42.3);
#1384=ELLIPSE('',#51598,65.1465238200804,42.3);
#1385=ELLIPSE('',#51600,65.1465238200804,42.3);
#1386=ELLIPSE('',#51602,65.1465238200804,42.3);
#1387=ELLIPSE('',#51604,65.1465238200804,42.3);
#1388=ELLIPSE('',#51606,65.1465238200804,42.3);
#1389=ELLIPSE('',#51608,65.1465238200804,42.3);
#1390=ELLIPSE('',#51610,65.1465238200804,42.3);
#1391=ELLIPSE('',#51612,65.1465238200804,42.3);
#1392=ELLIPSE('',#51614,65.1465238200804,42.3);
#1393=ELLIPSE('',#51616,65.1465238200804,42.3);
#1394=ELLIPSE('',#51618,65.1465238200804,42.3);
#1395=ELLIPSE('',#51694,42.7157063175375,42.3);
#1396=ELLIPSE('',#51696,684.784865862974,42.3);
#1397=ELLIPSE('',#51698,148.655022233233,42.3);
#1398=ELLIPSE('',#51700,86.0962585581534,42.3);
#1399=ELLIPSE('',#51702,135.078923826262,42.3);
#1400=ELLIPSE('',#51705,135.078923826262,42.3);
#1401=ELLIPSE('',#51707,86.0962585581532,42.3);
#1402=ELLIPSE('',#51709,148.655022233233,42.3);
#1403=ELLIPSE('',#51711,684.784865862975,42.3);
#1404=ELLIPSE('',#51713,42.7157063175375,42.3);
#1405=ELLIPSE('',#51716,65.1465238200804,42.3);
#1406=ELLIPSE('',#51719,42.7157063175375,42.3);
#1407=ELLIPSE('',#51721,684.784865862975,42.3);
#1408=ELLIPSE('',#51723,148.655022233233,42.3);
#1409=ELLIPSE('',#51725,86.0962585581532,42.3);
#1410=ELLIPSE('',#51727,135.078923826262,42.3);
#1411=ELLIPSE('',#51730,135.078923826262,42.3);
#1412=ELLIPSE('',#51732,86.0962585581534,42.3);
#1413=ELLIPSE('',#51734,148.655022233233,42.3);
#1414=ELLIPSE('',#51736,684.784865862974,42.3);
#1415=ELLIPSE('',#51738,42.7157063175375,42.3);
#1416=ELLIPSE('',#51781,65.1465238200804,42.3);
#1417=ELLIPSE('',#51782,42.7157063175375,42.3);
#1418=ELLIPSE('',#51783,684.784865862975,42.3);
#1419=ELLIPSE('',#51784,148.655022233233,42.3);
#1420=ELLIPSE('',#51785,86.0962585581532,42.3);
#1421=ELLIPSE('',#51786,135.078923826262,42.3);
#1422=ELLIPSE('',#51787,135.078923826262,42.3);
#1423=ELLIPSE('',#51788,86.0962585581534,42.3);
#1424=ELLIPSE('',#51789,148.655022233233,42.3);
#1425=ELLIPSE('',#51790,684.784865862974,42.3);
#1426=ELLIPSE('',#51791,42.7157063175375,42.3);
#1427=ELLIPSE('',#51808,42.7157063175375,42.3);
#1428=ELLIPSE('',#51810,684.784865862975,42.3);
#1429=ELLIPSE('',#51812,148.655022233233,42.3);
#1430=ELLIPSE('',#51814,86.0962585581532,42.3);
#1431=ELLIPSE('',#51816,135.078923826262,42.3);
#1432=ELLIPSE('',#51819,135.078923826262,42.3);
#1433=ELLIPSE('',#51821,86.0962585581534,42.3);
#1434=ELLIPSE('',#51823,148.655022233233,42.3);
#1435=ELLIPSE('',#51825,684.784865862974,42.3);
#1436=ELLIPSE('',#51827,42.7157063175375,42.3);
#1437=ELLIPSE('',#51832,65.1465238200804,42.3);
#1438=ELLIPSE('',#51833,42.7157063175375,42.3);
#1439=ELLIPSE('',#51834,684.784865862975,42.3);
#1440=ELLIPSE('',#51835,148.655022233233,42.3);
#1441=ELLIPSE('',#51836,86.0962585581532,42.3);
#1442=ELLIPSE('',#51837,135.078923826262,42.3);
#1443=ELLIPSE('',#51838,135.078923826262,42.3);
#1444=ELLIPSE('',#51839,86.0962585581534,42.3);
#1445=ELLIPSE('',#51840,148.655022233233,42.3);
#1446=ELLIPSE('',#51841,684.784865862974,42.3);
#1447=ELLIPSE('',#51842,42.7157063175375,42.3);
#1448=ELLIPSE('',#51859,42.7157063175375,42.3);
#1449=ELLIPSE('',#51861,684.784865862975,42.3);
#1450=ELLIPSE('',#51863,148.655022233233,42.3);
#1451=ELLIPSE('',#51865,86.0962585581532,42.3);
#1452=ELLIPSE('',#51867,135.078923826262,42.3);
#1453=ELLIPSE('',#51870,135.078923826262,42.3);
#1454=ELLIPSE('',#51872,86.0962585581534,42.3);
#1455=ELLIPSE('',#51874,148.655022233233,42.3);
#1456=ELLIPSE('',#51876,684.784865862974,42.3);
#1457=ELLIPSE('',#51878,42.7157063175375,42.3);
#1458=ELLIPSE('',#51883,65.1465238200804,42.3);
#1459=ELLIPSE('',#51884,42.7157063175375,42.3);
#1460=ELLIPSE('',#51885,684.784865862975,42.3);
#1461=ELLIPSE('',#51886,148.655022233233,42.3);
#1462=ELLIPSE('',#51887,86.0962585581532,42.3);
#1463=ELLIPSE('',#51888,135.078923826262,42.3);
#1464=ELLIPSE('',#51889,135.078923826262,42.3);
#1465=ELLIPSE('',#51890,86.0962585581534,42.3);
#1466=ELLIPSE('',#51891,148.655022233233,42.3);
#1467=ELLIPSE('',#51892,684.784865862974,42.3);
#1468=ELLIPSE('',#51893,42.7157063175375,42.3);
#1469=ELLIPSE('',#51910,42.7157063175375,42.3);
#1470=ELLIPSE('',#51912,684.784865862975,42.3);
#1471=ELLIPSE('',#51914,148.655022233233,42.3);
#1472=ELLIPSE('',#51916,86.0962585581532,42.3);
#1473=ELLIPSE('',#51918,135.078923826262,42.3);
#1474=ELLIPSE('',#51921,135.078923826262,42.3);
#1475=ELLIPSE('',#51923,86.0962585581534,42.3);
#1476=ELLIPSE('',#51925,148.655022233233,42.3);
#1477=ELLIPSE('',#51927,684.784865862974,42.3);
#1478=ELLIPSE('',#51929,42.7157063175375,42.3);
#1479=ELLIPSE('',#51934,65.1465238200804,42.3);
#1480=ELLIPSE('',#51935,42.7157063175375,42.3);
#1481=ELLIPSE('',#51936,684.784865862975,42.3);
#1482=ELLIPSE('',#51937,148.655022233233,42.3);
#1483=ELLIPSE('',#51938,86.0962585581532,42.3);
#1484=ELLIPSE('',#51939,135.078923826262,42.3);
#1485=ELLIPSE('',#51940,135.078923826262,42.3);
#1486=ELLIPSE('',#51941,86.0962585581534,42.3);
#1487=ELLIPSE('',#51942,148.655022233233,42.3);
#1488=ELLIPSE('',#51943,684.784865862974,42.3);
#1489=ELLIPSE('',#51944,42.7157063175375,42.3);
#1490=ELLIPSE('',#51961,42.7157063175375,42.3);
#1491=ELLIPSE('',#51963,684.784865862975,42.3);
#1492=ELLIPSE('',#51965,148.655022233233,42.3);
#1493=ELLIPSE('',#51967,86.0962585581532,42.3);
#1494=ELLIPSE('',#51969,135.078923826262,42.3);
#1495=ELLIPSE('',#51972,135.078923826262,42.3);
#1496=ELLIPSE('',#51974,86.0962585581534,42.3);
#1497=ELLIPSE('',#51976,148.655022233233,42.3);
#1498=ELLIPSE('',#51978,684.784865862974,42.3);
#1499=ELLIPSE('',#51980,42.7157063175375,42.3);
#1500=ELLIPSE('',#51985,65.1465238200804,42.3);
#1501=ELLIPSE('',#51986,42.7157063175375,42.3);
#1502=ELLIPSE('',#51987,684.784865862975,42.3);
#1503=ELLIPSE('',#51988,148.655022233233,42.3);
#1504=ELLIPSE('',#51989,86.0962585581532,42.3);
#1505=ELLIPSE('',#51990,135.078923826262,42.3);
#1506=ELLIPSE('',#51991,135.078923826262,42.3);
#1507=ELLIPSE('',#51992,86.0962585581534,42.3);
#1508=ELLIPSE('',#51993,148.655022233233,42.3);
#1509=ELLIPSE('',#51994,684.784865862974,42.3);
#1510=ELLIPSE('',#51995,42.7157063175375,42.3);
#1511=ELLIPSE('',#52012,42.7157063175375,42.3);
#1512=ELLIPSE('',#52014,684.784865862975,42.3);
#1513=ELLIPSE('',#52016,148.655022233233,42.3);
#1514=ELLIPSE('',#52018,86.0962585581532,42.3);
#1515=ELLIPSE('',#52020,135.078923826262,42.3);
#1516=ELLIPSE('',#52023,135.078923826262,42.3);
#1517=ELLIPSE('',#52025,86.0962585581534,42.3);
#1518=ELLIPSE('',#52027,148.655022233233,42.3);
#1519=ELLIPSE('',#52029,684.784865862974,42.3);
#1520=ELLIPSE('',#52031,42.7157063175375,42.3);
#1521=ELLIPSE('',#52036,65.1465238200804,42.3);
#1522=ELLIPSE('',#52037,42.7157063175375,42.3);
#1523=ELLIPSE('',#52038,684.784865862975,42.3);
#1524=ELLIPSE('',#52039,148.655022233233,42.3);
#1525=ELLIPSE('',#52040,86.0962585581532,42.3);
#1526=ELLIPSE('',#52041,135.078923826262,42.3);
#1527=ELLIPSE('',#52042,135.078923826262,42.3);
#1528=ELLIPSE('',#52043,86.0962585581534,42.3);
#1529=ELLIPSE('',#52044,148.655022233233,42.3);
#1530=ELLIPSE('',#52045,684.784865862974,42.3);
#1531=ELLIPSE('',#52046,42.7157063175375,42.3);
#1532=ELLIPSE('',#52063,42.7157063175375,42.3);
#1533=ELLIPSE('',#52065,684.784865862975,42.3);
#1534=ELLIPSE('',#52067,148.655022233233,42.3);
#1535=ELLIPSE('',#52069,86.0962585581532,42.3);
#1536=ELLIPSE('',#52071,135.078923826262,42.3);
#1537=ELLIPSE('',#52074,135.078923826262,42.3);
#1538=ELLIPSE('',#52076,86.0962585581534,42.3);
#1539=ELLIPSE('',#52078,148.655022233233,42.3);
#1540=ELLIPSE('',#52080,684.784865862974,42.3);
#1541=ELLIPSE('',#52082,42.7157063175375,42.3);
#1542=ELLIPSE('',#52087,65.1465238200804,42.3);
#1543=ELLIPSE('',#52088,42.7157063175375,42.3);
#1544=ELLIPSE('',#52089,684.784865862975,42.3);
#1545=ELLIPSE('',#52090,148.655022233233,42.3);
#1546=ELLIPSE('',#52091,86.0962585581532,42.3);
#1547=ELLIPSE('',#52092,135.078923826262,42.3);
#1548=ELLIPSE('',#52093,135.078923826262,42.3);
#1549=ELLIPSE('',#52094,86.0962585581534,42.3);
#1550=ELLIPSE('',#52095,148.655022233233,42.3);
#1551=ELLIPSE('',#52096,684.784865862974,42.3);
#1552=ELLIPSE('',#52097,42.7157063175375,42.3);
#1553=ELLIPSE('',#52114,42.7157063175375,42.3);
#1554=ELLIPSE('',#52116,684.784865862975,42.3);
#1555=ELLIPSE('',#52118,148.655022233233,42.3);
#1556=ELLIPSE('',#52120,86.0962585581532,42.3);
#1557=ELLIPSE('',#52122,135.078923826262,42.3);
#1558=ELLIPSE('',#52125,135.078923826262,42.3);
#1559=ELLIPSE('',#52127,86.0962585581534,42.3);
#1560=ELLIPSE('',#52129,148.655022233233,42.3);
#1561=ELLIPSE('',#52131,684.784865862974,42.3);
#1562=ELLIPSE('',#52133,42.7157063175375,42.3);
#1563=ELLIPSE('',#52138,65.1465238200804,42.3);
#1564=ELLIPSE('',#52139,42.7157063175375,42.3);
#1565=ELLIPSE('',#52140,684.784865862975,42.3);
#1566=ELLIPSE('',#52141,148.655022233233,42.3);
#1567=ELLIPSE('',#52142,86.0962585581532,42.3);
#1568=ELLIPSE('',#52143,135.078923826262,42.3);
#1569=ELLIPSE('',#52144,135.078923826262,42.3);
#1570=ELLIPSE('',#52145,86.0962585581534,42.3);
#1571=ELLIPSE('',#52146,148.655022233233,42.3);
#1572=ELLIPSE('',#52147,684.784865862974,42.3);
#1573=ELLIPSE('',#52148,42.7157063175375,42.3);
#1574=ELLIPSE('',#52165,42.7157063175375,42.3);
#1575=ELLIPSE('',#52167,684.784865862975,42.3);
#1576=ELLIPSE('',#52169,148.655022233233,42.3);
#1577=ELLIPSE('',#52171,86.0962585581532,42.3);
#1578=ELLIPSE('',#52173,135.078923826262,42.3);
#1579=ELLIPSE('',#52176,135.078923826262,42.3);
#1580=ELLIPSE('',#52178,86.0962585581534,42.3);
#1581=ELLIPSE('',#52180,148.655022233233,42.3);
#1582=ELLIPSE('',#52182,684.784865862974,42.3);
#1583=ELLIPSE('',#52184,42.7157063175375,42.3);
#1584=ELLIPSE('',#52189,65.1465238200804,42.3);
#1585=ELLIPSE('',#52190,42.7157063175375,42.3);
#1586=ELLIPSE('',#52191,684.784865862975,42.3);
#1587=ELLIPSE('',#52192,148.655022233233,42.3);
#1588=ELLIPSE('',#52193,86.0962585581532,42.3);
#1589=ELLIPSE('',#52194,135.078923826262,42.3);
#1590=ELLIPSE('',#52195,135.078923826262,42.3);
#1591=ELLIPSE('',#52196,86.0962585581534,42.3);
#1592=ELLIPSE('',#52197,148.655022233233,42.3);
#1593=ELLIPSE('',#52198,684.784865862974,42.3);
#1594=ELLIPSE('',#52199,42.7157063175375,42.3);
#1595=ELLIPSE('',#52216,42.7157063175375,42.3);
#1596=ELLIPSE('',#52218,684.784865862975,42.3);
#1597=ELLIPSE('',#52220,148.655022233233,42.3);
#1598=ELLIPSE('',#52222,86.0962585581532,42.3);
#1599=ELLIPSE('',#52224,135.078923826262,42.3);
#1600=ELLIPSE('',#52227,135.078923826262,42.3);
#1601=ELLIPSE('',#52229,86.0962585581534,42.3);
#1602=ELLIPSE('',#52231,148.655022233233,42.3);
#1603=ELLIPSE('',#52233,684.784865862974,42.3);
#1604=ELLIPSE('',#52235,42.7157063175375,42.3);
#1605=ELLIPSE('',#52240,65.1465238200804,42.3);
#1606=ELLIPSE('',#52241,42.7157063175375,42.3);
#1607=ELLIPSE('',#52242,684.784865862975,42.3);
#1608=ELLIPSE('',#52243,148.655022233233,42.3);
#1609=ELLIPSE('',#52244,86.0962585581532,42.3);
#1610=ELLIPSE('',#52245,135.078923826262,42.3);
#1611=ELLIPSE('',#52246,135.078923826262,42.3);
#1612=ELLIPSE('',#52247,86.0962585581534,42.3);
#1613=ELLIPSE('',#52248,148.655022233233,42.3);
#1614=ELLIPSE('',#52249,684.784865862974,42.3);
#1615=ELLIPSE('',#52250,42.7157063175375,42.3);
#1616=ELLIPSE('',#52267,42.7157063175375,42.3);
#1617=ELLIPSE('',#52269,684.784865862975,42.3);
#1618=ELLIPSE('',#52271,148.655022233233,42.3);
#1619=ELLIPSE('',#52273,86.0962585581532,42.3);
#1620=ELLIPSE('',#52275,135.078923826262,42.3);
#1621=ELLIPSE('',#52278,135.078923826262,42.3);
#1622=ELLIPSE('',#52280,86.0962585581534,42.3);
#1623=ELLIPSE('',#52282,148.655022233233,42.3);
#1624=ELLIPSE('',#52284,684.784865862974,42.3);
#1625=ELLIPSE('',#52286,42.7157063175375,42.3);
#1626=ELLIPSE('',#52291,65.1465238200804,42.3);
#1627=ELLIPSE('',#52292,42.7157063175375,42.3);
#1628=ELLIPSE('',#52293,684.784865862975,42.3);
#1629=ELLIPSE('',#52294,148.655022233233,42.3);
#1630=ELLIPSE('',#52295,86.0962585581532,42.3);
#1631=ELLIPSE('',#52296,135.078923826262,42.3);
#1632=ELLIPSE('',#52297,135.078923826262,42.3);
#1633=ELLIPSE('',#52298,86.0962585581534,42.3);
#1634=ELLIPSE('',#52299,148.655022233233,42.3);
#1635=ELLIPSE('',#52300,684.784865862974,42.3);
#1636=ELLIPSE('',#52301,42.7157063175375,42.3);
#1637=ELLIPSE('',#52318,42.7157063175375,42.3);
#1638=ELLIPSE('',#52320,684.784865862975,42.3);
#1639=ELLIPSE('',#52322,148.655022233233,42.3);
#1640=ELLIPSE('',#52324,86.0962585581532,42.3);
#1641=ELLIPSE('',#52326,135.078923826262,42.3);
#1642=ELLIPSE('',#52329,135.078923826262,42.3);
#1643=ELLIPSE('',#52331,86.0962585581534,42.3);
#1644=ELLIPSE('',#52333,148.655022233233,42.3);
#1645=ELLIPSE('',#52335,684.784865862974,42.3);
#1646=ELLIPSE('',#52337,42.7157063175375,42.3);
#1647=ELLIPSE('',#52342,65.1465238200804,42.3);
#1648=ELLIPSE('',#52343,42.7157063175375,42.3);
#1649=ELLIPSE('',#52344,684.784865862975,42.3);
#1650=ELLIPSE('',#52345,148.655022233233,42.3);
#1651=ELLIPSE('',#52346,86.0962585581532,42.3);
#1652=ELLIPSE('',#52347,135.078923826262,42.3);
#1653=ELLIPSE('',#52348,135.078923826262,42.3);
#1654=ELLIPSE('',#52349,86.0962585581534,42.3);
#1655=ELLIPSE('',#52350,148.655022233233,42.3);
#1656=ELLIPSE('',#52351,684.784865862974,42.3);
#1657=ELLIPSE('',#52352,42.7157063175375,42.3);
#1658=ELLIPSE('',#52369,42.7157063175375,42.3);
#1659=ELLIPSE('',#52371,684.784865862975,42.3);
#1660=ELLIPSE('',#52373,148.655022233233,42.3);
#1661=ELLIPSE('',#52375,86.0962585581532,42.3);
#1662=ELLIPSE('',#52377,135.078923826262,42.3);
#1663=ELLIPSE('',#52380,135.078923826262,42.3);
#1664=ELLIPSE('',#52382,86.0962585581534,42.3);
#1665=ELLIPSE('',#52384,148.655022233233,42.3);
#1666=ELLIPSE('',#52386,684.784865862974,42.3);
#1667=ELLIPSE('',#52388,42.7157063175375,42.3);
#1668=ELLIPSE('',#52393,65.1465238200804,42.3);
#1669=ELLIPSE('',#52394,42.7157063175375,42.3);
#1670=ELLIPSE('',#52395,684.784865862975,42.3);
#1671=ELLIPSE('',#52396,148.655022233233,42.3);
#1672=ELLIPSE('',#52397,86.0962585581532,42.3);
#1673=ELLIPSE('',#52398,135.078923826262,42.3);
#1674=ELLIPSE('',#52399,135.078923826262,42.3);
#1675=ELLIPSE('',#52400,86.0962585581534,42.3);
#1676=ELLIPSE('',#52401,148.655022233233,42.3);
#1677=ELLIPSE('',#52402,684.784865862974,42.3);
#1678=ELLIPSE('',#52403,42.7157063175375,42.3);
#1679=ELLIPSE('',#52420,42.7157063175375,42.3);
#1680=ELLIPSE('',#52422,684.784865862975,42.3);
#1681=ELLIPSE('',#52424,148.655022233233,42.3);
#1682=ELLIPSE('',#52426,86.0962585581532,42.3);
#1683=ELLIPSE('',#52428,135.078923826262,42.3);
#1684=ELLIPSE('',#52431,135.078923826262,42.3);
#1685=ELLIPSE('',#52433,86.0962585581534,42.3);
#1686=ELLIPSE('',#52435,148.655022233233,42.3);
#1687=ELLIPSE('',#52437,684.784865862974,42.3);
#1688=ELLIPSE('',#52439,42.7157063175375,42.3);
#1689=ELLIPSE('',#52444,65.1465238200804,42.3);
#1690=ELLIPSE('',#52445,42.7157063175375,42.3);
#1691=ELLIPSE('',#52446,684.784865862975,42.3);
#1692=ELLIPSE('',#52447,148.655022233233,42.3);
#1693=ELLIPSE('',#52448,86.0962585581532,42.3);
#1694=ELLIPSE('',#52449,135.078923826262,42.3);
#1695=ELLIPSE('',#52450,135.078923826262,42.3);
#1696=ELLIPSE('',#52451,86.0962585581534,42.3);
#1697=ELLIPSE('',#52452,148.655022233233,42.3);
#1698=ELLIPSE('',#52453,684.784865862974,42.3);
#1699=ELLIPSE('',#52454,42.7157063175375,42.3);
#1700=ELLIPSE('',#52471,42.7157063175375,42.3);
#1701=ELLIPSE('',#52473,684.784865862975,42.3);
#1702=ELLIPSE('',#52475,148.655022233233,42.3);
#1703=ELLIPSE('',#52477,86.0962585581532,42.3);
#1704=ELLIPSE('',#52479,135.078923826262,42.3);
#1705=ELLIPSE('',#52482,135.078923826262,42.3);
#1706=ELLIPSE('',#52484,86.0962585581534,42.3);
#1707=ELLIPSE('',#52486,148.655022233233,42.3);
#1708=ELLIPSE('',#52488,684.784865862974,42.3);
#1709=ELLIPSE('',#52490,42.7157063175375,42.3);
#1710=ELLIPSE('',#52495,65.1465238200804,42.3);
#1711=ELLIPSE('',#52496,42.7157063175375,42.3);
#1712=ELLIPSE('',#52497,684.784865862975,42.3);
#1713=ELLIPSE('',#52498,148.655022233233,42.3);
#1714=ELLIPSE('',#52499,86.0962585581532,42.3);
#1715=ELLIPSE('',#52500,135.078923826262,42.3);
#1716=ELLIPSE('',#52501,135.078923826262,42.3);
#1717=ELLIPSE('',#52502,86.0962585581534,42.3);
#1718=ELLIPSE('',#52503,148.655022233233,42.3);
#1719=ELLIPSE('',#52504,684.784865862974,42.3);
#1720=ELLIPSE('',#52505,42.7157063175375,42.3);
#1721=ELLIPSE('',#52522,42.7157063175375,42.3);
#1722=ELLIPSE('',#52524,684.784865862975,42.3);
#1723=ELLIPSE('',#52526,148.655022233233,42.3);
#1724=ELLIPSE('',#52528,86.0962585581532,42.3);
#1725=ELLIPSE('',#52530,135.078923826262,42.3);
#1726=ELLIPSE('',#52533,135.078923826262,42.3);
#1727=ELLIPSE('',#52535,86.0962585581534,42.3);
#1728=ELLIPSE('',#52537,148.655022233233,42.3);
#1729=ELLIPSE('',#52539,684.784865862974,42.3);
#1730=ELLIPSE('',#52541,42.7157063175375,42.3);
#1731=ELLIPSE('',#52546,65.1465238200804,42.3);
#1732=ELLIPSE('',#52547,42.7157063175375,42.3);
#1733=ELLIPSE('',#52548,684.784865862975,42.3);
#1734=ELLIPSE('',#52549,148.655022233233,42.3);
#1735=ELLIPSE('',#52550,86.0962585581532,42.3);
#1736=ELLIPSE('',#52551,135.078923826262,42.3);
#1737=ELLIPSE('',#52552,135.078923826262,42.3);
#1738=ELLIPSE('',#52553,86.0962585581534,42.3);
#1739=ELLIPSE('',#52554,148.655022233233,42.3);
#1740=ELLIPSE('',#52555,684.784865862974,42.3);
#1741=ELLIPSE('',#52556,42.7157063175375,42.3);
#1742=ELLIPSE('',#52573,42.7157063175375,42.3);
#1743=ELLIPSE('',#52575,684.784865862975,42.3);
#1744=ELLIPSE('',#52577,148.655022233233,42.3);
#1745=ELLIPSE('',#52579,86.0962585581532,42.3);
#1746=ELLIPSE('',#52581,135.078923826262,42.3);
#1747=ELLIPSE('',#52584,135.078923826262,42.3);
#1748=ELLIPSE('',#52586,86.0962585581534,42.3);
#1749=ELLIPSE('',#52588,148.655022233233,42.3);
#1750=ELLIPSE('',#52590,684.784865862974,42.3);
#1751=ELLIPSE('',#52592,42.7157063175375,42.3);
#1752=ELLIPSE('',#52597,65.1465238200804,42.3);
#1753=ELLIPSE('',#52598,42.7157063175375,42.3);
#1754=ELLIPSE('',#52599,684.784865862975,42.3);
#1755=ELLIPSE('',#52600,148.655022233233,42.3);
#1756=ELLIPSE('',#52601,86.0962585581532,42.3);
#1757=ELLIPSE('',#52602,135.078923826262,42.3);
#1758=ELLIPSE('',#52603,135.078923826262,42.3);
#1759=ELLIPSE('',#52604,86.0962585581534,42.3);
#1760=ELLIPSE('',#52605,148.655022233233,42.3);
#1761=ELLIPSE('',#52606,684.784865862974,42.3);
#1762=ELLIPSE('',#52607,42.7157063175375,42.3);
#1763=ELLIPSE('',#52624,42.7157063175375,42.3);
#1764=ELLIPSE('',#52626,684.784865862975,42.3);
#1765=ELLIPSE('',#52628,148.655022233233,42.3);
#1766=ELLIPSE('',#52630,86.0962585581532,42.3);
#1767=ELLIPSE('',#52632,135.078923826262,42.3);
#1768=ELLIPSE('',#52635,135.078923826262,42.3);
#1769=ELLIPSE('',#52637,86.0962585581534,42.3);
#1770=ELLIPSE('',#52639,148.655022233233,42.3);
#1771=ELLIPSE('',#52641,684.784865862974,42.3);
#1772=ELLIPSE('',#52643,42.7157063175375,42.3);
#1773=ELLIPSE('',#52648,65.1465238200804,42.3);
#1774=ELLIPSE('',#52649,42.7157063175375,42.3);
#1775=ELLIPSE('',#52650,684.784865862975,42.3);
#1776=ELLIPSE('',#52651,148.655022233233,42.3);
#1777=ELLIPSE('',#52652,86.0962585581532,42.3);
#1778=ELLIPSE('',#52653,135.078923826262,42.3);
#1779=ELLIPSE('',#52654,135.078923826262,42.3);
#1780=ELLIPSE('',#52655,86.0962585581534,42.3);
#1781=ELLIPSE('',#52656,148.655022233233,42.3);
#1782=ELLIPSE('',#52657,684.784865862974,42.3);
#1783=ELLIPSE('',#52658,42.7157063175375,42.3);
#1784=ELLIPSE('',#52675,42.7157063175375,42.3);
#1785=ELLIPSE('',#52677,684.784865862975,42.3);
#1786=ELLIPSE('',#52679,148.655022233233,42.3);
#1787=ELLIPSE('',#52681,86.0962585581532,42.3);
#1788=ELLIPSE('',#52683,135.078923826262,42.3);
#1789=ELLIPSE('',#52686,135.078923826262,42.3);
#1790=ELLIPSE('',#52688,86.0962585581534,42.3);
#1791=ELLIPSE('',#52690,148.655022233233,42.3);
#1792=ELLIPSE('',#52692,684.784865862974,42.3);
#1793=ELLIPSE('',#52694,42.7157063175375,42.3);
#1794=ELLIPSE('',#52699,65.1465238200804,42.3);
#1795=ELLIPSE('',#52700,42.7157063175375,42.3);
#1796=ELLIPSE('',#52701,684.784865862975,42.3);
#1797=ELLIPSE('',#52702,148.655022233233,42.3);
#1798=ELLIPSE('',#52703,86.0962585581532,42.3);
#1799=ELLIPSE('',#52704,135.078923826262,42.3);
#1800=ELLIPSE('',#52705,135.078923826262,42.3);
#1801=ELLIPSE('',#52706,86.0962585581534,42.3);
#1802=ELLIPSE('',#52707,148.655022233233,42.3);
#1803=ELLIPSE('',#52708,684.784865862974,42.3);
#1804=ELLIPSE('',#52709,42.7157063175375,42.3);
#1805=ELLIPSE('',#52726,42.7157063175375,42.3);
#1806=ELLIPSE('',#52728,684.784865862975,42.3);
#1807=ELLIPSE('',#52730,148.655022233233,42.3);
#1808=ELLIPSE('',#52732,86.0962585581532,42.3);
#1809=ELLIPSE('',#52734,135.078923826262,42.3);
#1810=ELLIPSE('',#52737,135.078923826262,42.3);
#1811=ELLIPSE('',#52739,86.0962585581534,42.3);
#1812=ELLIPSE('',#52741,148.655022233233,42.3);
#1813=ELLIPSE('',#52743,684.784865862974,42.3);
#1814=ELLIPSE('',#52745,42.7157063175375,42.3);
#1815=ELLIPSE('',#52750,65.1465238200804,42.3);
#1816=ELLIPSE('',#52751,42.7157063175375,42.3);
#1817=ELLIPSE('',#52752,684.784865862975,42.3);
#1818=ELLIPSE('',#52753,148.655022233233,42.3);
#1819=ELLIPSE('',#52754,86.0962585581532,42.3);
#1820=ELLIPSE('',#52755,135.078923826262,42.3);
#1821=ELLIPSE('',#52756,135.078923826262,42.3);
#1822=ELLIPSE('',#52757,86.0962585581534,42.3);
#1823=ELLIPSE('',#52758,148.655022233233,42.3);
#1824=ELLIPSE('',#52759,684.784865862974,42.3);
#1825=ELLIPSE('',#52760,42.7157063175375,42.3);
#1826=ELLIPSE('',#52777,42.7157063175375,42.3);
#1827=ELLIPSE('',#52779,684.784865862975,42.3);
#1828=ELLIPSE('',#52781,148.655022233233,42.3);
#1829=ELLIPSE('',#52783,86.0962585581532,42.3);
#1830=ELLIPSE('',#52785,135.078923826262,42.3);
#1831=ELLIPSE('',#52788,135.078923826262,42.3);
#1832=ELLIPSE('',#52790,86.0962585581534,42.3);
#1833=ELLIPSE('',#52792,148.655022233233,42.3);
#1834=ELLIPSE('',#52794,684.784865862974,42.3);
#1835=ELLIPSE('',#52796,42.7157063175375,42.3);
#1836=ELLIPSE('',#52801,65.1465238200804,42.3);
#1837=ELLIPSE('',#52802,42.7157063175375,42.3);
#1838=ELLIPSE('',#52803,684.784865862975,42.3);
#1839=ELLIPSE('',#52804,148.655022233233,42.3);
#1840=ELLIPSE('',#52805,86.0962585581532,42.3);
#1841=ELLIPSE('',#52806,135.078923826262,42.3);
#1842=ELLIPSE('',#52807,135.078923826262,42.3);
#1843=ELLIPSE('',#52808,86.0962585581534,42.3);
#1844=ELLIPSE('',#52809,148.655022233233,42.3);
#1845=ELLIPSE('',#52810,684.784865862974,42.3);
#1846=ELLIPSE('',#52811,42.7157063175375,42.3);
#1847=ELLIPSE('',#52828,42.7157063175375,42.3);
#1848=ELLIPSE('',#52830,684.784865862975,42.3);
#1849=ELLIPSE('',#52832,148.655022233233,42.3);
#1850=ELLIPSE('',#52834,86.0962585581532,42.3);
#1851=ELLIPSE('',#52836,135.078923826262,42.3);
#1852=ELLIPSE('',#52839,135.078923826262,42.3);
#1853=ELLIPSE('',#52841,86.0962585581534,42.3);
#1854=ELLIPSE('',#52843,148.655022233233,42.3);
#1855=ELLIPSE('',#52845,684.784865862974,42.3);
#1856=ELLIPSE('',#52847,42.7157063175375,42.3);
#1857=ELLIPSE('',#52852,65.1465238200804,42.3);
#1858=ELLIPSE('',#52853,42.7157063175375,42.3);
#1859=ELLIPSE('',#52854,684.784865862975,42.3);
#1860=ELLIPSE('',#52855,148.655022233233,42.3);
#1861=ELLIPSE('',#52856,86.0962585581532,42.3);
#1862=ELLIPSE('',#52857,135.078923826262,42.3);
#1863=ELLIPSE('',#52858,135.078923826262,42.3);
#1864=ELLIPSE('',#52859,86.0962585581534,42.3);
#1865=ELLIPSE('',#52860,148.655022233233,42.3);
#1866=ELLIPSE('',#52861,684.784865862974,42.3);
#1867=ELLIPSE('',#52862,42.7157063175375,42.3);
#1868=ELLIPSE('',#52879,42.7157063175375,42.3);
#1869=ELLIPSE('',#52881,684.784865862975,42.3);
#1870=ELLIPSE('',#52883,148.655022233233,42.3);
#1871=ELLIPSE('',#52885,86.0962585581532,42.3);
#1872=ELLIPSE('',#52887,135.078923826262,42.3);
#1873=ELLIPSE('',#52890,135.078923826262,42.3);
#1874=ELLIPSE('',#52892,86.0962585581534,42.3);
#1875=ELLIPSE('',#52894,148.655022233233,42.3);
#1876=ELLIPSE('',#52896,684.784865862974,42.3);
#1877=ELLIPSE('',#52898,42.7157063175375,42.3);
#1878=ELLIPSE('',#52903,65.1465238200804,42.3);
#1879=ELLIPSE('',#52904,42.7157063175375,42.3);
#1880=ELLIPSE('',#52905,684.784865862975,42.3);
#1881=ELLIPSE('',#52906,148.655022233233,42.3);
#1882=ELLIPSE('',#52907,86.0962585581532,42.3);
#1883=ELLIPSE('',#52908,135.078923826262,42.3);
#1884=ELLIPSE('',#52909,135.078923826262,42.3);
#1885=ELLIPSE('',#52910,86.0962585581534,42.3);
#1886=ELLIPSE('',#52911,148.655022233233,42.3);
#1887=ELLIPSE('',#52912,684.784865862974,42.3);
#1888=ELLIPSE('',#52913,42.7157063175375,42.3);
#1889=ELLIPSE('',#52930,42.7157063175375,42.3);
#1890=ELLIPSE('',#52932,684.784865862975,42.3);
#1891=ELLIPSE('',#52934,148.655022233233,42.3);
#1892=ELLIPSE('',#52936,86.0962585581532,42.3);
#1893=ELLIPSE('',#52938,135.078923826262,42.3);
#1894=ELLIPSE('',#52941,135.078923826262,42.3);
#1895=ELLIPSE('',#52943,86.0962585581534,42.3);
#1896=ELLIPSE('',#52945,148.655022233233,42.3);
#1897=ELLIPSE('',#52947,684.784865862974,42.3);
#1898=ELLIPSE('',#52949,42.7157063175375,42.3);
#1899=ELLIPSE('',#52954,65.1465238200804,42.3);
#1900=ELLIPSE('',#52955,42.7157063175375,42.3);
#1901=ELLIPSE('',#52956,684.784865862975,42.3);
#1902=ELLIPSE('',#52957,148.655022233233,42.3);
#1903=ELLIPSE('',#52958,86.0962585581532,42.3);
#1904=ELLIPSE('',#52959,135.078923826262,42.3);
#1905=ELLIPSE('',#52960,135.078923826262,42.3);
#1906=ELLIPSE('',#52961,86.0962585581534,42.3);
#1907=ELLIPSE('',#52962,148.655022233233,42.3);
#1908=ELLIPSE('',#52963,684.784865862974,42.3);
#1909=ELLIPSE('',#52964,42.7157063175375,42.3);
#1910=ELLIPSE('',#52981,42.7157063175375,42.3);
#1911=ELLIPSE('',#52983,684.784865862975,42.3);
#1912=ELLIPSE('',#52985,148.655022233233,42.3);
#1913=ELLIPSE('',#52987,86.0962585581532,42.3);
#1914=ELLIPSE('',#52989,135.078923826262,42.3);
#1915=ELLIPSE('',#52992,135.078923826262,42.3);
#1916=ELLIPSE('',#52994,86.0962585581534,42.3);
#1917=ELLIPSE('',#52996,148.655022233233,42.3);
#1918=ELLIPSE('',#52998,684.784865862974,42.3);
#1919=ELLIPSE('',#53000,42.7157063175375,42.3);
#1920=ELLIPSE('',#53005,65.1465238200804,42.3);
#1921=ELLIPSE('',#53006,42.7157063175375,42.3);
#1922=ELLIPSE('',#53007,684.784865862975,42.3);
#1923=ELLIPSE('',#53008,148.655022233233,42.3);
#1924=ELLIPSE('',#53009,86.0962585581532,42.3);
#1925=ELLIPSE('',#53010,135.078923826262,42.3);
#1926=ELLIPSE('',#53011,135.078923826262,42.3);
#1927=ELLIPSE('',#53012,86.0962585581534,42.3);
#1928=ELLIPSE('',#53013,148.655022233233,42.3);
#1929=ELLIPSE('',#53014,684.784865862974,42.3);
#1930=ELLIPSE('',#53015,42.7157063175375,42.3);
#1931=ELLIPSE('',#53032,42.7157063175375,42.3);
#1932=ELLIPSE('',#53034,684.784865862975,42.3);
#1933=ELLIPSE('',#53036,148.655022233233,42.3);
#1934=ELLIPSE('',#53038,86.0962585581532,42.3);
#1935=ELLIPSE('',#53040,135.078923826262,42.3);
#1936=ELLIPSE('',#53043,135.078923826262,42.3);
#1937=ELLIPSE('',#53045,86.0962585581534,42.3);
#1938=ELLIPSE('',#53047,148.655022233233,42.3);
#1939=ELLIPSE('',#53049,684.784865862974,42.3);
#1940=ELLIPSE('',#53051,42.7157063175375,42.3);
#1941=ELLIPSE('',#53056,65.1465238200804,42.3);
#1942=ELLIPSE('',#53057,42.7157063175375,42.3);
#1943=ELLIPSE('',#53058,684.784865862975,42.3);
#1944=ELLIPSE('',#53059,148.655022233233,42.3);
#1945=ELLIPSE('',#53060,86.0962585581532,42.3);
#1946=ELLIPSE('',#53061,135.078923826262,42.3);
#1947=ELLIPSE('',#53062,135.078923826262,42.3);
#1948=ELLIPSE('',#53063,86.0962585581534,42.3);
#1949=ELLIPSE('',#53064,148.655022233233,42.3);
#1950=ELLIPSE('',#53065,684.784865862974,42.3);
#1951=ELLIPSE('',#53066,42.7157063175375,42.3);
#1952=ELLIPSE('',#53083,42.7157063175375,42.3);
#1953=ELLIPSE('',#53085,684.784865862975,42.3);
#1954=ELLIPSE('',#53087,148.655022233233,42.3);
#1955=ELLIPSE('',#53089,86.0962585581532,42.3);
#1956=ELLIPSE('',#53091,135.078923826262,42.3);
#1957=ELLIPSE('',#53094,135.078923826262,42.3);
#1958=ELLIPSE('',#53096,86.0962585581534,42.3);
#1959=ELLIPSE('',#53098,148.655022233233,42.3);
#1960=ELLIPSE('',#53100,684.784865862974,42.3);
#1961=ELLIPSE('',#53102,42.7157063175375,42.3);
#1962=ELLIPSE('',#53107,65.1465238200804,42.3);
#1963=ELLIPSE('',#53108,42.7157063175375,42.3);
#1964=ELLIPSE('',#53109,684.784865862975,42.3);
#1965=ELLIPSE('',#53110,148.655022233233,42.3);
#1966=ELLIPSE('',#53111,86.0962585581532,42.3);
#1967=ELLIPSE('',#53112,135.078923826262,42.3);
#1968=ELLIPSE('',#53113,135.078923826262,42.3);
#1969=ELLIPSE('',#53114,86.0962585581534,42.3);
#1970=ELLIPSE('',#53115,148.655022233233,42.3);
#1971=ELLIPSE('',#53116,684.784865862974,42.3);
#1972=ELLIPSE('',#53117,42.7157063175375,42.3);
#1973=ELLIPSE('',#53134,42.7157063175375,42.3);
#1974=ELLIPSE('',#53136,684.784865862975,42.3);
#1975=ELLIPSE('',#53138,148.655022233233,42.3);
#1976=ELLIPSE('',#53140,86.0962585581532,42.3);
#1977=ELLIPSE('',#53142,135.078923826262,42.3);
#1978=ELLIPSE('',#53145,135.078923826262,42.3);
#1979=ELLIPSE('',#53147,86.0962585581534,42.3);
#1980=ELLIPSE('',#53149,148.655022233233,42.3);
#1981=ELLIPSE('',#53151,684.784865862974,42.3);
#1982=ELLIPSE('',#53153,42.7157063175375,42.3);
#1983=ELLIPSE('',#53158,65.1465238200804,42.3);
#1984=ELLIPSE('',#53159,42.7157063175375,42.3);
#1985=ELLIPSE('',#53160,684.784865862975,42.3);
#1986=ELLIPSE('',#53161,148.655022233233,42.3);
#1987=ELLIPSE('',#53162,86.0962585581532,42.3);
#1988=ELLIPSE('',#53163,135.078923826262,42.3);
#1989=ELLIPSE('',#53164,135.078923826262,42.3);
#1990=ELLIPSE('',#53165,86.0962585581534,42.3);
#1991=ELLIPSE('',#53166,148.655022233233,42.3);
#1992=ELLIPSE('',#53167,684.784865862974,42.3);
#1993=ELLIPSE('',#53168,42.7157063175375,42.3);
#1994=ELLIPSE('',#53185,42.7157063175375,42.3);
#1995=ELLIPSE('',#53187,684.784865862975,42.3);
#1996=ELLIPSE('',#53189,148.655022233233,42.3);
#1997=ELLIPSE('',#53191,86.0962585581532,42.3);
#1998=ELLIPSE('',#53193,135.078923826262,42.3);
#1999=ELLIPSE('',#53196,135.078923826262,42.3);
#2000=ELLIPSE('',#53198,86.0962585581534,42.3);
#2001=ELLIPSE('',#53200,148.655022233233,42.3);
#2002=ELLIPSE('',#53202,684.784865862974,42.3);
#2003=ELLIPSE('',#53204,42.7157063175375,42.3);
#2004=ELLIPSE('',#53209,65.1465238200804,42.3);
#2005=ELLIPSE('',#53210,42.7157063175375,42.3);
#2006=ELLIPSE('',#53211,684.784865862975,42.3);
#2007=ELLIPSE('',#53212,148.655022233233,42.3);
#2008=ELLIPSE('',#53213,86.0962585581532,42.3);
#2009=ELLIPSE('',#53214,135.078923826262,42.3);
#2010=ELLIPSE('',#53215,135.078923826262,42.3);
#2011=ELLIPSE('',#53216,86.0962585581534,42.3);
#2012=ELLIPSE('',#53217,148.655022233233,42.3);
#2013=ELLIPSE('',#53218,684.784865862974,42.3);
#2014=ELLIPSE('',#53219,42.7157063175375,42.3);
#2015=ELLIPSE('',#53236,42.7157063175375,42.3);
#2016=ELLIPSE('',#53238,684.784865862975,42.3);
#2017=ELLIPSE('',#53240,148.655022233233,42.3);
#2018=ELLIPSE('',#53242,86.0962585581532,42.3);
#2019=ELLIPSE('',#53244,135.078923826262,42.3);
#2020=ELLIPSE('',#53247,135.078923826262,42.3);
#2021=ELLIPSE('',#53249,86.0962585581534,42.3);
#2022=ELLIPSE('',#53251,148.655022233233,42.3);
#2023=ELLIPSE('',#53253,684.784865862974,42.3);
#2024=ELLIPSE('',#53255,42.7157063175375,42.3);
#2025=ELLIPSE('',#53260,65.1465238200804,42.3);
#2026=ELLIPSE('',#53261,42.7157063175375,42.3);
#2027=ELLIPSE('',#53262,684.784865862975,42.3);
#2028=ELLIPSE('',#53263,148.655022233233,42.3);
#2029=ELLIPSE('',#53264,86.0962585581532,42.3);
#2030=ELLIPSE('',#53265,135.078923826262,42.3);
#2031=ELLIPSE('',#53266,135.078923826262,42.3);
#2032=ELLIPSE('',#53267,86.0962585581534,42.3);
#2033=ELLIPSE('',#53268,148.655022233233,42.3);
#2034=ELLIPSE('',#53269,684.784865862974,42.3);
#2035=ELLIPSE('',#53270,42.7157063175375,42.3);
#2036=ELLIPSE('',#53287,42.7157063175375,42.3);
#2037=ELLIPSE('',#53289,684.784865862975,42.3);
#2038=ELLIPSE('',#53291,148.655022233233,42.3);
#2039=ELLIPSE('',#53293,86.0962585581532,42.3);
#2040=ELLIPSE('',#53295,135.078923826262,42.3);
#2041=ELLIPSE('',#53298,135.078923826262,42.3);
#2042=ELLIPSE('',#53300,86.0962585581534,42.3);
#2043=ELLIPSE('',#53302,148.655022233233,42.3);
#2044=ELLIPSE('',#53304,684.784865862974,42.3);
#2045=ELLIPSE('',#53306,42.7157063175375,42.3);
#2046=ELLIPSE('',#53311,65.1465238200804,42.3);
#2047=ELLIPSE('',#53312,42.7157063175375,42.3);
#2048=ELLIPSE('',#53313,684.784865862975,42.3);
#2049=ELLIPSE('',#53314,148.655022233233,42.3);
#2050=ELLIPSE('',#53315,86.0962585581532,42.3);
#2051=ELLIPSE('',#53316,135.078923826262,42.3);
#2052=ELLIPSE('',#53317,135.078923826262,42.3);
#2053=ELLIPSE('',#53318,86.0962585581534,42.3);
#2054=ELLIPSE('',#53319,148.655022233233,42.3);
#2055=ELLIPSE('',#53320,684.784865862974,42.3);
#2056=ELLIPSE('',#53321,42.7157063175375,42.3);
#2057=ELLIPSE('',#53338,42.7157063175375,42.3);
#2058=ELLIPSE('',#53340,684.784865862975,42.3);
#2059=ELLIPSE('',#53342,148.655022233233,42.3);
#2060=ELLIPSE('',#53344,86.0962585581532,42.3);
#2061=ELLIPSE('',#53346,135.078923826262,42.3);
#2062=ELLIPSE('',#53349,135.078923826262,42.3);
#2063=ELLIPSE('',#53351,86.0962585581534,42.3);
#2064=ELLIPSE('',#53353,148.655022233233,42.3);
#2065=ELLIPSE('',#53355,684.784865862974,42.3);
#2066=ELLIPSE('',#53357,42.7157063175375,42.3);
#2067=ELLIPSE('',#53362,65.1465238200804,42.3);
#2068=ELLIPSE('',#53363,42.7157063175375,42.3);
#2069=ELLIPSE('',#53364,684.784865862975,42.3);
#2070=ELLIPSE('',#53365,148.655022233233,42.3);
#2071=ELLIPSE('',#53366,86.0962585581532,42.3);
#2072=ELLIPSE('',#53367,135.078923826262,42.3);
#2073=ELLIPSE('',#53368,135.078923826262,42.3);
#2074=ELLIPSE('',#53369,86.0962585581534,42.3);
#2075=ELLIPSE('',#53370,148.655022233233,42.3);
#2076=ELLIPSE('',#53371,684.784865862974,42.3);
#2077=ELLIPSE('',#53372,42.7157063175375,42.3);
#2078=ELLIPSE('',#53389,42.7157063175375,42.3);
#2079=ELLIPSE('',#53391,684.784865862975,42.3);
#2080=ELLIPSE('',#53393,148.655022233233,42.3);
#2081=ELLIPSE('',#53395,86.0962585581532,42.3);
#2082=ELLIPSE('',#53397,135.078923826262,42.3);
#2083=ELLIPSE('',#53400,135.078923826262,42.3);
#2084=ELLIPSE('',#53402,86.0962585581534,42.3);
#2085=ELLIPSE('',#53404,148.655022233233,42.3);
#2086=ELLIPSE('',#53406,684.784865862974,42.3);
#2087=ELLIPSE('',#53408,42.7157063175375,42.3);
#2088=ELLIPSE('',#53413,65.1465238200804,42.3);
#2089=ELLIPSE('',#53414,42.7157063175375,42.3);
#2090=ELLIPSE('',#53415,684.784865862975,42.3);
#2091=ELLIPSE('',#53416,148.655022233233,42.3);
#2092=ELLIPSE('',#53417,86.0962585581532,42.3);
#2093=ELLIPSE('',#53418,135.078923826262,42.3);
#2094=ELLIPSE('',#53419,135.078923826262,42.3);
#2095=ELLIPSE('',#53420,86.0962585581534,42.3);
#2096=ELLIPSE('',#53421,148.655022233233,42.3);
#2097=ELLIPSE('',#53422,684.784865862974,42.3);
#2098=ELLIPSE('',#53423,42.7157063175375,42.3);
#2099=ELLIPSE('',#53440,42.7157063175375,42.3);
#2100=ELLIPSE('',#53442,684.784865862975,42.3);
#2101=ELLIPSE('',#53444,148.655022233233,42.3);
#2102=ELLIPSE('',#53446,86.0962585581532,42.3);
#2103=ELLIPSE('',#53448,135.078923826262,42.3);
#2104=ELLIPSE('',#53451,135.078923826262,42.3);
#2105=ELLIPSE('',#53453,86.0962585581534,42.3);
#2106=ELLIPSE('',#53455,148.655022233233,42.3);
#2107=ELLIPSE('',#53457,684.784865862974,42.3);
#2108=ELLIPSE('',#53459,42.7157063175375,42.3);
#2109=ELLIPSE('',#53464,65.1465238200804,42.3);
#2110=ELLIPSE('',#53465,42.7157063175375,42.3);
#2111=ELLIPSE('',#53466,684.784865862975,42.3);
#2112=ELLIPSE('',#53467,148.655022233233,42.3);
#2113=ELLIPSE('',#53468,86.0962585581532,42.3);
#2114=ELLIPSE('',#53469,135.078923826262,42.3);
#2115=ELLIPSE('',#53470,135.078923826262,42.3);
#2116=ELLIPSE('',#53471,86.0962585581534,42.3);
#2117=ELLIPSE('',#53472,148.655022233233,42.3);
#2118=ELLIPSE('',#53473,684.784865862974,42.3);
#2119=ELLIPSE('',#53474,42.7157063175375,42.3);
#2120=ELLIPSE('',#53491,42.7157063175375,42.3);
#2121=ELLIPSE('',#53493,684.784865862975,42.3);
#2122=ELLIPSE('',#53495,148.655022233233,42.3);
#2123=ELLIPSE('',#53497,86.0962585581532,42.3);
#2124=ELLIPSE('',#53499,135.078923826262,42.3);
#2125=ELLIPSE('',#53502,135.078923826262,42.3);
#2126=ELLIPSE('',#53504,86.0962585581534,42.3);
#2127=ELLIPSE('',#53506,148.655022233233,42.3);
#2128=ELLIPSE('',#53508,684.784865862974,42.3);
#2129=ELLIPSE('',#53510,42.7157063175375,42.3);
#2130=ELLIPSE('',#53515,65.1465238200804,42.3);
#2131=ELLIPSE('',#53516,42.7157063175375,42.3);
#2132=ELLIPSE('',#53517,684.784865862975,42.3);
#2133=ELLIPSE('',#53518,148.655022233233,42.3);
#2134=ELLIPSE('',#53519,86.0962585581532,42.3);
#2135=ELLIPSE('',#53520,135.078923826262,42.3);
#2136=ELLIPSE('',#53521,135.078923826262,42.3);
#2137=ELLIPSE('',#53522,86.0962585581534,42.3);
#2138=ELLIPSE('',#53523,148.655022233233,42.3);
#2139=ELLIPSE('',#53524,684.784865862974,42.3);
#2140=ELLIPSE('',#53525,42.7157063175375,42.3);
#2141=ELLIPSE('',#53528,42.7157063175375,42.3);
#2142=ELLIPSE('',#53530,684.784865862975,42.3);
#2143=ELLIPSE('',#53532,148.655022233233,42.3);
#2144=ELLIPSE('',#53534,86.0962585581532,42.3);
#2145=ELLIPSE('',#53536,135.078923826262,42.3);
#2146=ELLIPSE('',#53539,135.078923826262,42.3);
#2147=ELLIPSE('',#53541,86.0962585581534,42.3);
#2148=ELLIPSE('',#53543,148.655022233233,42.3);
#2149=ELLIPSE('',#53545,684.784865862974,42.3);
#2150=ELLIPSE('',#53547,42.7157063175375,42.3);
#2151=ELLIPSE('',#53550,65.1465238200804,42.3);
#2152=ELLIPSE('',#54832,10.2,5.1);
#2153=ELLIPSE('',#54836,18.1,9.05);
#2154=ELLIPSE('',#54839,18.1,9.05);
#2155=ELLIPSE('',#54841,10.2,5.1);
#2156=ELLIPSE('',#55291,14.8,7.4);
#2157=ELLIPSE('',#55294,14.8,7.4);
#2158=ELLIPSE('',#55295,8.1,4.05);
#2159=ELLIPSE('',#55297,8.1,4.05);
#2160=LINE('',#68802,#6688);
#2161=LINE('',#68804,#6689);
#2162=LINE('',#68806,#6690);
#2163=LINE('',#68808,#6691);
#2164=LINE('',#68810,#6692);
#2165=LINE('',#68812,#6693);
#2166=LINE('',#68814,#6694);
#2167=LINE('',#68816,#6695);
#2168=LINE('',#68818,#6696);
#2169=LINE('',#68820,#6697);
#2170=LINE('',#68822,#6698);
#2171=LINE('',#68824,#6699);
#2172=LINE('',#68826,#6700);
#2173=LINE('',#68828,#6701);
#2174=LINE('',#68830,#6702);
#2175=LINE('',#68836,#6703);
#2176=LINE('',#68838,#6704);
#2177=LINE('',#68840,#6705);
#2178=LINE('',#68842,#6706);
#2179=LINE('',#68844,#6707);
#2180=LINE('',#68846,#6708);
#2181=LINE('',#68848,#6709);
#2182=LINE('',#68850,#6710);
#2183=LINE('',#68852,#6711);
#2184=LINE('',#68854,#6712);
#2185=LINE('',#68856,#6713);
#2186=LINE('',#68858,#6714);
#2187=LINE('',#68860,#6715);
#2188=LINE('',#68862,#6716);
#2189=LINE('',#68863,#6717);
#2190=LINE('',#68866,#6718);
#2191=LINE('',#68868,#6719);
#2192=LINE('',#68875,#6720);
#2193=LINE('',#68878,#6721);
#2194=LINE('',#68880,#6722);
#2195=LINE('',#68882,#6723);
#2196=LINE('',#68884,#6724);
#2197=LINE('',#68886,#6725);
#2198=LINE('',#68888,#6726);
#2199=LINE('',#68890,#6727);
#2200=LINE('',#68892,#6728);
#2201=LINE('',#68894,#6729);
#2202=LINE('',#68896,#6730);
#2203=LINE('',#68898,#6731);
#2204=LINE('',#68900,#6732);
#2205=LINE('',#68902,#6733);
#2206=LINE('',#68904,#6734);
#2207=LINE('',#68906,#6735);
#2208=LINE('',#68912,#6736);
#2209=LINE('',#68914,#6737);
#2210=LINE('',#68916,#6738);
#2211=LINE('',#68918,#6739);
#2212=LINE('',#68920,#6740);
#2213=LINE('',#68922,#6741);
#2214=LINE('',#68924,#6742);
#2215=LINE('',#68926,#6743);
#2216=LINE('',#68928,#6744);
#2217=LINE('',#68930,#6745);
#2218=LINE('',#68932,#6746);
#2219=LINE('',#68934,#6747);
#2220=LINE('',#68936,#6748);
#2221=LINE('',#68938,#6749);
#2222=LINE('',#68939,#6750);
#2223=LINE('',#68942,#6751);
#2224=LINE('',#68944,#6752);
#2225=LINE('',#68951,#6753);
#2226=LINE('',#68954,#6754);
#2227=LINE('',#68956,#6755);
#2228=LINE('',#68958,#6756);
#2229=LINE('',#68960,#6757);
#2230=LINE('',#68962,#6758);
#2231=LINE('',#68964,#6759);
#2232=LINE('',#68966,#6760);
#2233=LINE('',#68968,#6761);
#2234=LINE('',#68970,#6762);
#2235=LINE('',#68972,#6763);
#2236=LINE('',#68974,#6764);
#2237=LINE('',#68976,#6765);
#2238=LINE('',#68978,#6766);
#2239=LINE('',#68980,#6767);
#2240=LINE('',#68982,#6768);
#2241=LINE('',#68988,#6769);
#2242=LINE('',#68990,#6770);
#2243=LINE('',#68992,#6771);
#2244=LINE('',#68994,#6772);
#2245=LINE('',#68996,#6773);
#2246=LINE('',#68998,#6774);
#2247=LINE('',#69000,#6775);
#2248=LINE('',#69002,#6776);
#2249=LINE('',#69004,#6777);
#2250=LINE('',#69006,#6778);
#2251=LINE('',#69008,#6779);
#2252=LINE('',#69010,#6780);
#2253=LINE('',#69012,#6781);
#2254=LINE('',#69014,#6782);
#2255=LINE('',#69015,#6783);
#2256=LINE('',#69018,#6784);
#2257=LINE('',#69020,#6785);
#2258=LINE('',#69027,#6786);
#2259=LINE('',#69030,#6787);
#2260=LINE('',#69032,#6788);
#2261=LINE('',#69034,#6789);
#2262=LINE('',#69036,#6790);
#2263=LINE('',#69038,#6791);
#2264=LINE('',#69040,#6792);
#2265=LINE('',#69042,#6793);
#2266=LINE('',#69044,#6794);
#2267=LINE('',#69046,#6795);
#2268=LINE('',#69048,#6796);
#2269=LINE('',#69050,#6797);
#2270=LINE('',#69052,#6798);
#2271=LINE('',#69054,#6799);
#2272=LINE('',#69056,#6800);
#2273=LINE('',#69058,#6801);
#2274=LINE('',#69064,#6802);
#2275=LINE('',#69066,#6803);
#2276=LINE('',#69068,#6804);
#2277=LINE('',#69070,#6805);
#2278=LINE('',#69072,#6806);
#2279=LINE('',#69074,#6807);
#2280=LINE('',#69076,#6808);
#2281=LINE('',#69078,#6809);
#2282=LINE('',#69080,#6810);
#2283=LINE('',#69082,#6811);
#2284=LINE('',#69084,#6812);
#2285=LINE('',#69086,#6813);
#2286=LINE('',#69088,#6814);
#2287=LINE('',#69090,#6815);
#2288=LINE('',#69091,#6816);
#2289=LINE('',#69094,#6817);
#2290=LINE('',#69096,#6818);
#2291=LINE('',#69103,#6819);
#2292=LINE('',#69106,#6820);
#2293=LINE('',#69108,#6821);
#2294=LINE('',#69110,#6822);
#2295=LINE('',#69112,#6823);
#2296=LINE('',#69114,#6824);
#2297=LINE('',#69116,#6825);
#2298=LINE('',#69118,#6826);
#2299=LINE('',#69120,#6827);
#2300=LINE('',#69122,#6828);
#2301=LINE('',#69124,#6829);
#2302=LINE('',#69126,#6830);
#2303=LINE('',#69128,#6831);
#2304=LINE('',#69130,#6832);
#2305=LINE('',#69132,#6833);
#2306=LINE('',#69134,#6834);
#2307=LINE('',#69140,#6835);
#2308=LINE('',#69142,#6836);
#2309=LINE('',#69144,#6837);
#2310=LINE('',#69146,#6838);
#2311=LINE('',#69148,#6839);
#2312=LINE('',#69150,#6840);
#2313=LINE('',#69152,#6841);
#2314=LINE('',#69154,#6842);
#2315=LINE('',#69156,#6843);
#2316=LINE('',#69158,#6844);
#2317=LINE('',#69160,#6845);
#2318=LINE('',#69162,#6846);
#2319=LINE('',#69164,#6847);
#2320=LINE('',#69166,#6848);
#2321=LINE('',#69167,#6849);
#2322=LINE('',#69170,#6850);
#2323=LINE('',#69172,#6851);
#2324=LINE('',#69179,#6852);
#2325=LINE('',#69182,#6853);
#2326=LINE('',#69184,#6854);
#2327=LINE('',#69186,#6855);
#2328=LINE('',#69188,#6856);
#2329=LINE('',#69190,#6857);
#2330=LINE('',#69192,#6858);
#2331=LINE('',#69194,#6859);
#2332=LINE('',#69196,#6860);
#2333=LINE('',#69198,#6861);
#2334=LINE('',#69200,#6862);
#2335=LINE('',#69202,#6863);
#2336=LINE('',#69204,#6864);
#2337=LINE('',#69206,#6865);
#2338=LINE('',#69208,#6866);
#2339=LINE('',#69210,#6867);
#2340=LINE('',#69216,#6868);
#2341=LINE('',#69218,#6869);
#2342=LINE('',#69220,#6870);
#2343=LINE('',#69222,#6871);
#2344=LINE('',#69224,#6872);
#2345=LINE('',#69226,#6873);
#2346=LINE('',#69228,#6874);
#2347=LINE('',#69230,#6875);
#2348=LINE('',#69232,#6876);
#2349=LINE('',#69234,#6877);
#2350=LINE('',#69236,#6878);
#2351=LINE('',#69238,#6879);
#2352=LINE('',#69240,#6880);
#2353=LINE('',#69242,#6881);
#2354=LINE('',#69243,#6882);
#2355=LINE('',#69246,#6883);
#2356=LINE('',#69248,#6884);
#2357=LINE('',#69255,#6885);
#2358=LINE('',#69258,#6886);
#2359=LINE('',#69260,#6887);
#2360=LINE('',#69262,#6888);
#2361=LINE('',#69264,#6889);
#2362=LINE('',#69266,#6890);
#2363=LINE('',#69268,#6891);
#2364=LINE('',#69270,#6892);
#2365=LINE('',#69272,#6893);
#2366=LINE('',#69274,#6894);
#2367=LINE('',#69276,#6895);
#2368=LINE('',#69278,#6896);
#2369=LINE('',#69280,#6897);
#2370=LINE('',#69282,#6898);
#2371=LINE('',#69284,#6899);
#2372=LINE('',#69286,#6900);
#2373=LINE('',#69292,#6901);
#2374=LINE('',#69294,#6902);
#2375=LINE('',#69296,#6903);
#2376=LINE('',#69298,#6904);
#2377=LINE('',#69300,#6905);
#2378=LINE('',#69302,#6906);
#2379=LINE('',#69304,#6907);
#2380=LINE('',#69306,#6908);
#2381=LINE('',#69308,#6909);
#2382=LINE('',#69310,#6910);
#2383=LINE('',#69312,#6911);
#2384=LINE('',#69314,#6912);
#2385=LINE('',#69316,#6913);
#2386=LINE('',#69318,#6914);
#2387=LINE('',#69319,#6915);
#2388=LINE('',#69322,#6916);
#2389=LINE('',#69324,#6917);
#2390=LINE('',#69331,#6918);
#2391=LINE('',#69334,#6919);
#2392=LINE('',#69336,#6920);
#2393=LINE('',#69338,#6921);
#2394=LINE('',#69340,#6922);
#2395=LINE('',#69342,#6923);
#2396=LINE('',#69344,#6924);
#2397=LINE('',#69346,#6925);
#2398=LINE('',#69348,#6926);
#2399=LINE('',#69350,#6927);
#2400=LINE('',#69352,#6928);
#2401=LINE('',#69354,#6929);
#2402=LINE('',#69356,#6930);
#2403=LINE('',#69358,#6931);
#2404=LINE('',#69360,#6932);
#2405=LINE('',#69362,#6933);
#2406=LINE('',#69368,#6934);
#2407=LINE('',#69370,#6935);
#2408=LINE('',#69372,#6936);
#2409=LINE('',#69374,#6937);
#2410=LINE('',#69376,#6938);
#2411=LINE('',#69378,#6939);
#2412=LINE('',#69380,#6940);
#2413=LINE('',#69382,#6941);
#2414=LINE('',#69384,#6942);
#2415=LINE('',#69386,#6943);
#2416=LINE('',#69388,#6944);
#2417=LINE('',#69390,#6945);
#2418=LINE('',#69392,#6946);
#2419=LINE('',#69394,#6947);
#2420=LINE('',#69395,#6948);
#2421=LINE('',#69398,#6949);
#2422=LINE('',#69400,#6950);
#2423=LINE('',#69407,#6951);
#2424=LINE('',#69410,#6952);
#2425=LINE('',#69412,#6953);
#2426=LINE('',#69414,#6954);
#2427=LINE('',#69416,#6955);
#2428=LINE('',#69418,#6956);
#2429=LINE('',#69420,#6957);
#2430=LINE('',#69422,#6958);
#2431=LINE('',#69424,#6959);
#2432=LINE('',#69426,#6960);
#2433=LINE('',#69428,#6961);
#2434=LINE('',#69430,#6962);
#2435=LINE('',#69432,#6963);
#2436=LINE('',#69434,#6964);
#2437=LINE('',#69436,#6965);
#2438=LINE('',#69438,#6966);
#2439=LINE('',#69444,#6967);
#2440=LINE('',#69446,#6968);
#2441=LINE('',#69448,#6969);
#2442=LINE('',#69450,#6970);
#2443=LINE('',#69452,#6971);
#2444=LINE('',#69454,#6972);
#2445=LINE('',#69456,#6973);
#2446=LINE('',#69458,#6974);
#2447=LINE('',#69460,#6975);
#2448=LINE('',#69462,#6976);
#2449=LINE('',#69464,#6977);
#2450=LINE('',#69466,#6978);
#2451=LINE('',#69468,#6979);
#2452=LINE('',#69470,#6980);
#2453=LINE('',#69471,#6981);
#2454=LINE('',#69474,#6982);
#2455=LINE('',#69476,#6983);
#2456=LINE('',#69483,#6984);
#2457=LINE('',#69486,#6985);
#2458=LINE('',#69488,#6986);
#2459=LINE('',#69490,#6987);
#2460=LINE('',#69492,#6988);
#2461=LINE('',#69494,#6989);
#2462=LINE('',#69496,#6990);
#2463=LINE('',#69498,#6991);
#2464=LINE('',#69500,#6992);
#2465=LINE('',#69502,#6993);
#2466=LINE('',#69504,#6994);
#2467=LINE('',#69506,#6995);
#2468=LINE('',#69508,#6996);
#2469=LINE('',#69510,#6997);
#2470=LINE('',#69512,#6998);
#2471=LINE('',#69514,#6999);
#2472=LINE('',#69520,#7000);
#2473=LINE('',#69522,#7001);
#2474=LINE('',#69524,#7002);
#2475=LINE('',#69526,#7003);
#2476=LINE('',#69528,#7004);
#2477=LINE('',#69530,#7005);
#2478=LINE('',#69532,#7006);
#2479=LINE('',#69534,#7007);
#2480=LINE('',#69536,#7008);
#2481=LINE('',#69538,#7009);
#2482=LINE('',#69540,#7010);
#2483=LINE('',#69542,#7011);
#2484=LINE('',#69544,#7012);
#2485=LINE('',#69546,#7013);
#2486=LINE('',#69547,#7014);
#2487=LINE('',#69550,#7015);
#2488=LINE('',#69552,#7016);
#2489=LINE('',#69559,#7017);
#2490=LINE('',#69562,#7018);
#2491=LINE('',#69564,#7019);
#2492=LINE('',#69566,#7020);
#2493=LINE('',#69568,#7021);
#2494=LINE('',#69570,#7022);
#2495=LINE('',#69572,#7023);
#2496=LINE('',#69574,#7024);
#2497=LINE('',#69576,#7025);
#2498=LINE('',#69578,#7026);
#2499=LINE('',#69580,#7027);
#2500=LINE('',#69582,#7028);
#2501=LINE('',#69584,#7029);
#2502=LINE('',#69586,#7030);
#2503=LINE('',#69588,#7031);
#2504=LINE('',#69590,#7032);
#2505=LINE('',#69596,#7033);
#2506=LINE('',#69598,#7034);
#2507=LINE('',#69600,#7035);
#2508=LINE('',#69602,#7036);
#2509=LINE('',#69604,#7037);
#2510=LINE('',#69606,#7038);
#2511=LINE('',#69608,#7039);
#2512=LINE('',#69610,#7040);
#2513=LINE('',#69612,#7041);
#2514=LINE('',#69614,#7042);
#2515=LINE('',#69616,#7043);
#2516=LINE('',#69618,#7044);
#2517=LINE('',#69620,#7045);
#2518=LINE('',#69622,#7046);
#2519=LINE('',#69623,#7047);
#2520=LINE('',#69626,#7048);
#2521=LINE('',#69628,#7049);
#2522=LINE('',#69635,#7050);
#2523=LINE('',#69638,#7051);
#2524=LINE('',#69640,#7052);
#2525=LINE('',#69642,#7053);
#2526=LINE('',#69644,#7054);
#2527=LINE('',#69646,#7055);
#2528=LINE('',#69648,#7056);
#2529=LINE('',#69650,#7057);
#2530=LINE('',#69652,#7058);
#2531=LINE('',#69654,#7059);
#2532=LINE('',#69656,#7060);
#2533=LINE('',#69658,#7061);
#2534=LINE('',#69660,#7062);
#2535=LINE('',#69662,#7063);
#2536=LINE('',#69664,#7064);
#2537=LINE('',#69666,#7065);
#2538=LINE('',#69672,#7066);
#2539=LINE('',#69674,#7067);
#2540=LINE('',#69676,#7068);
#2541=LINE('',#69678,#7069);
#2542=LINE('',#69680,#7070);
#2543=LINE('',#69682,#7071);
#2544=LINE('',#69684,#7072);
#2545=LINE('',#69686,#7073);
#2546=LINE('',#69688,#7074);
#2547=LINE('',#69690,#7075);
#2548=LINE('',#69692,#7076);
#2549=LINE('',#69694,#7077);
#2550=LINE('',#69696,#7078);
#2551=LINE('',#69698,#7079);
#2552=LINE('',#69699,#7080);
#2553=LINE('',#69702,#7081);
#2554=LINE('',#69704,#7082);
#2555=LINE('',#69711,#7083);
#2556=LINE('',#69714,#7084);
#2557=LINE('',#69716,#7085);
#2558=LINE('',#69718,#7086);
#2559=LINE('',#69720,#7087);
#2560=LINE('',#69722,#7088);
#2561=LINE('',#69724,#7089);
#2562=LINE('',#69726,#7090);
#2563=LINE('',#69728,#7091);
#2564=LINE('',#69730,#7092);
#2565=LINE('',#69732,#7093);
#2566=LINE('',#69734,#7094);
#2567=LINE('',#69736,#7095);
#2568=LINE('',#69738,#7096);
#2569=LINE('',#69740,#7097);
#2570=LINE('',#69742,#7098);
#2571=LINE('',#69748,#7099);
#2572=LINE('',#69750,#7100);
#2573=LINE('',#69752,#7101);
#2574=LINE('',#69754,#7102);
#2575=LINE('',#69756,#7103);
#2576=LINE('',#69758,#7104);
#2577=LINE('',#69760,#7105);
#2578=LINE('',#69762,#7106);
#2579=LINE('',#69764,#7107);
#2580=LINE('',#69766,#7108);
#2581=LINE('',#69768,#7109);
#2582=LINE('',#69770,#7110);
#2583=LINE('',#69772,#7111);
#2584=LINE('',#69774,#7112);
#2585=LINE('',#69775,#7113);
#2586=LINE('',#69778,#7114);
#2587=LINE('',#69780,#7115);
#2588=LINE('',#69787,#7116);
#2589=LINE('',#69790,#7117);
#2590=LINE('',#69792,#7118);
#2591=LINE('',#69794,#7119);
#2592=LINE('',#69796,#7120);
#2593=LINE('',#69798,#7121);
#2594=LINE('',#69800,#7122);
#2595=LINE('',#69802,#7123);
#2596=LINE('',#69804,#7124);
#2597=LINE('',#69806,#7125);
#2598=LINE('',#69808,#7126);
#2599=LINE('',#69810,#7127);
#2600=LINE('',#69812,#7128);
#2601=LINE('',#69814,#7129);
#2602=LINE('',#69816,#7130);
#2603=LINE('',#69818,#7131);
#2604=LINE('',#69824,#7132);
#2605=LINE('',#69826,#7133);
#2606=LINE('',#69828,#7134);
#2607=LINE('',#69830,#7135);
#2608=LINE('',#69832,#7136);
#2609=LINE('',#69834,#7137);
#2610=LINE('',#69836,#7138);
#2611=LINE('',#69838,#7139);
#2612=LINE('',#69840,#7140);
#2613=LINE('',#69842,#7141);
#2614=LINE('',#69844,#7142);
#2615=LINE('',#69846,#7143);
#2616=LINE('',#69848,#7144);
#2617=LINE('',#69850,#7145);
#2618=LINE('',#69851,#7146);
#2619=LINE('',#69854,#7147);
#2620=LINE('',#69856,#7148);
#2621=LINE('',#69863,#7149);
#2622=LINE('',#69866,#7150);
#2623=LINE('',#69868,#7151);
#2624=LINE('',#69870,#7152);
#2625=LINE('',#69872,#7153);
#2626=LINE('',#69874,#7154);
#2627=LINE('',#69876,#7155);
#2628=LINE('',#69878,#7156);
#2629=LINE('',#69880,#7157);
#2630=LINE('',#69882,#7158);
#2631=LINE('',#69884,#7159);
#2632=LINE('',#69886,#7160);
#2633=LINE('',#69888,#7161);
#2634=LINE('',#69890,#7162);
#2635=LINE('',#69892,#7163);
#2636=LINE('',#69894,#7164);
#2637=LINE('',#69900,#7165);
#2638=LINE('',#69902,#7166);
#2639=LINE('',#69904,#7167);
#2640=LINE('',#69906,#7168);
#2641=LINE('',#69908,#7169);
#2642=LINE('',#69910,#7170);
#2643=LINE('',#69912,#7171);
#2644=LINE('',#69914,#7172);
#2645=LINE('',#69916,#7173);
#2646=LINE('',#69918,#7174);
#2647=LINE('',#69920,#7175);
#2648=LINE('',#69922,#7176);
#2649=LINE('',#69924,#7177);
#2650=LINE('',#69926,#7178);
#2651=LINE('',#69927,#7179);
#2652=LINE('',#69930,#7180);
#2653=LINE('',#69932,#7181);
#2654=LINE('',#69939,#7182);
#2655=LINE('',#69942,#7183);
#2656=LINE('',#69944,#7184);
#2657=LINE('',#69946,#7185);
#2658=LINE('',#69948,#7186);
#2659=LINE('',#69950,#7187);
#2660=LINE('',#69952,#7188);
#2661=LINE('',#69954,#7189);
#2662=LINE('',#69956,#7190);
#2663=LINE('',#69958,#7191);
#2664=LINE('',#69960,#7192);
#2665=LINE('',#69962,#7193);
#2666=LINE('',#69964,#7194);
#2667=LINE('',#69966,#7195);
#2668=LINE('',#69968,#7196);
#2669=LINE('',#69970,#7197);
#2670=LINE('',#69976,#7198);
#2671=LINE('',#69978,#7199);
#2672=LINE('',#69980,#7200);
#2673=LINE('',#69982,#7201);
#2674=LINE('',#69984,#7202);
#2675=LINE('',#69986,#7203);
#2676=LINE('',#69988,#7204);
#2677=LINE('',#69990,#7205);
#2678=LINE('',#69992,#7206);
#2679=LINE('',#69994,#7207);
#2680=LINE('',#69996,#7208);
#2681=LINE('',#69998,#7209);
#2682=LINE('',#70000,#7210);
#2683=LINE('',#70002,#7211);
#2684=LINE('',#70003,#7212);
#2685=LINE('',#70006,#7213);
#2686=LINE('',#70008,#7214);
#2687=LINE('',#70015,#7215);
#2688=LINE('',#70018,#7216);
#2689=LINE('',#70020,#7217);
#2690=LINE('',#70022,#7218);
#2691=LINE('',#70024,#7219);
#2692=LINE('',#70026,#7220);
#2693=LINE('',#70028,#7221);
#2694=LINE('',#70030,#7222);
#2695=LINE('',#70032,#7223);
#2696=LINE('',#70034,#7224);
#2697=LINE('',#70036,#7225);
#2698=LINE('',#70038,#7226);
#2699=LINE('',#70040,#7227);
#2700=LINE('',#70042,#7228);
#2701=LINE('',#70044,#7229);
#2702=LINE('',#70046,#7230);
#2703=LINE('',#70052,#7231);
#2704=LINE('',#70054,#7232);
#2705=LINE('',#70056,#7233);
#2706=LINE('',#70058,#7234);
#2707=LINE('',#70060,#7235);
#2708=LINE('',#70062,#7236);
#2709=LINE('',#70064,#7237);
#2710=LINE('',#70066,#7238);
#2711=LINE('',#70068,#7239);
#2712=LINE('',#70070,#7240);
#2713=LINE('',#70072,#7241);
#2714=LINE('',#70074,#7242);
#2715=LINE('',#70076,#7243);
#2716=LINE('',#70078,#7244);
#2717=LINE('',#70079,#7245);
#2718=LINE('',#70082,#7246);
#2719=LINE('',#70084,#7247);
#2720=LINE('',#70091,#7248);
#2721=LINE('',#70094,#7249);
#2722=LINE('',#70096,#7250);
#2723=LINE('',#70098,#7251);
#2724=LINE('',#70100,#7252);
#2725=LINE('',#70102,#7253);
#2726=LINE('',#70104,#7254);
#2727=LINE('',#70106,#7255);
#2728=LINE('',#70108,#7256);
#2729=LINE('',#70110,#7257);
#2730=LINE('',#70112,#7258);
#2731=LINE('',#70114,#7259);
#2732=LINE('',#70116,#7260);
#2733=LINE('',#70118,#7261);
#2734=LINE('',#70120,#7262);
#2735=LINE('',#70122,#7263);
#2736=LINE('',#70128,#7264);
#2737=LINE('',#70130,#7265);
#2738=LINE('',#70132,#7266);
#2739=LINE('',#70134,#7267);
#2740=LINE('',#70136,#7268);
#2741=LINE('',#70138,#7269);
#2742=LINE('',#70140,#7270);
#2743=LINE('',#70142,#7271);
#2744=LINE('',#70144,#7272);
#2745=LINE('',#70146,#7273);
#2746=LINE('',#70148,#7274);
#2747=LINE('',#70150,#7275);
#2748=LINE('',#70152,#7276);
#2749=LINE('',#70154,#7277);
#2750=LINE('',#70155,#7278);
#2751=LINE('',#70158,#7279);
#2752=LINE('',#70160,#7280);
#2753=LINE('',#70167,#7281);
#2754=LINE('',#70170,#7282);
#2755=LINE('',#70172,#7283);
#2756=LINE('',#70174,#7284);
#2757=LINE('',#70176,#7285);
#2758=LINE('',#70178,#7286);
#2759=LINE('',#70180,#7287);
#2760=LINE('',#70182,#7288);
#2761=LINE('',#70184,#7289);
#2762=LINE('',#70186,#7290);
#2763=LINE('',#70188,#7291);
#2764=LINE('',#70190,#7292);
#2765=LINE('',#70192,#7293);
#2766=LINE('',#70194,#7294);
#2767=LINE('',#70196,#7295);
#2768=LINE('',#70198,#7296);
#2769=LINE('',#70204,#7297);
#2770=LINE('',#70206,#7298);
#2771=LINE('',#70208,#7299);
#2772=LINE('',#70210,#7300);
#2773=LINE('',#70212,#7301);
#2774=LINE('',#70214,#7302);
#2775=LINE('',#70216,#7303);
#2776=LINE('',#70218,#7304);
#2777=LINE('',#70220,#7305);
#2778=LINE('',#70222,#7306);
#2779=LINE('',#70224,#7307);
#2780=LINE('',#70226,#7308);
#2781=LINE('',#70228,#7309);
#2782=LINE('',#70230,#7310);
#2783=LINE('',#70231,#7311);
#2784=LINE('',#70234,#7312);
#2785=LINE('',#70236,#7313);
#2786=LINE('',#70243,#7314);
#2787=LINE('',#70246,#7315);
#2788=LINE('',#70248,#7316);
#2789=LINE('',#70250,#7317);
#2790=LINE('',#70252,#7318);
#2791=LINE('',#70254,#7319);
#2792=LINE('',#70256,#7320);
#2793=LINE('',#70258,#7321);
#2794=LINE('',#70260,#7322);
#2795=LINE('',#70262,#7323);
#2796=LINE('',#70264,#7324);
#2797=LINE('',#70266,#7325);
#2798=LINE('',#70268,#7326);
#2799=LINE('',#70270,#7327);
#2800=LINE('',#70272,#7328);
#2801=LINE('',#70274,#7329);
#2802=LINE('',#70280,#7330);
#2803=LINE('',#70282,#7331);
#2804=LINE('',#70284,#7332);
#2805=LINE('',#70286,#7333);
#2806=LINE('',#70288,#7334);
#2807=LINE('',#70290,#7335);
#2808=LINE('',#70292,#7336);
#2809=LINE('',#70294,#7337);
#2810=LINE('',#70296,#7338);
#2811=LINE('',#70298,#7339);
#2812=LINE('',#70300,#7340);
#2813=LINE('',#70302,#7341);
#2814=LINE('',#70304,#7342);
#2815=LINE('',#70306,#7343);
#2816=LINE('',#70307,#7344);
#2817=LINE('',#70310,#7345);
#2818=LINE('',#70312,#7346);
#2819=LINE('',#70319,#7347);
#2820=LINE('',#70322,#7348);
#2821=LINE('',#70324,#7349);
#2822=LINE('',#70326,#7350);
#2823=LINE('',#70328,#7351);
#2824=LINE('',#70330,#7352);
#2825=LINE('',#70332,#7353);
#2826=LINE('',#70334,#7354);
#2827=LINE('',#70336,#7355);
#2828=LINE('',#70338,#7356);
#2829=LINE('',#70340,#7357);
#2830=LINE('',#70342,#7358);
#2831=LINE('',#70344,#7359);
#2832=LINE('',#70346,#7360);
#2833=LINE('',#70348,#7361);
#2834=LINE('',#70350,#7362);
#2835=LINE('',#70356,#7363);
#2836=LINE('',#70358,#7364);
#2837=LINE('',#70360,#7365);
#2838=LINE('',#70362,#7366);
#2839=LINE('',#70364,#7367);
#2840=LINE('',#70366,#7368);
#2841=LINE('',#70368,#7369);
#2842=LINE('',#70370,#7370);
#2843=LINE('',#70372,#7371);
#2844=LINE('',#70374,#7372);
#2845=LINE('',#70376,#7373);
#2846=LINE('',#70378,#7374);
#2847=LINE('',#70380,#7375);
#2848=LINE('',#70382,#7376);
#2849=LINE('',#70383,#7377);
#2850=LINE('',#70386,#7378);
#2851=LINE('',#70388,#7379);
#2852=LINE('',#70395,#7380);
#2853=LINE('',#70398,#7381);
#2854=LINE('',#70400,#7382);
#2855=LINE('',#70402,#7383);
#2856=LINE('',#70404,#7384);
#2857=LINE('',#70406,#7385);
#2858=LINE('',#70408,#7386);
#2859=LINE('',#70410,#7387);
#2860=LINE('',#70412,#7388);
#2861=LINE('',#70414,#7389);
#2862=LINE('',#70416,#7390);
#2863=LINE('',#70418,#7391);
#2864=LINE('',#70420,#7392);
#2865=LINE('',#70422,#7393);
#2866=LINE('',#70424,#7394);
#2867=LINE('',#70426,#7395);
#2868=LINE('',#70432,#7396);
#2869=LINE('',#70434,#7397);
#2870=LINE('',#70436,#7398);
#2871=LINE('',#70438,#7399);
#2872=LINE('',#70440,#7400);
#2873=LINE('',#70442,#7401);
#2874=LINE('',#70444,#7402);
#2875=LINE('',#70446,#7403);
#2876=LINE('',#70448,#7404);
#2877=LINE('',#70450,#7405);
#2878=LINE('',#70452,#7406);
#2879=LINE('',#70454,#7407);
#2880=LINE('',#70456,#7408);
#2881=LINE('',#70458,#7409);
#2882=LINE('',#70459,#7410);
#2883=LINE('',#70462,#7411);
#2884=LINE('',#70464,#7412);
#2885=LINE('',#70471,#7413);
#2886=LINE('',#70474,#7414);
#2887=LINE('',#70476,#7415);
#2888=LINE('',#70478,#7416);
#2889=LINE('',#70480,#7417);
#2890=LINE('',#70482,#7418);
#2891=LINE('',#70484,#7419);
#2892=LINE('',#70486,#7420);
#2893=LINE('',#70488,#7421);
#2894=LINE('',#70490,#7422);
#2895=LINE('',#70492,#7423);
#2896=LINE('',#70494,#7424);
#2897=LINE('',#70496,#7425);
#2898=LINE('',#70498,#7426);
#2899=LINE('',#70500,#7427);
#2900=LINE('',#70502,#7428);
#2901=LINE('',#70508,#7429);
#2902=LINE('',#70510,#7430);
#2903=LINE('',#70512,#7431);
#2904=LINE('',#70514,#7432);
#2905=LINE('',#70516,#7433);
#2906=LINE('',#70518,#7434);
#2907=LINE('',#70520,#7435);
#2908=LINE('',#70522,#7436);
#2909=LINE('',#70524,#7437);
#2910=LINE('',#70526,#7438);
#2911=LINE('',#70528,#7439);
#2912=LINE('',#70530,#7440);
#2913=LINE('',#70532,#7441);
#2914=LINE('',#70534,#7442);
#2915=LINE('',#70535,#7443);
#2916=LINE('',#70538,#7444);
#2917=LINE('',#70540,#7445);
#2918=LINE('',#70547,#7446);
#2919=LINE('',#70550,#7447);
#2920=LINE('',#70552,#7448);
#2921=LINE('',#70554,#7449);
#2922=LINE('',#70556,#7450);
#2923=LINE('',#70558,#7451);
#2924=LINE('',#70560,#7452);
#2925=LINE('',#70562,#7453);
#2926=LINE('',#70564,#7454);
#2927=LINE('',#70566,#7455);
#2928=LINE('',#70568,#7456);
#2929=LINE('',#70570,#7457);
#2930=LINE('',#70572,#7458);
#2931=LINE('',#70574,#7459);
#2932=LINE('',#70576,#7460);
#2933=LINE('',#70578,#7461);
#2934=LINE('',#70584,#7462);
#2935=LINE('',#70586,#7463);
#2936=LINE('',#70588,#7464);
#2937=LINE('',#70590,#7465);
#2938=LINE('',#70592,#7466);
#2939=LINE('',#70594,#7467);
#2940=LINE('',#70596,#7468);
#2941=LINE('',#70598,#7469);
#2942=LINE('',#70600,#7470);
#2943=LINE('',#70602,#7471);
#2944=LINE('',#70604,#7472);
#2945=LINE('',#70606,#7473);
#2946=LINE('',#70608,#7474);
#2947=LINE('',#70610,#7475);
#2948=LINE('',#70611,#7476);
#2949=LINE('',#70614,#7477);
#2950=LINE('',#70616,#7478);
#2951=LINE('',#70623,#7479);
#2952=LINE('',#70626,#7480);
#2953=LINE('',#70628,#7481);
#2954=LINE('',#70630,#7482);
#2955=LINE('',#70632,#7483);
#2956=LINE('',#70634,#7484);
#2957=LINE('',#70636,#7485);
#2958=LINE('',#70638,#7486);
#2959=LINE('',#70640,#7487);
#2960=LINE('',#70642,#7488);
#2961=LINE('',#70644,#7489);
#2962=LINE('',#70646,#7490);
#2963=LINE('',#70648,#7491);
#2964=LINE('',#70650,#7492);
#2965=LINE('',#70652,#7493);
#2966=LINE('',#70654,#7494);
#2967=LINE('',#70660,#7495);
#2968=LINE('',#70662,#7496);
#2969=LINE('',#70664,#7497);
#2970=LINE('',#70666,#7498);
#2971=LINE('',#70668,#7499);
#2972=LINE('',#70670,#7500);
#2973=LINE('',#70672,#7501);
#2974=LINE('',#70674,#7502);
#2975=LINE('',#70676,#7503);
#2976=LINE('',#70678,#7504);
#2977=LINE('',#70680,#7505);
#2978=LINE('',#70682,#7506);
#2979=LINE('',#70684,#7507);
#2980=LINE('',#70686,#7508);
#2981=LINE('',#70687,#7509);
#2982=LINE('',#70690,#7510);
#2983=LINE('',#70692,#7511);
#2984=LINE('',#70699,#7512);
#2985=LINE('',#70702,#7513);
#2986=LINE('',#70704,#7514);
#2987=LINE('',#70706,#7515);
#2988=LINE('',#70708,#7516);
#2989=LINE('',#70710,#7517);
#2990=LINE('',#70712,#7518);
#2991=LINE('',#70714,#7519);
#2992=LINE('',#70716,#7520);
#2993=LINE('',#70718,#7521);
#2994=LINE('',#70720,#7522);
#2995=LINE('',#70722,#7523);
#2996=LINE('',#70724,#7524);
#2997=LINE('',#70726,#7525);
#2998=LINE('',#70728,#7526);
#2999=LINE('',#70730,#7527);
#3000=LINE('',#70736,#7528);
#3001=LINE('',#70738,#7529);
#3002=LINE('',#70740,#7530);
#3003=LINE('',#70742,#7531);
#3004=LINE('',#70744,#7532);
#3005=LINE('',#70746,#7533);
#3006=LINE('',#70748,#7534);
#3007=LINE('',#70750,#7535);
#3008=LINE('',#70752,#7536);
#3009=LINE('',#70754,#7537);
#3010=LINE('',#70756,#7538);
#3011=LINE('',#70758,#7539);
#3012=LINE('',#70760,#7540);
#3013=LINE('',#70762,#7541);
#3014=LINE('',#70763,#7542);
#3015=LINE('',#70766,#7543);
#3016=LINE('',#70768,#7544);
#3017=LINE('',#70775,#7545);
#3018=LINE('',#70778,#7546);
#3019=LINE('',#70780,#7547);
#3020=LINE('',#70782,#7548);
#3021=LINE('',#70784,#7549);
#3022=LINE('',#70786,#7550);
#3023=LINE('',#70788,#7551);
#3024=LINE('',#70790,#7552);
#3025=LINE('',#70792,#7553);
#3026=LINE('',#70794,#7554);
#3027=LINE('',#70796,#7555);
#3028=LINE('',#70798,#7556);
#3029=LINE('',#70800,#7557);
#3030=LINE('',#70802,#7558);
#3031=LINE('',#70804,#7559);
#3032=LINE('',#70806,#7560);
#3033=LINE('',#70812,#7561);
#3034=LINE('',#70814,#7562);
#3035=LINE('',#70816,#7563);
#3036=LINE('',#70818,#7564);
#3037=LINE('',#70820,#7565);
#3038=LINE('',#70822,#7566);
#3039=LINE('',#70824,#7567);
#3040=LINE('',#70826,#7568);
#3041=LINE('',#70828,#7569);
#3042=LINE('',#70830,#7570);
#3043=LINE('',#70832,#7571);
#3044=LINE('',#70834,#7572);
#3045=LINE('',#70836,#7573);
#3046=LINE('',#70838,#7574);
#3047=LINE('',#70839,#7575);
#3048=LINE('',#70842,#7576);
#3049=LINE('',#70844,#7577);
#3050=LINE('',#70851,#7578);
#3051=LINE('',#70854,#7579);
#3052=LINE('',#70856,#7580);
#3053=LINE('',#70858,#7581);
#3054=LINE('',#70860,#7582);
#3055=LINE('',#70862,#7583);
#3056=LINE('',#70864,#7584);
#3057=LINE('',#70866,#7585);
#3058=LINE('',#70868,#7586);
#3059=LINE('',#70870,#7587);
#3060=LINE('',#70872,#7588);
#3061=LINE('',#70874,#7589);
#3062=LINE('',#70876,#7590);
#3063=LINE('',#70878,#7591);
#3064=LINE('',#70880,#7592);
#3065=LINE('',#70882,#7593);
#3066=LINE('',#70888,#7594);
#3067=LINE('',#70890,#7595);
#3068=LINE('',#70892,#7596);
#3069=LINE('',#70894,#7597);
#3070=LINE('',#70896,#7598);
#3071=LINE('',#70898,#7599);
#3072=LINE('',#70900,#7600);
#3073=LINE('',#70902,#7601);
#3074=LINE('',#70904,#7602);
#3075=LINE('',#70906,#7603);
#3076=LINE('',#70908,#7604);
#3077=LINE('',#70910,#7605);
#3078=LINE('',#70912,#7606);
#3079=LINE('',#70914,#7607);
#3080=LINE('',#70915,#7608);
#3081=LINE('',#70918,#7609);
#3082=LINE('',#70920,#7610);
#3083=LINE('',#70927,#7611);
#3084=LINE('',#70930,#7612);
#3085=LINE('',#70932,#7613);
#3086=LINE('',#70934,#7614);
#3087=LINE('',#70936,#7615);
#3088=LINE('',#70938,#7616);
#3089=LINE('',#70940,#7617);
#3090=LINE('',#70942,#7618);
#3091=LINE('',#70944,#7619);
#3092=LINE('',#70946,#7620);
#3093=LINE('',#70948,#7621);
#3094=LINE('',#70950,#7622);
#3095=LINE('',#70952,#7623);
#3096=LINE('',#70954,#7624);
#3097=LINE('',#70956,#7625);
#3098=LINE('',#70958,#7626);
#3099=LINE('',#70964,#7627);
#3100=LINE('',#70966,#7628);
#3101=LINE('',#70968,#7629);
#3102=LINE('',#70970,#7630);
#3103=LINE('',#70972,#7631);
#3104=LINE('',#70974,#7632);
#3105=LINE('',#70976,#7633);
#3106=LINE('',#70978,#7634);
#3107=LINE('',#70980,#7635);
#3108=LINE('',#70982,#7636);
#3109=LINE('',#70984,#7637);
#3110=LINE('',#70986,#7638);
#3111=LINE('',#70988,#7639);
#3112=LINE('',#70990,#7640);
#3113=LINE('',#70991,#7641);
#3114=LINE('',#70994,#7642);
#3115=LINE('',#70996,#7643);
#3116=LINE('',#71003,#7644);
#3117=LINE('',#71006,#7645);
#3118=LINE('',#71008,#7646);
#3119=LINE('',#71010,#7647);
#3120=LINE('',#71012,#7648);
#3121=LINE('',#71014,#7649);
#3122=LINE('',#71016,#7650);
#3123=LINE('',#71018,#7651);
#3124=LINE('',#71020,#7652);
#3125=LINE('',#71022,#7653);
#3126=LINE('',#71024,#7654);
#3127=LINE('',#71026,#7655);
#3128=LINE('',#71028,#7656);
#3129=LINE('',#71030,#7657);
#3130=LINE('',#71032,#7658);
#3131=LINE('',#71034,#7659);
#3132=LINE('',#71040,#7660);
#3133=LINE('',#71042,#7661);
#3134=LINE('',#71044,#7662);
#3135=LINE('',#71046,#7663);
#3136=LINE('',#71048,#7664);
#3137=LINE('',#71050,#7665);
#3138=LINE('',#71052,#7666);
#3139=LINE('',#71054,#7667);
#3140=LINE('',#71056,#7668);
#3141=LINE('',#71058,#7669);
#3142=LINE('',#71060,#7670);
#3143=LINE('',#71062,#7671);
#3144=LINE('',#71064,#7672);
#3145=LINE('',#71066,#7673);
#3146=LINE('',#71067,#7674);
#3147=LINE('',#71070,#7675);
#3148=LINE('',#71072,#7676);
#3149=LINE('',#71079,#7677);
#3150=LINE('',#71082,#7678);
#3151=LINE('',#71084,#7679);
#3152=LINE('',#71086,#7680);
#3153=LINE('',#71088,#7681);
#3154=LINE('',#71090,#7682);
#3155=LINE('',#71092,#7683);
#3156=LINE('',#71094,#7684);
#3157=LINE('',#71096,#7685);
#3158=LINE('',#71098,#7686);
#3159=LINE('',#71100,#7687);
#3160=LINE('',#71102,#7688);
#3161=LINE('',#71104,#7689);
#3162=LINE('',#71106,#7690);
#3163=LINE('',#71108,#7691);
#3164=LINE('',#71110,#7692);
#3165=LINE('',#71116,#7693);
#3166=LINE('',#71118,#7694);
#3167=LINE('',#71120,#7695);
#3168=LINE('',#71122,#7696);
#3169=LINE('',#71124,#7697);
#3170=LINE('',#71126,#7698);
#3171=LINE('',#71128,#7699);
#3172=LINE('',#71130,#7700);
#3173=LINE('',#71132,#7701);
#3174=LINE('',#71134,#7702);
#3175=LINE('',#71136,#7703);
#3176=LINE('',#71138,#7704);
#3177=LINE('',#71140,#7705);
#3178=LINE('',#71142,#7706);
#3179=LINE('',#71143,#7707);
#3180=LINE('',#71146,#7708);
#3181=LINE('',#71148,#7709);
#3182=LINE('',#71155,#7710);
#3183=LINE('',#71158,#7711);
#3184=LINE('',#71160,#7712);
#3185=LINE('',#71162,#7713);
#3186=LINE('',#71164,#7714);
#3187=LINE('',#71166,#7715);
#3188=LINE('',#71168,#7716);
#3189=LINE('',#71170,#7717);
#3190=LINE('',#71172,#7718);
#3191=LINE('',#71174,#7719);
#3192=LINE('',#71176,#7720);
#3193=LINE('',#71178,#7721);
#3194=LINE('',#71180,#7722);
#3195=LINE('',#71182,#7723);
#3196=LINE('',#71184,#7724);
#3197=LINE('',#71186,#7725);
#3198=LINE('',#71192,#7726);
#3199=LINE('',#71194,#7727);
#3200=LINE('',#71196,#7728);
#3201=LINE('',#71198,#7729);
#3202=LINE('',#71200,#7730);
#3203=LINE('',#71202,#7731);
#3204=LINE('',#71204,#7732);
#3205=LINE('',#71206,#7733);
#3206=LINE('',#71208,#7734);
#3207=LINE('',#71210,#7735);
#3208=LINE('',#71212,#7736);
#3209=LINE('',#71214,#7737);
#3210=LINE('',#71216,#7738);
#3211=LINE('',#71218,#7739);
#3212=LINE('',#71219,#7740);
#3213=LINE('',#71222,#7741);
#3214=LINE('',#71224,#7742);
#3215=LINE('',#71231,#7743);
#3216=LINE('',#71234,#7744);
#3217=LINE('',#71236,#7745);
#3218=LINE('',#71238,#7746);
#3219=LINE('',#71240,#7747);
#3220=LINE('',#71242,#7748);
#3221=LINE('',#71244,#7749);
#3222=LINE('',#71246,#7750);
#3223=LINE('',#71248,#7751);
#3224=LINE('',#71250,#7752);
#3225=LINE('',#71252,#7753);
#3226=LINE('',#71254,#7754);
#3227=LINE('',#71256,#7755);
#3228=LINE('',#71258,#7756);
#3229=LINE('',#71260,#7757);
#3230=LINE('',#71262,#7758);
#3231=LINE('',#71268,#7759);
#3232=LINE('',#71270,#7760);
#3233=LINE('',#71272,#7761);
#3234=LINE('',#71274,#7762);
#3235=LINE('',#71276,#7763);
#3236=LINE('',#71278,#7764);
#3237=LINE('',#71280,#7765);
#3238=LINE('',#71282,#7766);
#3239=LINE('',#71284,#7767);
#3240=LINE('',#71286,#7768);
#3241=LINE('',#71288,#7769);
#3242=LINE('',#71290,#7770);
#3243=LINE('',#71292,#7771);
#3244=LINE('',#71294,#7772);
#3245=LINE('',#71295,#7773);
#3246=LINE('',#71298,#7774);
#3247=LINE('',#71300,#7775);
#3248=LINE('',#71307,#7776);
#3249=LINE('',#71310,#7777);
#3250=LINE('',#71312,#7778);
#3251=LINE('',#71314,#7779);
#3252=LINE('',#71316,#7780);
#3253=LINE('',#71318,#7781);
#3254=LINE('',#71320,#7782);
#3255=LINE('',#71322,#7783);
#3256=LINE('',#71324,#7784);
#3257=LINE('',#71326,#7785);
#3258=LINE('',#71328,#7786);
#3259=LINE('',#71330,#7787);
#3260=LINE('',#71332,#7788);
#3261=LINE('',#71334,#7789);
#3262=LINE('',#71336,#7790);
#3263=LINE('',#71338,#7791);
#3264=LINE('',#71344,#7792);
#3265=LINE('',#71346,#7793);
#3266=LINE('',#71348,#7794);
#3267=LINE('',#71350,#7795);
#3268=LINE('',#71352,#7796);
#3269=LINE('',#71354,#7797);
#3270=LINE('',#71356,#7798);
#3271=LINE('',#71358,#7799);
#3272=LINE('',#71360,#7800);
#3273=LINE('',#71362,#7801);
#3274=LINE('',#71364,#7802);
#3275=LINE('',#71366,#7803);
#3276=LINE('',#71368,#7804);
#3277=LINE('',#71370,#7805);
#3278=LINE('',#71371,#7806);
#3279=LINE('',#71374,#7807);
#3280=LINE('',#71376,#7808);
#3281=LINE('',#71383,#7809);
#3282=LINE('',#71386,#7810);
#3283=LINE('',#71388,#7811);
#3284=LINE('',#71390,#7812);
#3285=LINE('',#71392,#7813);
#3286=LINE('',#71394,#7814);
#3287=LINE('',#71396,#7815);
#3288=LINE('',#71398,#7816);
#3289=LINE('',#71400,#7817);
#3290=LINE('',#71402,#7818);
#3291=LINE('',#71404,#7819);
#3292=LINE('',#71406,#7820);
#3293=LINE('',#71408,#7821);
#3294=LINE('',#71410,#7822);
#3295=LINE('',#71412,#7823);
#3296=LINE('',#71414,#7824);
#3297=LINE('',#71420,#7825);
#3298=LINE('',#71422,#7826);
#3299=LINE('',#71424,#7827);
#3300=LINE('',#71426,#7828);
#3301=LINE('',#71428,#7829);
#3302=LINE('',#71430,#7830);
#3303=LINE('',#71432,#7831);
#3304=LINE('',#71434,#7832);
#3305=LINE('',#71436,#7833);
#3306=LINE('',#71438,#7834);
#3307=LINE('',#71440,#7835);
#3308=LINE('',#71442,#7836);
#3309=LINE('',#71444,#7837);
#3310=LINE('',#71446,#7838);
#3311=LINE('',#71447,#7839);
#3312=LINE('',#71450,#7840);
#3313=LINE('',#71452,#7841);
#3314=LINE('',#71459,#7842);
#3315=LINE('',#71462,#7843);
#3316=LINE('',#71464,#7844);
#3317=LINE('',#71466,#7845);
#3318=LINE('',#71468,#7846);
#3319=LINE('',#71470,#7847);
#3320=LINE('',#71472,#7848);
#3321=LINE('',#71474,#7849);
#3322=LINE('',#71476,#7850);
#3323=LINE('',#71478,#7851);
#3324=LINE('',#71480,#7852);
#3325=LINE('',#71482,#7853);
#3326=LINE('',#71484,#7854);
#3327=LINE('',#71486,#7855);
#3328=LINE('',#71488,#7856);
#3329=LINE('',#71490,#7857);
#3330=LINE('',#71496,#7858);
#3331=LINE('',#71498,#7859);
#3332=LINE('',#71500,#7860);
#3333=LINE('',#71502,#7861);
#3334=LINE('',#71504,#7862);
#3335=LINE('',#71506,#7863);
#3336=LINE('',#71508,#7864);
#3337=LINE('',#71510,#7865);
#3338=LINE('',#71512,#7866);
#3339=LINE('',#71514,#7867);
#3340=LINE('',#71516,#7868);
#3341=LINE('',#71518,#7869);
#3342=LINE('',#71520,#7870);
#3343=LINE('',#71522,#7871);
#3344=LINE('',#71523,#7872);
#3345=LINE('',#71526,#7873);
#3346=LINE('',#71528,#7874);
#3347=LINE('',#71535,#7875);
#3348=LINE('',#71898,#7876);
#3349=LINE('',#71900,#7877);
#3350=LINE('',#71907,#7878);
#3351=LINE('',#71910,#7879);
#3352=LINE('',#71912,#7880);
#3353=LINE('',#71919,#7881);
#3354=LINE('',#71922,#7882);
#3355=LINE('',#71924,#7883);
#3356=LINE('',#71931,#7884);
#3357=LINE('',#71934,#7885);
#3358=LINE('',#71936,#7886);
#3359=LINE('',#71943,#7887);
#3360=LINE('',#71946,#7888);
#3361=LINE('',#71948,#7889);
#3362=LINE('',#71955,#7890);
#3363=LINE('',#71958,#7891);
#3364=LINE('',#71960,#7892);
#3365=LINE('',#71967,#7893);
#3366=LINE('',#71970,#7894);
#3367=LINE('',#71972,#7895);
#3368=LINE('',#71979,#7896);
#3369=LINE('',#71982,#7897);
#3370=LINE('',#71984,#7898);
#3371=LINE('',#71991,#7899);
#3372=LINE('',#71994,#7900);
#3373=LINE('',#71996,#7901);
#3374=LINE('',#72003,#7902);
#3375=LINE('',#72006,#7903);
#3376=LINE('',#72008,#7904);
#3377=LINE('',#72015,#7905);
#3378=LINE('',#72018,#7906);
#3379=LINE('',#72020,#7907);
#3380=LINE('',#72027,#7908);
#3381=LINE('',#72030,#7909);
#3382=LINE('',#72032,#7910);
#3383=LINE('',#72039,#7911);
#3384=LINE('',#72042,#7912);
#3385=LINE('',#72044,#7913);
#3386=LINE('',#72051,#7914);
#3387=LINE('',#72054,#7915);
#3388=LINE('',#72056,#7916);
#3389=LINE('',#72063,#7917);
#3390=LINE('',#72066,#7918);
#3391=LINE('',#72068,#7919);
#3392=LINE('',#72075,#7920);
#3393=LINE('',#72078,#7921);
#3394=LINE('',#72080,#7922);
#3395=LINE('',#72087,#7923);
#3396=LINE('',#72090,#7924);
#3397=LINE('',#72092,#7925);
#3398=LINE('',#72099,#7926);
#3399=LINE('',#72102,#7927);
#3400=LINE('',#72104,#7928);
#3401=LINE('',#72111,#7929);
#3402=LINE('',#72114,#7930);
#3403=LINE('',#72116,#7931);
#3404=LINE('',#72123,#7932);
#3405=LINE('',#72126,#7933);
#3406=LINE('',#72128,#7934);
#3407=LINE('',#72135,#7935);
#3408=LINE('',#72138,#7936);
#3409=LINE('',#72140,#7937);
#3410=LINE('',#72147,#7938);
#3411=LINE('',#72150,#7939);
#3412=LINE('',#72152,#7940);
#3413=LINE('',#72159,#7941);
#3414=LINE('',#72162,#7942);
#3415=LINE('',#72164,#7943);
#3416=LINE('',#72171,#7944);
#3417=LINE('',#72174,#7945);
#3418=LINE('',#72176,#7946);
#3419=LINE('',#72183,#7947);
#3420=LINE('',#72186,#7948);
#3421=LINE('',#72188,#7949);
#3422=LINE('',#72195,#7950);
#3423=LINE('',#72198,#7951);
#3424=LINE('',#72200,#7952);
#3425=LINE('',#72207,#7953);
#3426=LINE('',#72210,#7954);
#3427=LINE('',#72212,#7955);
#3428=LINE('',#72219,#7956);
#3429=LINE('',#72222,#7957);
#3430=LINE('',#72224,#7958);
#3431=LINE('',#72231,#7959);
#3432=LINE('',#72234,#7960);
#3433=LINE('',#72236,#7961);
#3434=LINE('',#72243,#7962);
#3435=LINE('',#72246,#7963);
#3436=LINE('',#72248,#7964);
#3437=LINE('',#72255,#7965);
#3438=LINE('',#72258,#7966);
#3439=LINE('',#72260,#7967);
#3440=LINE('',#72267,#7968);
#3441=LINE('',#72270,#7969);
#3442=LINE('',#72272,#7970);
#3443=LINE('',#72279,#7971);
#3444=LINE('',#72282,#7972);
#3445=LINE('',#72284,#7973);
#3446=LINE('',#72291,#7974);
#3447=LINE('',#72294,#7975);
#3448=LINE('',#72296,#7976);
#3449=LINE('',#72303,#7977);
#3450=LINE('',#72306,#7978);
#3451=LINE('',#72308,#7979);
#3452=LINE('',#72315,#7980);
#3453=LINE('',#72318,#7981);
#3454=LINE('',#72320,#7982);
#3455=LINE('',#72327,#7983);
#3456=LINE('',#72330,#7984);
#3457=LINE('',#72331,#7985);
#3458=LINE('',#72334,#7986);
#3459=LINE('',#72335,#7987);
#3460=LINE('',#72338,#7988);
#3461=LINE('',#72339,#7989);
#3462=LINE('',#72342,#7990);
#3463=LINE('',#72343,#7991);
#3464=LINE('',#72346,#7992);
#3465=LINE('',#72347,#7993);
#3466=LINE('',#72350,#7994);
#3467=LINE('',#72351,#7995);
#3468=LINE('',#72354,#7996);
#3469=LINE('',#72355,#7997);
#3470=LINE('',#72358,#7998);
#3471=LINE('',#72359,#7999);
#3472=LINE('',#72362,#8000);
#3473=LINE('',#72363,#8001);
#3474=LINE('',#72366,#8002);
#3475=LINE('',#72367,#8003);
#3476=LINE('',#72370,#8004);
#3477=LINE('',#72371,#8005);
#3478=LINE('',#72374,#8006);
#3479=LINE('',#72375,#8007);
#3480=LINE('',#72378,#8008);
#3481=LINE('',#72379,#8009);
#3482=LINE('',#72382,#8010);
#3483=LINE('',#72383,#8011);
#3484=LINE('',#72386,#8012);
#3485=LINE('',#72387,#8013);
#3486=LINE('',#72390,#8014);
#3487=LINE('',#72391,#8015);
#3488=LINE('',#72394,#8016);
#3489=LINE('',#72395,#8017);
#3490=LINE('',#72398,#8018);
#3491=LINE('',#72399,#8019);
#3492=LINE('',#72402,#8020);
#3493=LINE('',#72403,#8021);
#3494=LINE('',#72406,#8022);
#3495=LINE('',#72407,#8023);
#3496=LINE('',#72410,#8024);
#3497=LINE('',#72411,#8025);
#3498=LINE('',#72414,#8026);
#3499=LINE('',#72415,#8027);
#3500=LINE('',#72418,#8028);
#3501=LINE('',#72419,#8029);
#3502=LINE('',#72422,#8030);
#3503=LINE('',#72423,#8031);
#3504=LINE('',#72426,#8032);
#3505=LINE('',#72427,#8033);
#3506=LINE('',#72430,#8034);
#3507=LINE('',#72431,#8035);
#3508=LINE('',#72434,#8036);
#3509=LINE('',#72435,#8037);
#3510=LINE('',#72438,#8038);
#3511=LINE('',#72439,#8039);
#3512=LINE('',#72442,#8040);
#3513=LINE('',#72443,#8041);
#3514=LINE('',#72446,#8042);
#3515=LINE('',#72447,#8043);
#3516=LINE('',#72450,#8044);
#3517=LINE('',#72451,#8045);
#3518=LINE('',#72454,#8046);
#3519=LINE('',#72455,#8047);
#3520=LINE('',#72458,#8048);
#3521=LINE('',#72459,#8049);
#3522=LINE('',#72462,#8050);
#3523=LINE('',#72463,#8051);
#3524=LINE('',#72466,#8052);
#3525=LINE('',#72467,#8053);
#3526=LINE('',#72470,#8054);
#3527=LINE('',#72471,#8055);
#3528=LINE('',#72474,#8056);
#3529=LINE('',#72481,#8057);
#3530=LINE('',#72484,#8058);
#3531=LINE('',#72491,#8059);
#3532=LINE('',#72494,#8060);
#3533=LINE('',#72501,#8061);
#3534=LINE('',#72504,#8062);
#3535=LINE('',#72511,#8063);
#3536=LINE('',#72514,#8064);
#3537=LINE('',#72521,#8065);
#3538=LINE('',#72524,#8066);
#3539=LINE('',#72531,#8067);
#3540=LINE('',#72534,#8068);
#3541=LINE('',#72541,#8069);
#3542=LINE('',#72544,#8070);
#3543=LINE('',#72551,#8071);
#3544=LINE('',#72554,#8072);
#3545=LINE('',#72561,#8073);
#3546=LINE('',#72564,#8074);
#3547=LINE('',#72571,#8075);
#3548=LINE('',#72574,#8076);
#3549=LINE('',#72581,#8077);
#3550=LINE('',#72584,#8078);
#3551=LINE('',#72591,#8079);
#3552=LINE('',#72594,#8080);
#3553=LINE('',#72601,#8081);
#3554=LINE('',#72604,#8082);
#3555=LINE('',#72611,#8083);
#3556=LINE('',#72614,#8084);
#3557=LINE('',#72621,#8085);
#3558=LINE('',#72624,#8086);
#3559=LINE('',#72631,#8087);
#3560=LINE('',#72634,#8088);
#3561=LINE('',#72641,#8089);
#3562=LINE('',#72644,#8090);
#3563=LINE('',#72651,#8091);
#3564=LINE('',#72654,#8092);
#3565=LINE('',#72661,#8093);
#3566=LINE('',#72664,#8094);
#3567=LINE('',#72671,#8095);
#3568=LINE('',#72674,#8096);
#3569=LINE('',#72681,#8097);
#3570=LINE('',#72684,#8098);
#3571=LINE('',#72691,#8099);
#3572=LINE('',#72694,#8100);
#3573=LINE('',#72701,#8101);
#3574=LINE('',#72704,#8102);
#3575=LINE('',#72711,#8103);
#3576=LINE('',#72714,#8104);
#3577=LINE('',#72721,#8105);
#3578=LINE('',#72724,#8106);
#3579=LINE('',#72731,#8107);
#3580=LINE('',#72734,#8108);
#3581=LINE('',#72741,#8109);
#3582=LINE('',#72744,#8110);
#3583=LINE('',#72751,#8111);
#3584=LINE('',#72754,#8112);
#3585=LINE('',#72761,#8113);
#3586=LINE('',#72764,#8114);
#3587=LINE('',#72771,#8115);
#3588=LINE('',#72774,#8116);
#3589=LINE('',#72781,#8117);
#3590=LINE('',#72784,#8118);
#3591=LINE('',#72791,#8119);
#3592=LINE('',#72794,#8120);
#3593=LINE('',#72801,#8121);
#3594=LINE('',#72804,#8122);
#3595=LINE('',#72811,#8123);
#3596=LINE('',#72814,#8124);
#3597=LINE('',#72821,#8125);
#3598=LINE('',#72824,#8126);
#3599=LINE('',#72830,#8127);
#3600=LINE('',#72831,#8128);
#3601=LINE('',#72834,#8129);
#3602=LINE('',#72835,#8130);
#3603=LINE('',#72838,#8131);
#3604=LINE('',#72839,#8132);
#3605=LINE('',#72842,#8133);
#3606=LINE('',#72843,#8134);
#3607=LINE('',#72846,#8135);
#3608=LINE('',#72847,#8136);
#3609=LINE('',#72850,#8137);
#3610=LINE('',#72851,#8138);
#3611=LINE('',#72854,#8139);
#3612=LINE('',#72855,#8140);
#3613=LINE('',#72858,#8141);
#3614=LINE('',#72859,#8142);
#3615=LINE('',#72862,#8143);
#3616=LINE('',#72863,#8144);
#3617=LINE('',#72866,#8145);
#3618=LINE('',#72867,#8146);
#3619=LINE('',#72870,#8147);
#3620=LINE('',#72871,#8148);
#3621=LINE('',#72874,#8149);
#3622=LINE('',#72875,#8150);
#3623=LINE('',#72878,#8151);
#3624=LINE('',#72879,#8152);
#3625=LINE('',#72882,#8153);
#3626=LINE('',#72883,#8154);
#3627=LINE('',#72886,#8155);
#3628=LINE('',#72887,#8156);
#3629=LINE('',#72890,#8157);
#3630=LINE('',#72891,#8158);
#3631=LINE('',#72894,#8159);
#3632=LINE('',#72895,#8160);
#3633=LINE('',#72898,#8161);
#3634=LINE('',#72899,#8162);
#3635=LINE('',#72902,#8163);
#3636=LINE('',#72903,#8164);
#3637=LINE('',#72906,#8165);
#3638=LINE('',#72907,#8166);
#3639=LINE('',#72910,#8167);
#3640=LINE('',#72911,#8168);
#3641=LINE('',#72914,#8169);
#3642=LINE('',#72915,#8170);
#3643=LINE('',#72918,#8171);
#3644=LINE('',#72919,#8172);
#3645=LINE('',#72922,#8173);
#3646=LINE('',#72923,#8174);
#3647=LINE('',#72926,#8175);
#3648=LINE('',#72927,#8176);
#3649=LINE('',#72930,#8177);
#3650=LINE('',#72931,#8178);
#3651=LINE('',#72934,#8179);
#3652=LINE('',#72935,#8180);
#3653=LINE('',#72938,#8181);
#3654=LINE('',#72939,#8182);
#3655=LINE('',#72942,#8183);
#3656=LINE('',#72943,#8184);
#3657=LINE('',#72946,#8185);
#3658=LINE('',#72947,#8186);
#3659=LINE('',#72950,#8187);
#3660=LINE('',#72951,#8188);
#3661=LINE('',#72954,#8189);
#3662=LINE('',#72955,#8190);
#3663=LINE('',#72958,#8191);
#3664=LINE('',#72959,#8192);
#3665=LINE('',#72962,#8193);
#3666=LINE('',#72963,#8194);
#3667=LINE('',#72966,#8195);
#3668=LINE('',#72967,#8196);
#3669=LINE('',#72970,#8197);
#3670=LINE('',#72971,#8198);
#3671=LINE('',#72974,#8199);
#3672=LINE('',#72980,#8200);
#3673=LINE('',#72986,#8201);
#3674=LINE('',#72992,#8202);
#3675=LINE('',#72998,#8203);
#3676=LINE('',#73004,#8204);
#3677=LINE('',#73010,#8205);
#3678=LINE('',#73016,#8206);
#3679=LINE('',#73022,#8207);
#3680=LINE('',#73028,#8208);
#3681=LINE('',#73034,#8209);
#3682=LINE('',#73040,#8210);
#3683=LINE('',#73046,#8211);
#3684=LINE('',#73052,#8212);
#3685=LINE('',#73058,#8213);
#3686=LINE('',#73064,#8214);
#3687=LINE('',#73070,#8215);
#3688=LINE('',#73076,#8216);
#3689=LINE('',#73086,#8217);
#3690=LINE('',#73092,#8218);
#3691=LINE('',#73098,#8219);
#3692=LINE('',#73104,#8220);
#3693=LINE('',#73110,#8221);
#3694=LINE('',#73116,#8222);
#3695=LINE('',#73122,#8223);
#3696=LINE('',#73128,#8224);
#3697=LINE('',#73134,#8225);
#3698=LINE('',#73140,#8226);
#3699=LINE('',#73146,#8227);
#3700=LINE('',#73152,#8228);
#3701=LINE('',#73158,#8229);
#3702=LINE('',#73164,#8230);
#3703=LINE('',#73170,#8231);
#3704=LINE('',#73176,#8232);
#3705=LINE('',#73182,#8233);
#3706=LINE('',#73188,#8234);
#3707=LINE('',#73194,#8235);
#3708=LINE('',#73195,#8236);
#3709=LINE('',#73199,#8237);
#3710=LINE('',#73203,#8238);
#3711=LINE('',#73207,#8239);
#3712=LINE('',#73211,#8240);
#3713=LINE('',#73215,#8241);
#3714=LINE('',#73218,#8242);
#3715=LINE('',#73219,#8243);
#3716=LINE('',#73223,#8244);
#3717=LINE('',#73227,#8245);
#3718=LINE('',#73231,#8246);
#3719=LINE('',#73235,#8247);
#3720=LINE('',#73239,#8248);
#3721=LINE('',#73242,#8249);
#3722=LINE('',#73243,#8250);
#3723=LINE('',#73252,#8251);
#3724=LINE('',#73253,#8252);
#3725=LINE('',#73257,#8253);
#3726=LINE('',#73261,#8254);
#3727=LINE('',#73265,#8255);
#3728=LINE('',#73269,#8256);
#3729=LINE('',#73273,#8257);
#3730=LINE('',#73276,#8258);
#3731=LINE('',#73277,#8259);
#3732=LINE('',#73281,#8260);
#3733=LINE('',#73285,#8261);
#3734=LINE('',#73289,#8262);
#3735=LINE('',#73293,#8263);
#3736=LINE('',#73297,#8264);
#3737=LINE('',#73299,#8265);
#3738=LINE('',#73308,#8266);
#3739=LINE('',#73460,#8267);
#3740=LINE('',#73472,#8268);
#3741=LINE('',#73483,#8269);
#3742=LINE('',#73485,#8270);
#3743=LINE('',#73487,#8271);
#3744=LINE('',#73489,#8272);
#3745=LINE('',#73491,#8273);
#3746=LINE('',#73493,#8274);
#3747=LINE('',#73495,#8275);
#3748=LINE('',#73497,#8276);
#3749=LINE('',#73499,#8277);
#3750=LINE('',#73501,#8278);
#3751=LINE('',#73503,#8279);
#3752=LINE('',#73505,#8280);
#3753=LINE('',#73507,#8281);
#3754=LINE('',#73509,#8282);
#3755=LINE('',#73516,#8283);
#3756=LINE('',#73517,#8284);
#3757=LINE('',#73521,#8285);
#3758=LINE('',#73525,#8286);
#3759=LINE('',#73529,#8287);
#3760=LINE('',#73533,#8288);
#3761=LINE('',#73537,#8289);
#3762=LINE('',#73540,#8290);
#3763=LINE('',#73541,#8291);
#3764=LINE('',#73545,#8292);
#3765=LINE('',#73549,#8293);
#3766=LINE('',#73553,#8294);
#3767=LINE('',#73557,#8295);
#3768=LINE('',#73561,#8296);
#3769=LINE('',#73563,#8297);
#3770=LINE('',#73571,#8298);
#3771=LINE('',#73583,#8299);
#3772=LINE('',#73594,#8300);
#3773=LINE('',#73596,#8301);
#3774=LINE('',#73598,#8302);
#3775=LINE('',#73600,#8303);
#3776=LINE('',#73602,#8304);
#3777=LINE('',#73604,#8305);
#3778=LINE('',#73606,#8306);
#3779=LINE('',#73608,#8307);
#3780=LINE('',#73610,#8308);
#3781=LINE('',#73612,#8309);
#3782=LINE('',#73614,#8310);
#3783=LINE('',#73616,#8311);
#3784=LINE('',#73618,#8312);
#3785=LINE('',#73620,#8313);
#3786=LINE('',#73627,#8314);
#3787=LINE('',#73628,#8315);
#3788=LINE('',#73632,#8316);
#3789=LINE('',#73636,#8317);
#3790=LINE('',#73640,#8318);
#3791=LINE('',#73644,#8319);
#3792=LINE('',#73648,#8320);
#3793=LINE('',#73651,#8321);
#3794=LINE('',#73652,#8322);
#3795=LINE('',#73656,#8323);
#3796=LINE('',#73660,#8324);
#3797=LINE('',#73664,#8325);
#3798=LINE('',#73668,#8326);
#3799=LINE('',#73672,#8327);
#3800=LINE('',#73674,#8328);
#3801=LINE('',#73682,#8329);
#3802=LINE('',#73694,#8330);
#3803=LINE('',#73705,#8331);
#3804=LINE('',#73707,#8332);
#3805=LINE('',#73709,#8333);
#3806=LINE('',#73711,#8334);
#3807=LINE('',#73713,#8335);
#3808=LINE('',#73715,#8336);
#3809=LINE('',#73717,#8337);
#3810=LINE('',#73719,#8338);
#3811=LINE('',#73721,#8339);
#3812=LINE('',#73723,#8340);
#3813=LINE('',#73725,#8341);
#3814=LINE('',#73727,#8342);
#3815=LINE('',#73729,#8343);
#3816=LINE('',#73731,#8344);
#3817=LINE('',#73738,#8345);
#3818=LINE('',#73739,#8346);
#3819=LINE('',#73743,#8347);
#3820=LINE('',#73747,#8348);
#3821=LINE('',#73751,#8349);
#3822=LINE('',#73755,#8350);
#3823=LINE('',#73759,#8351);
#3824=LINE('',#73762,#8352);
#3825=LINE('',#73763,#8353);
#3826=LINE('',#73767,#8354);
#3827=LINE('',#73771,#8355);
#3828=LINE('',#73775,#8356);
#3829=LINE('',#73779,#8357);
#3830=LINE('',#73783,#8358);
#3831=LINE('',#73785,#8359);
#3832=LINE('',#73793,#8360);
#3833=LINE('',#73805,#8361);
#3834=LINE('',#73816,#8362);
#3835=LINE('',#73818,#8363);
#3836=LINE('',#73820,#8364);
#3837=LINE('',#73822,#8365);
#3838=LINE('',#73824,#8366);
#3839=LINE('',#73826,#8367);
#3840=LINE('',#73828,#8368);
#3841=LINE('',#73830,#8369);
#3842=LINE('',#73832,#8370);
#3843=LINE('',#73834,#8371);
#3844=LINE('',#73836,#8372);
#3845=LINE('',#73838,#8373);
#3846=LINE('',#73840,#8374);
#3847=LINE('',#73842,#8375);
#3848=LINE('',#73849,#8376);
#3849=LINE('',#73850,#8377);
#3850=LINE('',#73854,#8378);
#3851=LINE('',#73858,#8379);
#3852=LINE('',#73862,#8380);
#3853=LINE('',#73866,#8381);
#3854=LINE('',#73870,#8382);
#3855=LINE('',#73873,#8383);
#3856=LINE('',#73874,#8384);
#3857=LINE('',#73878,#8385);
#3858=LINE('',#73882,#8386);
#3859=LINE('',#73886,#8387);
#3860=LINE('',#73890,#8388);
#3861=LINE('',#73894,#8389);
#3862=LINE('',#73896,#8390);
#3863=LINE('',#73904,#8391);
#3864=LINE('',#73916,#8392);
#3865=LINE('',#73927,#8393);
#3866=LINE('',#73929,#8394);
#3867=LINE('',#73931,#8395);
#3868=LINE('',#73933,#8396);
#3869=LINE('',#73935,#8397);
#3870=LINE('',#73937,#8398);
#3871=LINE('',#73939,#8399);
#3872=LINE('',#73941,#8400);
#3873=LINE('',#73943,#8401);
#3874=LINE('',#73945,#8402);
#3875=LINE('',#73947,#8403);
#3876=LINE('',#73949,#8404);
#3877=LINE('',#73951,#8405);
#3878=LINE('',#73953,#8406);
#3879=LINE('',#73960,#8407);
#3880=LINE('',#73961,#8408);
#3881=LINE('',#73965,#8409);
#3882=LINE('',#73969,#8410);
#3883=LINE('',#73973,#8411);
#3884=LINE('',#73977,#8412);
#3885=LINE('',#73981,#8413);
#3886=LINE('',#73984,#8414);
#3887=LINE('',#73985,#8415);
#3888=LINE('',#73989,#8416);
#3889=LINE('',#73993,#8417);
#3890=LINE('',#73997,#8418);
#3891=LINE('',#74001,#8419);
#3892=LINE('',#74005,#8420);
#3893=LINE('',#74007,#8421);
#3894=LINE('',#74015,#8422);
#3895=LINE('',#74027,#8423);
#3896=LINE('',#74038,#8424);
#3897=LINE('',#74040,#8425);
#3898=LINE('',#74042,#8426);
#3899=LINE('',#74044,#8427);
#3900=LINE('',#74046,#8428);
#3901=LINE('',#74048,#8429);
#3902=LINE('',#74050,#8430);
#3903=LINE('',#74052,#8431);
#3904=LINE('',#74054,#8432);
#3905=LINE('',#74056,#8433);
#3906=LINE('',#74058,#8434);
#3907=LINE('',#74060,#8435);
#3908=LINE('',#74062,#8436);
#3909=LINE('',#74064,#8437);
#3910=LINE('',#74071,#8438);
#3911=LINE('',#74072,#8439);
#3912=LINE('',#74076,#8440);
#3913=LINE('',#74080,#8441);
#3914=LINE('',#74084,#8442);
#3915=LINE('',#74088,#8443);
#3916=LINE('',#74092,#8444);
#3917=LINE('',#74095,#8445);
#3918=LINE('',#74096,#8446);
#3919=LINE('',#74100,#8447);
#3920=LINE('',#74104,#8448);
#3921=LINE('',#74108,#8449);
#3922=LINE('',#74112,#8450);
#3923=LINE('',#74116,#8451);
#3924=LINE('',#74118,#8452);
#3925=LINE('',#74126,#8453);
#3926=LINE('',#74138,#8454);
#3927=LINE('',#74149,#8455);
#3928=LINE('',#74151,#8456);
#3929=LINE('',#74153,#8457);
#3930=LINE('',#74155,#8458);
#3931=LINE('',#74157,#8459);
#3932=LINE('',#74159,#8460);
#3933=LINE('',#74161,#8461);
#3934=LINE('',#74163,#8462);
#3935=LINE('',#74165,#8463);
#3936=LINE('',#74167,#8464);
#3937=LINE('',#74169,#8465);
#3938=LINE('',#74171,#8466);
#3939=LINE('',#74173,#8467);
#3940=LINE('',#74175,#8468);
#3941=LINE('',#74182,#8469);
#3942=LINE('',#74183,#8470);
#3943=LINE('',#74187,#8471);
#3944=LINE('',#74191,#8472);
#3945=LINE('',#74195,#8473);
#3946=LINE('',#74199,#8474);
#3947=LINE('',#74203,#8475);
#3948=LINE('',#74206,#8476);
#3949=LINE('',#74207,#8477);
#3950=LINE('',#74211,#8478);
#3951=LINE('',#74215,#8479);
#3952=LINE('',#74219,#8480);
#3953=LINE('',#74223,#8481);
#3954=LINE('',#74227,#8482);
#3955=LINE('',#74229,#8483);
#3956=LINE('',#74237,#8484);
#3957=LINE('',#74249,#8485);
#3958=LINE('',#74260,#8486);
#3959=LINE('',#74262,#8487);
#3960=LINE('',#74264,#8488);
#3961=LINE('',#74266,#8489);
#3962=LINE('',#74268,#8490);
#3963=LINE('',#74270,#8491);
#3964=LINE('',#74272,#8492);
#3965=LINE('',#74274,#8493);
#3966=LINE('',#74276,#8494);
#3967=LINE('',#74278,#8495);
#3968=LINE('',#74280,#8496);
#3969=LINE('',#74282,#8497);
#3970=LINE('',#74284,#8498);
#3971=LINE('',#74286,#8499);
#3972=LINE('',#74293,#8500);
#3973=LINE('',#74294,#8501);
#3974=LINE('',#74298,#8502);
#3975=LINE('',#74302,#8503);
#3976=LINE('',#74306,#8504);
#3977=LINE('',#74310,#8505);
#3978=LINE('',#74314,#8506);
#3979=LINE('',#74317,#8507);
#3980=LINE('',#74318,#8508);
#3981=LINE('',#74322,#8509);
#3982=LINE('',#74326,#8510);
#3983=LINE('',#74330,#8511);
#3984=LINE('',#74334,#8512);
#3985=LINE('',#74338,#8513);
#3986=LINE('',#74340,#8514);
#3987=LINE('',#74348,#8515);
#3988=LINE('',#74360,#8516);
#3989=LINE('',#74371,#8517);
#3990=LINE('',#74373,#8518);
#3991=LINE('',#74375,#8519);
#3992=LINE('',#74377,#8520);
#3993=LINE('',#74379,#8521);
#3994=LINE('',#74381,#8522);
#3995=LINE('',#74383,#8523);
#3996=LINE('',#74385,#8524);
#3997=LINE('',#74387,#8525);
#3998=LINE('',#74389,#8526);
#3999=LINE('',#74391,#8527);
#4000=LINE('',#74393,#8528);
#4001=LINE('',#74395,#8529);
#4002=LINE('',#74397,#8530);
#4003=LINE('',#74404,#8531);
#4004=LINE('',#74405,#8532);
#4005=LINE('',#74409,#8533);
#4006=LINE('',#74413,#8534);
#4007=LINE('',#74417,#8535);
#4008=LINE('',#74421,#8536);
#4009=LINE('',#74425,#8537);
#4010=LINE('',#74428,#8538);
#4011=LINE('',#74429,#8539);
#4012=LINE('',#74433,#8540);
#4013=LINE('',#74437,#8541);
#4014=LINE('',#74441,#8542);
#4015=LINE('',#74445,#8543);
#4016=LINE('',#74449,#8544);
#4017=LINE('',#74451,#8545);
#4018=LINE('',#74459,#8546);
#4019=LINE('',#74471,#8547);
#4020=LINE('',#74482,#8548);
#4021=LINE('',#74484,#8549);
#4022=LINE('',#74486,#8550);
#4023=LINE('',#74488,#8551);
#4024=LINE('',#74490,#8552);
#4025=LINE('',#74492,#8553);
#4026=LINE('',#74494,#8554);
#4027=LINE('',#74496,#8555);
#4028=LINE('',#74498,#8556);
#4029=LINE('',#74500,#8557);
#4030=LINE('',#74502,#8558);
#4031=LINE('',#74504,#8559);
#4032=LINE('',#74506,#8560);
#4033=LINE('',#74508,#8561);
#4034=LINE('',#74515,#8562);
#4035=LINE('',#74516,#8563);
#4036=LINE('',#74520,#8564);
#4037=LINE('',#74524,#8565);
#4038=LINE('',#74528,#8566);
#4039=LINE('',#74532,#8567);
#4040=LINE('',#74536,#8568);
#4041=LINE('',#74539,#8569);
#4042=LINE('',#74540,#8570);
#4043=LINE('',#74544,#8571);
#4044=LINE('',#74548,#8572);
#4045=LINE('',#74552,#8573);
#4046=LINE('',#74556,#8574);
#4047=LINE('',#74560,#8575);
#4048=LINE('',#74562,#8576);
#4049=LINE('',#74570,#8577);
#4050=LINE('',#74582,#8578);
#4051=LINE('',#74593,#8579);
#4052=LINE('',#74595,#8580);
#4053=LINE('',#74597,#8581);
#4054=LINE('',#74599,#8582);
#4055=LINE('',#74601,#8583);
#4056=LINE('',#74603,#8584);
#4057=LINE('',#74605,#8585);
#4058=LINE('',#74607,#8586);
#4059=LINE('',#74609,#8587);
#4060=LINE('',#74611,#8588);
#4061=LINE('',#74613,#8589);
#4062=LINE('',#74615,#8590);
#4063=LINE('',#74617,#8591);
#4064=LINE('',#74619,#8592);
#4065=LINE('',#74626,#8593);
#4066=LINE('',#74627,#8594);
#4067=LINE('',#74631,#8595);
#4068=LINE('',#74635,#8596);
#4069=LINE('',#74639,#8597);
#4070=LINE('',#74643,#8598);
#4071=LINE('',#74647,#8599);
#4072=LINE('',#74650,#8600);
#4073=LINE('',#74651,#8601);
#4074=LINE('',#74655,#8602);
#4075=LINE('',#74659,#8603);
#4076=LINE('',#74663,#8604);
#4077=LINE('',#74667,#8605);
#4078=LINE('',#74671,#8606);
#4079=LINE('',#74673,#8607);
#4080=LINE('',#74681,#8608);
#4081=LINE('',#74693,#8609);
#4082=LINE('',#74704,#8610);
#4083=LINE('',#74706,#8611);
#4084=LINE('',#74708,#8612);
#4085=LINE('',#74710,#8613);
#4086=LINE('',#74712,#8614);
#4087=LINE('',#74714,#8615);
#4088=LINE('',#74716,#8616);
#4089=LINE('',#74718,#8617);
#4090=LINE('',#74720,#8618);
#4091=LINE('',#74722,#8619);
#4092=LINE('',#74724,#8620);
#4093=LINE('',#74726,#8621);
#4094=LINE('',#74728,#8622);
#4095=LINE('',#74730,#8623);
#4096=LINE('',#74737,#8624);
#4097=LINE('',#74738,#8625);
#4098=LINE('',#74742,#8626);
#4099=LINE('',#74746,#8627);
#4100=LINE('',#74750,#8628);
#4101=LINE('',#74754,#8629);
#4102=LINE('',#74758,#8630);
#4103=LINE('',#74761,#8631);
#4104=LINE('',#74762,#8632);
#4105=LINE('',#74766,#8633);
#4106=LINE('',#74770,#8634);
#4107=LINE('',#74774,#8635);
#4108=LINE('',#74778,#8636);
#4109=LINE('',#74782,#8637);
#4110=LINE('',#74784,#8638);
#4111=LINE('',#74792,#8639);
#4112=LINE('',#74804,#8640);
#4113=LINE('',#74815,#8641);
#4114=LINE('',#74817,#8642);
#4115=LINE('',#74819,#8643);
#4116=LINE('',#74821,#8644);
#4117=LINE('',#74823,#8645);
#4118=LINE('',#74825,#8646);
#4119=LINE('',#74827,#8647);
#4120=LINE('',#74829,#8648);
#4121=LINE('',#74831,#8649);
#4122=LINE('',#74833,#8650);
#4123=LINE('',#74835,#8651);
#4124=LINE('',#74837,#8652);
#4125=LINE('',#74839,#8653);
#4126=LINE('',#74841,#8654);
#4127=LINE('',#74848,#8655);
#4128=LINE('',#74849,#8656);
#4129=LINE('',#74853,#8657);
#4130=LINE('',#74857,#8658);
#4131=LINE('',#74861,#8659);
#4132=LINE('',#74865,#8660);
#4133=LINE('',#74869,#8661);
#4134=LINE('',#74872,#8662);
#4135=LINE('',#74873,#8663);
#4136=LINE('',#74877,#8664);
#4137=LINE('',#74881,#8665);
#4138=LINE('',#74885,#8666);
#4139=LINE('',#74889,#8667);
#4140=LINE('',#74893,#8668);
#4141=LINE('',#74895,#8669);
#4142=LINE('',#74903,#8670);
#4143=LINE('',#74915,#8671);
#4144=LINE('',#74926,#8672);
#4145=LINE('',#74928,#8673);
#4146=LINE('',#74930,#8674);
#4147=LINE('',#74932,#8675);
#4148=LINE('',#74934,#8676);
#4149=LINE('',#74936,#8677);
#4150=LINE('',#74938,#8678);
#4151=LINE('',#74940,#8679);
#4152=LINE('',#74942,#8680);
#4153=LINE('',#74944,#8681);
#4154=LINE('',#74946,#8682);
#4155=LINE('',#74948,#8683);
#4156=LINE('',#74950,#8684);
#4157=LINE('',#74952,#8685);
#4158=LINE('',#74959,#8686);
#4159=LINE('',#74960,#8687);
#4160=LINE('',#74964,#8688);
#4161=LINE('',#74968,#8689);
#4162=LINE('',#74972,#8690);
#4163=LINE('',#74976,#8691);
#4164=LINE('',#74980,#8692);
#4165=LINE('',#74983,#8693);
#4166=LINE('',#74984,#8694);
#4167=LINE('',#74988,#8695);
#4168=LINE('',#74992,#8696);
#4169=LINE('',#74996,#8697);
#4170=LINE('',#75000,#8698);
#4171=LINE('',#75004,#8699);
#4172=LINE('',#75006,#8700);
#4173=LINE('',#75014,#8701);
#4174=LINE('',#75026,#8702);
#4175=LINE('',#75037,#8703);
#4176=LINE('',#75039,#8704);
#4177=LINE('',#75041,#8705);
#4178=LINE('',#75043,#8706);
#4179=LINE('',#75045,#8707);
#4180=LINE('',#75047,#8708);
#4181=LINE('',#75049,#8709);
#4182=LINE('',#75051,#8710);
#4183=LINE('',#75053,#8711);
#4184=LINE('',#75055,#8712);
#4185=LINE('',#75057,#8713);
#4186=LINE('',#75059,#8714);
#4187=LINE('',#75061,#8715);
#4188=LINE('',#75063,#8716);
#4189=LINE('',#75070,#8717);
#4190=LINE('',#75071,#8718);
#4191=LINE('',#75075,#8719);
#4192=LINE('',#75079,#8720);
#4193=LINE('',#75083,#8721);
#4194=LINE('',#75087,#8722);
#4195=LINE('',#75091,#8723);
#4196=LINE('',#75094,#8724);
#4197=LINE('',#75095,#8725);
#4198=LINE('',#75099,#8726);
#4199=LINE('',#75103,#8727);
#4200=LINE('',#75107,#8728);
#4201=LINE('',#75111,#8729);
#4202=LINE('',#75115,#8730);
#4203=LINE('',#75117,#8731);
#4204=LINE('',#75125,#8732);
#4205=LINE('',#75137,#8733);
#4206=LINE('',#75148,#8734);
#4207=LINE('',#75150,#8735);
#4208=LINE('',#75152,#8736);
#4209=LINE('',#75154,#8737);
#4210=LINE('',#75156,#8738);
#4211=LINE('',#75158,#8739);
#4212=LINE('',#75160,#8740);
#4213=LINE('',#75162,#8741);
#4214=LINE('',#75164,#8742);
#4215=LINE('',#75166,#8743);
#4216=LINE('',#75168,#8744);
#4217=LINE('',#75170,#8745);
#4218=LINE('',#75172,#8746);
#4219=LINE('',#75174,#8747);
#4220=LINE('',#75181,#8748);
#4221=LINE('',#75182,#8749);
#4222=LINE('',#75186,#8750);
#4223=LINE('',#75190,#8751);
#4224=LINE('',#75194,#8752);
#4225=LINE('',#75198,#8753);
#4226=LINE('',#75202,#8754);
#4227=LINE('',#75205,#8755);
#4228=LINE('',#75206,#8756);
#4229=LINE('',#75210,#8757);
#4230=LINE('',#75214,#8758);
#4231=LINE('',#75218,#8759);
#4232=LINE('',#75222,#8760);
#4233=LINE('',#75226,#8761);
#4234=LINE('',#75228,#8762);
#4235=LINE('',#75236,#8763);
#4236=LINE('',#75248,#8764);
#4237=LINE('',#75259,#8765);
#4238=LINE('',#75261,#8766);
#4239=LINE('',#75263,#8767);
#4240=LINE('',#75265,#8768);
#4241=LINE('',#75267,#8769);
#4242=LINE('',#75269,#8770);
#4243=LINE('',#75271,#8771);
#4244=LINE('',#75273,#8772);
#4245=LINE('',#75275,#8773);
#4246=LINE('',#75277,#8774);
#4247=LINE('',#75279,#8775);
#4248=LINE('',#75281,#8776);
#4249=LINE('',#75283,#8777);
#4250=LINE('',#75285,#8778);
#4251=LINE('',#75292,#8779);
#4252=LINE('',#75293,#8780);
#4253=LINE('',#75297,#8781);
#4254=LINE('',#75301,#8782);
#4255=LINE('',#75305,#8783);
#4256=LINE('',#75309,#8784);
#4257=LINE('',#75313,#8785);
#4258=LINE('',#75316,#8786);
#4259=LINE('',#75317,#8787);
#4260=LINE('',#75321,#8788);
#4261=LINE('',#75325,#8789);
#4262=LINE('',#75329,#8790);
#4263=LINE('',#75333,#8791);
#4264=LINE('',#75337,#8792);
#4265=LINE('',#75339,#8793);
#4266=LINE('',#75347,#8794);
#4267=LINE('',#75359,#8795);
#4268=LINE('',#75370,#8796);
#4269=LINE('',#75372,#8797);
#4270=LINE('',#75374,#8798);
#4271=LINE('',#75376,#8799);
#4272=LINE('',#75378,#8800);
#4273=LINE('',#75380,#8801);
#4274=LINE('',#75382,#8802);
#4275=LINE('',#75384,#8803);
#4276=LINE('',#75386,#8804);
#4277=LINE('',#75388,#8805);
#4278=LINE('',#75390,#8806);
#4279=LINE('',#75392,#8807);
#4280=LINE('',#75394,#8808);
#4281=LINE('',#75396,#8809);
#4282=LINE('',#75403,#8810);
#4283=LINE('',#75404,#8811);
#4284=LINE('',#75408,#8812);
#4285=LINE('',#75412,#8813);
#4286=LINE('',#75416,#8814);
#4287=LINE('',#75420,#8815);
#4288=LINE('',#75424,#8816);
#4289=LINE('',#75427,#8817);
#4290=LINE('',#75428,#8818);
#4291=LINE('',#75432,#8819);
#4292=LINE('',#75436,#8820);
#4293=LINE('',#75440,#8821);
#4294=LINE('',#75444,#8822);
#4295=LINE('',#75448,#8823);
#4296=LINE('',#75450,#8824);
#4297=LINE('',#75458,#8825);
#4298=LINE('',#75470,#8826);
#4299=LINE('',#75481,#8827);
#4300=LINE('',#75483,#8828);
#4301=LINE('',#75485,#8829);
#4302=LINE('',#75487,#8830);
#4303=LINE('',#75489,#8831);
#4304=LINE('',#75491,#8832);
#4305=LINE('',#75493,#8833);
#4306=LINE('',#75495,#8834);
#4307=LINE('',#75497,#8835);
#4308=LINE('',#75499,#8836);
#4309=LINE('',#75501,#8837);
#4310=LINE('',#75503,#8838);
#4311=LINE('',#75505,#8839);
#4312=LINE('',#75507,#8840);
#4313=LINE('',#75514,#8841);
#4314=LINE('',#75515,#8842);
#4315=LINE('',#75519,#8843);
#4316=LINE('',#75523,#8844);
#4317=LINE('',#75527,#8845);
#4318=LINE('',#75531,#8846);
#4319=LINE('',#75535,#8847);
#4320=LINE('',#75538,#8848);
#4321=LINE('',#75539,#8849);
#4322=LINE('',#75543,#8850);
#4323=LINE('',#75547,#8851);
#4324=LINE('',#75551,#8852);
#4325=LINE('',#75555,#8853);
#4326=LINE('',#75559,#8854);
#4327=LINE('',#75561,#8855);
#4328=LINE('',#75569,#8856);
#4329=LINE('',#75581,#8857);
#4330=LINE('',#75592,#8858);
#4331=LINE('',#75594,#8859);
#4332=LINE('',#75596,#8860);
#4333=LINE('',#75598,#8861);
#4334=LINE('',#75600,#8862);
#4335=LINE('',#75602,#8863);
#4336=LINE('',#75604,#8864);
#4337=LINE('',#75606,#8865);
#4338=LINE('',#75608,#8866);
#4339=LINE('',#75610,#8867);
#4340=LINE('',#75612,#8868);
#4341=LINE('',#75614,#8869);
#4342=LINE('',#75616,#8870);
#4343=LINE('',#75618,#8871);
#4344=LINE('',#75625,#8872);
#4345=LINE('',#75626,#8873);
#4346=LINE('',#75630,#8874);
#4347=LINE('',#75634,#8875);
#4348=LINE('',#75638,#8876);
#4349=LINE('',#75642,#8877);
#4350=LINE('',#75646,#8878);
#4351=LINE('',#75649,#8879);
#4352=LINE('',#75650,#8880);
#4353=LINE('',#75654,#8881);
#4354=LINE('',#75658,#8882);
#4355=LINE('',#75662,#8883);
#4356=LINE('',#75666,#8884);
#4357=LINE('',#75670,#8885);
#4358=LINE('',#75672,#8886);
#4359=LINE('',#75680,#8887);
#4360=LINE('',#75692,#8888);
#4361=LINE('',#75703,#8889);
#4362=LINE('',#75705,#8890);
#4363=LINE('',#75707,#8891);
#4364=LINE('',#75709,#8892);
#4365=LINE('',#75711,#8893);
#4366=LINE('',#75713,#8894);
#4367=LINE('',#75715,#8895);
#4368=LINE('',#75717,#8896);
#4369=LINE('',#75719,#8897);
#4370=LINE('',#75721,#8898);
#4371=LINE('',#75723,#8899);
#4372=LINE('',#75725,#8900);
#4373=LINE('',#75727,#8901);
#4374=LINE('',#75729,#8902);
#4375=LINE('',#75736,#8903);
#4376=LINE('',#75737,#8904);
#4377=LINE('',#75741,#8905);
#4378=LINE('',#75745,#8906);
#4379=LINE('',#75749,#8907);
#4380=LINE('',#75753,#8908);
#4381=LINE('',#75757,#8909);
#4382=LINE('',#75760,#8910);
#4383=LINE('',#75761,#8911);
#4384=LINE('',#75765,#8912);
#4385=LINE('',#75769,#8913);
#4386=LINE('',#75773,#8914);
#4387=LINE('',#75777,#8915);
#4388=LINE('',#75781,#8916);
#4389=LINE('',#75783,#8917);
#4390=LINE('',#75791,#8918);
#4391=LINE('',#75803,#8919);
#4392=LINE('',#75814,#8920);
#4393=LINE('',#75816,#8921);
#4394=LINE('',#75818,#8922);
#4395=LINE('',#75820,#8923);
#4396=LINE('',#75822,#8924);
#4397=LINE('',#75824,#8925);
#4398=LINE('',#75826,#8926);
#4399=LINE('',#75828,#8927);
#4400=LINE('',#75830,#8928);
#4401=LINE('',#75832,#8929);
#4402=LINE('',#75834,#8930);
#4403=LINE('',#75836,#8931);
#4404=LINE('',#75838,#8932);
#4405=LINE('',#75840,#8933);
#4406=LINE('',#75847,#8934);
#4407=LINE('',#75848,#8935);
#4408=LINE('',#75852,#8936);
#4409=LINE('',#75856,#8937);
#4410=LINE('',#75860,#8938);
#4411=LINE('',#75864,#8939);
#4412=LINE('',#75868,#8940);
#4413=LINE('',#75871,#8941);
#4414=LINE('',#75872,#8942);
#4415=LINE('',#75876,#8943);
#4416=LINE('',#75880,#8944);
#4417=LINE('',#75884,#8945);
#4418=LINE('',#75888,#8946);
#4419=LINE('',#75892,#8947);
#4420=LINE('',#75894,#8948);
#4421=LINE('',#75902,#8949);
#4422=LINE('',#75914,#8950);
#4423=LINE('',#75925,#8951);
#4424=LINE('',#75927,#8952);
#4425=LINE('',#75929,#8953);
#4426=LINE('',#75931,#8954);
#4427=LINE('',#75933,#8955);
#4428=LINE('',#75935,#8956);
#4429=LINE('',#75937,#8957);
#4430=LINE('',#75939,#8958);
#4431=LINE('',#75941,#8959);
#4432=LINE('',#75943,#8960);
#4433=LINE('',#75945,#8961);
#4434=LINE('',#75947,#8962);
#4435=LINE('',#75949,#8963);
#4436=LINE('',#75951,#8964);
#4437=LINE('',#75958,#8965);
#4438=LINE('',#75959,#8966);
#4439=LINE('',#75963,#8967);
#4440=LINE('',#75967,#8968);
#4441=LINE('',#75971,#8969);
#4442=LINE('',#75975,#8970);
#4443=LINE('',#75979,#8971);
#4444=LINE('',#75982,#8972);
#4445=LINE('',#75983,#8973);
#4446=LINE('',#75987,#8974);
#4447=LINE('',#75991,#8975);
#4448=LINE('',#75995,#8976);
#4449=LINE('',#75999,#8977);
#4450=LINE('',#76003,#8978);
#4451=LINE('',#76005,#8979);
#4452=LINE('',#76013,#8980);
#4453=LINE('',#76025,#8981);
#4454=LINE('',#76036,#8982);
#4455=LINE('',#76038,#8983);
#4456=LINE('',#76040,#8984);
#4457=LINE('',#76042,#8985);
#4458=LINE('',#76044,#8986);
#4459=LINE('',#76046,#8987);
#4460=LINE('',#76048,#8988);
#4461=LINE('',#76050,#8989);
#4462=LINE('',#76052,#8990);
#4463=LINE('',#76054,#8991);
#4464=LINE('',#76056,#8992);
#4465=LINE('',#76058,#8993);
#4466=LINE('',#76060,#8994);
#4467=LINE('',#76062,#8995);
#4468=LINE('',#76069,#8996);
#4469=LINE('',#76070,#8997);
#4470=LINE('',#76074,#8998);
#4471=LINE('',#76078,#8999);
#4472=LINE('',#76082,#9000);
#4473=LINE('',#76086,#9001);
#4474=LINE('',#76090,#9002);
#4475=LINE('',#76093,#9003);
#4476=LINE('',#76094,#9004);
#4477=LINE('',#76098,#9005);
#4478=LINE('',#76102,#9006);
#4479=LINE('',#76106,#9007);
#4480=LINE('',#76110,#9008);
#4481=LINE('',#76114,#9009);
#4482=LINE('',#76116,#9010);
#4483=LINE('',#76124,#9011);
#4484=LINE('',#76136,#9012);
#4485=LINE('',#76147,#9013);
#4486=LINE('',#76149,#9014);
#4487=LINE('',#76151,#9015);
#4488=LINE('',#76153,#9016);
#4489=LINE('',#76155,#9017);
#4490=LINE('',#76157,#9018);
#4491=LINE('',#76159,#9019);
#4492=LINE('',#76161,#9020);
#4493=LINE('',#76163,#9021);
#4494=LINE('',#76165,#9022);
#4495=LINE('',#76167,#9023);
#4496=LINE('',#76169,#9024);
#4497=LINE('',#76171,#9025);
#4498=LINE('',#76173,#9026);
#4499=LINE('',#76180,#9027);
#4500=LINE('',#76181,#9028);
#4501=LINE('',#76185,#9029);
#4502=LINE('',#76189,#9030);
#4503=LINE('',#76193,#9031);
#4504=LINE('',#76197,#9032);
#4505=LINE('',#76201,#9033);
#4506=LINE('',#76204,#9034);
#4507=LINE('',#76205,#9035);
#4508=LINE('',#76209,#9036);
#4509=LINE('',#76213,#9037);
#4510=LINE('',#76217,#9038);
#4511=LINE('',#76221,#9039);
#4512=LINE('',#76225,#9040);
#4513=LINE('',#76227,#9041);
#4514=LINE('',#76235,#9042);
#4515=LINE('',#76247,#9043);
#4516=LINE('',#76258,#9044);
#4517=LINE('',#76260,#9045);
#4518=LINE('',#76262,#9046);
#4519=LINE('',#76264,#9047);
#4520=LINE('',#76266,#9048);
#4521=LINE('',#76268,#9049);
#4522=LINE('',#76270,#9050);
#4523=LINE('',#76272,#9051);
#4524=LINE('',#76274,#9052);
#4525=LINE('',#76276,#9053);
#4526=LINE('',#76278,#9054);
#4527=LINE('',#76280,#9055);
#4528=LINE('',#76282,#9056);
#4529=LINE('',#76284,#9057);
#4530=LINE('',#76291,#9058);
#4531=LINE('',#76292,#9059);
#4532=LINE('',#76296,#9060);
#4533=LINE('',#76300,#9061);
#4534=LINE('',#76304,#9062);
#4535=LINE('',#76308,#9063);
#4536=LINE('',#76312,#9064);
#4537=LINE('',#76315,#9065);
#4538=LINE('',#76316,#9066);
#4539=LINE('',#76320,#9067);
#4540=LINE('',#76324,#9068);
#4541=LINE('',#76328,#9069);
#4542=LINE('',#76332,#9070);
#4543=LINE('',#76336,#9071);
#4544=LINE('',#76338,#9072);
#4545=LINE('',#76346,#9073);
#4546=LINE('',#76358,#9074);
#4547=LINE('',#76369,#9075);
#4548=LINE('',#76371,#9076);
#4549=LINE('',#76373,#9077);
#4550=LINE('',#76375,#9078);
#4551=LINE('',#76377,#9079);
#4552=LINE('',#76379,#9080);
#4553=LINE('',#76381,#9081);
#4554=LINE('',#76383,#9082);
#4555=LINE('',#76385,#9083);
#4556=LINE('',#76387,#9084);
#4557=LINE('',#76389,#9085);
#4558=LINE('',#76391,#9086);
#4559=LINE('',#76393,#9087);
#4560=LINE('',#76395,#9088);
#4561=LINE('',#76402,#9089);
#4562=LINE('',#76403,#9090);
#4563=LINE('',#76407,#9091);
#4564=LINE('',#76411,#9092);
#4565=LINE('',#76415,#9093);
#4566=LINE('',#76419,#9094);
#4567=LINE('',#76423,#9095);
#4568=LINE('',#76426,#9096);
#4569=LINE('',#76427,#9097);
#4570=LINE('',#76431,#9098);
#4571=LINE('',#76435,#9099);
#4572=LINE('',#76439,#9100);
#4573=LINE('',#76443,#9101);
#4574=LINE('',#76447,#9102);
#4575=LINE('',#76449,#9103);
#4576=LINE('',#76457,#9104);
#4577=LINE('',#76469,#9105);
#4578=LINE('',#76480,#9106);
#4579=LINE('',#76482,#9107);
#4580=LINE('',#76484,#9108);
#4581=LINE('',#76486,#9109);
#4582=LINE('',#76488,#9110);
#4583=LINE('',#76490,#9111);
#4584=LINE('',#76492,#9112);
#4585=LINE('',#76494,#9113);
#4586=LINE('',#76496,#9114);
#4587=LINE('',#76498,#9115);
#4588=LINE('',#76500,#9116);
#4589=LINE('',#76502,#9117);
#4590=LINE('',#76504,#9118);
#4591=LINE('',#76506,#9119);
#4592=LINE('',#76513,#9120);
#4593=LINE('',#76514,#9121);
#4594=LINE('',#76518,#9122);
#4595=LINE('',#76522,#9123);
#4596=LINE('',#76526,#9124);
#4597=LINE('',#76530,#9125);
#4598=LINE('',#76534,#9126);
#4599=LINE('',#76537,#9127);
#4600=LINE('',#76538,#9128);
#4601=LINE('',#76542,#9129);
#4602=LINE('',#76546,#9130);
#4603=LINE('',#76550,#9131);
#4604=LINE('',#76554,#9132);
#4605=LINE('',#76558,#9133);
#4606=LINE('',#76560,#9134);
#4607=LINE('',#76568,#9135);
#4608=LINE('',#76580,#9136);
#4609=LINE('',#76591,#9137);
#4610=LINE('',#76593,#9138);
#4611=LINE('',#76595,#9139);
#4612=LINE('',#76597,#9140);
#4613=LINE('',#76599,#9141);
#4614=LINE('',#76601,#9142);
#4615=LINE('',#76603,#9143);
#4616=LINE('',#76605,#9144);
#4617=LINE('',#76607,#9145);
#4618=LINE('',#76609,#9146);
#4619=LINE('',#76611,#9147);
#4620=LINE('',#76613,#9148);
#4621=LINE('',#76615,#9149);
#4622=LINE('',#76617,#9150);
#4623=LINE('',#76624,#9151);
#4624=LINE('',#76625,#9152);
#4625=LINE('',#76629,#9153);
#4626=LINE('',#76633,#9154);
#4627=LINE('',#76637,#9155);
#4628=LINE('',#76641,#9156);
#4629=LINE('',#76645,#9157);
#4630=LINE('',#76648,#9158);
#4631=LINE('',#76649,#9159);
#4632=LINE('',#76653,#9160);
#4633=LINE('',#76657,#9161);
#4634=LINE('',#76661,#9162);
#4635=LINE('',#76665,#9163);
#4636=LINE('',#76669,#9164);
#4637=LINE('',#76671,#9165);
#4638=LINE('',#76679,#9166);
#4639=LINE('',#76691,#9167);
#4640=LINE('',#76702,#9168);
#4641=LINE('',#76704,#9169);
#4642=LINE('',#76706,#9170);
#4643=LINE('',#76708,#9171);
#4644=LINE('',#76710,#9172);
#4645=LINE('',#76712,#9173);
#4646=LINE('',#76714,#9174);
#4647=LINE('',#76716,#9175);
#4648=LINE('',#76718,#9176);
#4649=LINE('',#76720,#9177);
#4650=LINE('',#76722,#9178);
#4651=LINE('',#76724,#9179);
#4652=LINE('',#76726,#9180);
#4653=LINE('',#76728,#9181);
#4654=LINE('',#76735,#9182);
#4655=LINE('',#76736,#9183);
#4656=LINE('',#76740,#9184);
#4657=LINE('',#76744,#9185);
#4658=LINE('',#76748,#9186);
#4659=LINE('',#76752,#9187);
#4660=LINE('',#76756,#9188);
#4661=LINE('',#76759,#9189);
#4662=LINE('',#76760,#9190);
#4663=LINE('',#76764,#9191);
#4664=LINE('',#76768,#9192);
#4665=LINE('',#76772,#9193);
#4666=LINE('',#76776,#9194);
#4667=LINE('',#76780,#9195);
#4668=LINE('',#76782,#9196);
#4669=LINE('',#76790,#9197);
#4670=LINE('',#76802,#9198);
#4671=LINE('',#76813,#9199);
#4672=LINE('',#76815,#9200);
#4673=LINE('',#76817,#9201);
#4674=LINE('',#76819,#9202);
#4675=LINE('',#76821,#9203);
#4676=LINE('',#76823,#9204);
#4677=LINE('',#76825,#9205);
#4678=LINE('',#76827,#9206);
#4679=LINE('',#76829,#9207);
#4680=LINE('',#76831,#9208);
#4681=LINE('',#76833,#9209);
#4682=LINE('',#76835,#9210);
#4683=LINE('',#76837,#9211);
#4684=LINE('',#76839,#9212);
#4685=LINE('',#76846,#9213);
#4686=LINE('',#76847,#9214);
#4687=LINE('',#76851,#9215);
#4688=LINE('',#76855,#9216);
#4689=LINE('',#76859,#9217);
#4690=LINE('',#76863,#9218);
#4691=LINE('',#76867,#9219);
#4692=LINE('',#76870,#9220);
#4693=LINE('',#76871,#9221);
#4694=LINE('',#76875,#9222);
#4695=LINE('',#76879,#9223);
#4696=LINE('',#76883,#9224);
#4697=LINE('',#76887,#9225);
#4698=LINE('',#76891,#9226);
#4699=LINE('',#76893,#9227);
#4700=LINE('',#76901,#9228);
#4701=LINE('',#76913,#9229);
#4702=LINE('',#76924,#9230);
#4703=LINE('',#76926,#9231);
#4704=LINE('',#76928,#9232);
#4705=LINE('',#76930,#9233);
#4706=LINE('',#76932,#9234);
#4707=LINE('',#76934,#9235);
#4708=LINE('',#76936,#9236);
#4709=LINE('',#76938,#9237);
#4710=LINE('',#76940,#9238);
#4711=LINE('',#76942,#9239);
#4712=LINE('',#76944,#9240);
#4713=LINE('',#76946,#9241);
#4714=LINE('',#76948,#9242);
#4715=LINE('',#76950,#9243);
#4716=LINE('',#76957,#9244);
#4717=LINE('',#76958,#9245);
#4718=LINE('',#76962,#9246);
#4719=LINE('',#76966,#9247);
#4720=LINE('',#76970,#9248);
#4721=LINE('',#76974,#9249);
#4722=LINE('',#76978,#9250);
#4723=LINE('',#76981,#9251);
#4724=LINE('',#76982,#9252);
#4725=LINE('',#76986,#9253);
#4726=LINE('',#76990,#9254);
#4727=LINE('',#76994,#9255);
#4728=LINE('',#76998,#9256);
#4729=LINE('',#77002,#9257);
#4730=LINE('',#77004,#9258);
#4731=LINE('',#77012,#9259);
#4732=LINE('',#77024,#9260);
#4733=LINE('',#77035,#9261);
#4734=LINE('',#77037,#9262);
#4735=LINE('',#77039,#9263);
#4736=LINE('',#77041,#9264);
#4737=LINE('',#77043,#9265);
#4738=LINE('',#77045,#9266);
#4739=LINE('',#77047,#9267);
#4740=LINE('',#77049,#9268);
#4741=LINE('',#77051,#9269);
#4742=LINE('',#77053,#9270);
#4743=LINE('',#77055,#9271);
#4744=LINE('',#77057,#9272);
#4745=LINE('',#77059,#9273);
#4746=LINE('',#77061,#9274);
#4747=LINE('',#77068,#9275);
#4748=LINE('',#77069,#9276);
#4749=LINE('',#77073,#9277);
#4750=LINE('',#77077,#9278);
#4751=LINE('',#77081,#9279);
#4752=LINE('',#77085,#9280);
#4753=LINE('',#77089,#9281);
#4754=LINE('',#77092,#9282);
#4755=LINE('',#77093,#9283);
#4756=LINE('',#77097,#9284);
#4757=LINE('',#77101,#9285);
#4758=LINE('',#77105,#9286);
#4759=LINE('',#77109,#9287);
#4760=LINE('',#77113,#9288);
#4761=LINE('',#77115,#9289);
#4762=LINE('',#77123,#9290);
#4763=LINE('',#77135,#9291);
#4764=LINE('',#77146,#9292);
#4765=LINE('',#77148,#9293);
#4766=LINE('',#77150,#9294);
#4767=LINE('',#77152,#9295);
#4768=LINE('',#77154,#9296);
#4769=LINE('',#77156,#9297);
#4770=LINE('',#77158,#9298);
#4771=LINE('',#77160,#9299);
#4772=LINE('',#77162,#9300);
#4773=LINE('',#77164,#9301);
#4774=LINE('',#77166,#9302);
#4775=LINE('',#77168,#9303);
#4776=LINE('',#77170,#9304);
#4777=LINE('',#77172,#9305);
#4778=LINE('',#77179,#9306);
#4779=LINE('',#77180,#9307);
#4780=LINE('',#77184,#9308);
#4781=LINE('',#77188,#9309);
#4782=LINE('',#77192,#9310);
#4783=LINE('',#77196,#9311);
#4784=LINE('',#77200,#9312);
#4785=LINE('',#77203,#9313);
#4786=LINE('',#77204,#9314);
#4787=LINE('',#77208,#9315);
#4788=LINE('',#77212,#9316);
#4789=LINE('',#77216,#9317);
#4790=LINE('',#77220,#9318);
#4791=LINE('',#77224,#9319);
#4792=LINE('',#77226,#9320);
#4793=LINE('',#77234,#9321);
#4794=LINE('',#77246,#9322);
#4795=LINE('',#77257,#9323);
#4796=LINE('',#77260,#9324);
#4797=LINE('',#77261,#9325);
#4798=LINE('',#77265,#9326);
#4799=LINE('',#77269,#9327);
#4800=LINE('',#77273,#9328);
#4801=LINE('',#77277,#9329);
#4802=LINE('',#77281,#9330);
#4803=LINE('',#77284,#9331);
#4804=LINE('',#77285,#9332);
#4805=LINE('',#77289,#9333);
#4806=LINE('',#77293,#9334);
#4807=LINE('',#77297,#9335);
#4808=LINE('',#77301,#9336);
#4809=LINE('',#77305,#9337);
#4810=LINE('',#77308,#9338);
#4811=LINE('',#77309,#9339);
#4812=LINE('',#77313,#9340);
#4813=LINE('',#77315,#9341);
#4814=LINE('',#77317,#9342);
#4815=LINE('',#77319,#9343);
#4816=LINE('',#77321,#9344);
#4817=LINE('',#77323,#9345);
#4818=LINE('',#77325,#9346);
#4819=LINE('',#77327,#9347);
#4820=LINE('',#77329,#9348);
#4821=LINE('',#77331,#9349);
#4822=LINE('',#77333,#9350);
#4823=LINE('',#77335,#9351);
#4824=LINE('',#77337,#9352);
#4825=LINE('',#77345,#9353);
#4826=LINE('',#77351,#9354);
#4827=LINE('',#77357,#9355);
#4828=LINE('',#77370,#9356);
#4829=LINE('',#77382,#9357);
#4830=LINE('',#77403,#9358);
#4831=LINE('',#77407,#9359);
#4832=LINE('',#77409,#9360);
#4833=LINE('',#77413,#9361);
#4834=LINE('',#77415,#9362);
#4835=LINE('',#77424,#9363);
#4836=LINE('',#77426,#9364);
#4837=LINE('',#77428,#9365);
#4838=LINE('',#77433,#9366);
#4839=LINE('',#77441,#9367);
#4840=LINE('',#77447,#9368);
#4841=LINE('',#77449,#9369);
#4842=LINE('',#77450,#9370);
#4843=LINE('',#77452,#9371);
#4844=LINE('',#77453,#9372);
#4845=LINE('',#77458,#9373);
#4846=LINE('',#77626,#9374);
#4847=LINE('',#77628,#9375);
#4848=LINE('',#77630,#9376);
#4849=LINE('',#77634,#9377);
#4850=LINE('',#77636,#9378);
#4851=LINE('',#77638,#9379);
#4852=LINE('',#77962,#9380);
#4853=LINE('',#77963,#9381);
#4854=LINE('',#77964,#9382);
#4855=LINE('',#77972,#9383);
#4856=LINE('',#77977,#9384);
#4857=LINE('',#77978,#9385);
#4858=LINE('',#77980,#9386);
#4859=LINE('',#78304,#9387);
#4860=LINE('',#78467,#9388);
#4861=LINE('',#78468,#9389);
#4862=LINE('',#78469,#9390);
#4863=LINE('',#78471,#9391);
#4864=LINE('',#78473,#9392);
#4865=LINE('',#78474,#9393);
#4866=LINE('',#78476,#9394);
#4867=LINE('',#78478,#9395);
#4868=LINE('',#78976,#9396);
#4869=LINE('',#78982,#9397);
#4870=LINE('',#78983,#9398);
#4871=LINE('',#78984,#9399);
#4872=LINE('',#78986,#9400);
#4873=LINE('',#78987,#9401);
#4874=LINE('',#78990,#9402);
#4875=LINE('',#78996,#9403);
#4876=LINE('',#79002,#9404);
#4877=LINE('',#79003,#9405);
#4878=LINE('',#79004,#9406);
#4879=LINE('',#79006,#9407);
#4880=LINE('',#79007,#9408);
#4881=LINE('',#79010,#9409);
#4882=LINE('',#79016,#9410);
#4883=LINE('',#79022,#9411);
#4884=LINE('',#79023,#9412);
#4885=LINE('',#79024,#9413);
#4886=LINE('',#79026,#9414);
#4887=LINE('',#79027,#9415);
#4888=LINE('',#79030,#9416);
#4889=LINE('',#79036,#9417);
#4890=LINE('',#79042,#9418);
#4891=LINE('',#79043,#9419);
#4892=LINE('',#79044,#9420);
#4893=LINE('',#79046,#9421);
#4894=LINE('',#79047,#9422);
#4895=LINE('',#79050,#9423);
#4896=LINE('',#79056,#9424);
#4897=LINE('',#79062,#9425);
#4898=LINE('',#79063,#9426);
#4899=LINE('',#79064,#9427);
#4900=LINE('',#79066,#9428);
#4901=LINE('',#79067,#9429);
#4902=LINE('',#79070,#9430);
#4903=LINE('',#79076,#9431);
#4904=LINE('',#79082,#9432);
#4905=LINE('',#79083,#9433);
#4906=LINE('',#79084,#9434);
#4907=LINE('',#79086,#9435);
#4908=LINE('',#79087,#9436);
#4909=LINE('',#79090,#9437);
#4910=LINE('',#79096,#9438);
#4911=LINE('',#79102,#9439);
#4912=LINE('',#79103,#9440);
#4913=LINE('',#79104,#9441);
#4914=LINE('',#79106,#9442);
#4915=LINE('',#79107,#9443);
#4916=LINE('',#79110,#9444);
#4917=LINE('',#79116,#9445);
#4918=LINE('',#79122,#9446);
#4919=LINE('',#79123,#9447);
#4920=LINE('',#79124,#9448);
#4921=LINE('',#79126,#9449);
#4922=LINE('',#79127,#9450);
#4923=LINE('',#79130,#9451);
#4924=LINE('',#79136,#9452);
#4925=LINE('',#79142,#9453);
#4926=LINE('',#79143,#9454);
#4927=LINE('',#79144,#9455);
#4928=LINE('',#79146,#9456);
#4929=LINE('',#79147,#9457);
#4930=LINE('',#79150,#9458);
#4931=LINE('',#79156,#9459);
#4932=LINE('',#79162,#9460);
#4933=LINE('',#79163,#9461);
#4934=LINE('',#79164,#9462);
#4935=LINE('',#79166,#9463);
#4936=LINE('',#79167,#9464);
#4937=LINE('',#79170,#9465);
#4938=LINE('',#79176,#9466);
#4939=LINE('',#79182,#9467);
#4940=LINE('',#79183,#9468);
#4941=LINE('',#79184,#9469);
#4942=LINE('',#79186,#9470);
#4943=LINE('',#79187,#9471);
#4944=LINE('',#79190,#9472);
#4945=LINE('',#79196,#9473);
#4946=LINE('',#79202,#9474);
#4947=LINE('',#79203,#9475);
#4948=LINE('',#79204,#9476);
#4949=LINE('',#79206,#9477);
#4950=LINE('',#79207,#9478);
#4951=LINE('',#79210,#9479);
#4952=LINE('',#79216,#9480);
#4953=LINE('',#79222,#9481);
#4954=LINE('',#79223,#9482);
#4955=LINE('',#79224,#9483);
#4956=LINE('',#79226,#9484);
#4957=LINE('',#79227,#9485);
#4958=LINE('',#79230,#9486);
#4959=LINE('',#79236,#9487);
#4960=LINE('',#79242,#9488);
#4961=LINE('',#79243,#9489);
#4962=LINE('',#79244,#9490);
#4963=LINE('',#79246,#9491);
#4964=LINE('',#79247,#9492);
#4965=LINE('',#79250,#9493);
#4966=LINE('',#79256,#9494);
#4967=LINE('',#79262,#9495);
#4968=LINE('',#79263,#9496);
#4969=LINE('',#79264,#9497);
#4970=LINE('',#79266,#9498);
#4971=LINE('',#79267,#9499);
#4972=LINE('',#79270,#9500);
#4973=LINE('',#79276,#9501);
#4974=LINE('',#79282,#9502);
#4975=LINE('',#79283,#9503);
#4976=LINE('',#79284,#9504);
#4977=LINE('',#79286,#9505);
#4978=LINE('',#79287,#9506);
#4979=LINE('',#79290,#9507);
#4980=LINE('',#79296,#9508);
#4981=LINE('',#79302,#9509);
#4982=LINE('',#79303,#9510);
#4983=LINE('',#79304,#9511);
#4984=LINE('',#79306,#9512);
#4985=LINE('',#79307,#9513);
#4986=LINE('',#79310,#9514);
#4987=LINE('',#79316,#9515);
#4988=LINE('',#79322,#9516);
#4989=LINE('',#79323,#9517);
#4990=LINE('',#79324,#9518);
#4991=LINE('',#79326,#9519);
#4992=LINE('',#79327,#9520);
#4993=LINE('',#79330,#9521);
#4994=LINE('',#79336,#9522);
#4995=LINE('',#79342,#9523);
#4996=LINE('',#79343,#9524);
#4997=LINE('',#79344,#9525);
#4998=LINE('',#79346,#9526);
#4999=LINE('',#79347,#9527);
#5000=LINE('',#79350,#9528);
#5001=LINE('',#79356,#9529);
#5002=LINE('',#79362,#9530);
#5003=LINE('',#79363,#9531);
#5004=LINE('',#79364,#9532);
#5005=LINE('',#79366,#9533);
#5006=LINE('',#79367,#9534);
#5007=LINE('',#79370,#9535);
#5008=LINE('',#79376,#9536);
#5009=LINE('',#79382,#9537);
#5010=LINE('',#79383,#9538);
#5011=LINE('',#79384,#9539);
#5012=LINE('',#79386,#9540);
#5013=LINE('',#79387,#9541);
#5014=LINE('',#79390,#9542);
#5015=LINE('',#79396,#9543);
#5016=LINE('',#79402,#9544);
#5017=LINE('',#79403,#9545);
#5018=LINE('',#79404,#9546);
#5019=LINE('',#79406,#9547);
#5020=LINE('',#79407,#9548);
#5021=LINE('',#79410,#9549);
#5022=LINE('',#79416,#9550);
#5023=LINE('',#79422,#9551);
#5024=LINE('',#79423,#9552);
#5025=LINE('',#79424,#9553);
#5026=LINE('',#79426,#9554);
#5027=LINE('',#79427,#9555);
#5028=LINE('',#79430,#9556);
#5029=LINE('',#79436,#9557);
#5030=LINE('',#79442,#9558);
#5031=LINE('',#79443,#9559);
#5032=LINE('',#79444,#9560);
#5033=LINE('',#79446,#9561);
#5034=LINE('',#79447,#9562);
#5035=LINE('',#79450,#9563);
#5036=LINE('',#79456,#9564);
#5037=LINE('',#79462,#9565);
#5038=LINE('',#79463,#9566);
#5039=LINE('',#79464,#9567);
#5040=LINE('',#79466,#9568);
#5041=LINE('',#79467,#9569);
#5042=LINE('',#79470,#9570);
#5043=LINE('',#79476,#9571);
#5044=LINE('',#79482,#9572);
#5045=LINE('',#79483,#9573);
#5046=LINE('',#79484,#9574);
#5047=LINE('',#79486,#9575);
#5048=LINE('',#79487,#9576);
#5049=LINE('',#79490,#9577);
#5050=LINE('',#79496,#9578);
#5051=LINE('',#79502,#9579);
#5052=LINE('',#79503,#9580);
#5053=LINE('',#79504,#9581);
#5054=LINE('',#79506,#9582);
#5055=LINE('',#79507,#9583);
#5056=LINE('',#79510,#9584);
#5057=LINE('',#79516,#9585);
#5058=LINE('',#79522,#9586);
#5059=LINE('',#79523,#9587);
#5060=LINE('',#79524,#9588);
#5061=LINE('',#79526,#9589);
#5062=LINE('',#79527,#9590);
#5063=LINE('',#79530,#9591);
#5064=LINE('',#79536,#9592);
#5065=LINE('',#79542,#9593);
#5066=LINE('',#79543,#9594);
#5067=LINE('',#79544,#9595);
#5068=LINE('',#79546,#9596);
#5069=LINE('',#79547,#9597);
#5070=LINE('',#79550,#9598);
#5071=LINE('',#79556,#9599);
#5072=LINE('',#79562,#9600);
#5073=LINE('',#79563,#9601);
#5074=LINE('',#79564,#9602);
#5075=LINE('',#79566,#9603);
#5076=LINE('',#79567,#9604);
#5077=LINE('',#79570,#9605);
#5078=LINE('',#79576,#9606);
#5079=LINE('',#79582,#9607);
#5080=LINE('',#79583,#9608);
#5081=LINE('',#79584,#9609);
#5082=LINE('',#79586,#9610);
#5083=LINE('',#79587,#9611);
#5084=LINE('',#79590,#9612);
#5085=LINE('',#79596,#9613);
#5086=LINE('',#79602,#9614);
#5087=LINE('',#79603,#9615);
#5088=LINE('',#79604,#9616);
#5089=LINE('',#79606,#9617);
#5090=LINE('',#79607,#9618);
#5091=LINE('',#79610,#9619);
#5092=LINE('',#79616,#9620);
#5093=LINE('',#79622,#9621);
#5094=LINE('',#79623,#9622);
#5095=LINE('',#79624,#9623);
#5096=LINE('',#79626,#9624);
#5097=LINE('',#79627,#9625);
#5098=LINE('',#79630,#9626);
#5099=LINE('',#79834,#9627);
#5100=LINE('',#79835,#9628);
#5101=LINE('',#79836,#9629);
#5102=LINE('',#79838,#9630);
#5103=LINE('',#79839,#9631);
#5104=LINE('',#79842,#9632);
#5105=LINE('',#79843,#9633);
#5106=LINE('',#79844,#9634);
#5107=LINE('',#79846,#9635);
#5108=LINE('',#79847,#9636);
#5109=LINE('',#79850,#9637);
#5110=LINE('',#79851,#9638);
#5111=LINE('',#79852,#9639);
#5112=LINE('',#79854,#9640);
#5113=LINE('',#79855,#9641);
#5114=LINE('',#79858,#9642);
#5115=LINE('',#79859,#9643);
#5116=LINE('',#79860,#9644);
#5117=LINE('',#79862,#9645);
#5118=LINE('',#79863,#9646);
#5119=LINE('',#79866,#9647);
#5120=LINE('',#79867,#9648);
#5121=LINE('',#79868,#9649);
#5122=LINE('',#79870,#9650);
#5123=LINE('',#79871,#9651);
#5124=LINE('',#79874,#9652);
#5125=LINE('',#79875,#9653);
#5126=LINE('',#79876,#9654);
#5127=LINE('',#79878,#9655);
#5128=LINE('',#79879,#9656);
#5129=LINE('',#79882,#9657);
#5130=LINE('',#79883,#9658);
#5131=LINE('',#79884,#9659);
#5132=LINE('',#79886,#9660);
#5133=LINE('',#79887,#9661);
#5134=LINE('',#79890,#9662);
#5135=LINE('',#79891,#9663);
#5136=LINE('',#79892,#9664);
#5137=LINE('',#79894,#9665);
#5138=LINE('',#79895,#9666);
#5139=LINE('',#79898,#9667);
#5140=LINE('',#79899,#9668);
#5141=LINE('',#79900,#9669);
#5142=LINE('',#79902,#9670);
#5143=LINE('',#79903,#9671);
#5144=LINE('',#79906,#9672);
#5145=LINE('',#79907,#9673);
#5146=LINE('',#79908,#9674);
#5147=LINE('',#79910,#9675);
#5148=LINE('',#79911,#9676);
#5149=LINE('',#79914,#9677);
#5150=LINE('',#79915,#9678);
#5151=LINE('',#79917,#9679);
#5152=LINE('',#79918,#9680);
#5153=LINE('',#79921,#9681);
#5154=LINE('',#79922,#9682);
#5155=LINE('',#79923,#9683);
#5156=LINE('',#79925,#9684);
#5157=LINE('',#79926,#9685);
#5158=LINE('',#79929,#9686);
#5159=LINE('',#79930,#9687);
#5160=LINE('',#79931,#9688);
#5161=LINE('',#79933,#9689);
#5162=LINE('',#79934,#9690);
#5163=LINE('',#79937,#9691);
#5164=LINE('',#79938,#9692);
#5165=LINE('',#79939,#9693);
#5166=LINE('',#79941,#9694);
#5167=LINE('',#79942,#9695);
#5168=LINE('',#79945,#9696);
#5169=LINE('',#79946,#9697);
#5170=LINE('',#79947,#9698);
#5171=LINE('',#79949,#9699);
#5172=LINE('',#79950,#9700);
#5173=LINE('',#79953,#9701);
#5174=LINE('',#79954,#9702);
#5175=LINE('',#79955,#9703);
#5176=LINE('',#79957,#9704);
#5177=LINE('',#79958,#9705);
#5178=LINE('',#79961,#9706);
#5179=LINE('',#79962,#9707);
#5180=LINE('',#79963,#9708);
#5181=LINE('',#79965,#9709);
#5182=LINE('',#79966,#9710);
#5183=LINE('',#79969,#9711);
#5184=LINE('',#79970,#9712);
#5185=LINE('',#79971,#9713);
#5186=LINE('',#79973,#9714);
#5187=LINE('',#79974,#9715);
#5188=LINE('',#79977,#9716);
#5189=LINE('',#79978,#9717);
#5190=LINE('',#79979,#9718);
#5191=LINE('',#79981,#9719);
#5192=LINE('',#79982,#9720);
#5193=LINE('',#79985,#9721);
#5194=LINE('',#79986,#9722);
#5195=LINE('',#79987,#9723);
#5196=LINE('',#79989,#9724);
#5197=LINE('',#79990,#9725);
#5198=LINE('',#79993,#9726);
#5199=LINE('',#79994,#9727);
#5200=LINE('',#79995,#9728);
#5201=LINE('',#79997,#9729);
#5202=LINE('',#79998,#9730);
#5203=LINE('',#80001,#9731);
#5204=LINE('',#80002,#9732);
#5205=LINE('',#80004,#9733);
#5206=LINE('',#80005,#9734);
#5207=LINE('',#80008,#9735);
#5208=LINE('',#80009,#9736);
#5209=LINE('',#80010,#9737);
#5210=LINE('',#80012,#9738);
#5211=LINE('',#80013,#9739);
#5212=LINE('',#80016,#9740);
#5213=LINE('',#80017,#9741);
#5214=LINE('',#80018,#9742);
#5215=LINE('',#80020,#9743);
#5216=LINE('',#80021,#9744);
#5217=LINE('',#80024,#9745);
#5218=LINE('',#80025,#9746);
#5219=LINE('',#80026,#9747);
#5220=LINE('',#80028,#9748);
#5221=LINE('',#80029,#9749);
#5222=LINE('',#80032,#9750);
#5223=LINE('',#80033,#9751);
#5224=LINE('',#80034,#9752);
#5225=LINE('',#80036,#9753);
#5226=LINE('',#80037,#9754);
#5227=LINE('',#80040,#9755);
#5228=LINE('',#80041,#9756);
#5229=LINE('',#80042,#9757);
#5230=LINE('',#80044,#9758);
#5231=LINE('',#80045,#9759);
#5232=LINE('',#80048,#9760);
#5233=LINE('',#80049,#9761);
#5234=LINE('',#80050,#9762);
#5235=LINE('',#80052,#9763);
#5236=LINE('',#80053,#9764);
#5237=LINE('',#80056,#9765);
#5238=LINE('',#80057,#9766);
#5239=LINE('',#80058,#9767);
#5240=LINE('',#80060,#9768);
#5241=LINE('',#80061,#9769);
#5242=LINE('',#80064,#9770);
#5243=LINE('',#80065,#9771);
#5244=LINE('',#80066,#9772);
#5245=LINE('',#80068,#9773);
#5246=LINE('',#80069,#9774);
#5247=LINE('',#80072,#9775);
#5248=LINE('',#80073,#9776);
#5249=LINE('',#80074,#9777);
#5250=LINE('',#80076,#9778);
#5251=LINE('',#80077,#9779);
#5252=LINE('',#80080,#9780);
#5253=LINE('',#80081,#9781);
#5254=LINE('',#80082,#9782);
#5255=LINE('',#80084,#9783);
#5256=LINE('',#80085,#9784);
#5257=LINE('',#80088,#9785);
#5258=LINE('',#80089,#9786);
#5259=LINE('',#80091,#9787);
#5260=LINE('',#80092,#9788);
#5261=LINE('',#80094,#9789);
#5262=LINE('',#80096,#9790);
#5263=LINE('',#80102,#9791);
#5264=LINE('',#80104,#9792);
#5265=LINE('',#80109,#9793);
#5266=LINE('',#80111,#9794);
#5267=LINE('',#80116,#9795);
#5268=LINE('',#80118,#9796);
#5269=LINE('',#80123,#9797);
#5270=LINE('',#80125,#9798);
#5271=LINE('',#80130,#9799);
#5272=LINE('',#80132,#9800);
#5273=LINE('',#80137,#9801);
#5274=LINE('',#80139,#9802);
#5275=LINE('',#80144,#9803);
#5276=LINE('',#80146,#9804);
#5277=LINE('',#80151,#9805);
#5278=LINE('',#80153,#9806);
#5279=LINE('',#80158,#9807);
#5280=LINE('',#80160,#9808);
#5281=LINE('',#80165,#9809);
#5282=LINE('',#80167,#9810);
#5283=LINE('',#80172,#9811);
#5284=LINE('',#80174,#9812);
#5285=LINE('',#80179,#9813);
#5286=LINE('',#80181,#9814);
#5287=LINE('',#80186,#9815);
#5288=LINE('',#80188,#9816);
#5289=LINE('',#80193,#9817);
#5290=LINE('',#80195,#9818);
#5291=LINE('',#80200,#9819);
#5292=LINE('',#80202,#9820);
#5293=LINE('',#80207,#9821);
#5294=LINE('',#80209,#9822);
#5295=LINE('',#80214,#9823);
#5296=LINE('',#80216,#9824);
#5297=LINE('',#80221,#9825);
#5298=LINE('',#80223,#9826);
#5299=LINE('',#80228,#9827);
#5300=LINE('',#80230,#9828);
#5301=LINE('',#80235,#9829);
#5302=LINE('',#80237,#9830);
#5303=LINE('',#80242,#9831);
#5304=LINE('',#80244,#9832);
#5305=LINE('',#80249,#9833);
#5306=LINE('',#80251,#9834);
#5307=LINE('',#80256,#9835);
#5308=LINE('',#80258,#9836);
#5309=LINE('',#80263,#9837);
#5310=LINE('',#80265,#9838);
#5311=LINE('',#80270,#9839);
#5312=LINE('',#80272,#9840);
#5313=LINE('',#80277,#9841);
#5314=LINE('',#80279,#9842);
#5315=LINE('',#80284,#9843);
#5316=LINE('',#80286,#9844);
#5317=LINE('',#80291,#9845);
#5318=LINE('',#80293,#9846);
#5319=LINE('',#80298,#9847);
#5320=LINE('',#80300,#9848);
#5321=LINE('',#80305,#9849);
#5322=LINE('',#80307,#9850);
#5323=LINE('',#80312,#9851);
#5324=LINE('',#80314,#9852);
#5325=LINE('',#80319,#9853);
#5326=LINE('',#80321,#9854);
#5327=LINE('',#80338,#9855);
#5328=LINE('',#80351,#9856);
#5329=LINE('',#80361,#9857);
#5330=LINE('',#80370,#9858);
#5331=LINE('',#80376,#9859);
#5332=LINE('',#80380,#9860);
#5333=LINE('',#80388,#9861);
#5334=LINE('',#80394,#9862);
#5335=LINE('',#80414,#9863);
#5336=LINE('',#80417,#9864);
#5337=LINE('',#80422,#9865);
#5338=LINE('',#80427,#9866);
#5339=LINE('',#80433,#9867);
#5340=LINE('',#80439,#9868);
#5341=LINE('',#80445,#9869);
#5342=LINE('',#80450,#9870);
#5343=LINE('',#80455,#9871);
#5344=LINE('',#80460,#9872);
#5345=LINE('',#80465,#9873);
#5346=LINE('',#80470,#9874);
#5347=LINE('',#80474,#9875);
#5348=LINE('',#80478,#9876);
#5349=LINE('',#80489,#9877);
#5350=LINE('',#80496,#9878);
#5351=LINE('',#80500,#9879);
#5352=LINE('',#80507,#9880);
#5353=LINE('',#80511,#9881);
#5354=LINE('',#80513,#9882);
#5355=LINE('',#80520,#9883);
#5356=LINE('',#80524,#9884);
#5357=LINE('',#80530,#9885);
#5358=LINE('',#80532,#9886);
#5359=LINE('',#80534,#9887);
#5360=LINE('',#80535,#9888);
#5361=LINE('',#80538,#9889);
#5362=LINE('',#80540,#9890);
#5363=LINE('',#80541,#9891);
#5364=LINE('',#80544,#9892);
#5365=LINE('',#80546,#9893);
#5366=LINE('',#80547,#9894);
#5367=LINE('',#80550,#9895);
#5368=LINE('',#80552,#9896);
#5369=LINE('',#80553,#9897);
#5370=LINE('',#80556,#9898);
#5371=LINE('',#80558,#9899);
#5372=LINE('',#80559,#9900);
#5373=LINE('',#80562,#9901);
#5374=LINE('',#80564,#9902);
#5375=LINE('',#80565,#9903);
#5376=LINE('',#80568,#9904);
#5377=LINE('',#80570,#9905);
#5378=LINE('',#80571,#9906);
#5379=LINE('',#80574,#9907);
#5380=LINE('',#80576,#9908);
#5381=LINE('',#80577,#9909);
#5382=LINE('',#80580,#9910);
#5383=LINE('',#80582,#9911);
#5384=LINE('',#80583,#9912);
#5385=LINE('',#80586,#9913);
#5386=LINE('',#80588,#9914);
#5387=LINE('',#80589,#9915);
#5388=LINE('',#80592,#9916);
#5389=LINE('',#80594,#9917);
#5390=LINE('',#80595,#9918);
#5391=LINE('',#80597,#9919);
#5392=LINE('',#80598,#9920);
#5393=LINE('',#80603,#9921);
#5394=LINE('',#80605,#9922);
#5395=LINE('',#80607,#9923);
#5396=LINE('',#80608,#9924);
#5397=LINE('',#80611,#9925);
#5398=LINE('',#80613,#9926);
#5399=LINE('',#80614,#9927);
#5400=LINE('',#80617,#9928);
#5401=LINE('',#80619,#9929);
#5402=LINE('',#80620,#9930);
#5403=LINE('',#80622,#9931);
#5404=LINE('',#80623,#9932);
#5405=LINE('',#80637,#9933);
#5406=LINE('',#80642,#9934);
#5407=LINE('',#80654,#9935);
#5408=LINE('',#80669,#9936);
#5409=LINE('',#80684,#9937);
#5410=LINE('',#80699,#9938);
#5411=LINE('',#80714,#9939);
#5412=LINE('',#80729,#9940);
#5413=LINE('',#80744,#9941);
#5414=LINE('',#80759,#9942);
#5415=LINE('',#80774,#9943);
#5416=LINE('',#80789,#9944);
#5417=LINE('',#80804,#9945);
#5418=LINE('',#80819,#9946);
#5419=LINE('',#80825,#9947);
#5420=LINE('',#80827,#9948);
#5421=LINE('',#80828,#9949);
#5422=LINE('',#80840,#9950);
#5423=LINE('',#80855,#9951);
#5424=LINE('',#80870,#9952);
#5425=LINE('',#80885,#9953);
#5426=LINE('',#80900,#9954);
#5427=LINE('',#80915,#9955);
#5428=LINE('',#80930,#9956);
#5429=LINE('',#80945,#9957);
#5430=LINE('',#80960,#9958);
#5431=LINE('',#80975,#9959);
#5432=LINE('',#80990,#9960);
#5433=LINE('',#81005,#9961);
#5434=LINE('',#81020,#9962);
#5435=LINE('',#81035,#9963);
#5436=LINE('',#81050,#9964);
#5437=LINE('',#81065,#9965);
#5438=LINE('',#81080,#9966);
#5439=LINE('',#81095,#9967);
#5440=LINE('',#81101,#9968);
#5441=LINE('',#81103,#9969);
#5442=LINE('',#81104,#9970);
#5443=LINE('',#81116,#9971);
#5444=LINE('',#81145,#9972);
#5445=LINE('',#81150,#9973);
#5446=LINE('',#81162,#9974);
#5447=LINE('',#81177,#9975);
#5448=LINE('',#81192,#9976);
#5449=LINE('',#81207,#9977);
#5450=LINE('',#81222,#9978);
#5451=LINE('',#81237,#9979);
#5452=LINE('',#81252,#9980);
#5453=LINE('',#81258,#9981);
#5454=LINE('',#81260,#9982);
#5455=LINE('',#81261,#9983);
#5456=LINE('',#81273,#9984);
#5457=LINE('',#81288,#9985);
#5458=LINE('',#81303,#9986);
#5459=LINE('',#81318,#9987);
#5460=LINE('',#81333,#9988);
#5461=LINE('',#81348,#9989);
#5462=LINE('',#81363,#9990);
#5463=LINE('',#81378,#9991);
#5464=LINE('',#81393,#9992);
#5465=LINE('',#81408,#9993);
#5466=LINE('',#81414,#9994);
#5467=LINE('',#81416,#9995);
#5468=LINE('',#81417,#9996);
#5469=LINE('',#81429,#9997);
#5470=LINE('',#81449,#9998);
#5471=LINE('',#81451,#9999);
#5472=LINE('',#81453,#10000);
#5473=LINE('',#81454,#10001);
#5474=LINE('',#81457,#10002);
#5475=LINE('',#81459,#10003);
#5476=LINE('',#81460,#10004);
#5477=LINE('',#81463,#10005);
#5478=LINE('',#81465,#10006);
#5479=LINE('',#81466,#10007);
#5480=LINE('',#81469,#10008);
#5481=LINE('',#81471,#10009);
#5482=LINE('',#81472,#10010);
#5483=LINE('',#81475,#10011);
#5484=LINE('',#81477,#10012);
#5485=LINE('',#81478,#10013);
#5486=LINE('',#81480,#10014);
#5487=LINE('',#81481,#10015);
#5488=LINE('',#81486,#10016);
#5489=LINE('',#81488,#10017);
#5490=LINE('',#81490,#10018);
#5491=LINE('',#81491,#10019);
#5492=LINE('',#81494,#10020);
#5493=LINE('',#81496,#10021);
#5494=LINE('',#81497,#10022);
#5495=LINE('',#81500,#10023);
#5496=LINE('',#81502,#10024);
#5497=LINE('',#81503,#10025);
#5498=LINE('',#81506,#10026);
#5499=LINE('',#81508,#10027);
#5500=LINE('',#81509,#10028);
#5501=LINE('',#81512,#10029);
#5502=LINE('',#81514,#10030);
#5503=LINE('',#81515,#10031);
#5504=LINE('',#81518,#10032);
#5505=LINE('',#81520,#10033);
#5506=LINE('',#81521,#10034);
#5507=LINE('',#81524,#10035);
#5508=LINE('',#81526,#10036);
#5509=LINE('',#81527,#10037);
#5510=LINE('',#81529,#10038);
#5511=LINE('',#81530,#10039);
#5512=LINE('',#81544,#10040);
#5513=LINE('',#81549,#10041);
#5514=LINE('',#81561,#10042);
#5515=LINE('',#81576,#10043);
#5516=LINE('',#81591,#10044);
#5517=LINE('',#81597,#10045);
#5518=LINE('',#81599,#10046);
#5519=LINE('',#81600,#10047);
#5520=LINE('',#81603,#10048);
#5521=LINE('',#81605,#10049);
#5522=LINE('',#81606,#10050);
#5523=LINE('',#81609,#10051);
#5524=LINE('',#81611,#10052);
#5525=LINE('',#81612,#10053);
#5526=LINE('',#81624,#10054);
#5527=LINE('',#81639,#10055);
#5528=LINE('',#81654,#10056);
#5529=LINE('',#81669,#10057);
#5530=LINE('',#81684,#10058);
#5531=LINE('',#81699,#10059);
#5532=LINE('',#81705,#10060);
#5533=LINE('',#81707,#10061);
#5534=LINE('',#81708,#10062);
#5535=LINE('',#81711,#10063);
#5536=LINE('',#81713,#10064);
#5537=LINE('',#81714,#10065);
#5538=LINE('',#81717,#10066);
#5539=LINE('',#81719,#10067);
#5540=LINE('',#81720,#10068);
#5541=LINE('',#81737,#10069);
#5542=LINE('',#81739,#10070);
#5543=LINE('',#81741,#10071);
#5544=LINE('',#81742,#10072);
#5545=LINE('',#81754,#10073);
#5546=LINE('',#81769,#10074);
#5547=LINE('',#81784,#10075);
#5548=LINE('',#81799,#10076);
#5549=LINE('',#81805,#10077);
#5550=LINE('',#81807,#10078);
#5551=LINE('',#81808,#10079);
#5552=LINE('',#81811,#10080);
#5553=LINE('',#81813,#10081);
#5554=LINE('',#81814,#10082);
#5555=LINE('',#81817,#10083);
#5556=LINE('',#81819,#10084);
#5557=LINE('',#81820,#10085);
#5558=LINE('',#81832,#10086);
#5559=LINE('',#81847,#10087);
#5560=LINE('',#81862,#10088);
#5561=LINE('',#81877,#10089);
#5562=LINE('',#81892,#10090);
#5563=LINE('',#81907,#10091);
#5564=LINE('',#81922,#10092);
#5565=LINE('',#81928,#10093);
#5566=LINE('',#81930,#10094);
#5567=LINE('',#81931,#10095);
#5568=LINE('',#81934,#10096);
#5569=LINE('',#81936,#10097);
#5570=LINE('',#81937,#10098);
#5571=LINE('',#81940,#10099);
#5572=LINE('',#81942,#10100);
#5573=LINE('',#81943,#10101);
#5574=LINE('',#81945,#10102);
#5575=LINE('',#81946,#10103);
#5576=LINE('',#81951,#10104);
#5577=LINE('',#81953,#10105);
#5578=LINE('',#81955,#10106);
#5579=LINE('',#81956,#10107);
#5580=LINE('',#81959,#10108);
#5581=LINE('',#81961,#10109);
#5582=LINE('',#81962,#10110);
#5583=LINE('',#81965,#10111);
#5584=LINE('',#81967,#10112);
#5585=LINE('',#81968,#10113);
#5586=LINE('',#81971,#10114);
#5587=LINE('',#81973,#10115);
#5588=LINE('',#81974,#10116);
#5589=LINE('',#81977,#10117);
#5590=LINE('',#81979,#10118);
#5591=LINE('',#81980,#10119);
#5592=LINE('',#81983,#10120);
#5593=LINE('',#81985,#10121);
#5594=LINE('',#81986,#10122);
#5595=LINE('',#81989,#10123);
#5596=LINE('',#81991,#10124);
#5597=LINE('',#81992,#10125);
#5598=LINE('',#81994,#10126);
#5599=LINE('',#81995,#10127);
#5600=LINE('',#82009,#10128);
#5601=LINE('',#82014,#10129);
#5602=LINE('',#82026,#10130);
#5603=LINE('',#82032,#10131);
#5604=LINE('',#82034,#10132);
#5605=LINE('',#82035,#10133);
#5606=LINE('',#82047,#10134);
#5607=LINE('',#82062,#10135);
#5608=LINE('',#82068,#10136);
#5609=LINE('',#82070,#10137);
#5610=LINE('',#82071,#10138);
#5611=LINE('',#82074,#10139);
#5612=LINE('',#82076,#10140);
#5613=LINE('',#82077,#10141);
#5614=LINE('',#82080,#10142);
#5615=LINE('',#82082,#10143);
#5616=LINE('',#82083,#10144);
#5617=LINE('',#82085,#10145);
#5618=LINE('',#82086,#10146);
#5619=LINE('',#82100,#10147);
#5620=LINE('',#82105,#10148);
#5621=LINE('',#82117,#10149);
#5622=LINE('',#82132,#10150);
#5623=LINE('',#82147,#10151);
#5624=LINE('',#82162,#10152);
#5625=LINE('',#82177,#10153);
#5626=LINE('',#82192,#10154);
#5627=LINE('',#82207,#10155);
#5628=LINE('',#82222,#10156);
#5629=LINE('',#82237,#10157);
#5630=LINE('',#82252,#10158);
#5631=LINE('',#82281,#10159);
#5632=LINE('',#82286,#10160);
#5633=LINE('',#82298,#10161);
#5634=LINE('',#82304,#10162);
#5635=LINE('',#82306,#10163);
#5636=LINE('',#82307,#10164);
#5637=LINE('',#82319,#10165);
#5638=LINE('',#82334,#10166);
#5639=LINE('',#82340,#10167);
#5640=LINE('',#82342,#10168);
#5641=LINE('',#82343,#10169);
#5642=LINE('',#82346,#10170);
#5643=LINE('',#82348,#10171);
#5644=LINE('',#82349,#10172);
#5645=LINE('',#82352,#10173);
#5646=LINE('',#82354,#10174);
#5647=LINE('',#82355,#10175);
#5648=LINE('',#82357,#10176);
#5649=LINE('',#82358,#10177);
#5650=LINE('',#82363,#10178);
#5651=LINE('',#82365,#10179);
#5652=LINE('',#82367,#10180);
#5653=LINE('',#82368,#10181);
#5654=LINE('',#82371,#10182);
#5655=LINE('',#82373,#10183);
#5656=LINE('',#82374,#10184);
#5657=LINE('',#82377,#10185);
#5658=LINE('',#82379,#10186);
#5659=LINE('',#82380,#10187);
#5660=LINE('',#82382,#10188);
#5661=LINE('',#82383,#10189);
#5662=LINE('',#82397,#10190);
#5663=LINE('',#82402,#10191);
#5664=LINE('',#82414,#10192);
#5665=LINE('',#82429,#10193);
#5666=LINE('',#82444,#10194);
#5667=LINE('',#82459,#10195);
#5668=LINE('',#82465,#10196);
#5669=LINE('',#82467,#10197);
#5670=LINE('',#82468,#10198);
#5671=LINE('',#82471,#10199);
#5672=LINE('',#82473,#10200);
#5673=LINE('',#82474,#10201);
#5674=LINE('',#82477,#10202);
#5675=LINE('',#82479,#10203);
#5676=LINE('',#82480,#10204);
#5677=LINE('',#82483,#10205);
#5678=LINE('',#82485,#10206);
#5679=LINE('',#82486,#10207);
#5680=LINE('',#82489,#10208);
#5681=LINE('',#82491,#10209);
#5682=LINE('',#82492,#10210);
#5683=LINE('',#82495,#10211);
#5684=LINE('',#82497,#10212);
#5685=LINE('',#82498,#10213);
#5686=LINE('',#82510,#10214);
#5687=LINE('',#82525,#10215);
#5688=LINE('',#82540,#10216);
#5689=LINE('',#82555,#10217);
#5690=LINE('',#82570,#10218);
#5691=LINE('',#82585,#10219);
#5692=LINE('',#82600,#10220);
#5693=LINE('',#82615,#10221);
#5694=LINE('',#82621,#10222);
#5695=LINE('',#82623,#10223);
#5696=LINE('',#82624,#10224);
#5697=LINE('',#82636,#10225);
#5698=LINE('',#82665,#10226);
#5699=LINE('',#82670,#10227);
#5700=LINE('',#82682,#10228);
#5701=LINE('',#82697,#10229);
#5702=LINE('',#82712,#10230);
#5703=LINE('',#82727,#10231);
#5704=LINE('',#82742,#10232);
#5705=LINE('',#82757,#10233);
#5706=LINE('',#82772,#10234);
#5707=LINE('',#82787,#10235);
#5708=LINE('',#82802,#10236);
#5709=LINE('',#82831,#10237);
#5710=LINE('',#82836,#10238);
#5711=LINE('',#82848,#10239);
#5712=LINE('',#82863,#10240);
#5713=LINE('',#82878,#10241);
#5714=LINE('',#82893,#10242);
#5715=LINE('',#82908,#10243);
#5716=LINE('',#82923,#10244);
#5717=LINE('',#82938,#10245);
#5718=LINE('',#82953,#10246);
#5719=LINE('',#82968,#10247);
#5720=LINE('',#82983,#10248);
#5721=LINE('',#82989,#10249);
#5722=LINE('',#82991,#10250);
#5723=LINE('',#82992,#10251);
#5724=LINE('',#83004,#10252);
#5725=LINE('',#83019,#10253);
#5726=LINE('',#83039,#10254);
#5727=LINE('',#83041,#10255);
#5728=LINE('',#83043,#10256);
#5729=LINE('',#83044,#10257);
#5730=LINE('',#83047,#10258);
#5731=LINE('',#83049,#10259);
#5732=LINE('',#83050,#10260);
#5733=LINE('',#83053,#10261);
#5734=LINE('',#83055,#10262);
#5735=LINE('',#83056,#10263);
#5736=LINE('',#83059,#10264);
#5737=LINE('',#83061,#10265);
#5738=LINE('',#83062,#10266);
#5739=LINE('',#83065,#10267);
#5740=LINE('',#83067,#10268);
#5741=LINE('',#83068,#10269);
#5742=LINE('',#83071,#10270);
#5743=LINE('',#83073,#10271);
#5744=LINE('',#83074,#10272);
#5745=LINE('',#83077,#10273);
#5746=LINE('',#83079,#10274);
#5747=LINE('',#83080,#10275);
#5748=LINE('',#83083,#10276);
#5749=LINE('',#83085,#10277);
#5750=LINE('',#83086,#10278);
#5751=LINE('',#83089,#10279);
#5752=LINE('',#83091,#10280);
#5753=LINE('',#83092,#10281);
#5754=LINE('',#83095,#10282);
#5755=LINE('',#83097,#10283);
#5756=LINE('',#83098,#10284);
#5757=LINE('',#83101,#10285);
#5758=LINE('',#83103,#10286);
#5759=LINE('',#83104,#10287);
#5760=LINE('',#83106,#10288);
#5761=LINE('',#83107,#10289);
#5762=LINE('',#83112,#10290);
#5763=LINE('',#83114,#10291);
#5764=LINE('',#83116,#10292);
#5765=LINE('',#83117,#10293);
#5766=LINE('',#83120,#10294);
#5767=LINE('',#83122,#10295);
#5768=LINE('',#83123,#10296);
#5769=LINE('',#83126,#10297);
#5770=LINE('',#83128,#10298);
#5771=LINE('',#83129,#10299);
#5772=LINE('',#83131,#10300);
#5773=LINE('',#83132,#10301);
#5774=LINE('',#83146,#10302);
#5775=LINE('',#83151,#10303);
#5776=LINE('',#83163,#10304);
#5777=LINE('',#83178,#10305);
#5778=LINE('',#83193,#10306);
#5779=LINE('',#83208,#10307);
#5780=LINE('',#83223,#10308);
#5781=LINE('',#83238,#10309);
#5782=LINE('',#83253,#10310);
#5783=LINE('',#83268,#10311);
#5784=LINE('',#83283,#10312);
#5785=LINE('',#83303,#10313);
#5786=LINE('',#83305,#10314);
#5787=LINE('',#83307,#10315);
#5788=LINE('',#83308,#10316);
#5789=LINE('',#83311,#10317);
#5790=LINE('',#83313,#10318);
#5791=LINE('',#83314,#10319);
#5792=LINE('',#83317,#10320);
#5793=LINE('',#83319,#10321);
#5794=LINE('',#83320,#10322);
#5795=LINE('',#83323,#10323);
#5796=LINE('',#83325,#10324);
#5797=LINE('',#83326,#10325);
#5798=LINE('',#83329,#10326);
#5799=LINE('',#83331,#10327);
#5800=LINE('',#83332,#10328);
#5801=LINE('',#83335,#10329);
#5802=LINE('',#83337,#10330);
#5803=LINE('',#83338,#10331);
#5804=LINE('',#83341,#10332);
#5805=LINE('',#83343,#10333);
#5806=LINE('',#83344,#10334);
#5807=LINE('',#83347,#10335);
#5808=LINE('',#83349,#10336);
#5809=LINE('',#83350,#10337);
#5810=LINE('',#83353,#10338);
#5811=LINE('',#83355,#10339);
#5812=LINE('',#83356,#10340);
#5813=LINE('',#83359,#10341);
#5814=LINE('',#83361,#10342);
#5815=LINE('',#83362,#10343);
#5816=LINE('',#83365,#10344);
#5817=LINE('',#83367,#10345);
#5818=LINE('',#83368,#10346);
#5819=LINE('',#83370,#10347);
#5820=LINE('',#83371,#10348);
#5821=LINE('',#83376,#10349);
#5822=LINE('',#83378,#10350);
#5823=LINE('',#83380,#10351);
#5824=LINE('',#83381,#10352);
#5825=LINE('',#83384,#10353);
#5826=LINE('',#83386,#10354);
#5827=LINE('',#83387,#10355);
#5828=LINE('',#83390,#10356);
#5829=LINE('',#83392,#10357);
#5830=LINE('',#83393,#10358);
#5831=LINE('',#83396,#10359);
#5832=LINE('',#83398,#10360);
#5833=LINE('',#83399,#10361);
#5834=LINE('',#83402,#10362);
#5835=LINE('',#83404,#10363);
#5836=LINE('',#83405,#10364);
#5837=LINE('',#83407,#10365);
#5838=LINE('',#83408,#10366);
#5839=LINE('',#83422,#10367);
#5840=LINE('',#83427,#10368);
#5841=LINE('',#83439,#10369);
#5842=LINE('',#83454,#10370);
#5843=LINE('',#83469,#10371);
#5844=LINE('',#83484,#10372);
#5845=LINE('',#83499,#10373);
#5846=LINE('',#83514,#10374);
#5847=LINE('',#83529,#10375);
#5848=LINE('',#83535,#10376);
#5849=LINE('',#83537,#10377);
#5850=LINE('',#83538,#10378);
#5851=LINE('',#83541,#10379);
#5852=LINE('',#83543,#10380);
#5853=LINE('',#83544,#10381);
#5854=LINE('',#83547,#10382);
#5855=LINE('',#83549,#10383);
#5856=LINE('',#83550,#10384);
#5857=LINE('',#83567,#10385);
#5858=LINE('',#83569,#10386);
#5859=LINE('',#83571,#10387);
#5860=LINE('',#83572,#10388);
#5861=LINE('',#83584,#10389);
#5862=LINE('',#83599,#10390);
#5863=LINE('',#83614,#10391);
#5864=LINE('',#83629,#10392);
#5865=LINE('',#83635,#10393);
#5866=LINE('',#83637,#10394);
#5867=LINE('',#83638,#10395);
#5868=LINE('',#83641,#10396);
#5869=LINE('',#83643,#10397);
#5870=LINE('',#83644,#10398);
#5871=LINE('',#83647,#10399);
#5872=LINE('',#83649,#10400);
#5873=LINE('',#83650,#10401);
#5874=LINE('',#83662,#10402);
#5875=LINE('',#83677,#10403);
#5876=LINE('',#83692,#10404);
#5877=LINE('',#83707,#10405);
#5878=LINE('',#83722,#10406);
#5879=LINE('',#83737,#10407);
#5880=LINE('',#83752,#10408);
#5881=LINE('',#83758,#10409);
#5882=LINE('',#83760,#10410);
#5883=LINE('',#83761,#10411);
#5884=LINE('',#83764,#10412);
#5885=LINE('',#83766,#10413);
#5886=LINE('',#83767,#10414);
#5887=LINE('',#83770,#10415);
#5888=LINE('',#83772,#10416);
#5889=LINE('',#83773,#10417);
#5890=LINE('',#83775,#10418);
#5891=LINE('',#83776,#10419);
#5892=LINE('',#83781,#10420);
#5893=LINE('',#83783,#10421);
#5894=LINE('',#83785,#10422);
#5895=LINE('',#83786,#10423);
#5896=LINE('',#83789,#10424);
#5897=LINE('',#83791,#10425);
#5898=LINE('',#83792,#10426);
#5899=LINE('',#83795,#10427);
#5900=LINE('',#83797,#10428);
#5901=LINE('',#83798,#10429);
#5902=LINE('',#83800,#10430);
#5903=LINE('',#83801,#10431);
#5904=LINE('',#83807,#10432);
#5905=LINE('',#83812,#10433);
#5906=LINE('',#83816,#10434);
#5907=LINE('',#83820,#10435);
#5908=LINE('',#83824,#10436);
#5909=LINE('',#83828,#10437);
#5910=LINE('',#83853,#10438);
#5911=LINE('',#83859,#10439);
#5912=LINE('',#83863,#10440);
#5913=LINE('',#83867,#10441);
#5914=LINE('',#83870,#10442);
#5915=LINE('',#83879,#10443);
#5916=LINE('',#83884,#10444);
#5917=LINE('',#83886,#10445);
#5918=LINE('',#83889,#10446);
#5919=LINE('',#83894,#10447);
#5920=LINE('',#83896,#10448);
#5921=LINE('',#83899,#10449);
#5922=LINE('',#83904,#10450);
#5923=LINE('',#83906,#10451);
#5924=LINE('',#83911,#10452);
#5925=LINE('',#83913,#10453);
#5926=LINE('',#83918,#10454);
#5927=LINE('',#83920,#10455);
#5928=LINE('',#83925,#10456);
#5929=LINE('',#83928,#10457);
#5930=LINE('',#83931,#10458);
#5931=LINE('',#83936,#10459);
#5932=LINE('',#83939,#10460);
#5933=LINE('',#83942,#10461);
#5934=LINE('',#83947,#10462);
#5935=LINE('',#83950,#10463);
#5936=LINE('',#83953,#10464);
#5937=LINE('',#83958,#10465);
#5938=LINE('',#83961,#10466);
#5939=LINE('',#83964,#10467);
#5940=LINE('',#83968,#10468);
#5941=LINE('',#83972,#10469);
#5942=LINE('',#83975,#10470);
#5943=LINE('',#83978,#10471);
#5944=LINE('',#83979,#10472);
#5945=LINE('',#83982,#10473);
#5946=LINE('',#83986,#10474);
#5947=LINE('',#83987,#10475);
#5948=LINE('',#83990,#10476);
#5949=LINE('',#83994,#10477);
#5950=LINE('',#83995,#10478);
#5951=LINE('',#83998,#10479);
#5952=LINE('',#84001,#10480);
#5953=LINE('',#84004,#10481);
#5954=LINE('',#84006,#10482);
#5955=LINE('',#84007,#10483);
#5956=LINE('',#84010,#10484);
#5957=LINE('',#84014,#10485);
#5958=LINE('',#84015,#10486);
#5959=LINE('',#84018,#10487);
#5960=LINE('',#84021,#10488);
#5961=LINE('',#84022,#10489);
#5962=LINE('',#84024,#10490);
#5963=LINE('',#84026,#10491);
#5964=LINE('',#84028,#10492);
#5965=LINE('',#84031,#10493);
#5966=LINE('',#84032,#10494);
#5967=LINE('',#84035,#10495);
#5968=LINE('',#84039,#10496);
#5969=LINE('',#84040,#10497);
#5970=LINE('',#84044,#10498);
#5971=LINE('',#84046,#10499);
#5972=LINE('',#84048,#10500);
#5973=LINE('',#84055,#10501);
#5974=LINE('',#84059,#10502);
#5975=LINE('',#84067,#10503);
#5976=LINE('',#84071,#10504);
#5977=LINE('',#84075,#10505);
#5978=LINE('',#84080,#10506);
#5979=LINE('',#84085,#10507);
#5980=LINE('',#84112,#10508);
#5981=LINE('',#84160,#10509);
#5982=LINE('',#84208,#10510);
#5983=LINE('',#84262,#10511);
#5984=LINE('',#84310,#10512);
#5985=LINE('',#84358,#10513);
#5986=LINE('',#84412,#10514);
#5987=LINE('',#84460,#10515);
#5988=LINE('',#84508,#10516);
#5989=LINE('',#84562,#10517);
#5990=LINE('',#84610,#10518);
#5991=LINE('',#84658,#10519);
#5992=LINE('',#84712,#10520);
#5993=LINE('',#84760,#10521);
#5994=LINE('',#84808,#10522);
#5995=LINE('',#84862,#10523);
#5996=LINE('',#84872,#10524);
#5997=LINE('',#84899,#10525);
#5998=LINE('',#84924,#10526);
#5999=LINE('',#84948,#10527);
#6000=LINE('',#84973,#10528);
#6001=LINE('',#84998,#10529);
#6002=LINE('',#85022,#10530);
#6003=LINE('',#85047,#10531);
#6004=LINE('',#85072,#10532);
#6005=LINE('',#85096,#10533);
#6006=LINE('',#85121,#10534);
#6007=LINE('',#85146,#10535);
#6008=LINE('',#85170,#10536);
#6009=LINE('',#85195,#10537);
#6010=LINE('',#85220,#10538);
#6011=LINE('',#86591,#10539);
#6012=LINE('',#86593,#10540);
#6013=LINE('',#86595,#10541);
#6014=LINE('',#86596,#10542);
#6015=LINE('',#86600,#10543);
#6016=LINE('',#86603,#10544);
#6017=LINE('',#86604,#10545);
#6018=LINE('',#86610,#10546);
#6019=LINE('',#86612,#10547);
#6020=LINE('',#86614,#10548);
#6021=LINE('',#86615,#10549);
#6022=LINE('',#86619,#10550);
#6023=LINE('',#86622,#10551);
#6024=LINE('',#86623,#10552);
#6025=LINE('',#86629,#10553);
#6026=LINE('',#86631,#10554);
#6027=LINE('',#86633,#10555);
#6028=LINE('',#86634,#10556);
#6029=LINE('',#86638,#10557);
#6030=LINE('',#86641,#10558);
#6031=LINE('',#86642,#10559);
#6032=LINE('',#86648,#10560);
#6033=LINE('',#86650,#10561);
#6034=LINE('',#86652,#10562);
#6035=LINE('',#86653,#10563);
#6036=LINE('',#86657,#10564);
#6037=LINE('',#86660,#10565);
#6038=LINE('',#86661,#10566);
#6039=LINE('',#86667,#10567);
#6040=LINE('',#86669,#10568);
#6041=LINE('',#86671,#10569);
#6042=LINE('',#86672,#10570);
#6043=LINE('',#86676,#10571);
#6044=LINE('',#86679,#10572);
#6045=LINE('',#86680,#10573);
#6046=LINE('',#86686,#10574);
#6047=LINE('',#86688,#10575);
#6048=LINE('',#86690,#10576);
#6049=LINE('',#86691,#10577);
#6050=LINE('',#86695,#10578);
#6051=LINE('',#86698,#10579);
#6052=LINE('',#86699,#10580);
#6053=LINE('',#86705,#10581);
#6054=LINE('',#86707,#10582);
#6055=LINE('',#86709,#10583);
#6056=LINE('',#86710,#10584);
#6057=LINE('',#86714,#10585);
#6058=LINE('',#86717,#10586);
#6059=LINE('',#86718,#10587);
#6060=LINE('',#86724,#10588);
#6061=LINE('',#86726,#10589);
#6062=LINE('',#86728,#10590);
#6063=LINE('',#86729,#10591);
#6064=LINE('',#86733,#10592);
#6065=LINE('',#86736,#10593);
#6066=LINE('',#86737,#10594);
#6067=LINE('',#86743,#10595);
#6068=LINE('',#86745,#10596);
#6069=LINE('',#86747,#10597);
#6070=LINE('',#86748,#10598);
#6071=LINE('',#86752,#10599);
#6072=LINE('',#86755,#10600);
#6073=LINE('',#86756,#10601);
#6074=LINE('',#86762,#10602);
#6075=LINE('',#86764,#10603);
#6076=LINE('',#86766,#10604);
#6077=LINE('',#86767,#10605);
#6078=LINE('',#86771,#10606);
#6079=LINE('',#86774,#10607);
#6080=LINE('',#86775,#10608);
#6081=LINE('',#86781,#10609);
#6082=LINE('',#86783,#10610);
#6083=LINE('',#86785,#10611);
#6084=LINE('',#86786,#10612);
#6085=LINE('',#86790,#10613);
#6086=LINE('',#86793,#10614);
#6087=LINE('',#86794,#10615);
#6088=LINE('',#86800,#10616);
#6089=LINE('',#86802,#10617);
#6090=LINE('',#86804,#10618);
#6091=LINE('',#86805,#10619);
#6092=LINE('',#86809,#10620);
#6093=LINE('',#86812,#10621);
#6094=LINE('',#86813,#10622);
#6095=LINE('',#86819,#10623);
#6096=LINE('',#86821,#10624);
#6097=LINE('',#86823,#10625);
#6098=LINE('',#86824,#10626);
#6099=LINE('',#86828,#10627);
#6100=LINE('',#86831,#10628);
#6101=LINE('',#86832,#10629);
#6102=LINE('',#86838,#10630);
#6103=LINE('',#86840,#10631);
#6104=LINE('',#86842,#10632);
#6105=LINE('',#86843,#10633);
#6106=LINE('',#86847,#10634);
#6107=LINE('',#86850,#10635);
#6108=LINE('',#86851,#10636);
#6109=LINE('',#86857,#10637);
#6110=LINE('',#86859,#10638);
#6111=LINE('',#86861,#10639);
#6112=LINE('',#86862,#10640);
#6113=LINE('',#86866,#10641);
#6114=LINE('',#86869,#10642);
#6115=LINE('',#86870,#10643);
#6116=LINE('',#86876,#10644);
#6117=LINE('',#86878,#10645);
#6118=LINE('',#86880,#10646);
#6119=LINE('',#86881,#10647);
#6120=LINE('',#86885,#10648);
#6121=LINE('',#86888,#10649);
#6122=LINE('',#86889,#10650);
#6123=LINE('',#86895,#10651);
#6124=LINE('',#86897,#10652);
#6125=LINE('',#86899,#10653);
#6126=LINE('',#86900,#10654);
#6127=LINE('',#86904,#10655);
#6128=LINE('',#86907,#10656);
#6129=LINE('',#86908,#10657);
#6130=LINE('',#86914,#10658);
#6131=LINE('',#86916,#10659);
#6132=LINE('',#86918,#10660);
#6133=LINE('',#86919,#10661);
#6134=LINE('',#86924,#10662);
#6135=LINE('',#86928,#10663);
#6136=LINE('',#86929,#10664);
#6137=LINE('',#86937,#10665);
#6138=LINE('',#86939,#10666);
#6139=LINE('',#86941,#10667);
#6140=LINE('',#86942,#10668);
#6141=LINE('',#86946,#10669);
#6142=LINE('',#86949,#10670);
#6143=LINE('',#86950,#10671);
#6144=LINE('',#86956,#10672);
#6145=LINE('',#86958,#10673);
#6146=LINE('',#86960,#10674);
#6147=LINE('',#86961,#10675);
#6148=LINE('',#86965,#10676);
#6149=LINE('',#86968,#10677);
#6150=LINE('',#86969,#10678);
#6151=LINE('',#86975,#10679);
#6152=LINE('',#86977,#10680);
#6153=LINE('',#86979,#10681);
#6154=LINE('',#86980,#10682);
#6155=LINE('',#86984,#10683);
#6156=LINE('',#86987,#10684);
#6157=LINE('',#86988,#10685);
#6158=LINE('',#86994,#10686);
#6159=LINE('',#86996,#10687);
#6160=LINE('',#86998,#10688);
#6161=LINE('',#86999,#10689);
#6162=LINE('',#87003,#10690);
#6163=LINE('',#87006,#10691);
#6164=LINE('',#87007,#10692);
#6165=LINE('',#87013,#10693);
#6166=LINE('',#87015,#10694);
#6167=LINE('',#87017,#10695);
#6168=LINE('',#87018,#10696);
#6169=LINE('',#87022,#10697);
#6170=LINE('',#87025,#10698);
#6171=LINE('',#87026,#10699);
#6172=LINE('',#87032,#10700);
#6173=LINE('',#87034,#10701);
#6174=LINE('',#87036,#10702);
#6175=LINE('',#87037,#10703);
#6176=LINE('',#87041,#10704);
#6177=LINE('',#87044,#10705);
#6178=LINE('',#87045,#10706);
#6179=LINE('',#87051,#10707);
#6180=LINE('',#87053,#10708);
#6181=LINE('',#87055,#10709);
#6182=LINE('',#87056,#10710);
#6183=LINE('',#87060,#10711);
#6184=LINE('',#87063,#10712);
#6185=LINE('',#87064,#10713);
#6186=LINE('',#87070,#10714);
#6187=LINE('',#87072,#10715);
#6188=LINE('',#87074,#10716);
#6189=LINE('',#87075,#10717);
#6190=LINE('',#87079,#10718);
#6191=LINE('',#87082,#10719);
#6192=LINE('',#87083,#10720);
#6193=LINE('',#87089,#10721);
#6194=LINE('',#87091,#10722);
#6195=LINE('',#87093,#10723);
#6196=LINE('',#87094,#10724);
#6197=LINE('',#87098,#10725);
#6198=LINE('',#87101,#10726);
#6199=LINE('',#87102,#10727);
#6200=LINE('',#87108,#10728);
#6201=LINE('',#87110,#10729);
#6202=LINE('',#87112,#10730);
#6203=LINE('',#87113,#10731);
#6204=LINE('',#87117,#10732);
#6205=LINE('',#87120,#10733);
#6206=LINE('',#87121,#10734);
#6207=LINE('',#87127,#10735);
#6208=LINE('',#87129,#10736);
#6209=LINE('',#87131,#10737);
#6210=LINE('',#87132,#10738);
#6211=LINE('',#87136,#10739);
#6212=LINE('',#87139,#10740);
#6213=LINE('',#87140,#10741);
#6214=LINE('',#87146,#10742);
#6215=LINE('',#87148,#10743);
#6216=LINE('',#87150,#10744);
#6217=LINE('',#87151,#10745);
#6218=LINE('',#87155,#10746);
#6219=LINE('',#87158,#10747);
#6220=LINE('',#87159,#10748);
#6221=LINE('',#87165,#10749);
#6222=LINE('',#87167,#10750);
#6223=LINE('',#87169,#10751);
#6224=LINE('',#87170,#10752);
#6225=LINE('',#87174,#10753);
#6226=LINE('',#87177,#10754);
#6227=LINE('',#87178,#10755);
#6228=LINE('',#87184,#10756);
#6229=LINE('',#87186,#10757);
#6230=LINE('',#87188,#10758);
#6231=LINE('',#87189,#10759);
#6232=LINE('',#87193,#10760);
#6233=LINE('',#87196,#10761);
#6234=LINE('',#87197,#10762);
#6235=LINE('',#87203,#10763);
#6236=LINE('',#87205,#10764);
#6237=LINE('',#87207,#10765);
#6238=LINE('',#87208,#10766);
#6239=LINE('',#87212,#10767);
#6240=LINE('',#87215,#10768);
#6241=LINE('',#87216,#10769);
#6242=LINE('',#87222,#10770);
#6243=LINE('',#87224,#10771);
#6244=LINE('',#87226,#10772);
#6245=LINE('',#87227,#10773);
#6246=LINE('',#87231,#10774);
#6247=LINE('',#87234,#10775);
#6248=LINE('',#87235,#10776);
#6249=LINE('',#87241,#10777);
#6250=LINE('',#87243,#10778);
#6251=LINE('',#87245,#10779);
#6252=LINE('',#87246,#10780);
#6253=LINE('',#87250,#10781);
#6254=LINE('',#87253,#10782);
#6255=LINE('',#87254,#10783);
#6256=LINE('',#87262,#10784);
#6257=LINE('',#87263,#10785);
#6258=LINE('',#87266,#10786);
#6259=LINE('',#87268,#10787);
#6260=LINE('',#87269,#10788);
#6261=LINE('',#87272,#10789);
#6262=LINE('',#87273,#10790);
#6263=LINE('',#87279,#10791);
#6264=LINE('',#87284,#10792);
#6265=LINE('',#87286,#10793);
#6266=LINE('',#87288,#10794);
#6267=LINE('',#87289,#10795);
#6268=LINE('',#87292,#10796);
#6269=LINE('',#87294,#10797);
#6270=LINE('',#87295,#10798);
#6271=LINE('',#87298,#10799);
#6272=LINE('',#87300,#10800);
#6273=LINE('',#87301,#10801);
#6274=LINE('',#87304,#10802);
#6275=LINE('',#87306,#10803);
#6276=LINE('',#87307,#10804);
#6277=LINE('',#87310,#10805);
#6278=LINE('',#87312,#10806);
#6279=LINE('',#87313,#10807);
#6280=LINE('',#87315,#10808);
#6281=LINE('',#87316,#10809);
#6282=LINE('',#87322,#10810);
#6283=LINE('',#87341,#10811);
#6284=LINE('',#87364,#10812);
#6285=LINE('',#87371,#10813);
#6286=LINE('',#87376,#10814);
#6287=LINE('',#87380,#10815);
#6288=LINE('',#87386,#10816);
#6289=LINE('',#87390,#10817);
#6290=LINE('',#87394,#10818);
#6291=LINE('',#87401,#10819);
#6292=LINE('',#87410,#10820);
#6293=LINE('',#87422,#10821);
#6294=LINE('',#87434,#10822);
#6295=LINE('',#87451,#10823);
#6296=LINE('',#87459,#10824);
#6297=LINE('',#87480,#10825);
#6298=LINE('',#87504,#10826);
#6299=LINE('',#87552,#10827);
#6300=LINE('',#87600,#10828);
#6301=LINE('',#87654,#10829);
#6302=LINE('',#87702,#10830);
#6303=LINE('',#87750,#10831);
#6304=LINE('',#87798,#10832);
#6305=LINE('',#87852,#10833);
#6306=LINE('',#87900,#10834);
#6307=LINE('',#87948,#10835);
#6308=LINE('',#88002,#10836);
#6309=LINE('',#88050,#10837);
#6310=LINE('',#88098,#10838);
#6311=LINE('',#88152,#10839);
#6312=LINE('',#88200,#10840);
#6313=LINE('',#88247,#10841);
#6314=LINE('',#88267,#10842);
#6315=LINE('',#88291,#10843);
#6316=LINE('',#88316,#10844);
#6317=LINE('',#88341,#10845);
#6318=LINE('',#88365,#10846);
#6319=LINE('',#88390,#10847);
#6320=LINE('',#88415,#10848);
#6321=LINE('',#88439,#10849);
#6322=LINE('',#88464,#10850);
#6323=LINE('',#88489,#10851);
#6324=LINE('',#88513,#10852);
#6325=LINE('',#88537,#10853);
#6326=LINE('',#88562,#10854);
#6327=LINE('',#88587,#10855);
#6328=LINE('',#89832,#10856);
#6329=LINE('',#89834,#10857);
#6330=LINE('',#89836,#10858);
#6331=LINE('',#89837,#10859);
#6332=LINE('',#89841,#10860);
#6333=LINE('',#89844,#10861);
#6334=LINE('',#89845,#10862);
#6335=LINE('',#89851,#10863);
#6336=LINE('',#89853,#10864);
#6337=LINE('',#89855,#10865);
#6338=LINE('',#89856,#10866);
#6339=LINE('',#89860,#10867);
#6340=LINE('',#89863,#10868);
#6341=LINE('',#89864,#10869);
#6342=LINE('',#89870,#10870);
#6343=LINE('',#89872,#10871);
#6344=LINE('',#89874,#10872);
#6345=LINE('',#89875,#10873);
#6346=LINE('',#89879,#10874);
#6347=LINE('',#89882,#10875);
#6348=LINE('',#89883,#10876);
#6349=LINE('',#89889,#10877);
#6350=LINE('',#89891,#10878);
#6351=LINE('',#89893,#10879);
#6352=LINE('',#89894,#10880);
#6353=LINE('',#89898,#10881);
#6354=LINE('',#89901,#10882);
#6355=LINE('',#89902,#10883);
#6356=LINE('',#89908,#10884);
#6357=LINE('',#89910,#10885);
#6358=LINE('',#89912,#10886);
#6359=LINE('',#89913,#10887);
#6360=LINE('',#89917,#10888);
#6361=LINE('',#89920,#10889);
#6362=LINE('',#89921,#10890);
#6363=LINE('',#89927,#10891);
#6364=LINE('',#89929,#10892);
#6365=LINE('',#89931,#10893);
#6366=LINE('',#89932,#10894);
#6367=LINE('',#89936,#10895);
#6368=LINE('',#89939,#10896);
#6369=LINE('',#89940,#10897);
#6370=LINE('',#89946,#10898);
#6371=LINE('',#89948,#10899);
#6372=LINE('',#89950,#10900);
#6373=LINE('',#89951,#10901);
#6374=LINE('',#89955,#10902);
#6375=LINE('',#89958,#10903);
#6376=LINE('',#89959,#10904);
#6377=LINE('',#89965,#10905);
#6378=LINE('',#89967,#10906);
#6379=LINE('',#89969,#10907);
#6380=LINE('',#89970,#10908);
#6381=LINE('',#89974,#10909);
#6382=LINE('',#89977,#10910);
#6383=LINE('',#89978,#10911);
#6384=LINE('',#89984,#10912);
#6385=LINE('',#89986,#10913);
#6386=LINE('',#89988,#10914);
#6387=LINE('',#89989,#10915);
#6388=LINE('',#89993,#10916);
#6389=LINE('',#89996,#10917);
#6390=LINE('',#89997,#10918);
#6391=LINE('',#90003,#10919);
#6392=LINE('',#90005,#10920);
#6393=LINE('',#90007,#10921);
#6394=LINE('',#90008,#10922);
#6395=LINE('',#90012,#10923);
#6396=LINE('',#90015,#10924);
#6397=LINE('',#90016,#10925);
#6398=LINE('',#90022,#10926);
#6399=LINE('',#90024,#10927);
#6400=LINE('',#90026,#10928);
#6401=LINE('',#90027,#10929);
#6402=LINE('',#90031,#10930);
#6403=LINE('',#90034,#10931);
#6404=LINE('',#90035,#10932);
#6405=LINE('',#90041,#10933);
#6406=LINE('',#90043,#10934);
#6407=LINE('',#90045,#10935);
#6408=LINE('',#90046,#10936);
#6409=LINE('',#90050,#10937);
#6410=LINE('',#90053,#10938);
#6411=LINE('',#90054,#10939);
#6412=LINE('',#90060,#10940);
#6413=LINE('',#90062,#10941);
#6414=LINE('',#90064,#10942);
#6415=LINE('',#90065,#10943);
#6416=LINE('',#90069,#10944);
#6417=LINE('',#90072,#10945);
#6418=LINE('',#90073,#10946);
#6419=LINE('',#90079,#10947);
#6420=LINE('',#90081,#10948);
#6421=LINE('',#90083,#10949);
#6422=LINE('',#90084,#10950);
#6423=LINE('',#90088,#10951);
#6424=LINE('',#90091,#10952);
#6425=LINE('',#90092,#10953);
#6426=LINE('',#90098,#10954);
#6427=LINE('',#90100,#10955);
#6428=LINE('',#90102,#10956);
#6429=LINE('',#90103,#10957);
#6430=LINE('',#90107,#10958);
#6431=LINE('',#90110,#10959);
#6432=LINE('',#90111,#10960);
#6433=LINE('',#90117,#10961);
#6434=LINE('',#90119,#10962);
#6435=LINE('',#90121,#10963);
#6436=LINE('',#90122,#10964);
#6437=LINE('',#90126,#10965);
#6438=LINE('',#90129,#10966);
#6439=LINE('',#90130,#10967);
#6440=LINE('',#90136,#10968);
#6441=LINE('',#90138,#10969);
#6442=LINE('',#90140,#10970);
#6443=LINE('',#90141,#10971);
#6444=LINE('',#90145,#10972);
#6445=LINE('',#90148,#10973);
#6446=LINE('',#90149,#10974);
#6447=LINE('',#90155,#10975);
#6448=LINE('',#90157,#10976);
#6449=LINE('',#90159,#10977);
#6450=LINE('',#90160,#10978);
#6451=LINE('',#90165,#10979);
#6452=LINE('',#90169,#10980);
#6453=LINE('',#90170,#10981);
#6454=LINE('',#90178,#10982);
#6455=LINE('',#90180,#10983);
#6456=LINE('',#90182,#10984);
#6457=LINE('',#90183,#10985);
#6458=LINE('',#90187,#10986);
#6459=LINE('',#90190,#10987);
#6460=LINE('',#90191,#10988);
#6461=LINE('',#90197,#10989);
#6462=LINE('',#90199,#10990);
#6463=LINE('',#90201,#10991);
#6464=LINE('',#90202,#10992);
#6465=LINE('',#90206,#10993);
#6466=LINE('',#90209,#10994);
#6467=LINE('',#90210,#10995);
#6468=LINE('',#90216,#10996);
#6469=LINE('',#90218,#10997);
#6470=LINE('',#90220,#10998);
#6471=LINE('',#90221,#10999);
#6472=LINE('',#90225,#11000);
#6473=LINE('',#90228,#11001);
#6474=LINE('',#90229,#11002);
#6475=LINE('',#90235,#11003);
#6476=LINE('',#90237,#11004);
#6477=LINE('',#90239,#11005);
#6478=LINE('',#90240,#11006);
#6479=LINE('',#90244,#11007);
#6480=LINE('',#90247,#11008);
#6481=LINE('',#90248,#11009);
#6482=LINE('',#90254,#11010);
#6483=LINE('',#90256,#11011);
#6484=LINE('',#90258,#11012);
#6485=LINE('',#90259,#11013);
#6486=LINE('',#90263,#11014);
#6487=LINE('',#90266,#11015);
#6488=LINE('',#90267,#11016);
#6489=LINE('',#90273,#11017);
#6490=LINE('',#90275,#11018);
#6491=LINE('',#90277,#11019);
#6492=LINE('',#90278,#11020);
#6493=LINE('',#90282,#11021);
#6494=LINE('',#90285,#11022);
#6495=LINE('',#90286,#11023);
#6496=LINE('',#90292,#11024);
#6497=LINE('',#90294,#11025);
#6498=LINE('',#90296,#11026);
#6499=LINE('',#90297,#11027);
#6500=LINE('',#90301,#11028);
#6501=LINE('',#90304,#11029);
#6502=LINE('',#90305,#11030);
#6503=LINE('',#90311,#11031);
#6504=LINE('',#90313,#11032);
#6505=LINE('',#90315,#11033);
#6506=LINE('',#90316,#11034);
#6507=LINE('',#90320,#11035);
#6508=LINE('',#90323,#11036);
#6509=LINE('',#90324,#11037);
#6510=LINE('',#90330,#11038);
#6511=LINE('',#90332,#11039);
#6512=LINE('',#90334,#11040);
#6513=LINE('',#90335,#11041);
#6514=LINE('',#90339,#11042);
#6515=LINE('',#90342,#11043);
#6516=LINE('',#90343,#11044);
#6517=LINE('',#90349,#11045);
#6518=LINE('',#90351,#11046);
#6519=LINE('',#90353,#11047);
#6520=LINE('',#90354,#11048);
#6521=LINE('',#90358,#11049);
#6522=LINE('',#90361,#11050);
#6523=LINE('',#90362,#11051);
#6524=LINE('',#90368,#11052);
#6525=LINE('',#90370,#11053);
#6526=LINE('',#90372,#11054);
#6527=LINE('',#90373,#11055);
#6528=LINE('',#90377,#11056);
#6529=LINE('',#90380,#11057);
#6530=LINE('',#90381,#11058);
#6531=LINE('',#90387,#11059);
#6532=LINE('',#90389,#11060);
#6533=LINE('',#90391,#11061);
#6534=LINE('',#90392,#11062);
#6535=LINE('',#90396,#11063);
#6536=LINE('',#90399,#11064);
#6537=LINE('',#90400,#11065);
#6538=LINE('',#90406,#11066);
#6539=LINE('',#90408,#11067);
#6540=LINE('',#90410,#11068);
#6541=LINE('',#90411,#11069);
#6542=LINE('',#90415,#11070);
#6543=LINE('',#90418,#11071);
#6544=LINE('',#90419,#11072);
#6545=LINE('',#90425,#11073);
#6546=LINE('',#90427,#11074);
#6547=LINE('',#90429,#11075);
#6548=LINE('',#90430,#11076);
#6549=LINE('',#90434,#11077);
#6550=LINE('',#90437,#11078);
#6551=LINE('',#90438,#11079);
#6552=LINE('',#90444,#11080);
#6553=LINE('',#90446,#11081);
#6554=LINE('',#90448,#11082);
#6555=LINE('',#90449,#11083);
#6556=LINE('',#90453,#11084);
#6557=LINE('',#90456,#11085);
#6558=LINE('',#90457,#11086);
#6559=LINE('',#90463,#11087);
#6560=LINE('',#90465,#11088);
#6561=LINE('',#90467,#11089);
#6562=LINE('',#90468,#11090);
#6563=LINE('',#90472,#11091);
#6564=LINE('',#90475,#11092);
#6565=LINE('',#90476,#11093);
#6566=LINE('',#90482,#11094);
#6567=LINE('',#90484,#11095);
#6568=LINE('',#90486,#11096);
#6569=LINE('',#90487,#11097);
#6570=LINE('',#90491,#11098);
#6571=LINE('',#90494,#11099);
#6572=LINE('',#90495,#11100);
#6573=LINE('',#90503,#11101);
#6574=LINE('',#90504,#11102);
#6575=LINE('',#90507,#11103);
#6576=LINE('',#90509,#11104);
#6577=LINE('',#90510,#11105);
#6578=LINE('',#90513,#11106);
#6579=LINE('',#90514,#11107);
#6580=LINE('',#90520,#11108);
#6581=LINE('',#90525,#11109);
#6582=LINE('',#90527,#11110);
#6583=LINE('',#90529,#11111);
#6584=LINE('',#90530,#11112);
#6585=LINE('',#90533,#11113);
#6586=LINE('',#90535,#11114);
#6587=LINE('',#90536,#11115);
#6588=LINE('',#90539,#11116);
#6589=LINE('',#90541,#11117);
#6590=LINE('',#90542,#11118);
#6591=LINE('',#90545,#11119);
#6592=LINE('',#90547,#11120);
#6593=LINE('',#90548,#11121);
#6594=LINE('',#90551,#11122);
#6595=LINE('',#90553,#11123);
#6596=LINE('',#90554,#11124);
#6597=LINE('',#90556,#11125);
#6598=LINE('',#90557,#11126);
#6599=LINE('',#90563,#11127);
#6600=LINE('',#90582,#11128);
#6601=LINE('',#90605,#11129);
#6602=LINE('',#90618,#11130);
#6603=LINE('',#90627,#11131);
#6604=LINE('',#90629,#11132);
#6605=LINE('',#90634,#11133);
#6606=LINE('',#90658,#11134);
#6607=LINE('',#90706,#11135);
#6608=LINE('',#90754,#11136);
#6609=LINE('',#90808,#11137);
#6610=LINE('',#90856,#11138);
#6611=LINE('',#90904,#11139);
#6612=LINE('',#90958,#11140);
#6613=LINE('',#91006,#11141);
#6614=LINE('',#91054,#11142);
#6615=LINE('',#91102,#11143);
#6616=LINE('',#91156,#11144);
#6617=LINE('',#91204,#11145);
#6618=LINE('',#91252,#11146);
#6619=LINE('',#91306,#11147);
#6620=LINE('',#91354,#11148);
#6621=LINE('',#91402,#11149);
#6622=LINE('',#91456,#11150);
#6623=LINE('',#91504,#11151);
#6624=LINE('',#91552,#11152);
#6625=LINE('',#91606,#11153);
#6626=LINE('',#91654,#11154);
#6627=LINE('',#91702,#11155);
#6628=LINE('',#91756,#11156);
#6629=LINE('',#91774,#11157);
#6630=LINE('',#91799,#11158);
#6631=LINE('',#91824,#11159);
#6632=LINE('',#91848,#11160);
#6633=LINE('',#91873,#11161);
#6634=LINE('',#91898,#11162);
#6635=LINE('',#91922,#11163);
#6636=LINE('',#91947,#11164);
#6637=LINE('',#91972,#11165);
#6638=LINE('',#91996,#11166);
#6639=LINE('',#92021,#11167);
#6640=LINE('',#92046,#11168);
#6641=LINE('',#92070,#11169);
#6642=LINE('',#92095,#11170);
#6643=LINE('',#92120,#11171);
#6644=LINE('',#92144,#11172);
#6645=LINE('',#92168,#11173);
#6646=LINE('',#92193,#11174);
#6647=LINE('',#92218,#11175);
#6648=LINE('',#92242,#11176);
#6649=LINE('',#92267,#11177);
#6650=LINE('',#92292,#11178);
#6651=LINE('',#94007,#11179);
#6652=LINE('',#94014,#11180);
#6653=LINE('',#94016,#11181);
#6654=LINE('',#94017,#11182);
#6655=LINE('',#94020,#11183);
#6656=LINE('',#94021,#11184);
#6657=LINE('',#94024,#11185);
#6658=LINE('',#94025,#11186);
#6659=LINE('',#94029,#11187);
#6660=LINE('',#94034,#11188);
#6661=LINE('',#94037,#11189);
#6662=LINE('',#94038,#11190);
#6663=LINE('',#94041,#11191);
#6664=LINE('',#94042,#11192);
#6665=LINE('',#94044,#11193);
#6666=LINE('',#94052,#11194);
#6667=LINE('',#94057,#11195);
#6668=LINE('',#94061,#11196);
#6669=LINE('',#94067,#11197);
#6670=LINE('',#94071,#11198);
#6671=LINE('',#94075,#11199);
#6672=LINE('',#94082,#11200);
#6673=LINE('',#94095,#11201);
#6674=LINE('',#94107,#11202);
#6675=LINE('',#94126,#11203);
#6676=LINE('',#94134,#11204);
#6677=LINE('',#94156,#11205);
#6678=LINE('',#94160,#11206);
#6679=LINE('',#94164,#11207);
#6680=LINE('',#94170,#11208);
#6681=LINE('',#94196,#11209);
#6682=LINE('',#94201,#11210);
#6683=LINE('',#94204,#11211);
#6684=LINE('',#94210,#11212);
#6685=LINE('',#94224,#11213);
#6686=LINE('',#94230,#11214);
#6687=LINE('',#94232,#11215);
#6688=VECTOR('',#55518,10.);
#6689=VECTOR('',#55519,10.);
#6690=VECTOR('',#55520,10.);
#6691=VECTOR('',#55521,10.);
#6692=VECTOR('',#55522,10.);
#6693=VECTOR('',#55523,10.);
#6694=VECTOR('',#55524,10.);
#6695=VECTOR('',#55525,10.);
#6696=VECTOR('',#55526,10.);
#6697=VECTOR('',#55527,10.);
#6698=VECTOR('',#55528,10.);
#6699=VECTOR('',#55529,10.);
#6700=VECTOR('',#55530,10.);
#6701=VECTOR('',#55531,10.);
#6702=VECTOR('',#55532,10.);
#6703=VECTOR('',#55533,10.);
#6704=VECTOR('',#55534,10.);
#6705=VECTOR('',#55535,10.);
#6706=VECTOR('',#55536,10.);
#6707=VECTOR('',#55537,10.);
#6708=VECTOR('',#55538,10.);
#6709=VECTOR('',#55539,10.);
#6710=VECTOR('',#55540,10.);
#6711=VECTOR('',#55541,10.);
#6712=VECTOR('',#55542,10.);
#6713=VECTOR('',#55543,10.);
#6714=VECTOR('',#55544,10.);
#6715=VECTOR('',#55545,10.);
#6716=VECTOR('',#55546,10.);
#6717=VECTOR('',#55547,10.);
#6718=VECTOR('',#55550,10.);
#6719=VECTOR('',#55551,10.);
#6720=VECTOR('',#55554,10.);
#6721=VECTOR('',#55557,10.);
#6722=VECTOR('',#55558,10.);
#6723=VECTOR('',#55559,10.);
#6724=VECTOR('',#55560,10.);
#6725=VECTOR('',#55561,10.);
#6726=VECTOR('',#55562,10.);
#6727=VECTOR('',#55563,10.);
#6728=VECTOR('',#55564,10.);
#6729=VECTOR('',#55565,10.);
#6730=VECTOR('',#55566,10.);
#6731=VECTOR('',#55567,10.);
#6732=VECTOR('',#55568,10.);
#6733=VECTOR('',#55569,10.);
#6734=VECTOR('',#55570,10.);
#6735=VECTOR('',#55571,10.);
#6736=VECTOR('',#55572,10.);
#6737=VECTOR('',#55573,10.);
#6738=VECTOR('',#55574,10.);
#6739=VECTOR('',#55575,10.);
#6740=VECTOR('',#55576,10.);
#6741=VECTOR('',#55577,10.);
#6742=VECTOR('',#55578,10.);
#6743=VECTOR('',#55579,10.);
#6744=VECTOR('',#55580,10.);
#6745=VECTOR('',#55581,10.);
#6746=VECTOR('',#55582,10.);
#6747=VECTOR('',#55583,10.);
#6748=VECTOR('',#55584,10.);
#6749=VECTOR('',#55585,10.);
#6750=VECTOR('',#55586,10.);
#6751=VECTOR('',#55589,10.);
#6752=VECTOR('',#55590,10.);
#6753=VECTOR('',#55593,10.);
#6754=VECTOR('',#55596,10.);
#6755=VECTOR('',#55597,10.);
#6756=VECTOR('',#55598,10.);
#6757=VECTOR('',#55599,10.);
#6758=VECTOR('',#55600,10.);
#6759=VECTOR('',#55601,10.);
#6760=VECTOR('',#55602,10.);
#6761=VECTOR('',#55603,10.);
#6762=VECTOR('',#55604,10.);
#6763=VECTOR('',#55605,10.);
#6764=VECTOR('',#55606,10.);
#6765=VECTOR('',#55607,10.);
#6766=VECTOR('',#55608,10.);
#6767=VECTOR('',#55609,10.);
#6768=VECTOR('',#55610,10.);
#6769=VECTOR('',#55611,10.);
#6770=VECTOR('',#55612,10.);
#6771=VECTOR('',#55613,10.);
#6772=VECTOR('',#55614,10.);
#6773=VECTOR('',#55615,10.);
#6774=VECTOR('',#55616,10.);
#6775=VECTOR('',#55617,10.);
#6776=VECTOR('',#55618,10.);
#6777=VECTOR('',#55619,10.);
#6778=VECTOR('',#55620,10.);
#6779=VECTOR('',#55621,10.);
#6780=VECTOR('',#55622,10.);
#6781=VECTOR('',#55623,10.);
#6782=VECTOR('',#55624,10.);
#6783=VECTOR('',#55625,10.);
#6784=VECTOR('',#55628,10.);
#6785=VECTOR('',#55629,10.);
#6786=VECTOR('',#55632,10.);
#6787=VECTOR('',#55635,10.);
#6788=VECTOR('',#55636,10.);
#6789=VECTOR('',#55637,10.);
#6790=VECTOR('',#55638,10.);
#6791=VECTOR('',#55639,10.);
#6792=VECTOR('',#55640,10.);
#6793=VECTOR('',#55641,10.);
#6794=VECTOR('',#55642,10.);
#6795=VECTOR('',#55643,10.);
#6796=VECTOR('',#55644,10.);
#6797=VECTOR('',#55645,10.);
#6798=VECTOR('',#55646,10.);
#6799=VECTOR('',#55647,10.);
#6800=VECTOR('',#55648,10.);
#6801=VECTOR('',#55649,10.);
#6802=VECTOR('',#55650,10.);
#6803=VECTOR('',#55651,10.);
#6804=VECTOR('',#55652,10.);
#6805=VECTOR('',#55653,10.);
#6806=VECTOR('',#55654,10.);
#6807=VECTOR('',#55655,10.);
#6808=VECTOR('',#55656,10.);
#6809=VECTOR('',#55657,10.);
#6810=VECTOR('',#55658,10.);
#6811=VECTOR('',#55659,10.);
#6812=VECTOR('',#55660,10.);
#6813=VECTOR('',#55661,10.);
#6814=VECTOR('',#55662,10.);
#6815=VECTOR('',#55663,10.);
#6816=VECTOR('',#55664,10.);
#6817=VECTOR('',#55667,10.);
#6818=VECTOR('',#55668,10.);
#6819=VECTOR('',#55671,10.);
#6820=VECTOR('',#55674,10.);
#6821=VECTOR('',#55675,10.);
#6822=VECTOR('',#55676,10.);
#6823=VECTOR('',#55677,10.);
#6824=VECTOR('',#55678,10.);
#6825=VECTOR('',#55679,10.);
#6826=VECTOR('',#55680,10.);
#6827=VECTOR('',#55681,10.);
#6828=VECTOR('',#55682,10.);
#6829=VECTOR('',#55683,10.);
#6830=VECTOR('',#55684,10.);
#6831=VECTOR('',#55685,10.);
#6832=VECTOR('',#55686,10.);
#6833=VECTOR('',#55687,10.);
#6834=VECTOR('',#55688,10.);
#6835=VECTOR('',#55689,10.);
#6836=VECTOR('',#55690,10.);
#6837=VECTOR('',#55691,10.);
#6838=VECTOR('',#55692,10.);
#6839=VECTOR('',#55693,10.);
#6840=VECTOR('',#55694,10.);
#6841=VECTOR('',#55695,10.);
#6842=VECTOR('',#55696,10.);
#6843=VECTOR('',#55697,10.);
#6844=VECTOR('',#55698,10.);
#6845=VECTOR('',#55699,10.);
#6846=VECTOR('',#55700,10.);
#6847=VECTOR('',#55701,10.);
#6848=VECTOR('',#55702,10.);
#6849=VECTOR('',#55703,10.);
#6850=VECTOR('',#55706,10.);
#6851=VECTOR('',#55707,10.);
#6852=VECTOR('',#55710,10.);
#6853=VECTOR('',#55713,10.);
#6854=VECTOR('',#55714,10.);
#6855=VECTOR('',#55715,10.);
#6856=VECTOR('',#55716,10.);
#6857=VECTOR('',#55717,10.);
#6858=VECTOR('',#55718,10.);
#6859=VECTOR('',#55719,10.);
#6860=VECTOR('',#55720,10.);
#6861=VECTOR('',#55721,10.);
#6862=VECTOR('',#55722,10.);
#6863=VECTOR('',#55723,10.);
#6864=VECTOR('',#55724,10.);
#6865=VECTOR('',#55725,10.);
#6866=VECTOR('',#55726,10.);
#6867=VECTOR('',#55727,10.);
#6868=VECTOR('',#55728,10.);
#6869=VECTOR('',#55729,10.);
#6870=VECTOR('',#55730,10.);
#6871=VECTOR('',#55731,10.);
#6872=VECTOR('',#55732,10.);
#6873=VECTOR('',#55733,10.);
#6874=VECTOR('',#55734,10.);
#6875=VECTOR('',#55735,10.);
#6876=VECTOR('',#55736,10.);
#6877=VECTOR('',#55737,10.);
#6878=VECTOR('',#55738,10.);
#6879=VECTOR('',#55739,10.);
#6880=VECTOR('',#55740,10.);
#6881=VECTOR('',#55741,10.);
#6882=VECTOR('',#55742,10.);
#6883=VECTOR('',#55745,10.);
#6884=VECTOR('',#55746,10.);
#6885=VECTOR('',#55749,10.);
#6886=VECTOR('',#55752,10.);
#6887=VECTOR('',#55753,10.);
#6888=VECTOR('',#55754,10.);
#6889=VECTOR('',#55755,10.);
#6890=VECTOR('',#55756,10.);
#6891=VECTOR('',#55757,10.);
#6892=VECTOR('',#55758,10.);
#6893=VECTOR('',#55759,10.);
#6894=VECTOR('',#55760,10.);
#6895=VECTOR('',#55761,10.);
#6896=VECTOR('',#55762,10.);
#6897=VECTOR('',#55763,10.);
#6898=VECTOR('',#55764,10.);
#6899=VECTOR('',#55765,10.);
#6900=VECTOR('',#55766,10.);
#6901=VECTOR('',#55767,10.);
#6902=VECTOR('',#55768,10.);
#6903=VECTOR('',#55769,10.);
#6904=VECTOR('',#55770,10.);
#6905=VECTOR('',#55771,10.);
#6906=VECTOR('',#55772,10.);
#6907=VECTOR('',#55773,10.);
#6908=VECTOR('',#55774,10.);
#6909=VECTOR('',#55775,10.);
#6910=VECTOR('',#55776,10.);
#6911=VECTOR('',#55777,10.);
#6912=VECTOR('',#55778,10.);
#6913=VECTOR('',#55779,10.);
#6914=VECTOR('',#55780,10.);
#6915=VECTOR('',#55781,10.);
#6916=VECTOR('',#55784,10.);
#6917=VECTOR('',#55785,10.);
#6918=VECTOR('',#55788,10.);
#6919=VECTOR('',#55791,10.);
#6920=VECTOR('',#55792,10.);
#6921=VECTOR('',#55793,10.);
#6922=VECTOR('',#55794,10.);
#6923=VECTOR('',#55795,10.);
#6924=VECTOR('',#55796,10.);
#6925=VECTOR('',#55797,10.);
#6926=VECTOR('',#55798,10.);
#6927=VECTOR('',#55799,10.);
#6928=VECTOR('',#55800,10.);
#6929=VECTOR('',#55801,10.);
#6930=VECTOR('',#55802,10.);
#6931=VECTOR('',#55803,10.);
#6932=VECTOR('',#55804,10.);
#6933=VECTOR('',#55805,10.);
#6934=VECTOR('',#55806,10.);
#6935=VECTOR('',#55807,10.);
#6936=VECTOR('',#55808,10.);
#6937=VECTOR('',#55809,10.);
#6938=VECTOR('',#55810,10.);
#6939=VECTOR('',#55811,10.);
#6940=VECTOR('',#55812,10.);
#6941=VECTOR('',#55813,10.);
#6942=VECTOR('',#55814,10.);
#6943=VECTOR('',#55815,10.);
#6944=VECTOR('',#55816,10.);
#6945=VECTOR('',#55817,10.);
#6946=VECTOR('',#55818,10.);
#6947=VECTOR('',#55819,10.);
#6948=VECTOR('',#55820,10.);
#6949=VECTOR('',#55823,10.);
#6950=VECTOR('',#55824,10.);
#6951=VECTOR('',#55827,10.);
#6952=VECTOR('',#55830,10.);
#6953=VECTOR('',#55831,10.);
#6954=VECTOR('',#55832,10.);
#6955=VECTOR('',#55833,10.);
#6956=VECTOR('',#55834,10.);
#6957=VECTOR('',#55835,10.);
#6958=VECTOR('',#55836,10.);
#6959=VECTOR('',#55837,10.);
#6960=VECTOR('',#55838,10.);
#6961=VECTOR('',#55839,10.);
#6962=VECTOR('',#55840,10.);
#6963=VECTOR('',#55841,10.);
#6964=VECTOR('',#55842,10.);
#6965=VECTOR('',#55843,10.);
#6966=VECTOR('',#55844,10.);
#6967=VECTOR('',#55845,10.);
#6968=VECTOR('',#55846,10.);
#6969=VECTOR('',#55847,10.);
#6970=VECTOR('',#55848,10.);
#6971=VECTOR('',#55849,10.);
#6972=VECTOR('',#55850,10.);
#6973=VECTOR('',#55851,10.);
#6974=VECTOR('',#55852,10.);
#6975=VECTOR('',#55853,10.);
#6976=VECTOR('',#55854,10.);
#6977=VECTOR('',#55855,10.);
#6978=VECTOR('',#55856,10.);
#6979=VECTOR('',#55857,10.);
#6980=VECTOR('',#55858,10.);
#6981=VECTOR('',#55859,10.);
#6982=VECTOR('',#55862,10.);
#6983=VECTOR('',#55863,10.);
#6984=VECTOR('',#55866,10.);
#6985=VECTOR('',#55869,10.);
#6986=VECTOR('',#55870,10.);
#6987=VECTOR('',#55871,10.);
#6988=VECTOR('',#55872,10.);
#6989=VECTOR('',#55873,10.);
#6990=VECTOR('',#55874,10.);
#6991=VECTOR('',#55875,10.);
#6992=VECTOR('',#55876,10.);
#6993=VECTOR('',#55877,10.);
#6994=VECTOR('',#55878,10.);
#6995=VECTOR('',#55879,10.);
#6996=VECTOR('',#55880,10.);
#6997=VECTOR('',#55881,10.);
#6998=VECTOR('',#55882,10.);
#6999=VECTOR('',#55883,10.);
#7000=VECTOR('',#55884,10.);
#7001=VECTOR('',#55885,10.);
#7002=VECTOR('',#55886,10.);
#7003=VECTOR('',#55887,10.);
#7004=VECTOR('',#55888,10.);
#7005=VECTOR('',#55889,10.);
#7006=VECTOR('',#55890,10.);
#7007=VECTOR('',#55891,10.);
#7008=VECTOR('',#55892,10.);
#7009=VECTOR('',#55893,10.);
#7010=VECTOR('',#55894,10.);
#7011=VECTOR('',#55895,10.);
#7012=VECTOR('',#55896,10.);
#7013=VECTOR('',#55897,10.);
#7014=VECTOR('',#55898,10.);
#7015=VECTOR('',#55901,10.);
#7016=VECTOR('',#55902,10.);
#7017=VECTOR('',#55905,10.);
#7018=VECTOR('',#55908,10.);
#7019=VECTOR('',#55909,10.);
#7020=VECTOR('',#55910,10.);
#7021=VECTOR('',#55911,10.);
#7022=VECTOR('',#55912,10.);
#7023=VECTOR('',#55913,10.);
#7024=VECTOR('',#55914,10.);
#7025=VECTOR('',#55915,10.);
#7026=VECTOR('',#55916,10.);
#7027=VECTOR('',#55917,10.);
#7028=VECTOR('',#55918,10.);
#7029=VECTOR('',#55919,10.);
#7030=VECTOR('',#55920,10.);
#7031=VECTOR('',#55921,10.);
#7032=VECTOR('',#55922,10.);
#7033=VECTOR('',#55923,10.);
#7034=VECTOR('',#55924,10.);
#7035=VECTOR('',#55925,10.);
#7036=VECTOR('',#55926,10.);
#7037=VECTOR('',#55927,10.);
#7038=VECTOR('',#55928,10.);
#7039=VECTOR('',#55929,10.);
#7040=VECTOR('',#55930,10.);
#7041=VECTOR('',#55931,10.);
#7042=VECTOR('',#55932,10.);
#7043=VECTOR('',#55933,10.);
#7044=VECTOR('',#55934,10.);
#7045=VECTOR('',#55935,10.);
#7046=VECTOR('',#55936,10.);
#7047=VECTOR('',#55937,10.);
#7048=VECTOR('',#55940,10.);
#7049=VECTOR('',#55941,10.);
#7050=VECTOR('',#55944,10.);
#7051=VECTOR('',#55947,10.);
#7052=VECTOR('',#55948,10.);
#7053=VECTOR('',#55949,10.);
#7054=VECTOR('',#55950,10.);
#7055=VECTOR('',#55951,10.);
#7056=VECTOR('',#55952,10.);
#7057=VECTOR('',#55953,10.);
#7058=VECTOR('',#55954,10.);
#7059=VECTOR('',#55955,10.);
#7060=VECTOR('',#55956,10.);
#7061=VECTOR('',#55957,10.);
#7062=VECTOR('',#55958,10.);
#7063=VECTOR('',#55959,10.);
#7064=VECTOR('',#55960,10.);
#7065=VECTOR('',#55961,10.);
#7066=VECTOR('',#55962,10.);
#7067=VECTOR('',#55963,10.);
#7068=VECTOR('',#55964,10.);
#7069=VECTOR('',#55965,10.);
#7070=VECTOR('',#55966,10.);
#7071=VECTOR('',#55967,10.);
#7072=VECTOR('',#55968,10.);
#7073=VECTOR('',#55969,10.);
#7074=VECTOR('',#55970,10.);
#7075=VECTOR('',#55971,10.);
#7076=VECTOR('',#55972,10.);
#7077=VECTOR('',#55973,10.);
#7078=VECTOR('',#55974,10.);
#7079=VECTOR('',#55975,10.);
#7080=VECTOR('',#55976,10.);
#7081=VECTOR('',#55979,10.);
#7082=VECTOR('',#55980,10.);
#7083=VECTOR('',#55983,10.);
#7084=VECTOR('',#55986,10.);
#7085=VECTOR('',#55987,10.);
#7086=VECTOR('',#55988,10.);
#7087=VECTOR('',#55989,10.);
#7088=VECTOR('',#55990,10.);
#7089=VECTOR('',#55991,10.);
#7090=VECTOR('',#55992,10.);
#7091=VECTOR('',#55993,10.);
#7092=VECTOR('',#55994,10.);
#7093=VECTOR('',#55995,10.);
#7094=VECTOR('',#55996,10.);
#7095=VECTOR('',#55997,10.);
#7096=VECTOR('',#55998,10.);
#7097=VECTOR('',#55999,10.);
#7098=VECTOR('',#56000,10.);
#7099=VECTOR('',#56001,10.);
#7100=VECTOR('',#56002,10.);
#7101=VECTOR('',#56003,10.);
#7102=VECTOR('',#56004,10.);
#7103=VECTOR('',#56005,10.);
#7104=VECTOR('',#56006,10.);
#7105=VECTOR('',#56007,10.);
#7106=VECTOR('',#56008,10.);
#7107=VECTOR('',#56009,10.);
#7108=VECTOR('',#56010,10.);
#7109=VECTOR('',#56011,10.);
#7110=VECTOR('',#56012,10.);
#7111=VECTOR('',#56013,10.);
#7112=VECTOR('',#56014,10.);
#7113=VECTOR('',#56015,10.);
#7114=VECTOR('',#56018,10.);
#7115=VECTOR('',#56019,10.);
#7116=VECTOR('',#56022,10.);
#7117=VECTOR('',#56025,10.);
#7118=VECTOR('',#56026,10.);
#7119=VECTOR('',#56027,10.);
#7120=VECTOR('',#56028,10.);
#7121=VECTOR('',#56029,10.);
#7122=VECTOR('',#56030,10.);
#7123=VECTOR('',#56031,10.);
#7124=VECTOR('',#56032,10.);
#7125=VECTOR('',#56033,10.);
#7126=VECTOR('',#56034,10.);
#7127=VECTOR('',#56035,10.);
#7128=VECTOR('',#56036,10.);
#7129=VECTOR('',#56037,10.);
#7130=VECTOR('',#56038,10.);
#7131=VECTOR('',#56039,10.);
#7132=VECTOR('',#56040,10.);
#7133=VECTOR('',#56041,10.);
#7134=VECTOR('',#56042,10.);
#7135=VECTOR('',#56043,10.);
#7136=VECTOR('',#56044,10.);
#7137=VECTOR('',#56045,10.);
#7138=VECTOR('',#56046,10.);
#7139=VECTOR('',#56047,10.);
#7140=VECTOR('',#56048,10.);
#7141=VECTOR('',#56049,10.);
#7142=VECTOR('',#56050,10.);
#7143=VECTOR('',#56051,10.);
#7144=VECTOR('',#56052,10.);
#7145=VECTOR('',#56053,10.);
#7146=VECTOR('',#56054,10.);
#7147=VECTOR('',#56057,10.);
#7148=VECTOR('',#56058,10.);
#7149=VECTOR('',#56061,10.);
#7150=VECTOR('',#56064,10.);
#7151=VECTOR('',#56065,10.);
#7152=VECTOR('',#56066,10.);
#7153=VECTOR('',#56067,10.);
#7154=VECTOR('',#56068,10.);
#7155=VECTOR('',#56069,10.);
#7156=VECTOR('',#56070,10.);
#7157=VECTOR('',#56071,10.);
#7158=VECTOR('',#56072,10.);
#7159=VECTOR('',#56073,10.);
#7160=VECTOR('',#56074,10.);
#7161=VECTOR('',#56075,10.);
#7162=VECTOR('',#56076,10.);
#7163=VECTOR('',#56077,10.);
#7164=VECTOR('',#56078,10.);
#7165=VECTOR('',#56079,10.);
#7166=VECTOR('',#56080,10.);
#7167=VECTOR('',#56081,10.);
#7168=VECTOR('',#56082,10.);
#7169=VECTOR('',#56083,10.);
#7170=VECTOR('',#56084,10.);
#7171=VECTOR('',#56085,10.);
#7172=VECTOR('',#56086,10.);
#7173=VECTOR('',#56087,10.);
#7174=VECTOR('',#56088,10.);
#7175=VECTOR('',#56089,10.);
#7176=VECTOR('',#56090,10.);
#7177=VECTOR('',#56091,10.);
#7178=VECTOR('',#56092,10.);
#7179=VECTOR('',#56093,10.);
#7180=VECTOR('',#56096,10.);
#7181=VECTOR('',#56097,10.);
#7182=VECTOR('',#56100,10.);
#7183=VECTOR('',#56103,10.);
#7184=VECTOR('',#56104,10.);
#7185=VECTOR('',#56105,10.);
#7186=VECTOR('',#56106,10.);
#7187=VECTOR('',#56107,10.);
#7188=VECTOR('',#56108,10.);
#7189=VECTOR('',#56109,10.);
#7190=VECTOR('',#56110,10.);
#7191=VECTOR('',#56111,10.);
#7192=VECTOR('',#56112,10.);
#7193=VECTOR('',#56113,10.);
#7194=VECTOR('',#56114,10.);
#7195=VECTOR('',#56115,10.);
#7196=VECTOR('',#56116,10.);
#7197=VECTOR('',#56117,10.);
#7198=VECTOR('',#56118,10.);
#7199=VECTOR('',#56119,10.);
#7200=VECTOR('',#56120,10.);
#7201=VECTOR('',#56121,10.);
#7202=VECTOR('',#56122,10.);
#7203=VECTOR('',#56123,10.);
#7204=VECTOR('',#56124,10.);
#7205=VECTOR('',#56125,10.);
#7206=VECTOR('',#56126,10.);
#7207=VECTOR('',#56127,10.);
#7208=VECTOR('',#56128,10.);
#7209=VECTOR('',#56129,10.);
#7210=VECTOR('',#56130,10.);
#7211=VECTOR('',#56131,10.);
#7212=VECTOR('',#56132,10.);
#7213=VECTOR('',#56135,10.);
#7214=VECTOR('',#56136,10.);
#7215=VECTOR('',#56139,10.);
#7216=VECTOR('',#56142,10.);
#7217=VECTOR('',#56143,10.);
#7218=VECTOR('',#56144,10.);
#7219=VECTOR('',#56145,10.);
#7220=VECTOR('',#56146,10.);
#7221=VECTOR('',#56147,10.);
#7222=VECTOR('',#56148,10.);
#7223=VECTOR('',#56149,10.);
#7224=VECTOR('',#56150,10.);
#7225=VECTOR('',#56151,10.);
#7226=VECTOR('',#56152,10.);
#7227=VECTOR('',#56153,10.);
#7228=VECTOR('',#56154,10.);
#7229=VECTOR('',#56155,10.);
#7230=VECTOR('',#56156,10.);
#7231=VECTOR('',#56157,10.);
#7232=VECTOR('',#56158,10.);
#7233=VECTOR('',#56159,10.);
#7234=VECTOR('',#56160,10.);
#7235=VECTOR('',#56161,10.);
#7236=VECTOR('',#56162,10.);
#7237=VECTOR('',#56163,10.);
#7238=VECTOR('',#56164,10.);
#7239=VECTOR('',#56165,10.);
#7240=VECTOR('',#56166,10.);
#7241=VECTOR('',#56167,10.);
#7242=VECTOR('',#56168,10.);
#7243=VECTOR('',#56169,10.);
#7244=VECTOR('',#56170,10.);
#7245=VECTOR('',#56171,10.);
#7246=VECTOR('',#56174,10.);
#7247=VECTOR('',#56175,10.);
#7248=VECTOR('',#56178,10.);
#7249=VECTOR('',#56181,10.);
#7250=VECTOR('',#56182,10.);
#7251=VECTOR('',#56183,10.);
#7252=VECTOR('',#56184,10.);
#7253=VECTOR('',#56185,10.);
#7254=VECTOR('',#56186,10.);
#7255=VECTOR('',#56187,10.);
#7256=VECTOR('',#56188,10.);
#7257=VECTOR('',#56189,10.);
#7258=VECTOR('',#56190,10.);
#7259=VECTOR('',#56191,10.);
#7260=VECTOR('',#56192,10.);
#7261=VECTOR('',#56193,10.);
#7262=VECTOR('',#56194,10.);
#7263=VECTOR('',#56195,10.);
#7264=VECTOR('',#56196,10.);
#7265=VECTOR('',#56197,10.);
#7266=VECTOR('',#56198,10.);
#7267=VECTOR('',#56199,10.);
#7268=VECTOR('',#56200,10.);
#7269=VECTOR('',#56201,10.);
#7270=VECTOR('',#56202,10.);
#7271=VECTOR('',#56203,10.);
#7272=VECTOR('',#56204,10.);
#7273=VECTOR('',#56205,10.);
#7274=VECTOR('',#56206,10.);
#7275=VECTOR('',#56207,10.);
#7276=VECTOR('',#56208,10.);
#7277=VECTOR('',#56209,10.);
#7278=VECTOR('',#56210,10.);
#7279=VECTOR('',#56213,10.);
#7280=VECTOR('',#56214,10.);
#7281=VECTOR('',#56217,10.);
#7282=VECTOR('',#56220,10.);
#7283=VECTOR('',#56221,10.);
#7284=VECTOR('',#56222,10.);
#7285=VECTOR('',#56223,10.);
#7286=VECTOR('',#56224,10.);
#7287=VECTOR('',#56225,10.);
#7288=VECTOR('',#56226,10.);
#7289=VECTOR('',#56227,10.);
#7290=VECTOR('',#56228,10.);
#7291=VECTOR('',#56229,10.);
#7292=VECTOR('',#56230,10.);
#7293=VECTOR('',#56231,10.);
#7294=VECTOR('',#56232,10.);
#7295=VECTOR('',#56233,10.);
#7296=VECTOR('',#56234,10.);
#7297=VECTOR('',#56235,10.);
#7298=VECTOR('',#56236,10.);
#7299=VECTOR('',#56237,10.);
#7300=VECTOR('',#56238,10.);
#7301=VECTOR('',#56239,10.);
#7302=VECTOR('',#56240,10.);
#7303=VECTOR('',#56241,10.);
#7304=VECTOR('',#56242,10.);
#7305=VECTOR('',#56243,10.);
#7306=VECTOR('',#56244,10.);
#7307=VECTOR('',#56245,10.);
#7308=VECTOR('',#56246,10.);
#7309=VECTOR('',#56247,10.);
#7310=VECTOR('',#56248,10.);
#7311=VECTOR('',#56249,10.);
#7312=VECTOR('',#56252,10.);
#7313=VECTOR('',#56253,10.);
#7314=VECTOR('',#56256,10.);
#7315=VECTOR('',#56259,10.);
#7316=VECTOR('',#56260,10.);
#7317=VECTOR('',#56261,10.);
#7318=VECTOR('',#56262,10.);
#7319=VECTOR('',#56263,10.);
#7320=VECTOR('',#56264,10.);
#7321=VECTOR('',#56265,10.);
#7322=VECTOR('',#56266,10.);
#7323=VECTOR('',#56267,10.);
#7324=VECTOR('',#56268,10.);
#7325=VECTOR('',#56269,10.);
#7326=VECTOR('',#56270,10.);
#7327=VECTOR('',#56271,10.);
#7328=VECTOR('',#56272,10.);
#7329=VECTOR('',#56273,10.);
#7330=VECTOR('',#56274,10.);
#7331=VECTOR('',#56275,10.);
#7332=VECTOR('',#56276,10.);
#7333=VECTOR('',#56277,10.);
#7334=VECTOR('',#56278,10.);
#7335=VECTOR('',#56279,10.);
#7336=VECTOR('',#56280,10.);
#7337=VECTOR('',#56281,10.);
#7338=VECTOR('',#56282,10.);
#7339=VECTOR('',#56283,10.);
#7340=VECTOR('',#56284,10.);
#7341=VECTOR('',#56285,10.);
#7342=VECTOR('',#56286,10.);
#7343=VECTOR('',#56287,10.);
#7344=VECTOR('',#56288,10.);
#7345=VECTOR('',#56291,10.);
#7346=VECTOR('',#56292,10.);
#7347=VECTOR('',#56295,10.);
#7348=VECTOR('',#56298,10.);
#7349=VECTOR('',#56299,10.);
#7350=VECTOR('',#56300,10.);
#7351=VECTOR('',#56301,10.);
#7352=VECTOR('',#56302,10.);
#7353=VECTOR('',#56303,10.);
#7354=VECTOR('',#56304,10.);
#7355=VECTOR('',#56305,10.);
#7356=VECTOR('',#56306,10.);
#7357=VECTOR('',#56307,10.);
#7358=VECTOR('',#56308,10.);
#7359=VECTOR('',#56309,10.);
#7360=VECTOR('',#56310,10.);
#7361=VECTOR('',#56311,10.);
#7362=VECTOR('',#56312,10.);
#7363=VECTOR('',#56313,10.);
#7364=VECTOR('',#56314,10.);
#7365=VECTOR('',#56315,10.);
#7366=VECTOR('',#56316,10.);
#7367=VECTOR('',#56317,10.);
#7368=VECTOR('',#56318,10.);
#7369=VECTOR('',#56319,10.);
#7370=VECTOR('',#56320,10.);
#7371=VECTOR('',#56321,10.);
#7372=VECTOR('',#56322,10.);
#7373=VECTOR('',#56323,10.);
#7374=VECTOR('',#56324,10.);
#7375=VECTOR('',#56325,10.);
#7376=VECTOR('',#56326,10.);
#7377=VECTOR('',#56327,10.);
#7378=VECTOR('',#56330,10.);
#7379=VECTOR('',#56331,10.);
#7380=VECTOR('',#56334,10.);
#7381=VECTOR('',#56337,10.);
#7382=VECTOR('',#56338,10.);
#7383=VECTOR('',#56339,10.);
#7384=VECTOR('',#56340,10.);
#7385=VECTOR('',#56341,10.);
#7386=VECTOR('',#56342,10.);
#7387=VECTOR('',#56343,10.);
#7388=VECTOR('',#56344,10.);
#7389=VECTOR('',#56345,10.);
#7390=VECTOR('',#56346,10.);
#7391=VECTOR('',#56347,10.);
#7392=VECTOR('',#56348,10.);
#7393=VECTOR('',#56349,10.);
#7394=VECTOR('',#56350,10.);
#7395=VECTOR('',#56351,10.);
#7396=VECTOR('',#56352,10.);
#7397=VECTOR('',#56353,10.);
#7398=VECTOR('',#56354,10.);
#7399=VECTOR('',#56355,10.);
#7400=VECTOR('',#56356,10.);
#7401=VECTOR('',#56357,10.);
#7402=VECTOR('',#56358,10.);
#7403=VECTOR('',#56359,10.);
#7404=VECTOR('',#56360,10.);
#7405=VECTOR('',#56361,10.);
#7406=VECTOR('',#56362,10.);
#7407=VECTOR('',#56363,10.);
#7408=VECTOR('',#56364,10.);
#7409=VECTOR('',#56365,10.);
#7410=VECTOR('',#56366,10.);
#7411=VECTOR('',#56369,10.);
#7412=VECTOR('',#56370,10.);
#7413=VECTOR('',#56373,10.);
#7414=VECTOR('',#56376,10.);
#7415=VECTOR('',#56377,10.);
#7416=VECTOR('',#56378,10.);
#7417=VECTOR('',#56379,10.);
#7418=VECTOR('',#56380,10.);
#7419=VECTOR('',#56381,10.);
#7420=VECTOR('',#56382,10.);
#7421=VECTOR('',#56383,10.);
#7422=VECTOR('',#56384,10.);
#7423=VECTOR('',#56385,10.);
#7424=VECTOR('',#56386,10.);
#7425=VECTOR('',#56387,10.);
#7426=VECTOR('',#56388,10.);
#7427=VECTOR('',#56389,10.);
#7428=VECTOR('',#56390,10.);
#7429=VECTOR('',#56391,10.);
#7430=VECTOR('',#56392,10.);
#7431=VECTOR('',#56393,10.);
#7432=VECTOR('',#56394,10.);
#7433=VECTOR('',#56395,10.);
#7434=VECTOR('',#56396,10.);
#7435=VECTOR('',#56397,10.);
#7436=VECTOR('',#56398,10.);
#7437=VECTOR('',#56399,10.);
#7438=VECTOR('',#56400,10.);
#7439=VECTOR('',#56401,10.);
#7440=VECTOR('',#56402,10.);
#7441=VECTOR('',#56403,10.);
#7442=VECTOR('',#56404,10.);
#7443=VECTOR('',#56405,10.);
#7444=VECTOR('',#56408,10.);
#7445=VECTOR('',#56409,10.);
#7446=VECTOR('',#56412,10.);
#7447=VECTOR('',#56415,10.);
#7448=VECTOR('',#56416,10.);
#7449=VECTOR('',#56417,10.);
#7450=VECTOR('',#56418,10.);
#7451=VECTOR('',#56419,10.);
#7452=VECTOR('',#56420,10.);
#7453=VECTOR('',#56421,10.);
#7454=VECTOR('',#56422,10.);
#7455=VECTOR('',#56423,10.);
#7456=VECTOR('',#56424,10.);
#7457=VECTOR('',#56425,10.);
#7458=VECTOR('',#56426,10.);
#7459=VECTOR('',#56427,10.);
#7460=VECTOR('',#56428,10.);
#7461=VECTOR('',#56429,10.);
#7462=VECTOR('',#56430,10.);
#7463=VECTOR('',#56431,10.);
#7464=VECTOR('',#56432,10.);
#7465=VECTOR('',#56433,10.);
#7466=VECTOR('',#56434,10.);
#7467=VECTOR('',#56435,10.);
#7468=VECTOR('',#56436,10.);
#7469=VECTOR('',#56437,10.);
#7470=VECTOR('',#56438,10.);
#7471=VECTOR('',#56439,10.);
#7472=VECTOR('',#56440,10.);
#7473=VECTOR('',#56441,10.);
#7474=VECTOR('',#56442,10.);
#7475=VECTOR('',#56443,10.);
#7476=VECTOR('',#56444,10.);
#7477=VECTOR('',#56447,10.);
#7478=VECTOR('',#56448,10.);
#7479=VECTOR('',#56451,10.);
#7480=VECTOR('',#56454,10.);
#7481=VECTOR('',#56455,10.);
#7482=VECTOR('',#56456,10.);
#7483=VECTOR('',#56457,10.);
#7484=VECTOR('',#56458,10.);
#7485=VECTOR('',#56459,10.);
#7486=VECTOR('',#56460,10.);
#7487=VECTOR('',#56461,10.);
#7488=VECTOR('',#56462,10.);
#7489=VECTOR('',#56463,10.);
#7490=VECTOR('',#56464,10.);
#7491=VECTOR('',#56465,10.);
#7492=VECTOR('',#56466,10.);
#7493=VECTOR('',#56467,10.);
#7494=VECTOR('',#56468,10.);
#7495=VECTOR('',#56469,10.);
#7496=VECTOR('',#56470,10.);
#7497=VECTOR('',#56471,10.);
#7498=VECTOR('',#56472,10.);
#7499=VECTOR('',#56473,10.);
#7500=VECTOR('',#56474,10.);
#7501=VECTOR('',#56475,10.);
#7502=VECTOR('',#56476,10.);
#7503=VECTOR('',#56477,10.);
#7504=VECTOR('',#56478,10.);
#7505=VECTOR('',#56479,10.);
#7506=VECTOR('',#56480,10.);
#7507=VECTOR('',#56481,10.);
#7508=VECTOR('',#56482,10.);
#7509=VECTOR('',#56483,10.);
#7510=VECTOR('',#56486,10.);
#7511=VECTOR('',#56487,10.);
#7512=VECTOR('',#56490,10.);
#7513=VECTOR('',#56493,10.);
#7514=VECTOR('',#56494,10.);
#7515=VECTOR('',#56495,10.);
#7516=VECTOR('',#56496,10.);
#7517=VECTOR('',#56497,10.);
#7518=VECTOR('',#56498,10.);
#7519=VECTOR('',#56499,10.);
#7520=VECTOR('',#56500,10.);
#7521=VECTOR('',#56501,10.);
#7522=VECTOR('',#56502,10.);
#7523=VECTOR('',#56503,10.);
#7524=VECTOR('',#56504,10.);
#7525=VECTOR('',#56505,10.);
#7526=VECTOR('',#56506,10.);
#7527=VECTOR('',#56507,10.);
#7528=VECTOR('',#56508,10.);
#7529=VECTOR('',#56509,10.);
#7530=VECTOR('',#56510,10.);
#7531=VECTOR('',#56511,10.);
#7532=VECTOR('',#56512,10.);
#7533=VECTOR('',#56513,10.);
#7534=VECTOR('',#56514,10.);
#7535=VECTOR('',#56515,10.);
#7536=VECTOR('',#56516,10.);
#7537=VECTOR('',#56517,10.);
#7538=VECTOR('',#56518,10.);
#7539=VECTOR('',#56519,10.);
#7540=VECTOR('',#56520,10.);
#7541=VECTOR('',#56521,10.);
#7542=VECTOR('',#56522,10.);
#7543=VECTOR('',#56525,10.);
#7544=VECTOR('',#56526,10.);
#7545=VECTOR('',#56529,10.);
#7546=VECTOR('',#56532,10.);
#7547=VECTOR('',#56533,10.);
#7548=VECTOR('',#56534,10.);
#7549=VECTOR('',#56535,10.);
#7550=VECTOR('',#56536,10.);
#7551=VECTOR('',#56537,10.);
#7552=VECTOR('',#56538,10.);
#7553=VECTOR('',#56539,10.);
#7554=VECTOR('',#56540,10.);
#7555=VECTOR('',#56541,10.);
#7556=VECTOR('',#56542,10.);
#7557=VECTOR('',#56543,10.);
#7558=VECTOR('',#56544,10.);
#7559=VECTOR('',#56545,10.);
#7560=VECTOR('',#56546,10.);
#7561=VECTOR('',#56547,10.);
#7562=VECTOR('',#56548,10.);
#7563=VECTOR('',#56549,10.);
#7564=VECTOR('',#56550,10.);
#7565=VECTOR('',#56551,10.);
#7566=VECTOR('',#56552,10.);
#7567=VECTOR('',#56553,10.);
#7568=VECTOR('',#56554,10.);
#7569=VECTOR('',#56555,10.);
#7570=VECTOR('',#56556,10.);
#7571=VECTOR('',#56557,10.);
#7572=VECTOR('',#56558,10.);
#7573=VECTOR('',#56559,10.);
#7574=VECTOR('',#56560,10.);
#7575=VECTOR('',#56561,10.);
#7576=VECTOR('',#56564,10.);
#7577=VECTOR('',#56565,10.);
#7578=VECTOR('',#56568,10.);
#7579=VECTOR('',#56571,10.);
#7580=VECTOR('',#56572,10.);
#7581=VECTOR('',#56573,10.);
#7582=VECTOR('',#56574,10.);
#7583=VECTOR('',#56575,10.);
#7584=VECTOR('',#56576,10.);
#7585=VECTOR('',#56577,10.);
#7586=VECTOR('',#56578,10.);
#7587=VECTOR('',#56579,10.);
#7588=VECTOR('',#56580,10.);
#7589=VECTOR('',#56581,10.);
#7590=VECTOR('',#56582,10.);
#7591=VECTOR('',#56583,10.);
#7592=VECTOR('',#56584,10.);
#7593=VECTOR('',#56585,10.);
#7594=VECTOR('',#56586,10.);
#7595=VECTOR('',#56587,10.);
#7596=VECTOR('',#56588,10.);
#7597=VECTOR('',#56589,10.);
#7598=VECTOR('',#56590,10.);
#7599=VECTOR('',#56591,10.);
#7600=VECTOR('',#56592,10.);
#7601=VECTOR('',#56593,10.);
#7602=VECTOR('',#56594,10.);
#7603=VECTOR('',#56595,10.);
#7604=VECTOR('',#56596,10.);
#7605=VECTOR('',#56597,10.);
#7606=VECTOR('',#56598,10.);
#7607=VECTOR('',#56599,10.);
#7608=VECTOR('',#56600,10.);
#7609=VECTOR('',#56603,10.);
#7610=VECTOR('',#56604,10.);
#7611=VECTOR('',#56607,10.);
#7612=VECTOR('',#56610,10.);
#7613=VECTOR('',#56611,10.);
#7614=VECTOR('',#56612,10.);
#7615=VECTOR('',#56613,10.);
#7616=VECTOR('',#56614,10.);
#7617=VECTOR('',#56615,10.);
#7618=VECTOR('',#56616,10.);
#7619=VECTOR('',#56617,10.);
#7620=VECTOR('',#56618,10.);
#7621=VECTOR('',#56619,10.);
#7622=VECTOR('',#56620,10.);
#7623=VECTOR('',#56621,10.);
#7624=VECTOR('',#56622,10.);
#7625=VECTOR('',#56623,10.);
#7626=VECTOR('',#56624,10.);
#7627=VECTOR('',#56625,10.);
#7628=VECTOR('',#56626,10.);
#7629=VECTOR('',#56627,10.);
#7630=VECTOR('',#56628,10.);
#7631=VECTOR('',#56629,10.);
#7632=VECTOR('',#56630,10.);
#7633=VECTOR('',#56631,10.);
#7634=VECTOR('',#56632,10.);
#7635=VECTOR('',#56633,10.);
#7636=VECTOR('',#56634,10.);
#7637=VECTOR('',#56635,10.);
#7638=VECTOR('',#56636,10.);
#7639=VECTOR('',#56637,10.);
#7640=VECTOR('',#56638,10.);
#7641=VECTOR('',#56639,10.);
#7642=VECTOR('',#56642,10.);
#7643=VECTOR('',#56643,10.);
#7644=VECTOR('',#56646,10.);
#7645=VECTOR('',#56649,10.);
#7646=VECTOR('',#56650,10.);
#7647=VECTOR('',#56651,10.);
#7648=VECTOR('',#56652,10.);
#7649=VECTOR('',#56653,10.);
#7650=VECTOR('',#56654,10.);
#7651=VECTOR('',#56655,10.);
#7652=VECTOR('',#56656,10.);
#7653=VECTOR('',#56657,10.);
#7654=VECTOR('',#56658,10.);
#7655=VECTOR('',#56659,10.);
#7656=VECTOR('',#56660,10.);
#7657=VECTOR('',#56661,10.);
#7658=VECTOR('',#56662,10.);
#7659=VECTOR('',#56663,10.);
#7660=VECTOR('',#56664,10.);
#7661=VECTOR('',#56665,10.);
#7662=VECTOR('',#56666,10.);
#7663=VECTOR('',#56667,10.);
#7664=VECTOR('',#56668,10.);
#7665=VECTOR('',#56669,10.);
#7666=VECTOR('',#56670,10.);
#7667=VECTOR('',#56671,10.);
#7668=VECTOR('',#56672,10.);
#7669=VECTOR('',#56673,10.);
#7670=VECTOR('',#56674,10.);
#7671=VECTOR('',#56675,10.);
#7672=VECTOR('',#56676,10.);
#7673=VECTOR('',#56677,10.);
#7674=VECTOR('',#56678,10.);
#7675=VECTOR('',#56681,10.);
#7676=VECTOR('',#56682,10.);
#7677=VECTOR('',#56685,10.);
#7678=VECTOR('',#56688,10.);
#7679=VECTOR('',#56689,10.);
#7680=VECTOR('',#56690,10.);
#7681=VECTOR('',#56691,10.);
#7682=VECTOR('',#56692,10.);
#7683=VECTOR('',#56693,10.);
#7684=VECTOR('',#56694,10.);
#7685=VECTOR('',#56695,10.);
#7686=VECTOR('',#56696,10.);
#7687=VECTOR('',#56697,10.);
#7688=VECTOR('',#56698,10.);
#7689=VECTOR('',#56699,10.);
#7690=VECTOR('',#56700,10.);
#7691=VECTOR('',#56701,10.);
#7692=VECTOR('',#56702,10.);
#7693=VECTOR('',#56703,10.);
#7694=VECTOR('',#56704,10.);
#7695=VECTOR('',#56705,10.);
#7696=VECTOR('',#56706,10.);
#7697=VECTOR('',#56707,10.);
#7698=VECTOR('',#56708,10.);
#7699=VECTOR('',#56709,10.);
#7700=VECTOR('',#56710,10.);
#7701=VECTOR('',#56711,10.);
#7702=VECTOR('',#56712,10.);
#7703=VECTOR('',#56713,10.);
#7704=VECTOR('',#56714,10.);
#7705=VECTOR('',#56715,10.);
#7706=VECTOR('',#56716,10.);
#7707=VECTOR('',#56717,10.);
#7708=VECTOR('',#56720,10.);
#7709=VECTOR('',#56721,10.);
#7710=VECTOR('',#56724,10.);
#7711=VECTOR('',#56727,10.);
#7712=VECTOR('',#56728,10.);
#7713=VECTOR('',#56729,10.);
#7714=VECTOR('',#56730,10.);
#7715=VECTOR('',#56731,10.);
#7716=VECTOR('',#56732,10.);
#7717=VECTOR('',#56733,10.);
#7718=VECTOR('',#56734,10.);
#7719=VECTOR('',#56735,10.);
#7720=VECTOR('',#56736,10.);
#7721=VECTOR('',#56737,10.);
#7722=VECTOR('',#56738,10.);
#7723=VECTOR('',#56739,10.);
#7724=VECTOR('',#56740,10.);
#7725=VECTOR('',#56741,10.);
#7726=VECTOR('',#56742,10.);
#7727=VECTOR('',#56743,10.);
#7728=VECTOR('',#56744,10.);
#7729=VECTOR('',#56745,10.);
#7730=VECTOR('',#56746,10.);
#7731=VECTOR('',#56747,10.);
#7732=VECTOR('',#56748,10.);
#7733=VECTOR('',#56749,10.);
#7734=VECTOR('',#56750,10.);
#7735=VECTOR('',#56751,10.);
#7736=VECTOR('',#56752,10.);
#7737=VECTOR('',#56753,10.);
#7738=VECTOR('',#56754,10.);
#7739=VECTOR('',#56755,10.);
#7740=VECTOR('',#56756,10.);
#7741=VECTOR('',#56759,10.);
#7742=VECTOR('',#56760,10.);
#7743=VECTOR('',#56763,10.);
#7744=VECTOR('',#56766,10.);
#7745=VECTOR('',#56767,10.);
#7746=VECTOR('',#56768,10.);
#7747=VECTOR('',#56769,10.);
#7748=VECTOR('',#56770,10.);
#7749=VECTOR('',#56771,10.);
#7750=VECTOR('',#56772,10.);
#7751=VECTOR('',#56773,10.);
#7752=VECTOR('',#56774,10.);
#7753=VECTOR('',#56775,10.);
#7754=VECTOR('',#56776,10.);
#7755=VECTOR('',#56777,10.);
#7756=VECTOR('',#56778,10.);
#7757=VECTOR('',#56779,10.);
#7758=VECTOR('',#56780,10.);
#7759=VECTOR('',#56781,10.);
#7760=VECTOR('',#56782,10.);
#7761=VECTOR('',#56783,10.);
#7762=VECTOR('',#56784,10.);
#7763=VECTOR('',#56785,10.);
#7764=VECTOR('',#56786,10.);
#7765=VECTOR('',#56787,10.);
#7766=VECTOR('',#56788,10.);
#7767=VECTOR('',#56789,10.);
#7768=VECTOR('',#56790,10.);
#7769=VECTOR('',#56791,10.);
#7770=VECTOR('',#56792,10.);
#7771=VECTOR('',#56793,10.);
#7772=VECTOR('',#56794,10.);
#7773=VECTOR('',#56795,10.);
#7774=VECTOR('',#56798,10.);
#7775=VECTOR('',#56799,10.);
#7776=VECTOR('',#56802,10.);
#7777=VECTOR('',#56805,10.);
#7778=VECTOR('',#56806,10.);
#7779=VECTOR('',#56807,10.);
#7780=VECTOR('',#56808,10.);
#7781=VECTOR('',#56809,10.);
#7782=VECTOR('',#56810,10.);
#7783=VECTOR('',#56811,10.);
#7784=VECTOR('',#56812,10.);
#7785=VECTOR('',#56813,10.);
#7786=VECTOR('',#56814,10.);
#7787=VECTOR('',#56815,10.);
#7788=VECTOR('',#56816,10.);
#7789=VECTOR('',#56817,10.);
#7790=VECTOR('',#56818,10.);
#7791=VECTOR('',#56819,10.);
#7792=VECTOR('',#56820,10.);
#7793=VECTOR('',#56821,10.);
#7794=VECTOR('',#56822,10.);
#7795=VECTOR('',#56823,10.);
#7796=VECTOR('',#56824,10.);
#7797=VECTOR('',#56825,10.);
#7798=VECTOR('',#56826,10.);
#7799=VECTOR('',#56827,10.);
#7800=VECTOR('',#56828,10.);
#7801=VECTOR('',#56829,10.);
#7802=VECTOR('',#56830,10.);
#7803=VECTOR('',#56831,10.);
#7804=VECTOR('',#56832,10.);
#7805=VECTOR('',#56833,10.);
#7806=VECTOR('',#56834,10.);
#7807=VECTOR('',#56837,10.);
#7808=VECTOR('',#56838,10.);
#7809=VECTOR('',#56841,10.);
#7810=VECTOR('',#56844,10.);
#7811=VECTOR('',#56845,10.);
#7812=VECTOR('',#56846,10.);
#7813=VECTOR('',#56847,10.);
#7814=VECTOR('',#56848,10.);
#7815=VECTOR('',#56849,10.);
#7816=VECTOR('',#56850,10.);
#7817=VECTOR('',#56851,10.);
#7818=VECTOR('',#56852,10.);
#7819=VECTOR('',#56853,10.);
#7820=VECTOR('',#56854,10.);
#7821=VECTOR('',#56855,10.);
#7822=VECTOR('',#56856,10.);
#7823=VECTOR('',#56857,10.);
#7824=VECTOR('',#56858,10.);
#7825=VECTOR('',#56859,10.);
#7826=VECTOR('',#56860,10.);
#7827=VECTOR('',#56861,10.);
#7828=VECTOR('',#56862,10.);
#7829=VECTOR('',#56863,10.);
#7830=VECTOR('',#56864,10.);
#7831=VECTOR('',#56865,10.);
#7832=VECTOR('',#56866,10.);
#7833=VECTOR('',#56867,10.);
#7834=VECTOR('',#56868,10.);
#7835=VECTOR('',#56869,10.);
#7836=VECTOR('',#56870,10.);
#7837=VECTOR('',#56871,10.);
#7838=VECTOR('',#56872,10.);
#7839=VECTOR('',#56873,10.);
#7840=VECTOR('',#56876,10.);
#7841=VECTOR('',#56877,10.);
#7842=VECTOR('',#56880,10.);
#7843=VECTOR('',#56883,10.);
#7844=VECTOR('',#56884,10.);
#7845=VECTOR('',#56885,10.);
#7846=VECTOR('',#56886,10.);
#7847=VECTOR('',#56887,10.);
#7848=VECTOR('',#56888,10.);
#7849=VECTOR('',#56889,10.);
#7850=VECTOR('',#56890,10.);
#7851=VECTOR('',#56891,10.);
#7852=VECTOR('',#56892,10.);
#7853=VECTOR('',#56893,10.);
#7854=VECTOR('',#56894,10.);
#7855=VECTOR('',#56895,10.);
#7856=VECTOR('',#56896,10.);
#7857=VECTOR('',#56897,10.);
#7858=VECTOR('',#56898,10.);
#7859=VECTOR('',#56899,10.);
#7860=VECTOR('',#56900,10.);
#7861=VECTOR('',#56901,10.);
#7862=VECTOR('',#56902,10.);
#7863=VECTOR('',#56903,10.);
#7864=VECTOR('',#56904,10.);
#7865=VECTOR('',#56905,10.);
#7866=VECTOR('',#56906,10.);
#7867=VECTOR('',#56907,10.);
#7868=VECTOR('',#56908,10.);
#7869=VECTOR('',#56909,10.);
#7870=VECTOR('',#56910,10.);
#7871=VECTOR('',#56911,10.);
#7872=VECTOR('',#56912,10.);
#7873=VECTOR('',#56915,10.);
#7874=VECTOR('',#56916,10.);
#7875=VECTOR('',#56919,10.);
#7876=VECTOR('',#57066,10.);
#7877=VECTOR('',#57067,10.);
#7878=VECTOR('',#57070,10.);
#7879=VECTOR('',#57073,10.);
#7880=VECTOR('',#57074,10.);
#7881=VECTOR('',#57077,10.);
#7882=VECTOR('',#57080,10.);
#7883=VECTOR('',#57081,10.);
#7884=VECTOR('',#57084,10.);
#7885=VECTOR('',#57087,10.);
#7886=VECTOR('',#57088,10.);
#7887=VECTOR('',#57091,10.);
#7888=VECTOR('',#57094,10.);
#7889=VECTOR('',#57095,10.);
#7890=VECTOR('',#57098,10.);
#7891=VECTOR('',#57101,10.);
#7892=VECTOR('',#57102,10.);
#7893=VECTOR('',#57105,10.);
#7894=VECTOR('',#57108,10.);
#7895=VECTOR('',#57109,10.);
#7896=VECTOR('',#57112,10.);
#7897=VECTOR('',#57115,10.);
#7898=VECTOR('',#57116,10.);
#7899=VECTOR('',#57119,10.);
#7900=VECTOR('',#57122,10.);
#7901=VECTOR('',#57123,10.);
#7902=VECTOR('',#57126,10.);
#7903=VECTOR('',#57129,10.);
#7904=VECTOR('',#57130,10.);
#7905=VECTOR('',#57133,10.);
#7906=VECTOR('',#57136,10.);
#7907=VECTOR('',#57137,10.);
#7908=VECTOR('',#57140,10.);
#7909=VECTOR('',#57143,10.);
#7910=VECTOR('',#57144,10.);
#7911=VECTOR('',#57147,10.);
#7912=VECTOR('',#57150,10.);
#7913=VECTOR('',#57151,10.);
#7914=VECTOR('',#57154,10.);
#7915=VECTOR('',#57157,10.);
#7916=VECTOR('',#57158,10.);
#7917=VECTOR('',#57161,10.);
#7918=VECTOR('',#57164,10.);
#7919=VECTOR('',#57165,10.);
#7920=VECTOR('',#57168,10.);
#7921=VECTOR('',#57171,10.);
#7922=VECTOR('',#57172,10.);
#7923=VECTOR('',#57175,10.);
#7924=VECTOR('',#57178,10.);
#7925=VECTOR('',#57179,10.);
#7926=VECTOR('',#57182,10.);
#7927=VECTOR('',#57185,10.);
#7928=VECTOR('',#57186,10.);
#7929=VECTOR('',#57189,10.);
#7930=VECTOR('',#57192,10.);
#7931=VECTOR('',#57193,10.);
#7932=VECTOR('',#57196,10.);
#7933=VECTOR('',#57199,10.);
#7934=VECTOR('',#57200,10.);
#7935=VECTOR('',#57203,10.);
#7936=VECTOR('',#57206,10.);
#7937=VECTOR('',#57207,10.);
#7938=VECTOR('',#57210,10.);
#7939=VECTOR('',#57213,10.);
#7940=VECTOR('',#57214,10.);
#7941=VECTOR('',#57217,10.);
#7942=VECTOR('',#57220,10.);
#7943=VECTOR('',#57221,10.);
#7944=VECTOR('',#57224,10.);
#7945=VECTOR('',#57227,10.);
#7946=VECTOR('',#57228,10.);
#7947=VECTOR('',#57231,10.);
#7948=VECTOR('',#57234,10.);
#7949=VECTOR('',#57235,10.);
#7950=VECTOR('',#57238,10.);
#7951=VECTOR('',#57241,10.);
#7952=VECTOR('',#57242,10.);
#7953=VECTOR('',#57245,10.);
#7954=VECTOR('',#57248,10.);
#7955=VECTOR('',#57249,10.);
#7956=VECTOR('',#57252,10.);
#7957=VECTOR('',#57255,10.);
#7958=VECTOR('',#57256,10.);
#7959=VECTOR('',#57259,10.);
#7960=VECTOR('',#57262,10.);
#7961=VECTOR('',#57263,10.);
#7962=VECTOR('',#57266,10.);
#7963=VECTOR('',#57269,10.);
#7964=VECTOR('',#57270,10.);
#7965=VECTOR('',#57273,10.);
#7966=VECTOR('',#57276,10.);
#7967=VECTOR('',#57277,10.);
#7968=VECTOR('',#57280,10.);
#7969=VECTOR('',#57283,10.);
#7970=VECTOR('',#57284,10.);
#7971=VECTOR('',#57287,10.);
#7972=VECTOR('',#57290,10.);
#7973=VECTOR('',#57291,10.);
#7974=VECTOR('',#57294,10.);
#7975=VECTOR('',#57297,10.);
#7976=VECTOR('',#57298,10.);
#7977=VECTOR('',#57301,10.);
#7978=VECTOR('',#57304,10.);
#7979=VECTOR('',#57305,10.);
#7980=VECTOR('',#57308,10.);
#7981=VECTOR('',#57311,10.);
#7982=VECTOR('',#57312,10.);
#7983=VECTOR('',#57315,10.);
#7984=VECTOR('',#57318,10.);
#7985=VECTOR('',#57319,10.);
#7986=VECTOR('',#57322,10.);
#7987=VECTOR('',#57323,10.);
#7988=VECTOR('',#57326,10.);
#7989=VECTOR('',#57327,10.);
#7990=VECTOR('',#57330,10.);
#7991=VECTOR('',#57331,10.);
#7992=VECTOR('',#57334,10.);
#7993=VECTOR('',#57335,10.);
#7994=VECTOR('',#57338,10.);
#7995=VECTOR('',#57339,10.);
#7996=VECTOR('',#57342,10.);
#7997=VECTOR('',#57343,10.);
#7998=VECTOR('',#57346,10.);
#7999=VECTOR('',#57347,10.);
#8000=VECTOR('',#57350,10.);
#8001=VECTOR('',#57351,10.);
#8002=VECTOR('',#57354,10.);
#8003=VECTOR('',#57355,10.);
#8004=VECTOR('',#57358,10.);
#8005=VECTOR('',#57359,10.);
#8006=VECTOR('',#57362,10.);
#8007=VECTOR('',#57363,10.);
#8008=VECTOR('',#57366,10.);
#8009=VECTOR('',#57367,10.);
#8010=VECTOR('',#57370,10.);
#8011=VECTOR('',#57371,10.);
#8012=VECTOR('',#57374,10.);
#8013=VECTOR('',#57375,10.);
#8014=VECTOR('',#57378,10.);
#8015=VECTOR('',#57379,10.);
#8016=VECTOR('',#57382,10.);
#8017=VECTOR('',#57383,10.);
#8018=VECTOR('',#57386,10.);
#8019=VECTOR('',#57387,10.);
#8020=VECTOR('',#57390,10.);
#8021=VECTOR('',#57391,10.);
#8022=VECTOR('',#57394,10.);
#8023=VECTOR('',#57395,10.);
#8024=VECTOR('',#57398,10.);
#8025=VECTOR('',#57399,10.);
#8026=VECTOR('',#57402,10.);
#8027=VECTOR('',#57403,10.);
#8028=VECTOR('',#57406,10.);
#8029=VECTOR('',#57407,10.);
#8030=VECTOR('',#57410,10.);
#8031=VECTOR('',#57411,10.);
#8032=VECTOR('',#57414,10.);
#8033=VECTOR('',#57415,10.);
#8034=VECTOR('',#57418,10.);
#8035=VECTOR('',#57419,10.);
#8036=VECTOR('',#57422,10.);
#8037=VECTOR('',#57423,10.);
#8038=VECTOR('',#57426,10.);
#8039=VECTOR('',#57427,10.);
#8040=VECTOR('',#57430,10.);
#8041=VECTOR('',#57431,10.);
#8042=VECTOR('',#57434,10.);
#8043=VECTOR('',#57435,10.);
#8044=VECTOR('',#57438,10.);
#8045=VECTOR('',#57439,10.);
#8046=VECTOR('',#57442,10.);
#8047=VECTOR('',#57443,10.);
#8048=VECTOR('',#57446,10.);
#8049=VECTOR('',#57447,10.);
#8050=VECTOR('',#57450,10.);
#8051=VECTOR('',#57451,10.);
#8052=VECTOR('',#57454,10.);
#8053=VECTOR('',#57455,10.);
#8054=VECTOR('',#57458,10.);
#8055=VECTOR('',#57459,10.);
#8056=VECTOR('',#57462,10.);
#8057=VECTOR('',#57465,10.);
#8058=VECTOR('',#57468,10.);
#8059=VECTOR('',#57471,10.);
#8060=VECTOR('',#57474,10.);
#8061=VECTOR('',#57477,10.);
#8062=VECTOR('',#57480,10.);
#8063=VECTOR('',#57483,10.);
#8064=VECTOR('',#57486,10.);
#8065=VECTOR('',#57489,10.);
#8066=VECTOR('',#57492,10.);
#8067=VECTOR('',#57495,10.);
#8068=VECTOR('',#57498,10.);
#8069=VECTOR('',#57501,10.);
#8070=VECTOR('',#57504,10.);
#8071=VECTOR('',#57507,10.);
#8072=VECTOR('',#57510,10.);
#8073=VECTOR('',#57513,10.);
#8074=VECTOR('',#57516,10.);
#8075=VECTOR('',#57519,10.);
#8076=VECTOR('',#57522,10.);
#8077=VECTOR('',#57525,10.);
#8078=VECTOR('',#57528,10.);
#8079=VECTOR('',#57531,10.);
#8080=VECTOR('',#57534,10.);
#8081=VECTOR('',#57537,10.);
#8082=VECTOR('',#57540,10.);
#8083=VECTOR('',#57543,10.);
#8084=VECTOR('',#57546,10.);
#8085=VECTOR('',#57549,10.);
#8086=VECTOR('',#57552,10.);
#8087=VECTOR('',#57555,10.);
#8088=VECTOR('',#57558,10.);
#8089=VECTOR('',#57561,10.);
#8090=VECTOR('',#57564,10.);
#8091=VECTOR('',#57567,10.);
#8092=VECTOR('',#57570,10.);
#8093=VECTOR('',#57573,10.);
#8094=VECTOR('',#57576,10.);
#8095=VECTOR('',#57579,10.);
#8096=VECTOR('',#57582,10.);
#8097=VECTOR('',#57585,10.);
#8098=VECTOR('',#57588,10.);
#8099=VECTOR('',#57591,10.);
#8100=VECTOR('',#57594,10.);
#8101=VECTOR('',#57597,10.);
#8102=VECTOR('',#57600,10.);
#8103=VECTOR('',#57603,10.);
#8104=VECTOR('',#57606,10.);
#8105=VECTOR('',#57609,10.);
#8106=VECTOR('',#57612,10.);
#8107=VECTOR('',#57615,10.);
#8108=VECTOR('',#57618,10.);
#8109=VECTOR('',#57621,10.);
#8110=VECTOR('',#57624,10.);
#8111=VECTOR('',#57627,10.);
#8112=VECTOR('',#57630,10.);
#8113=VECTOR('',#57633,10.);
#8114=VECTOR('',#57636,10.);
#8115=VECTOR('',#57639,10.);
#8116=VECTOR('',#57642,10.);
#8117=VECTOR('',#57645,10.);
#8118=VECTOR('',#57648,10.);
#8119=VECTOR('',#57651,10.);
#8120=VECTOR('',#57654,10.);
#8121=VECTOR('',#57657,10.);
#8122=VECTOR('',#57660,10.);
#8123=VECTOR('',#57663,10.);
#8124=VECTOR('',#57666,10.);
#8125=VECTOR('',#57669,10.);
#8126=VECTOR('',#57672,10.);
#8127=VECTOR('',#57675,10.);
#8128=VECTOR('',#57676,10.);
#8129=VECTOR('',#57679,10.);
#8130=VECTOR('',#57680,10.);
#8131=VECTOR('',#57683,10.);
#8132=VECTOR('',#57684,10.);
#8133=VECTOR('',#57687,10.);
#8134=VECTOR('',#57688,10.);
#8135=VECTOR('',#57691,10.);
#8136=VECTOR('',#57692,10.);
#8137=VECTOR('',#57695,10.);
#8138=VECTOR('',#57696,10.);
#8139=VECTOR('',#57699,10.);
#8140=VECTOR('',#57700,10.);
#8141=VECTOR('',#57703,10.);
#8142=VECTOR('',#57704,10.);
#8143=VECTOR('',#57707,10.);
#8144=VECTOR('',#57708,10.);
#8145=VECTOR('',#57711,10.);
#8146=VECTOR('',#57712,10.);
#8147=VECTOR('',#57715,10.);
#8148=VECTOR('',#57716,10.);
#8149=VECTOR('',#57719,10.);
#8150=VECTOR('',#57720,10.);
#8151=VECTOR('',#57723,10.);
#8152=VECTOR('',#57724,10.);
#8153=VECTOR('',#57727,10.);
#8154=VECTOR('',#57728,10.);
#8155=VECTOR('',#57731,10.);
#8156=VECTOR('',#57732,10.);
#8157=VECTOR('',#57735,10.);
#8158=VECTOR('',#57736,10.);
#8159=VECTOR('',#57739,10.);
#8160=VECTOR('',#57740,10.);
#8161=VECTOR('',#57743,10.);
#8162=VECTOR('',#57744,10.);
#8163=VECTOR('',#57747,10.);
#8164=VECTOR('',#57748,10.);
#8165=VECTOR('',#57751,10.);
#8166=VECTOR('',#57752,10.);
#8167=VECTOR('',#57755,10.);
#8168=VECTOR('',#57756,10.);
#8169=VECTOR('',#57759,10.);
#8170=VECTOR('',#57760,10.);
#8171=VECTOR('',#57763,10.);
#8172=VECTOR('',#57764,10.);
#8173=VECTOR('',#57767,10.);
#8174=VECTOR('',#57768,10.);
#8175=VECTOR('',#57771,10.);
#8176=VECTOR('',#57772,10.);
#8177=VECTOR('',#57775,10.);
#8178=VECTOR('',#57776,10.);
#8179=VECTOR('',#57779,10.);
#8180=VECTOR('',#57780,10.);
#8181=VECTOR('',#57783,10.);
#8182=VECTOR('',#57784,10.);
#8183=VECTOR('',#57787,10.);
#8184=VECTOR('',#57788,10.);
#8185=VECTOR('',#57791,10.);
#8186=VECTOR('',#57792,10.);
#8187=VECTOR('',#57795,10.);
#8188=VECTOR('',#57796,10.);
#8189=VECTOR('',#57799,10.);
#8190=VECTOR('',#57800,10.);
#8191=VECTOR('',#57803,10.);
#8192=VECTOR('',#57804,10.);
#8193=VECTOR('',#57807,10.);
#8194=VECTOR('',#57808,10.);
#8195=VECTOR('',#57811,10.);
#8196=VECTOR('',#57812,10.);
#8197=VECTOR('',#57815,10.);
#8198=VECTOR('',#57816,10.);
#8199=VECTOR('',#57819,10.);
#8200=VECTOR('',#57822,10.);
#8201=VECTOR('',#57825,10.);
#8202=VECTOR('',#57828,10.);
#8203=VECTOR('',#57831,10.);
#8204=VECTOR('',#57834,10.);
#8205=VECTOR('',#57837,10.);
#8206=VECTOR('',#57840,10.);
#8207=VECTOR('',#57843,10.);
#8208=VECTOR('',#57846,10.);
#8209=VECTOR('',#57849,10.);
#8210=VECTOR('',#57852,10.);
#8211=VECTOR('',#57855,10.);
#8212=VECTOR('',#57858,10.);
#8213=VECTOR('',#57861,10.);
#8214=VECTOR('',#57864,10.);
#8215=VECTOR('',#57867,10.);
#8216=VECTOR('',#57870,10.);
#8217=VECTOR('',#57873,10.);
#8218=VECTOR('',#57876,10.);
#8219=VECTOR('',#57879,10.);
#8220=VECTOR('',#57882,10.);
#8221=VECTOR('',#57885,10.);
#8222=VECTOR('',#57888,10.);
#8223=VECTOR('',#57891,10.);
#8224=VECTOR('',#57894,10.);
#8225=VECTOR('',#57897,10.);
#8226=VECTOR('',#57900,10.);
#8227=VECTOR('',#57903,10.);
#8228=VECTOR('',#57906,10.);
#8229=VECTOR('',#57909,10.);
#8230=VECTOR('',#57912,10.);
#8231=VECTOR('',#57915,10.);
#8232=VECTOR('',#57918,10.);
#8233=VECTOR('',#57921,10.);
#8234=VECTOR('',#57924,10.);
#8235=VECTOR('',#57927,10.);
#8236=VECTOR('',#57928,10.);
#8237=VECTOR('',#57933,10.);
#8238=VECTOR('',#57938,10.);
#8239=VECTOR('',#57943,10.);
#8240=VECTOR('',#57948,10.);
#8241=VECTOR('',#57953,10.);
#8242=VECTOR('',#57956,10.);
#8243=VECTOR('',#57957,10.);
#8244=VECTOR('',#57962,10.);
#8245=VECTOR('',#57967,10.);
#8246=VECTOR('',#57972,10.);
#8247=VECTOR('',#57977,10.);
#8248=VECTOR('',#57982,10.);
#8249=VECTOR('',#57985,10.);
#8250=VECTOR('',#57986,10.);
#8251=VECTOR('',#57993,10.);
#8252=VECTOR('',#57994,10.);
#8253=VECTOR('',#57999,10.);
#8254=VECTOR('',#58004,10.);
#8255=VECTOR('',#58009,10.);
#8256=VECTOR('',#58014,10.);
#8257=VECTOR('',#58019,10.);
#8258=VECTOR('',#58022,10.);
#8259=VECTOR('',#58023,10.);
#8260=VECTOR('',#58028,10.);
#8261=VECTOR('',#58033,10.);
#8262=VECTOR('',#58038,10.);
#8263=VECTOR('',#58043,10.);
#8264=VECTOR('',#58048,10.);
#8265=VECTOR('',#58051,10.);
#8266=VECTOR('',#58058,42.6);
#8267=VECTOR('',#58137,10.);
#8268=VECTOR('',#58148,10.);
#8269=VECTOR('',#58159,10.);
#8270=VECTOR('',#58162,10.);
#8271=VECTOR('',#58165,10.);
#8272=VECTOR('',#58168,10.);
#8273=VECTOR('',#58171,10.);
#8274=VECTOR('',#58174,10.);
#8275=VECTOR('',#58177,10.);
#8276=VECTOR('',#58180,10.);
#8277=VECTOR('',#58183,10.);
#8278=VECTOR('',#58186,10.);
#8279=VECTOR('',#58189,10.);
#8280=VECTOR('',#58192,10.);
#8281=VECTOR('',#58195,10.);
#8282=VECTOR('',#58198,10.);
#8283=VECTOR('',#58203,10.);
#8284=VECTOR('',#58204,10.);
#8285=VECTOR('',#58209,10.);
#8286=VECTOR('',#58214,10.);
#8287=VECTOR('',#58219,10.);
#8288=VECTOR('',#58224,10.);
#8289=VECTOR('',#58229,10.);
#8290=VECTOR('',#58232,10.);
#8291=VECTOR('',#58233,10.);
#8292=VECTOR('',#58238,10.);
#8293=VECTOR('',#58243,10.);
#8294=VECTOR('',#58248,10.);
#8295=VECTOR('',#58253,10.);
#8296=VECTOR('',#58258,10.);
#8297=VECTOR('',#58261,10.);
#8298=VECTOR('',#58270,10.);
#8299=VECTOR('',#58281,10.);
#8300=VECTOR('',#58292,10.);
#8301=VECTOR('',#58295,10.);
#8302=VECTOR('',#58298,10.);
#8303=VECTOR('',#58301,10.);
#8304=VECTOR('',#58304,10.);
#8305=VECTOR('',#58307,10.);
#8306=VECTOR('',#58310,10.);
#8307=VECTOR('',#58313,10.);
#8308=VECTOR('',#58316,10.);
#8309=VECTOR('',#58319,10.);
#8310=VECTOR('',#58322,10.);
#8311=VECTOR('',#58325,10.);
#8312=VECTOR('',#58328,10.);
#8313=VECTOR('',#58331,10.);
#8314=VECTOR('',#58336,10.);
#8315=VECTOR('',#58337,10.);
#8316=VECTOR('',#58342,10.);
#8317=VECTOR('',#58347,10.);
#8318=VECTOR('',#58352,10.);
#8319=VECTOR('',#58357,10.);
#8320=VECTOR('',#58362,10.);
#8321=VECTOR('',#58365,10.);
#8322=VECTOR('',#58366,10.);
#8323=VECTOR('',#58371,10.);
#8324=VECTOR('',#58376,10.);
#8325=VECTOR('',#58381,10.);
#8326=VECTOR('',#58386,10.);
#8327=VECTOR('',#58391,10.);
#8328=VECTOR('',#58394,10.);
#8329=VECTOR('',#58403,10.);
#8330=VECTOR('',#58414,10.);
#8331=VECTOR('',#58425,10.);
#8332=VECTOR('',#58428,10.);
#8333=VECTOR('',#58431,10.);
#8334=VECTOR('',#58434,10.);
#8335=VECTOR('',#58437,10.);
#8336=VECTOR('',#58440,10.);
#8337=VECTOR('',#58443,10.);
#8338=VECTOR('',#58446,10.);
#8339=VECTOR('',#58449,10.);
#8340=VECTOR('',#58452,10.);
#8341=VECTOR('',#58455,10.);
#8342=VECTOR('',#58458,10.);
#8343=VECTOR('',#58461,10.);
#8344=VECTOR('',#58464,10.);
#8345=VECTOR('',#58469,10.);
#8346=VECTOR('',#58470,10.);
#8347=VECTOR('',#58475,10.);
#8348=VECTOR('',#58480,10.);
#8349=VECTOR('',#58485,10.);
#8350=VECTOR('',#58490,10.);
#8351=VECTOR('',#58495,10.);
#8352=VECTOR('',#58498,10.);
#8353=VECTOR('',#58499,10.);
#8354=VECTOR('',#58504,10.);
#8355=VECTOR('',#58509,10.);
#8356=VECTOR('',#58514,10.);
#8357=VECTOR('',#58519,10.);
#8358=VECTOR('',#58524,10.);
#8359=VECTOR('',#58527,10.);
#8360=VECTOR('',#58536,10.);
#8361=VECTOR('',#58547,10.);
#8362=VECTOR('',#58558,10.);
#8363=VECTOR('',#58561,10.);
#8364=VECTOR('',#58564,10.);
#8365=VECTOR('',#58567,10.);
#8366=VECTOR('',#58570,10.);
#8367=VECTOR('',#58573,10.);
#8368=VECTOR('',#58576,10.);
#8369=VECTOR('',#58579,10.);
#8370=VECTOR('',#58582,10.);
#8371=VECTOR('',#58585,10.);
#8372=VECTOR('',#58588,10.);
#8373=VECTOR('',#58591,10.);
#8374=VECTOR('',#58594,10.);
#8375=VECTOR('',#58597,10.);
#8376=VECTOR('',#58602,10.);
#8377=VECTOR('',#58603,10.);
#8378=VECTOR('',#58608,10.);
#8379=VECTOR('',#58613,10.);
#8380=VECTOR('',#58618,10.);
#8381=VECTOR('',#58623,10.);
#8382=VECTOR('',#58628,10.);
#8383=VECTOR('',#58631,10.);
#8384=VECTOR('',#58632,10.);
#8385=VECTOR('',#58637,10.);
#8386=VECTOR('',#58642,10.);
#8387=VECTOR('',#58647,10.);
#8388=VECTOR('',#58652,10.);
#8389=VECTOR('',#58657,10.);
#8390=VECTOR('',#58660,10.);
#8391=VECTOR('',#58669,10.);
#8392=VECTOR('',#58680,10.);
#8393=VECTOR('',#58691,10.);
#8394=VECTOR('',#58694,10.);
#8395=VECTOR('',#58697,10.);
#8396=VECTOR('',#58700,10.);
#8397=VECTOR('',#58703,10.);
#8398=VECTOR('',#58706,10.);
#8399=VECTOR('',#58709,10.);
#8400=VECTOR('',#58712,10.);
#8401=VECTOR('',#58715,10.);
#8402=VECTOR('',#58718,10.);
#8403=VECTOR('',#58721,10.);
#8404=VECTOR('',#58724,10.);
#8405=VECTOR('',#58727,10.);
#8406=VECTOR('',#58730,10.);
#8407=VECTOR('',#58735,10.);
#8408=VECTOR('',#58736,10.);
#8409=VECTOR('',#58741,10.);
#8410=VECTOR('',#58746,10.);
#8411=VECTOR('',#58751,10.);
#8412=VECTOR('',#58756,10.);
#8413=VECTOR('',#58761,10.);
#8414=VECTOR('',#58764,10.);
#8415=VECTOR('',#58765,10.);
#8416=VECTOR('',#58770,10.);
#8417=VECTOR('',#58775,10.);
#8418=VECTOR('',#58780,10.);
#8419=VECTOR('',#58785,10.);
#8420=VECTOR('',#58790,10.);
#8421=VECTOR('',#58793,10.);
#8422=VECTOR('',#58802,10.);
#8423=VECTOR('',#58813,10.);
#8424=VECTOR('',#58824,10.);
#8425=VECTOR('',#58827,10.);
#8426=VECTOR('',#58830,10.);
#8427=VECTOR('',#58833,10.);
#8428=VECTOR('',#58836,10.);
#8429=VECTOR('',#58839,10.);
#8430=VECTOR('',#58842,10.);
#8431=VECTOR('',#58845,10.);
#8432=VECTOR('',#58848,10.);
#8433=VECTOR('',#58851,10.);
#8434=VECTOR('',#58854,10.);
#8435=VECTOR('',#58857,10.);
#8436=VECTOR('',#58860,10.);
#8437=VECTOR('',#58863,10.);
#8438=VECTOR('',#58868,10.);
#8439=VECTOR('',#58869,10.);
#8440=VECTOR('',#58874,10.);
#8441=VECTOR('',#58879,10.);
#8442=VECTOR('',#58884,10.);
#8443=VECTOR('',#58889,10.);
#8444=VECTOR('',#58894,10.);
#8445=VECTOR('',#58897,10.);
#8446=VECTOR('',#58898,10.);
#8447=VECTOR('',#58903,10.);
#8448=VECTOR('',#58908,10.);
#8449=VECTOR('',#58913,10.);
#8450=VECTOR('',#58918,10.);
#8451=VECTOR('',#58923,10.);
#8452=VECTOR('',#58926,10.);
#8453=VECTOR('',#58935,10.);
#8454=VECTOR('',#58946,10.);
#8455=VECTOR('',#58957,10.);
#8456=VECTOR('',#58960,10.);
#8457=VECTOR('',#58963,10.);
#8458=VECTOR('',#58966,10.);
#8459=VECTOR('',#58969,10.);
#8460=VECTOR('',#58972,10.);
#8461=VECTOR('',#58975,10.);
#8462=VECTOR('',#58978,10.);
#8463=VECTOR('',#58981,10.);
#8464=VECTOR('',#58984,10.);
#8465=VECTOR('',#58987,10.);
#8466=VECTOR('',#58990,10.);
#8467=VECTOR('',#58993,10.);
#8468=VECTOR('',#58996,10.);
#8469=VECTOR('',#59001,10.);
#8470=VECTOR('',#59002,10.);
#8471=VECTOR('',#59007,10.);
#8472=VECTOR('',#59012,10.);
#8473=VECTOR('',#59017,10.);
#8474=VECTOR('',#59022,10.);
#8475=VECTOR('',#59027,10.);
#8476=VECTOR('',#59030,10.);
#8477=VECTOR('',#59031,10.);
#8478=VECTOR('',#59036,10.);
#8479=VECTOR('',#59041,10.);
#8480=VECTOR('',#59046,10.);
#8481=VECTOR('',#59051,10.);
#8482=VECTOR('',#59056,10.);
#8483=VECTOR('',#59059,10.);
#8484=VECTOR('',#59068,10.);
#8485=VECTOR('',#59079,10.);
#8486=VECTOR('',#59090,10.);
#8487=VECTOR('',#59093,10.);
#8488=VECTOR('',#59096,10.);
#8489=VECTOR('',#59099,10.);
#8490=VECTOR('',#59102,10.);
#8491=VECTOR('',#59105,10.);
#8492=VECTOR('',#59108,10.);
#8493=VECTOR('',#59111,10.);
#8494=VECTOR('',#59114,10.);
#8495=VECTOR('',#59117,10.);
#8496=VECTOR('',#59120,10.);
#8497=VECTOR('',#59123,10.);
#8498=VECTOR('',#59126,10.);
#8499=VECTOR('',#59129,10.);
#8500=VECTOR('',#59134,10.);
#8501=VECTOR('',#59135,10.);
#8502=VECTOR('',#59140,10.);
#8503=VECTOR('',#59145,10.);
#8504=VECTOR('',#59150,10.);
#8505=VECTOR('',#59155,10.);
#8506=VECTOR('',#59160,10.);
#8507=VECTOR('',#59163,10.);
#8508=VECTOR('',#59164,10.);
#8509=VECTOR('',#59169,10.);
#8510=VECTOR('',#59174,10.);
#8511=VECTOR('',#59179,10.);
#8512=VECTOR('',#59184,10.);
#8513=VECTOR('',#59189,10.);
#8514=VECTOR('',#59192,10.);
#8515=VECTOR('',#59201,10.);
#8516=VECTOR('',#59212,10.);
#8517=VECTOR('',#59223,10.);
#8518=VECTOR('',#59226,10.);
#8519=VECTOR('',#59229,10.);
#8520=VECTOR('',#59232,10.);
#8521=VECTOR('',#59235,10.);
#8522=VECTOR('',#59238,10.);
#8523=VECTOR('',#59241,10.);
#8524=VECTOR('',#59244,10.);
#8525=VECTOR('',#59247,10.);
#8526=VECTOR('',#59250,10.);
#8527=VECTOR('',#59253,10.);
#8528=VECTOR('',#59256,10.);
#8529=VECTOR('',#59259,10.);
#8530=VECTOR('',#59262,10.);
#8531=VECTOR('',#59267,10.);
#8532=VECTOR('',#59268,10.);
#8533=VECTOR('',#59273,10.);
#8534=VECTOR('',#59278,10.);
#8535=VECTOR('',#59283,10.);
#8536=VECTOR('',#59288,10.);
#8537=VECTOR('',#59293,10.);
#8538=VECTOR('',#59296,10.);
#8539=VECTOR('',#59297,10.);
#8540=VECTOR('',#59302,10.);
#8541=VECTOR('',#59307,10.);
#8542=VECTOR('',#59312,10.);
#8543=VECTOR('',#59317,10.);
#8544=VECTOR('',#59322,10.);
#8545=VECTOR('',#59325,10.);
#8546=VECTOR('',#59334,10.);
#8547=VECTOR('',#59345,10.);
#8548=VECTOR('',#59356,10.);
#8549=VECTOR('',#59359,10.);
#8550=VECTOR('',#59362,10.);
#8551=VECTOR('',#59365,10.);
#8552=VECTOR('',#59368,10.);
#8553=VECTOR('',#59371,10.);
#8554=VECTOR('',#59374,10.);
#8555=VECTOR('',#59377,10.);
#8556=VECTOR('',#59380,10.);
#8557=VECTOR('',#59383,10.);
#8558=VECTOR('',#59386,10.);
#8559=VECTOR('',#59389,10.);
#8560=VECTOR('',#59392,10.);
#8561=VECTOR('',#59395,10.);
#8562=VECTOR('',#59400,10.);
#8563=VECTOR('',#59401,10.);
#8564=VECTOR('',#59406,10.);
#8565=VECTOR('',#59411,10.);
#8566=VECTOR('',#59416,10.);
#8567=VECTOR('',#59421,10.);
#8568=VECTOR('',#59426,10.);
#8569=VECTOR('',#59429,10.);
#8570=VECTOR('',#59430,10.);
#8571=VECTOR('',#59435,10.);
#8572=VECTOR('',#59440,10.);
#8573=VECTOR('',#59445,10.);
#8574=VECTOR('',#59450,10.);
#8575=VECTOR('',#59455,10.);
#8576=VECTOR('',#59458,10.);
#8577=VECTOR('',#59467,10.);
#8578=VECTOR('',#59478,10.);
#8579=VECTOR('',#59489,10.);
#8580=VECTOR('',#59492,10.);
#8581=VECTOR('',#59495,10.);
#8582=VECTOR('',#59498,10.);
#8583=VECTOR('',#59501,10.);
#8584=VECTOR('',#59504,10.);
#8585=VECTOR('',#59507,10.);
#8586=VECTOR('',#59510,10.);
#8587=VECTOR('',#59513,10.);
#8588=VECTOR('',#59516,10.);
#8589=VECTOR('',#59519,10.);
#8590=VECTOR('',#59522,10.);
#8591=VECTOR('',#59525,10.);
#8592=VECTOR('',#59528,10.);
#8593=VECTOR('',#59533,10.);
#8594=VECTOR('',#59534,10.);
#8595=VECTOR('',#59539,10.);
#8596=VECTOR('',#59544,10.);
#8597=VECTOR('',#59549,10.);
#8598=VECTOR('',#59554,10.);
#8599=VECTOR('',#59559,10.);
#8600=VECTOR('',#59562,10.);
#8601=VECTOR('',#59563,10.);
#8602=VECTOR('',#59568,10.);
#8603=VECTOR('',#59573,10.);
#8604=VECTOR('',#59578,10.);
#8605=VECTOR('',#59583,10.);
#8606=VECTOR('',#59588,10.);
#8607=VECTOR('',#59591,10.);
#8608=VECTOR('',#59600,10.);
#8609=VECTOR('',#59611,10.);
#8610=VECTOR('',#59622,10.);
#8611=VECTOR('',#59625,10.);
#8612=VECTOR('',#59628,10.);
#8613=VECTOR('',#59631,10.);
#8614=VECTOR('',#59634,10.);
#8615=VECTOR('',#59637,10.);
#8616=VECTOR('',#59640,10.);
#8617=VECTOR('',#59643,10.);
#8618=VECTOR('',#59646,10.);
#8619=VECTOR('',#59649,10.);
#8620=VECTOR('',#59652,10.);
#8621=VECTOR('',#59655,10.);
#8622=VECTOR('',#59658,10.);
#8623=VECTOR('',#59661,10.);
#8624=VECTOR('',#59666,10.);
#8625=VECTOR('',#59667,10.);
#8626=VECTOR('',#59672,10.);
#8627=VECTOR('',#59677,10.);
#8628=VECTOR('',#59682,10.);
#8629=VECTOR('',#59687,10.);
#8630=VECTOR('',#59692,10.);
#8631=VECTOR('',#59695,10.);
#8632=VECTOR('',#59696,10.);
#8633=VECTOR('',#59701,10.);
#8634=VECTOR('',#59706,10.);
#8635=VECTOR('',#59711,10.);
#8636=VECTOR('',#59716,10.);
#8637=VECTOR('',#59721,10.);
#8638=VECTOR('',#59724,10.);
#8639=VECTOR('',#59733,10.);
#8640=VECTOR('',#59744,10.);
#8641=VECTOR('',#59755,10.);
#8642=VECTOR('',#59758,10.);
#8643=VECTOR('',#59761,10.);
#8644=VECTOR('',#59764,10.);
#8645=VECTOR('',#59767,10.);
#8646=VECTOR('',#59770,10.);
#8647=VECTOR('',#59773,10.);
#8648=VECTOR('',#59776,10.);
#8649=VECTOR('',#59779,10.);
#8650=VECTOR('',#59782,10.);
#8651=VECTOR('',#59785,10.);
#8652=VECTOR('',#59788,10.);
#8653=VECTOR('',#59791,10.);
#8654=VECTOR('',#59794,10.);
#8655=VECTOR('',#59799,10.);
#8656=VECTOR('',#59800,10.);
#8657=VECTOR('',#59805,10.);
#8658=VECTOR('',#59810,10.);
#8659=VECTOR('',#59815,10.);
#8660=VECTOR('',#59820,10.);
#8661=VECTOR('',#59825,10.);
#8662=VECTOR('',#59828,10.);
#8663=VECTOR('',#59829,10.);
#8664=VECTOR('',#59834,10.);
#8665=VECTOR('',#59839,10.);
#8666=VECTOR('',#59844,10.);
#8667=VECTOR('',#59849,10.);
#8668=VECTOR('',#59854,10.);
#8669=VECTOR('',#59857,10.);
#8670=VECTOR('',#59866,10.);
#8671=VECTOR('',#59877,10.);
#8672=VECTOR('',#59888,10.);
#8673=VECTOR('',#59891,10.);
#8674=VECTOR('',#59894,10.);
#8675=VECTOR('',#59897,10.);
#8676=VECTOR('',#59900,10.);
#8677=VECTOR('',#59903,10.);
#8678=VECTOR('',#59906,10.);
#8679=VECTOR('',#59909,10.);
#8680=VECTOR('',#59912,10.);
#8681=VECTOR('',#59915,10.);
#8682=VECTOR('',#59918,10.);
#8683=VECTOR('',#59921,10.);
#8684=VECTOR('',#59924,10.);
#8685=VECTOR('',#59927,10.);
#8686=VECTOR('',#59932,10.);
#8687=VECTOR('',#59933,10.);
#8688=VECTOR('',#59938,10.);
#8689=VECTOR('',#59943,10.);
#8690=VECTOR('',#59948,10.);
#8691=VECTOR('',#59953,10.);
#8692=VECTOR('',#59958,10.);
#8693=VECTOR('',#59961,10.);
#8694=VECTOR('',#59962,10.);
#8695=VECTOR('',#59967,10.);
#8696=VECTOR('',#59972,10.);
#8697=VECTOR('',#59977,10.);
#8698=VECTOR('',#59982,10.);
#8699=VECTOR('',#59987,10.);
#8700=VECTOR('',#59990,10.);
#8701=VECTOR('',#59999,10.);
#8702=VECTOR('',#60010,10.);
#8703=VECTOR('',#60021,10.);
#8704=VECTOR('',#60024,10.);
#8705=VECTOR('',#60027,10.);
#8706=VECTOR('',#60030,10.);
#8707=VECTOR('',#60033,10.);
#8708=VECTOR('',#60036,10.);
#8709=VECTOR('',#60039,10.);
#8710=VECTOR('',#60042,10.);
#8711=VECTOR('',#60045,10.);
#8712=VECTOR('',#60048,10.);
#8713=VECTOR('',#60051,10.);
#8714=VECTOR('',#60054,10.);
#8715=VECTOR('',#60057,10.);
#8716=VECTOR('',#60060,10.);
#8717=VECTOR('',#60065,10.);
#8718=VECTOR('',#60066,10.);
#8719=VECTOR('',#60071,10.);
#8720=VECTOR('',#60076,10.);
#8721=VECTOR('',#60081,10.);
#8722=VECTOR('',#60086,10.);
#8723=VECTOR('',#60091,10.);
#8724=VECTOR('',#60094,10.);
#8725=VECTOR('',#60095,10.);
#8726=VECTOR('',#60100,10.);
#8727=VECTOR('',#60105,10.);
#8728=VECTOR('',#60110,10.);
#8729=VECTOR('',#60115,10.);
#8730=VECTOR('',#60120,10.);
#8731=VECTOR('',#60123,10.);
#8732=VECTOR('',#60132,10.);
#8733=VECTOR('',#60143,10.);
#8734=VECTOR('',#60154,10.);
#8735=VECTOR('',#60157,10.);
#8736=VECTOR('',#60160,10.);
#8737=VECTOR('',#60163,10.);
#8738=VECTOR('',#60166,10.);
#8739=VECTOR('',#60169,10.);
#8740=VECTOR('',#60172,10.);
#8741=VECTOR('',#60175,10.);
#8742=VECTOR('',#60178,10.);
#8743=VECTOR('',#60181,10.);
#8744=VECTOR('',#60184,10.);
#8745=VECTOR('',#60187,10.);
#8746=VECTOR('',#60190,10.);
#8747=VECTOR('',#60193,10.);
#8748=VECTOR('',#60198,10.);
#8749=VECTOR('',#60199,10.);
#8750=VECTOR('',#60204,10.);
#8751=VECTOR('',#60209,10.);
#8752=VECTOR('',#60214,10.);
#8753=VECTOR('',#60219,10.);
#8754=VECTOR('',#60224,10.);
#8755=VECTOR('',#60227,10.);
#8756=VECTOR('',#60228,10.);
#8757=VECTOR('',#60233,10.);
#8758=VECTOR('',#60238,10.);
#8759=VECTOR('',#60243,10.);
#8760=VECTOR('',#60248,10.);
#8761=VECTOR('',#60253,10.);
#8762=VECTOR('',#60256,10.);
#8763=VECTOR('',#60265,10.);
#8764=VECTOR('',#60276,10.);
#8765=VECTOR('',#60287,10.);
#8766=VECTOR('',#60290,10.);
#8767=VECTOR('',#60293,10.);
#8768=VECTOR('',#60296,10.);
#8769=VECTOR('',#60299,10.);
#8770=VECTOR('',#60302,10.);
#8771=VECTOR('',#60305,10.);
#8772=VECTOR('',#60308,10.);
#8773=VECTOR('',#60311,10.);
#8774=VECTOR('',#60314,10.);
#8775=VECTOR('',#60317,10.);
#8776=VECTOR('',#60320,10.);
#8777=VECTOR('',#60323,10.);
#8778=VECTOR('',#60326,10.);
#8779=VECTOR('',#60331,10.);
#8780=VECTOR('',#60332,10.);
#8781=VECTOR('',#60337,10.);
#8782=VECTOR('',#60342,10.);
#8783=VECTOR('',#60347,10.);
#8784=VECTOR('',#60352,10.);
#8785=VECTOR('',#60357,10.);
#8786=VECTOR('',#60360,10.);
#8787=VECTOR('',#60361,10.);
#8788=VECTOR('',#60366,10.);
#8789=VECTOR('',#60371,10.);
#8790=VECTOR('',#60376,10.);
#8791=VECTOR('',#60381,10.);
#8792=VECTOR('',#60386,10.);
#8793=VECTOR('',#60389,10.);
#8794=VECTOR('',#60398,10.);
#8795=VECTOR('',#60409,10.);
#8796=VECTOR('',#60420,10.);
#8797=VECTOR('',#60423,10.);
#8798=VECTOR('',#60426,10.);
#8799=VECTOR('',#60429,10.);
#8800=VECTOR('',#60432,10.);
#8801=VECTOR('',#60435,10.);
#8802=VECTOR('',#60438,10.);
#8803=VECTOR('',#60441,10.);
#8804=VECTOR('',#60444,10.);
#8805=VECTOR('',#60447,10.);
#8806=VECTOR('',#60450,10.);
#8807=VECTOR('',#60453,10.);
#8808=VECTOR('',#60456,10.);
#8809=VECTOR('',#60459,10.);
#8810=VECTOR('',#60464,10.);
#8811=VECTOR('',#60465,10.);
#8812=VECTOR('',#60470,10.);
#8813=VECTOR('',#60475,10.);
#8814=VECTOR('',#60480,10.);
#8815=VECTOR('',#60485,10.);
#8816=VECTOR('',#60490,10.);
#8817=VECTOR('',#60493,10.);
#8818=VECTOR('',#60494,10.);
#8819=VECTOR('',#60499,10.);
#8820=VECTOR('',#60504,10.);
#8821=VECTOR('',#60509,10.);
#8822=VECTOR('',#60514,10.);
#8823=VECTOR('',#60519,10.);
#8824=VECTOR('',#60522,10.);
#8825=VECTOR('',#60531,10.);
#8826=VECTOR('',#60542,10.);
#8827=VECTOR('',#60553,10.);
#8828=VECTOR('',#60556,10.);
#8829=VECTOR('',#60559,10.);
#8830=VECTOR('',#60562,10.);
#8831=VECTOR('',#60565,10.);
#8832=VECTOR('',#60568,10.);
#8833=VECTOR('',#60571,10.);
#8834=VECTOR('',#60574,10.);
#8835=VECTOR('',#60577,10.);
#8836=VECTOR('',#60580,10.);
#8837=VECTOR('',#60583,10.);
#8838=VECTOR('',#60586,10.);
#8839=VECTOR('',#60589,10.);
#8840=VECTOR('',#60592,10.);
#8841=VECTOR('',#60597,10.);
#8842=VECTOR('',#60598,10.);
#8843=VECTOR('',#60603,10.);
#8844=VECTOR('',#60608,10.);
#8845=VECTOR('',#60613,10.);
#8846=VECTOR('',#60618,10.);
#8847=VECTOR('',#60623,10.);
#8848=VECTOR('',#60626,10.);
#8849=VECTOR('',#60627,10.);
#8850=VECTOR('',#60632,10.);
#8851=VECTOR('',#60637,10.);
#8852=VECTOR('',#60642,10.);
#8853=VECTOR('',#60647,10.);
#8854=VECTOR('',#60652,10.);
#8855=VECTOR('',#60655,10.);
#8856=VECTOR('',#60664,10.);
#8857=VECTOR('',#60675,10.);
#8858=VECTOR('',#60686,10.);
#8859=VECTOR('',#60689,10.);
#8860=VECTOR('',#60692,10.);
#8861=VECTOR('',#60695,10.);
#8862=VECTOR('',#60698,10.);
#8863=VECTOR('',#60701,10.);
#8864=VECTOR('',#60704,10.);
#8865=VECTOR('',#60707,10.);
#8866=VECTOR('',#60710,10.);
#8867=VECTOR('',#60713,10.);
#8868=VECTOR('',#60716,10.);
#8869=VECTOR('',#60719,10.);
#8870=VECTOR('',#60722,10.);
#8871=VECTOR('',#60725,10.);
#8872=VECTOR('',#60730,10.);
#8873=VECTOR('',#60731,10.);
#8874=VECTOR('',#60736,10.);
#8875=VECTOR('',#60741,10.);
#8876=VECTOR('',#60746,10.);
#8877=VECTOR('',#60751,10.);
#8878=VECTOR('',#60756,10.);
#8879=VECTOR('',#60759,10.);
#8880=VECTOR('',#60760,10.);
#8881=VECTOR('',#60765,10.);
#8882=VECTOR('',#60770,10.);
#8883=VECTOR('',#60775,10.);
#8884=VECTOR('',#60780,10.);
#8885=VECTOR('',#60785,10.);
#8886=VECTOR('',#60788,10.);
#8887=VECTOR('',#60797,10.);
#8888=VECTOR('',#60808,10.);
#8889=VECTOR('',#60819,10.);
#8890=VECTOR('',#60822,10.);
#8891=VECTOR('',#60825,10.);
#8892=VECTOR('',#60828,10.);
#8893=VECTOR('',#60831,10.);
#8894=VECTOR('',#60834,10.);
#8895=VECTOR('',#60837,10.);
#8896=VECTOR('',#60840,10.);
#8897=VECTOR('',#60843,10.);
#8898=VECTOR('',#60846,10.);
#8899=VECTOR('',#60849,10.);
#8900=VECTOR('',#60852,10.);
#8901=VECTOR('',#60855,10.);
#8902=VECTOR('',#60858,10.);
#8903=VECTOR('',#60863,10.);
#8904=VECTOR('',#60864,10.);
#8905=VECTOR('',#60869,10.);
#8906=VECTOR('',#60874,10.);
#8907=VECTOR('',#60879,10.);
#8908=VECTOR('',#60884,10.);
#8909=VECTOR('',#60889,10.);
#8910=VECTOR('',#60892,10.);
#8911=VECTOR('',#60893,10.);
#8912=VECTOR('',#60898,10.);
#8913=VECTOR('',#60903,10.);
#8914=VECTOR('',#60908,10.);
#8915=VECTOR('',#60913,10.);
#8916=VECTOR('',#60918,10.);
#8917=VECTOR('',#60921,10.);
#8918=VECTOR('',#60930,10.);
#8919=VECTOR('',#60941,10.);
#8920=VECTOR('',#60952,10.);
#8921=VECTOR('',#60955,10.);
#8922=VECTOR('',#60958,10.);
#8923=VECTOR('',#60961,10.);
#8924=VECTOR('',#60964,10.);
#8925=VECTOR('',#60967,10.);
#8926=VECTOR('',#60970,10.);
#8927=VECTOR('',#60973,10.);
#8928=VECTOR('',#60976,10.);
#8929=VECTOR('',#60979,10.);
#8930=VECTOR('',#60982,10.);
#8931=VECTOR('',#60985,10.);
#8932=VECTOR('',#60988,10.);
#8933=VECTOR('',#60991,10.);
#8934=VECTOR('',#60996,10.);
#8935=VECTOR('',#60997,10.);
#8936=VECTOR('',#61002,10.);
#8937=VECTOR('',#61007,10.);
#8938=VECTOR('',#61012,10.);
#8939=VECTOR('',#61017,10.);
#8940=VECTOR('',#61022,10.);
#8941=VECTOR('',#61025,10.);
#8942=VECTOR('',#61026,10.);
#8943=VECTOR('',#61031,10.);
#8944=VECTOR('',#61036,10.);
#8945=VECTOR('',#61041,10.);
#8946=VECTOR('',#61046,10.);
#8947=VECTOR('',#61051,10.);
#8948=VECTOR('',#61054,10.);
#8949=VECTOR('',#61063,10.);
#8950=VECTOR('',#61074,10.);
#8951=VECTOR('',#61085,10.);
#8952=VECTOR('',#61088,10.);
#8953=VECTOR('',#61091,10.);
#8954=VECTOR('',#61094,10.);
#8955=VECTOR('',#61097,10.);
#8956=VECTOR('',#61100,10.);
#8957=VECTOR('',#61103,10.);
#8958=VECTOR('',#61106,10.);
#8959=VECTOR('',#61109,10.);
#8960=VECTOR('',#61112,10.);
#8961=VECTOR('',#61115,10.);
#8962=VECTOR('',#61118,10.);
#8963=VECTOR('',#61121,10.);
#8964=VECTOR('',#61124,10.);
#8965=VECTOR('',#61129,10.);
#8966=VECTOR('',#61130,10.);
#8967=VECTOR('',#61135,10.);
#8968=VECTOR('',#61140,10.);
#8969=VECTOR('',#61145,10.);
#8970=VECTOR('',#61150,10.);
#8971=VECTOR('',#61155,10.);
#8972=VECTOR('',#61158,10.);
#8973=VECTOR('',#61159,10.);
#8974=VECTOR('',#61164,10.);
#8975=VECTOR('',#61169,10.);
#8976=VECTOR('',#61174,10.);
#8977=VECTOR('',#61179,10.);
#8978=VECTOR('',#61184,10.);
#8979=VECTOR('',#61187,10.);
#8980=VECTOR('',#61196,10.);
#8981=VECTOR('',#61207,10.);
#8982=VECTOR('',#61218,10.);
#8983=VECTOR('',#61221,10.);
#8984=VECTOR('',#61224,10.);
#8985=VECTOR('',#61227,10.);
#8986=VECTOR('',#61230,10.);
#8987=VECTOR('',#61233,10.);
#8988=VECTOR('',#61236,10.);
#8989=VECTOR('',#61239,10.);
#8990=VECTOR('',#61242,10.);
#8991=VECTOR('',#61245,10.);
#8992=VECTOR('',#61248,10.);
#8993=VECTOR('',#61251,10.);
#8994=VECTOR('',#61254,10.);
#8995=VECTOR('',#61257,10.);
#8996=VECTOR('',#61262,10.);
#8997=VECTOR('',#61263,10.);
#8998=VECTOR('',#61268,10.);
#8999=VECTOR('',#61273,10.);
#9000=VECTOR('',#61278,10.);
#9001=VECTOR('',#61283,10.);
#9002=VECTOR('',#61288,10.);
#9003=VECTOR('',#61291,10.);
#9004=VECTOR('',#61292,10.);
#9005=VECTOR('',#61297,10.);
#9006=VECTOR('',#61302,10.);
#9007=VECTOR('',#61307,10.);
#9008=VECTOR('',#61312,10.);
#9009=VECTOR('',#61317,10.);
#9010=VECTOR('',#61320,10.);
#9011=VECTOR('',#61329,10.);
#9012=VECTOR('',#61340,10.);
#9013=VECTOR('',#61351,10.);
#9014=VECTOR('',#61354,10.);
#9015=VECTOR('',#61357,10.);
#9016=VECTOR('',#61360,10.);
#9017=VECTOR('',#61363,10.);
#9018=VECTOR('',#61366,10.);
#9019=VECTOR('',#61369,10.);
#9020=VECTOR('',#61372,10.);
#9021=VECTOR('',#61375,10.);
#9022=VECTOR('',#61378,10.);
#9023=VECTOR('',#61381,10.);
#9024=VECTOR('',#61384,10.);
#9025=VECTOR('',#61387,10.);
#9026=VECTOR('',#61390,10.);
#9027=VECTOR('',#61395,10.);
#9028=VECTOR('',#61396,10.);
#9029=VECTOR('',#61401,10.);
#9030=VECTOR('',#61406,10.);
#9031=VECTOR('',#61411,10.);
#9032=VECTOR('',#61416,10.);
#9033=VECTOR('',#61421,10.);
#9034=VECTOR('',#61424,10.);
#9035=VECTOR('',#61425,10.);
#9036=VECTOR('',#61430,10.);
#9037=VECTOR('',#61435,10.);
#9038=VECTOR('',#61440,10.);
#9039=VECTOR('',#61445,10.);
#9040=VECTOR('',#61450,10.);
#9041=VECTOR('',#61453,10.);
#9042=VECTOR('',#61462,10.);
#9043=VECTOR('',#61473,10.);
#9044=VECTOR('',#61484,10.);
#9045=VECTOR('',#61487,10.);
#9046=VECTOR('',#61490,10.);
#9047=VECTOR('',#61493,10.);
#9048=VECTOR('',#61496,10.);
#9049=VECTOR('',#61499,10.);
#9050=VECTOR('',#61502,10.);
#9051=VECTOR('',#61505,10.);
#9052=VECTOR('',#61508,10.);
#9053=VECTOR('',#61511,10.);
#9054=VECTOR('',#61514,10.);
#9055=VECTOR('',#61517,10.);
#9056=VECTOR('',#61520,10.);
#9057=VECTOR('',#61523,10.);
#9058=VECTOR('',#61528,10.);
#9059=VECTOR('',#61529,10.);
#9060=VECTOR('',#61534,10.);
#9061=VECTOR('',#61539,10.);
#9062=VECTOR('',#61544,10.);
#9063=VECTOR('',#61549,10.);
#9064=VECTOR('',#61554,10.);
#9065=VECTOR('',#61557,10.);
#9066=VECTOR('',#61558,10.);
#9067=VECTOR('',#61563,10.);
#9068=VECTOR('',#61568,10.);
#9069=VECTOR('',#61573,10.);
#9070=VECTOR('',#61578,10.);
#9071=VECTOR('',#61583,10.);
#9072=VECTOR('',#61586,10.);
#9073=VECTOR('',#61595,10.);
#9074=VECTOR('',#61606,10.);
#9075=VECTOR('',#61617,10.);
#9076=VECTOR('',#61620,10.);
#9077=VECTOR('',#61623,10.);
#9078=VECTOR('',#61626,10.);
#9079=VECTOR('',#61629,10.);
#9080=VECTOR('',#61632,10.);
#9081=VECTOR('',#61635,10.);
#9082=VECTOR('',#61638,10.);
#9083=VECTOR('',#61641,10.);
#9084=VECTOR('',#61644,10.);
#9085=VECTOR('',#61647,10.);
#9086=VECTOR('',#61650,10.);
#9087=VECTOR('',#61653,10.);
#9088=VECTOR('',#61656,10.);
#9089=VECTOR('',#61661,10.);
#9090=VECTOR('',#61662,10.);
#9091=VECTOR('',#61667,10.);
#9092=VECTOR('',#61672,10.);
#9093=VECTOR('',#61677,10.);
#9094=VECTOR('',#61682,10.);
#9095=VECTOR('',#61687,10.);
#9096=VECTOR('',#61690,10.);
#9097=VECTOR('',#61691,10.);
#9098=VECTOR('',#61696,10.);
#9099=VECTOR('',#61701,10.);
#9100=VECTOR('',#61706,10.);
#9101=VECTOR('',#61711,10.);
#9102=VECTOR('',#61716,10.);
#9103=VECTOR('',#61719,10.);
#9104=VECTOR('',#61728,10.);
#9105=VECTOR('',#61739,10.);
#9106=VECTOR('',#61750,10.);
#9107=VECTOR('',#61753,10.);
#9108=VECTOR('',#61756,10.);
#9109=VECTOR('',#61759,10.);
#9110=VECTOR('',#61762,10.);
#9111=VECTOR('',#61765,10.);
#9112=VECTOR('',#61768,10.);
#9113=VECTOR('',#61771,10.);
#9114=VECTOR('',#61774,10.);
#9115=VECTOR('',#61777,10.);
#9116=VECTOR('',#61780,10.);
#9117=VECTOR('',#61783,10.);
#9118=VECTOR('',#61786,10.);
#9119=VECTOR('',#61789,10.);
#9120=VECTOR('',#61794,10.);
#9121=VECTOR('',#61795,10.);
#9122=VECTOR('',#61800,10.);
#9123=VECTOR('',#61805,10.);
#9124=VECTOR('',#61810,10.);
#9125=VECTOR('',#61815,10.);
#9126=VECTOR('',#61820,10.);
#9127=VECTOR('',#61823,10.);
#9128=VECTOR('',#61824,10.);
#9129=VECTOR('',#61829,10.);
#9130=VECTOR('',#61834,10.);
#9131=VECTOR('',#61839,10.);
#9132=VECTOR('',#61844,10.);
#9133=VECTOR('',#61849,10.);
#9134=VECTOR('',#61852,10.);
#9135=VECTOR('',#61861,10.);
#9136=VECTOR('',#61872,10.);
#9137=VECTOR('',#61883,10.);
#9138=VECTOR('',#61886,10.);
#9139=VECTOR('',#61889,10.);
#9140=VECTOR('',#61892,10.);
#9141=VECTOR('',#61895,10.);
#9142=VECTOR('',#61898,10.);
#9143=VECTOR('',#61901,10.);
#9144=VECTOR('',#61904,10.);
#9145=VECTOR('',#61907,10.);
#9146=VECTOR('',#61910,10.);
#9147=VECTOR('',#61913,10.);
#9148=VECTOR('',#61916,10.);
#9149=VECTOR('',#61919,10.);
#9150=VECTOR('',#61922,10.);
#9151=VECTOR('',#61927,10.);
#9152=VECTOR('',#61928,10.);
#9153=VECTOR('',#61933,10.);
#9154=VECTOR('',#61938,10.);
#9155=VECTOR('',#61943,10.);
#9156=VECTOR('',#61948,10.);
#9157=VECTOR('',#61953,10.);
#9158=VECTOR('',#61956,10.);
#9159=VECTOR('',#61957,10.);
#9160=VECTOR('',#61962,10.);
#9161=VECTOR('',#61967,10.);
#9162=VECTOR('',#61972,10.);
#9163=VECTOR('',#61977,10.);
#9164=VECTOR('',#61982,10.);
#9165=VECTOR('',#61985,10.);
#9166=VECTOR('',#61994,10.);
#9167=VECTOR('',#62005,10.);
#9168=VECTOR('',#62016,10.);
#9169=VECTOR('',#62019,10.);
#9170=VECTOR('',#62022,10.);
#9171=VECTOR('',#62025,10.);
#9172=VECTOR('',#62028,10.);
#9173=VECTOR('',#62031,10.);
#9174=VECTOR('',#62034,10.);
#9175=VECTOR('',#62037,10.);
#9176=VECTOR('',#62040,10.);
#9177=VECTOR('',#62043,10.);
#9178=VECTOR('',#62046,10.);
#9179=VECTOR('',#62049,10.);
#9180=VECTOR('',#62052,10.);
#9181=VECTOR('',#62055,10.);
#9182=VECTOR('',#62060,10.);
#9183=VECTOR('',#62061,10.);
#9184=VECTOR('',#62066,10.);
#9185=VECTOR('',#62071,10.);
#9186=VECTOR('',#62076,10.);
#9187=VECTOR('',#62081,10.);
#9188=VECTOR('',#62086,10.);
#9189=VECTOR('',#62089,10.);
#9190=VECTOR('',#62090,10.);
#9191=VECTOR('',#62095,10.);
#9192=VECTOR('',#62100,10.);
#9193=VECTOR('',#62105,10.);
#9194=VECTOR('',#62110,10.);
#9195=VECTOR('',#62115,10.);
#9196=VECTOR('',#62118,10.);
#9197=VECTOR('',#62127,10.);
#9198=VECTOR('',#62138,10.);
#9199=VECTOR('',#62149,10.);
#9200=VECTOR('',#62152,10.);
#9201=VECTOR('',#62155,10.);
#9202=VECTOR('',#62158,10.);
#9203=VECTOR('',#62161,10.);
#9204=VECTOR('',#62164,10.);
#9205=VECTOR('',#62167,10.);
#9206=VECTOR('',#62170,10.);
#9207=VECTOR('',#62173,10.);
#9208=VECTOR('',#62176,10.);
#9209=VECTOR('',#62179,10.);
#9210=VECTOR('',#62182,10.);
#9211=VECTOR('',#62185,10.);
#9212=VECTOR('',#62188,10.);
#9213=VECTOR('',#62193,10.);
#9214=VECTOR('',#62194,10.);
#9215=VECTOR('',#62199,10.);
#9216=VECTOR('',#62204,10.);
#9217=VECTOR('',#62209,10.);
#9218=VECTOR('',#62214,10.);
#9219=VECTOR('',#62219,10.);
#9220=VECTOR('',#62222,10.);
#9221=VECTOR('',#62223,10.);
#9222=VECTOR('',#62228,10.);
#9223=VECTOR('',#62233,10.);
#9224=VECTOR('',#62238,10.);
#9225=VECTOR('',#62243,10.);
#9226=VECTOR('',#62248,10.);
#9227=VECTOR('',#62251,10.);
#9228=VECTOR('',#62260,10.);
#9229=VECTOR('',#62271,10.);
#9230=VECTOR('',#62282,10.);
#9231=VECTOR('',#62285,10.);
#9232=VECTOR('',#62288,10.);
#9233=VECTOR('',#62291,10.);
#9234=VECTOR('',#62294,10.);
#9235=VECTOR('',#62297,10.);
#9236=VECTOR('',#62300,10.);
#9237=VECTOR('',#62303,10.);
#9238=VECTOR('',#62306,10.);
#9239=VECTOR('',#62309,10.);
#9240=VECTOR('',#62312,10.);
#9241=VECTOR('',#62315,10.);
#9242=VECTOR('',#62318,10.);
#9243=VECTOR('',#62321,10.);
#9244=VECTOR('',#62326,10.);
#9245=VECTOR('',#62327,10.);
#9246=VECTOR('',#62332,10.);
#9247=VECTOR('',#62337,10.);
#9248=VECTOR('',#62342,10.);
#9249=VECTOR('',#62347,10.);
#9250=VECTOR('',#62352,10.);
#9251=VECTOR('',#62355,10.);
#9252=VECTOR('',#62356,10.);
#9253=VECTOR('',#62361,10.);
#9254=VECTOR('',#62366,10.);
#9255=VECTOR('',#62371,10.);
#9256=VECTOR('',#62376,10.);
#9257=VECTOR('',#62381,10.);
#9258=VECTOR('',#62384,10.);
#9259=VECTOR('',#62393,10.);
#9260=VECTOR('',#62404,10.);
#9261=VECTOR('',#62415,10.);
#9262=VECTOR('',#62418,10.);
#9263=VECTOR('',#62421,10.);
#9264=VECTOR('',#62424,10.);
#9265=VECTOR('',#62427,10.);
#9266=VECTOR('',#62430,10.);
#9267=VECTOR('',#62433,10.);
#9268=VECTOR('',#62436,10.);
#9269=VECTOR('',#62439,10.);
#9270=VECTOR('',#62442,10.);
#9271=VECTOR('',#62445,10.);
#9272=VECTOR('',#62448,10.);
#9273=VECTOR('',#62451,10.);
#9274=VECTOR('',#62454,10.);
#9275=VECTOR('',#62459,10.);
#9276=VECTOR('',#62460,10.);
#9277=VECTOR('',#62465,10.);
#9278=VECTOR('',#62470,10.);
#9279=VECTOR('',#62475,10.);
#9280=VECTOR('',#62480,10.);
#9281=VECTOR('',#62485,10.);
#9282=VECTOR('',#62488,10.);
#9283=VECTOR('',#62489,10.);
#9284=VECTOR('',#62494,10.);
#9285=VECTOR('',#62499,10.);
#9286=VECTOR('',#62504,10.);
#9287=VECTOR('',#62509,10.);
#9288=VECTOR('',#62514,10.);
#9289=VECTOR('',#62517,10.);
#9290=VECTOR('',#62526,10.);
#9291=VECTOR('',#62537,10.);
#9292=VECTOR('',#62548,10.);
#9293=VECTOR('',#62551,10.);
#9294=VECTOR('',#62554,10.);
#9295=VECTOR('',#62557,10.);
#9296=VECTOR('',#62560,10.);
#9297=VECTOR('',#62563,10.);
#9298=VECTOR('',#62566,10.);
#9299=VECTOR('',#62569,10.);
#9300=VECTOR('',#62572,10.);
#9301=VECTOR('',#62575,10.);
#9302=VECTOR('',#62578,10.);
#9303=VECTOR('',#62581,10.);
#9304=VECTOR('',#62584,10.);
#9305=VECTOR('',#62587,10.);
#9306=VECTOR('',#62592,10.);
#9307=VECTOR('',#62593,10.);
#9308=VECTOR('',#62598,10.);
#9309=VECTOR('',#62603,10.);
#9310=VECTOR('',#62608,10.);
#9311=VECTOR('',#62613,10.);
#9312=VECTOR('',#62618,10.);
#9313=VECTOR('',#62621,10.);
#9314=VECTOR('',#62622,10.);
#9315=VECTOR('',#62627,10.);
#9316=VECTOR('',#62632,10.);
#9317=VECTOR('',#62637,10.);
#9318=VECTOR('',#62642,10.);
#9319=VECTOR('',#62647,10.);
#9320=VECTOR('',#62650,10.);
#9321=VECTOR('',#62659,10.);
#9322=VECTOR('',#62670,10.);
#9323=VECTOR('',#62681,10.);
#9324=VECTOR('',#62684,10.);
#9325=VECTOR('',#62685,10.);
#9326=VECTOR('',#62690,10.);
#9327=VECTOR('',#62695,10.);
#9328=VECTOR('',#62700,10.);
#9329=VECTOR('',#62705,10.);
#9330=VECTOR('',#62710,10.);
#9331=VECTOR('',#62713,10.);
#9332=VECTOR('',#62714,10.);
#9333=VECTOR('',#62719,10.);
#9334=VECTOR('',#62724,10.);
#9335=VECTOR('',#62729,10.);
#9336=VECTOR('',#62734,10.);
#9337=VECTOR('',#62739,10.);
#9338=VECTOR('',#62742,10.);
#9339=VECTOR('',#62743,10.);
#9340=VECTOR('',#62750,10.);
#9341=VECTOR('',#62753,10.);
#9342=VECTOR('',#62756,10.);
#9343=VECTOR('',#62759,10.);
#9344=VECTOR('',#62762,10.);
#9345=VECTOR('',#62765,10.);
#9346=VECTOR('',#62768,10.);
#9347=VECTOR('',#62771,10.);
#9348=VECTOR('',#62774,10.);
#9349=VECTOR('',#62777,10.);
#9350=VECTOR('',#62780,10.);
#9351=VECTOR('',#62783,10.);
#9352=VECTOR('',#62786,10.);
#9353=VECTOR('',#62793,42.6);
#9354=VECTOR('',#62800,47.3660700849456);
#9355=VECTOR('',#62807,49.25);
#9356=VECTOR('',#62824,51.);
#9357=VECTOR('',#62839,46.5);
#9358=VECTOR('',#62868,50.1);
#9359=VECTOR('',#62873,50.5);
#9360=VECTOR('',#62876,50.25);
#9361=VECTOR('',#62881,50.4);
#9362=VECTOR('',#62884,50.7);
#9363=VECTOR('',#62889,10.);
#9364=VECTOR('',#62890,10.);
#9365=VECTOR('',#62891,10.);
#9366=VECTOR('',#62892,10.);
#9367=VECTOR('',#62895,10.);
#9368=VECTOR('',#62896,10.);
#9369=VECTOR('',#62897,10.);
#9370=VECTOR('',#62898,10.);
#9371=VECTOR('',#62901,10.);
#9372=VECTOR('',#62902,10.);
#9373=VECTOR('',#62907,10.);
#9374=VECTOR('',#62942,10.);
#9375=VECTOR('',#62943,10.);
#9376=VECTOR('',#62944,10.);
#9377=VECTOR('',#62947,10.);
#9378=VECTOR('',#62948,10.);
#9379=VECTOR('',#62949,10.);
#9380=VECTOR('',#63006,10.);
#9381=VECTOR('',#63007,10.);
#9382=VECTOR('',#63008,10.);
#9383=VECTOR('',#63011,10.);
#9384=VECTOR('',#63012,10.);
#9385=VECTOR('',#63013,10.);
#9386=VECTOR('',#63016,10.);
#9387=VECTOR('',#63073,10.);
#9388=VECTOR('',#63102,10.);
#9389=VECTOR('',#63103,10.);
#9390=VECTOR('',#63104,10.);
#9391=VECTOR('',#63107,10.);
#9392=VECTOR('',#63108,10.);
#9393=VECTOR('',#63109,10.);
#9394=VECTOR('',#63112,10.);
#9395=VECTOR('',#63115,10.);
#9396=VECTOR('',#63250,10.);
#9397=VECTOR('',#63251,10.);
#9398=VECTOR('',#63252,10.);
#9399=VECTOR('',#63253,10.);
#9400=VECTOR('',#63254,10.);
#9401=VECTOR('',#63255,10.);
#9402=VECTOR('',#63258,10.);
#9403=VECTOR('',#63261,10.);
#9404=VECTOR('',#63262,10.);
#9405=VECTOR('',#63263,10.);
#9406=VECTOR('',#63264,10.);
#9407=VECTOR('',#63265,10.);
#9408=VECTOR('',#63266,10.);
#9409=VECTOR('',#63269,10.);
#9410=VECTOR('',#63272,10.);
#9411=VECTOR('',#63273,10.);
#9412=VECTOR('',#63274,10.);
#9413=VECTOR('',#63275,10.);
#9414=VECTOR('',#63276,10.);
#9415=VECTOR('',#63277,10.);
#9416=VECTOR('',#63280,10.);
#9417=VECTOR('',#63283,10.);
#9418=VECTOR('',#63284,10.);
#9419=VECTOR('',#63285,10.);
#9420=VECTOR('',#63286,10.);
#9421=VECTOR('',#63287,10.);
#9422=VECTOR('',#63288,10.);
#9423=VECTOR('',#63291,10.);
#9424=VECTOR('',#63294,10.);
#9425=VECTOR('',#63295,10.);
#9426=VECTOR('',#63296,10.);
#9427=VECTOR('',#63297,10.);
#9428=VECTOR('',#63298,10.);
#9429=VECTOR('',#63299,10.);
#9430=VECTOR('',#63302,10.);
#9431=VECTOR('',#63305,10.);
#9432=VECTOR('',#63306,10.);
#9433=VECTOR('',#63307,10.);
#9434=VECTOR('',#63308,10.);
#9435=VECTOR('',#63309,10.);
#9436=VECTOR('',#63310,10.);
#9437=VECTOR('',#63313,10.);
#9438=VECTOR('',#63316,10.);
#9439=VECTOR('',#63317,10.);
#9440=VECTOR('',#63318,10.);
#9441=VECTOR('',#63319,10.);
#9442=VECTOR('',#63320,10.);
#9443=VECTOR('',#63321,10.);
#9444=VECTOR('',#63324,10.);
#9445=VECTOR('',#63327,10.);
#9446=VECTOR('',#63328,10.);
#9447=VECTOR('',#63329,10.);
#9448=VECTOR('',#63330,10.);
#9449=VECTOR('',#63331,10.);
#9450=VECTOR('',#63332,10.);
#9451=VECTOR('',#63335,10.);
#9452=VECTOR('',#63338,10.);
#9453=VECTOR('',#63339,10.);
#9454=VECTOR('',#63340,10.);
#9455=VECTOR('',#63341,10.);
#9456=VECTOR('',#63342,10.);
#9457=VECTOR('',#63343,10.);
#9458=VECTOR('',#63346,10.);
#9459=VECTOR('',#63349,10.);
#9460=VECTOR('',#63350,10.);
#9461=VECTOR('',#63351,10.);
#9462=VECTOR('',#63352,10.);
#9463=VECTOR('',#63353,10.);
#9464=VECTOR('',#63354,10.);
#9465=VECTOR('',#63357,10.);
#9466=VECTOR('',#63360,10.);
#9467=VECTOR('',#63361,10.);
#9468=VECTOR('',#63362,10.);
#9469=VECTOR('',#63363,10.);
#9470=VECTOR('',#63364,10.);
#9471=VECTOR('',#63365,10.);
#9472=VECTOR('',#63368,10.);
#9473=VECTOR('',#63371,10.);
#9474=VECTOR('',#63372,10.);
#9475=VECTOR('',#63373,10.);
#9476=VECTOR('',#63374,10.);
#9477=VECTOR('',#63375,10.);
#9478=VECTOR('',#63376,10.);
#9479=VECTOR('',#63379,10.);
#9480=VECTOR('',#63382,10.);
#9481=VECTOR('',#63383,10.);
#9482=VECTOR('',#63384,10.);
#9483=VECTOR('',#63385,10.);
#9484=VECTOR('',#63386,10.);
#9485=VECTOR('',#63387,10.);
#9486=VECTOR('',#63390,10.);
#9487=VECTOR('',#63393,10.);
#9488=VECTOR('',#63394,10.);
#9489=VECTOR('',#63395,10.);
#9490=VECTOR('',#63396,10.);
#9491=VECTOR('',#63397,10.);
#9492=VECTOR('',#63398,10.);
#9493=VECTOR('',#63401,10.);
#9494=VECTOR('',#63404,10.);
#9495=VECTOR('',#63405,10.);
#9496=VECTOR('',#63406,10.);
#9497=VECTOR('',#63407,10.);
#9498=VECTOR('',#63408,10.);
#9499=VECTOR('',#63409,10.);
#9500=VECTOR('',#63412,10.);
#9501=VECTOR('',#63415,10.);
#9502=VECTOR('',#63416,10.);
#9503=VECTOR('',#63417,10.);
#9504=VECTOR('',#63418,10.);
#9505=VECTOR('',#63419,10.);
#9506=VECTOR('',#63420,10.);
#9507=VECTOR('',#63423,10.);
#9508=VECTOR('',#63426,10.);
#9509=VECTOR('',#63427,10.);
#9510=VECTOR('',#63428,10.);
#9511=VECTOR('',#63429,10.);
#9512=VECTOR('',#63430,10.);
#9513=VECTOR('',#63431,10.);
#9514=VECTOR('',#63434,10.);
#9515=VECTOR('',#63437,10.);
#9516=VECTOR('',#63438,10.);
#9517=VECTOR('',#63439,10.);
#9518=VECTOR('',#63440,10.);
#9519=VECTOR('',#63441,10.);
#9520=VECTOR('',#63442,10.);
#9521=VECTOR('',#63445,10.);
#9522=VECTOR('',#63448,10.);
#9523=VECTOR('',#63449,10.);
#9524=VECTOR('',#63450,10.);
#9525=VECTOR('',#63451,10.);
#9526=VECTOR('',#63452,10.);
#9527=VECTOR('',#63453,10.);
#9528=VECTOR('',#63456,10.);
#9529=VECTOR('',#63459,10.);
#9530=VECTOR('',#63460,10.);
#9531=VECTOR('',#63461,10.);
#9532=VECTOR('',#63462,10.);
#9533=VECTOR('',#63463,10.);
#9534=VECTOR('',#63464,10.);
#9535=VECTOR('',#63467,10.);
#9536=VECTOR('',#63470,10.);
#9537=VECTOR('',#63471,10.);
#9538=VECTOR('',#63472,10.);
#9539=VECTOR('',#63473,10.);
#9540=VECTOR('',#63474,10.);
#9541=VECTOR('',#63475,10.);
#9542=VECTOR('',#63478,10.);
#9543=VECTOR('',#63481,10.);
#9544=VECTOR('',#63482,10.);
#9545=VECTOR('',#63483,10.);
#9546=VECTOR('',#63484,10.);
#9547=VECTOR('',#63485,10.);
#9548=VECTOR('',#63486,10.);
#9549=VECTOR('',#63489,10.);
#9550=VECTOR('',#63492,10.);
#9551=VECTOR('',#63493,10.);
#9552=VECTOR('',#63494,10.);
#9553=VECTOR('',#63495,10.);
#9554=VECTOR('',#63496,10.);
#9555=VECTOR('',#63497,10.);
#9556=VECTOR('',#63500,10.);
#9557=VECTOR('',#63503,10.);
#9558=VECTOR('',#63504,10.);
#9559=VECTOR('',#63505,10.);
#9560=VECTOR('',#63506,10.);
#9561=VECTOR('',#63507,10.);
#9562=VECTOR('',#63508,10.);
#9563=VECTOR('',#63511,10.);
#9564=VECTOR('',#63514,10.);
#9565=VECTOR('',#63515,10.);
#9566=VECTOR('',#63516,10.);
#9567=VECTOR('',#63517,10.);
#9568=VECTOR('',#63518,10.);
#9569=VECTOR('',#63519,10.);
#9570=VECTOR('',#63522,10.);
#9571=VECTOR('',#63525,10.);
#9572=VECTOR('',#63526,10.);
#9573=VECTOR('',#63527,10.);
#9574=VECTOR('',#63528,10.);
#9575=VECTOR('',#63529,10.);
#9576=VECTOR('',#63530,10.);
#9577=VECTOR('',#63533,10.);
#9578=VECTOR('',#63536,10.);
#9579=VECTOR('',#63537,10.);
#9580=VECTOR('',#63538,10.);
#9581=VECTOR('',#63539,10.);
#9582=VECTOR('',#63540,10.);
#9583=VECTOR('',#63541,10.);
#9584=VECTOR('',#63544,10.);
#9585=VECTOR('',#63547,10.);
#9586=VECTOR('',#63548,10.);
#9587=VECTOR('',#63549,10.);
#9588=VECTOR('',#63550,10.);
#9589=VECTOR('',#63551,10.);
#9590=VECTOR('',#63552,10.);
#9591=VECTOR('',#63555,10.);
#9592=VECTOR('',#63558,10.);
#9593=VECTOR('',#63559,10.);
#9594=VECTOR('',#63560,10.);
#9595=VECTOR('',#63561,10.);
#9596=VECTOR('',#63562,10.);
#9597=VECTOR('',#63563,10.);
#9598=VECTOR('',#63566,10.);
#9599=VECTOR('',#63569,10.);
#9600=VECTOR('',#63570,10.);
#9601=VECTOR('',#63571,10.);
#9602=VECTOR('',#63572,10.);
#9603=VECTOR('',#63573,10.);
#9604=VECTOR('',#63574,10.);
#9605=VECTOR('',#63577,10.);
#9606=VECTOR('',#63580,10.);
#9607=VECTOR('',#63581,10.);
#9608=VECTOR('',#63582,10.);
#9609=VECTOR('',#63583,10.);
#9610=VECTOR('',#63584,10.);
#9611=VECTOR('',#63585,10.);
#9612=VECTOR('',#63588,10.);
#9613=VECTOR('',#63591,10.);
#9614=VECTOR('',#63592,10.);
#9615=VECTOR('',#63593,10.);
#9616=VECTOR('',#63594,10.);
#9617=VECTOR('',#63595,10.);
#9618=VECTOR('',#63596,10.);
#9619=VECTOR('',#63599,10.);
#9620=VECTOR('',#63602,10.);
#9621=VECTOR('',#63603,10.);
#9622=VECTOR('',#63604,10.);
#9623=VECTOR('',#63605,10.);
#9624=VECTOR('',#63606,10.);
#9625=VECTOR('',#63607,10.);
#9626=VECTOR('',#63610,10.);
#9627=VECTOR('',#63745,10.);
#9628=VECTOR('',#63746,10.);
#9629=VECTOR('',#63747,10.);
#9630=VECTOR('',#63748,10.);
#9631=VECTOR('',#63749,10.);
#9632=VECTOR('',#63752,10.);
#9633=VECTOR('',#63753,10.);
#9634=VECTOR('',#63754,10.);
#9635=VECTOR('',#63755,10.);
#9636=VECTOR('',#63756,10.);
#9637=VECTOR('',#63759,10.);
#9638=VECTOR('',#63760,10.);
#9639=VECTOR('',#63761,10.);
#9640=VECTOR('',#63762,10.);
#9641=VECTOR('',#63763,10.);
#9642=VECTOR('',#63766,10.);
#9643=VECTOR('',#63767,10.);
#9644=VECTOR('',#63768,10.);
#9645=VECTOR('',#63769,10.);
#9646=VECTOR('',#63770,10.);
#9647=VECTOR('',#63773,10.);
#9648=VECTOR('',#63774,10.);
#9649=VECTOR('',#63775,10.);
#9650=VECTOR('',#63776,10.);
#9651=VECTOR('',#63777,10.);
#9652=VECTOR('',#63780,10.);
#9653=VECTOR('',#63781,10.);
#9654=VECTOR('',#63782,10.);
#9655=VECTOR('',#63783,10.);
#9656=VECTOR('',#63784,10.);
#9657=VECTOR('',#63787,10.);
#9658=VECTOR('',#63788,10.);
#9659=VECTOR('',#63789,10.);
#9660=VECTOR('',#63790,10.);
#9661=VECTOR('',#63791,10.);
#9662=VECTOR('',#63794,10.);
#9663=VECTOR('',#63795,10.);
#9664=VECTOR('',#63796,10.);
#9665=VECTOR('',#63797,10.);
#9666=VECTOR('',#63798,10.);
#9667=VECTOR('',#63801,10.);
#9668=VECTOR('',#63802,10.);
#9669=VECTOR('',#63803,10.);
#9670=VECTOR('',#63804,10.);
#9671=VECTOR('',#63805,10.);
#9672=VECTOR('',#63808,10.);
#9673=VECTOR('',#63809,10.);
#9674=VECTOR('',#63810,10.);
#9675=VECTOR('',#63811,10.);
#9676=VECTOR('',#63812,10.);
#9677=VECTOR('',#63815,10.);
#9678=VECTOR('',#63816,10.);
#9679=VECTOR('',#63817,10.);
#9680=VECTOR('',#63818,10.);
#9681=VECTOR('',#63821,10.);
#9682=VECTOR('',#63822,10.);
#9683=VECTOR('',#63823,10.);
#9684=VECTOR('',#63824,10.);
#9685=VECTOR('',#63825,10.);
#9686=VECTOR('',#63828,10.);
#9687=VECTOR('',#63829,10.);
#9688=VECTOR('',#63830,10.);
#9689=VECTOR('',#63831,10.);
#9690=VECTOR('',#63832,10.);
#9691=VECTOR('',#63835,10.);
#9692=VECTOR('',#63836,10.);
#9693=VECTOR('',#63837,10.);
#9694=VECTOR('',#63838,10.);
#9695=VECTOR('',#63839,10.);
#9696=VECTOR('',#63842,10.);
#9697=VECTOR('',#63843,10.);
#9698=VECTOR('',#63844,10.);
#9699=VECTOR('',#63845,10.);
#9700=VECTOR('',#63846,10.);
#9701=VECTOR('',#63849,10.);
#9702=VECTOR('',#63850,10.);
#9703=VECTOR('',#63851,10.);
#9704=VECTOR('',#63852,10.);
#9705=VECTOR('',#63853,10.);
#9706=VECTOR('',#63856,10.);
#9707=VECTOR('',#63857,10.);
#9708=VECTOR('',#63858,10.);
#9709=VECTOR('',#63859,10.);
#9710=VECTOR('',#63860,10.);
#9711=VECTOR('',#63863,10.);
#9712=VECTOR('',#63864,10.);
#9713=VECTOR('',#63865,10.);
#9714=VECTOR('',#63866,10.);
#9715=VECTOR('',#63867,10.);
#9716=VECTOR('',#63870,10.);
#9717=VECTOR('',#63871,10.);
#9718=VECTOR('',#63872,10.);
#9719=VECTOR('',#63873,10.);
#9720=VECTOR('',#63874,10.);
#9721=VECTOR('',#63877,10.);
#9722=VECTOR('',#63878,10.);
#9723=VECTOR('',#63879,10.);
#9724=VECTOR('',#63880,10.);
#9725=VECTOR('',#63881,10.);
#9726=VECTOR('',#63884,10.);
#9727=VECTOR('',#63885,10.);
#9728=VECTOR('',#63886,10.);
#9729=VECTOR('',#63887,10.);
#9730=VECTOR('',#63888,10.);
#9731=VECTOR('',#63891,10.);
#9732=VECTOR('',#63892,10.);
#9733=VECTOR('',#63893,10.);
#9734=VECTOR('',#63894,10.);
#9735=VECTOR('',#63897,10.);
#9736=VECTOR('',#63898,10.);
#9737=VECTOR('',#63899,10.);
#9738=VECTOR('',#63900,10.);
#9739=VECTOR('',#63901,10.);
#9740=VECTOR('',#63904,10.);
#9741=VECTOR('',#63905,10.);
#9742=VECTOR('',#63906,10.);
#9743=VECTOR('',#63907,10.);
#9744=VECTOR('',#63908,10.);
#9745=VECTOR('',#63911,10.);
#9746=VECTOR('',#63912,10.);
#9747=VECTOR('',#63913,10.);
#9748=VECTOR('',#63914,10.);
#9749=VECTOR('',#63915,10.);
#9750=VECTOR('',#63918,10.);
#9751=VECTOR('',#63919,10.);
#9752=VECTOR('',#63920,10.);
#9753=VECTOR('',#63921,10.);
#9754=VECTOR('',#63922,10.);
#9755=VECTOR('',#63925,10.);
#9756=VECTOR('',#63926,10.);
#9757=VECTOR('',#63927,10.);
#9758=VECTOR('',#63928,10.);
#9759=VECTOR('',#63929,10.);
#9760=VECTOR('',#63932,10.);
#9761=VECTOR('',#63933,10.);
#9762=VECTOR('',#63934,10.);
#9763=VECTOR('',#63935,10.);
#9764=VECTOR('',#63936,10.);
#9765=VECTOR('',#63939,10.);
#9766=VECTOR('',#63940,10.);
#9767=VECTOR('',#63941,10.);
#9768=VECTOR('',#63942,10.);
#9769=VECTOR('',#63943,10.);
#9770=VECTOR('',#63946,10.);
#9771=VECTOR('',#63947,10.);
#9772=VECTOR('',#63948,10.);
#9773=VECTOR('',#63949,10.);
#9774=VECTOR('',#63950,10.);
#9775=VECTOR('',#63953,10.);
#9776=VECTOR('',#63954,10.);
#9777=VECTOR('',#63955,10.);
#9778=VECTOR('',#63956,10.);
#9779=VECTOR('',#63957,10.);
#9780=VECTOR('',#63960,10.);
#9781=VECTOR('',#63961,10.);
#9782=VECTOR('',#63962,10.);
#9783=VECTOR('',#63963,10.);
#9784=VECTOR('',#63964,10.);
#9785=VECTOR('',#63967,10.);
#9786=VECTOR('',#63968,10.);
#9787=VECTOR('',#63969,10.);
#9788=VECTOR('',#63970,10.);
#9789=VECTOR('',#63973,10.);
#9790=VECTOR('',#63976,10.);
#9791=VECTOR('',#63987,10.);
#9792=VECTOR('',#63990,10.);
#9793=VECTOR('',#63999,10.);
#9794=VECTOR('',#64002,10.);
#9795=VECTOR('',#64011,10.);
#9796=VECTOR('',#64014,10.);
#9797=VECTOR('',#64023,10.);
#9798=VECTOR('',#64026,10.);
#9799=VECTOR('',#64035,10.);
#9800=VECTOR('',#64038,10.);
#9801=VECTOR('',#64047,10.);
#9802=VECTOR('',#64050,10.);
#9803=VECTOR('',#64059,10.);
#9804=VECTOR('',#64062,10.);
#9805=VECTOR('',#64071,10.);
#9806=VECTOR('',#64074,10.);
#9807=VECTOR('',#64083,10.);
#9808=VECTOR('',#64086,10.);
#9809=VECTOR('',#64095,10.);
#9810=VECTOR('',#64098,10.);
#9811=VECTOR('',#64107,10.);
#9812=VECTOR('',#64110,10.);
#9813=VECTOR('',#64119,10.);
#9814=VECTOR('',#64122,10.);
#9815=VECTOR('',#64131,10.);
#9816=VECTOR('',#64134,10.);
#9817=VECTOR('',#64143,10.);
#9818=VECTOR('',#64146,10.);
#9819=VECTOR('',#64155,10.);
#9820=VECTOR('',#64158,10.);
#9821=VECTOR('',#64167,10.);
#9822=VECTOR('',#64170,10.);
#9823=VECTOR('',#64179,10.);
#9824=VECTOR('',#64182,10.);
#9825=VECTOR('',#64191,10.);
#9826=VECTOR('',#64194,10.);
#9827=VECTOR('',#64203,10.);
#9828=VECTOR('',#64206,10.);
#9829=VECTOR('',#64215,10.);
#9830=VECTOR('',#64218,10.);
#9831=VECTOR('',#64227,10.);
#9832=VECTOR('',#64230,10.);
#9833=VECTOR('',#64239,10.);
#9834=VECTOR('',#64242,10.);
#9835=VECTOR('',#64251,10.);
#9836=VECTOR('',#64254,10.);
#9837=VECTOR('',#64263,10.);
#9838=VECTOR('',#64266,10.);
#9839=VECTOR('',#64275,10.);
#9840=VECTOR('',#64278,10.);
#9841=VECTOR('',#64287,10.);
#9842=VECTOR('',#64290,10.);
#9843=VECTOR('',#64299,10.);
#9844=VECTOR('',#64302,10.);
#9845=VECTOR('',#64311,10.);
#9846=VECTOR('',#64314,10.);
#9847=VECTOR('',#64323,10.);
#9848=VECTOR('',#64326,10.);
#9849=VECTOR('',#64335,10.);
#9850=VECTOR('',#64338,10.);
#9851=VECTOR('',#64347,10.);
#9852=VECTOR('',#64350,10.);
#9853=VECTOR('',#64359,10.);
#9854=VECTOR('',#64362,10.);
#9855=VECTOR('',#64385,34.);
#9856=VECTOR('',#64402,34.);
#9857=VECTOR('',#64415,24.);
#9858=VECTOR('',#64426,24.);
#9859=VECTOR('',#64433,15.01);
#9860=VECTOR('',#64438,15.41);
#9861=VECTOR('',#64451,15.41);
#9862=VECTOR('',#64458,3.15);
#9863=VECTOR('',#64481,3.);
#9864=VECTOR('',#64484,3.15);
#9865=VECTOR('',#64491,3.);
#9866=VECTOR('',#64496,3.3);
#9867=VECTOR('',#64503,3.3);
#9868=VECTOR('',#64510,3.3);
#9869=VECTOR('',#64517,3.3);
#9870=VECTOR('',#64524,5.5);
#9871=VECTOR('',#64531,5.5);
#9872=VECTOR('',#64538,5.5);
#9873=VECTOR('',#64545,5.5);
#9874=VECTOR('',#64550,2.525);
#9875=VECTOR('',#64555,5.05);
#9876=VECTOR('',#64560,5.35);
#9877=VECTOR('',#64575,20.);
#9878=VECTOR('',#64584,19.75);
#9879=VECTOR('',#64589,20.);
#9880=VECTOR('',#64598,47.5);
#9881=VECTOR('',#64603,48.);
#9882=VECTOR('',#64606,47.5);
#9883=VECTOR('',#64615,14.995);
#9884=VECTOR('',#64620,14.495);
#9885=VECTOR('',#64627,10.);
#9886=VECTOR('',#64628,10.);
#9887=VECTOR('',#64629,10.);
#9888=VECTOR('',#64630,10.);
#9889=VECTOR('',#64633,10.);
#9890=VECTOR('',#64634,10.);
#9891=VECTOR('',#64635,10.);
#9892=VECTOR('',#64638,10.);
#9893=VECTOR('',#64639,10.);
#9894=VECTOR('',#64640,10.);
#9895=VECTOR('',#64643,10.);
#9896=VECTOR('',#64644,10.);
#9897=VECTOR('',#64645,10.);
#9898=VECTOR('',#64648,10.);
#9899=VECTOR('',#64649,10.);
#9900=VECTOR('',#64650,10.);
#9901=VECTOR('',#64653,10.);
#9902=VECTOR('',#64654,10.);
#9903=VECTOR('',#64655,10.);
#9904=VECTOR('',#64658,10.);
#9905=VECTOR('',#64659,10.);
#9906=VECTOR('',#64660,10.);
#9907=VECTOR('',#64663,10.);
#9908=VECTOR('',#64664,10.);
#9909=VECTOR('',#64665,10.);
#9910=VECTOR('',#64668,10.);
#9911=VECTOR('',#64669,10.);
#9912=VECTOR('',#64670,10.);
#9913=VECTOR('',#64673,10.);
#9914=VECTOR('',#64674,10.);
#9915=VECTOR('',#64675,10.);
#9916=VECTOR('',#64678,10.);
#9917=VECTOR('',#64679,10.);
#9918=VECTOR('',#64680,10.);
#9919=VECTOR('',#64683,10.);
#9920=VECTOR('',#64684,10.);
#9921=VECTOR('',#64689,10.);
#9922=VECTOR('',#64690,10.);
#9923=VECTOR('',#64691,10.);
#9924=VECTOR('',#64692,10.);
#9925=VECTOR('',#64695,10.);
#9926=VECTOR('',#64696,10.);
#9927=VECTOR('',#64697,10.);
#9928=VECTOR('',#64700,10.);
#9929=VECTOR('',#64701,10.);
#9930=VECTOR('',#64702,10.);
#9931=VECTOR('',#64705,10.);
#9932=VECTOR('',#64706,10.);
#9933=VECTOR('',#64709,10.);
#9934=VECTOR('',#64710,10.);
#9935=VECTOR('',#64711,10.);
#9936=VECTOR('',#64712,10.);
#9937=VECTOR('',#64713,10.);
#9938=VECTOR('',#64714,10.);
#9939=VECTOR('',#64715,10.);
#9940=VECTOR('',#64716,10.);
#9941=VECTOR('',#64717,10.);
#9942=VECTOR('',#64718,10.);
#9943=VECTOR('',#64719,10.);
#9944=VECTOR('',#64720,10.);
#9945=VECTOR('',#64721,10.);
#9946=VECTOR('',#64722,10.);
#9947=VECTOR('',#64725,10.);
#9948=VECTOR('',#64726,10.);
#9949=VECTOR('',#64727,10.);
#9950=VECTOR('',#64728,10.);
#9951=VECTOR('',#64729,10.);
#9952=VECTOR('',#64730,10.);
#9953=VECTOR('',#64731,10.);
#9954=VECTOR('',#64732,10.);
#9955=VECTOR('',#64733,10.);
#9956=VECTOR('',#64734,10.);
#9957=VECTOR('',#64735,10.);
#9958=VECTOR('',#64736,10.);
#9959=VECTOR('',#64737,10.);
#9960=VECTOR('',#64738,10.);
#9961=VECTOR('',#64739,10.);
#9962=VECTOR('',#64740,10.);
#9963=VECTOR('',#64741,10.);
#9964=VECTOR('',#64742,10.);
#9965=VECTOR('',#64743,10.);
#9966=VECTOR('',#64744,10.);
#9967=VECTOR('',#64745,10.);
#9968=VECTOR('',#64748,10.);
#9969=VECTOR('',#64749,10.);
#9970=VECTOR('',#64750,10.);
#9971=VECTOR('',#64751,10.);
#9972=VECTOR('',#64754,10.);
#9973=VECTOR('',#64755,10.);
#9974=VECTOR('',#64756,10.);
#9975=VECTOR('',#64757,10.);
#9976=VECTOR('',#64758,10.);
#9977=VECTOR('',#64759,10.);
#9978=VECTOR('',#64760,10.);
#9979=VECTOR('',#64761,10.);
#9980=VECTOR('',#64762,10.);
#9981=VECTOR('',#64765,10.);
#9982=VECTOR('',#64766,10.);
#9983=VECTOR('',#64767,10.);
#9984=VECTOR('',#64768,10.);
#9985=VECTOR('',#64769,10.);
#9986=VECTOR('',#64770,10.);
#9987=VECTOR('',#64771,10.);
#9988=VECTOR('',#64772,10.);
#9989=VECTOR('',#64773,10.);
#9990=VECTOR('',#64774,10.);
#9991=VECTOR('',#64775,10.);
#9992=VECTOR('',#64776,10.);
#9993=VECTOR('',#64777,10.);
#9994=VECTOR('',#64780,10.);
#9995=VECTOR('',#64781,10.);
#9996=VECTOR('',#64782,10.);
#9997=VECTOR('',#64783,10.);
#9998=VECTOR('',#64788,10.);
#9999=VECTOR('',#64789,10.);
#10000=VECTOR('',#64790,10.);
#10001=VECTOR('',#64791,10.);
#10002=VECTOR('',#64794,10.);
#10003=VECTOR('',#64795,10.);
#10004=VECTOR('',#64796,10.);
#10005=VECTOR('',#64799,10.);
#10006=VECTOR('',#64800,10.);
#10007=VECTOR('',#64801,10.);
#10008=VECTOR('',#64804,10.);
#10009=VECTOR('',#64805,10.);
#10010=VECTOR('',#64806,10.);
#10011=VECTOR('',#64809,10.);
#10012=VECTOR('',#64810,10.);
#10013=VECTOR('',#64811,10.);
#10014=VECTOR('',#64814,10.);
#10015=VECTOR('',#64815,10.);
#10016=VECTOR('',#64820,10.);
#10017=VECTOR('',#64821,10.);
#10018=VECTOR('',#64822,10.);
#10019=VECTOR('',#64823,10.);
#10020=VECTOR('',#64826,10.);
#10021=VECTOR('',#64827,10.);
#10022=VECTOR('',#64828,10.);
#10023=VECTOR('',#64831,10.);
#10024=VECTOR('',#64832,10.);
#10025=VECTOR('',#64833,10.);
#10026=VECTOR('',#64836,10.);
#10027=VECTOR('',#64837,10.);
#10028=VECTOR('',#64838,10.);
#10029=VECTOR('',#64841,10.);
#10030=VECTOR('',#64842,10.);
#10031=VECTOR('',#64843,10.);
#10032=VECTOR('',#64846,10.);
#10033=VECTOR('',#64847,10.);
#10034=VECTOR('',#64848,10.);
#10035=VECTOR('',#64851,10.);
#10036=VECTOR('',#64852,10.);
#10037=VECTOR('',#64853,10.);
#10038=VECTOR('',#64856,10.);
#10039=VECTOR('',#64857,10.);
#10040=VECTOR('',#64860,10.);
#10041=VECTOR('',#64861,10.);
#10042=VECTOR('',#64862,10.);
#10043=VECTOR('',#64863,10.);
#10044=VECTOR('',#64864,10.);
#10045=VECTOR('',#64867,10.);
#10046=VECTOR('',#64868,10.);
#10047=VECTOR('',#64869,10.);
#10048=VECTOR('',#64872,10.);
#10049=VECTOR('',#64873,10.);
#10050=VECTOR('',#64874,10.);
#10051=VECTOR('',#64877,10.);
#10052=VECTOR('',#64878,10.);
#10053=VECTOR('',#64879,10.);
#10054=VECTOR('',#64880,10.);
#10055=VECTOR('',#64881,10.);
#10056=VECTOR('',#64882,10.);
#10057=VECTOR('',#64883,10.);
#10058=VECTOR('',#64884,10.);
#10059=VECTOR('',#64885,10.);
#10060=VECTOR('',#64888,10.);
#10061=VECTOR('',#64889,10.);
#10062=VECTOR('',#64890,10.);
#10063=VECTOR('',#64893,10.);
#10064=VECTOR('',#64894,10.);
#10065=VECTOR('',#64895,10.);
#10066=VECTOR('',#64898,10.);
#10067=VECTOR('',#64899,10.);
#10068=VECTOR('',#64900,10.);
#10069=VECTOR('',#64905,10.);
#10070=VECTOR('',#64906,10.);
#10071=VECTOR('',#64907,10.);
#10072=VECTOR('',#64908,10.);
#10073=VECTOR('',#64909,10.);
#10074=VECTOR('',#64910,10.);
#10075=VECTOR('',#64911,10.);
#10076=VECTOR('',#64912,10.);
#10077=VECTOR('',#64915,10.);
#10078=VECTOR('',#64916,10.);
#10079=VECTOR('',#64917,10.);
#10080=VECTOR('',#64920,10.);
#10081=VECTOR('',#64921,10.);
#10082=VECTOR('',#64922,10.);
#10083=VECTOR('',#64925,10.);
#10084=VECTOR('',#64926,10.);
#10085=VECTOR('',#64927,10.);
#10086=VECTOR('',#64928,10.);
#10087=VECTOR('',#64929,10.);
#10088=VECTOR('',#64930,10.);
#10089=VECTOR('',#64931,10.);
#10090=VECTOR('',#64932,10.);
#10091=VECTOR('',#64933,10.);
#10092=VECTOR('',#64934,10.);
#10093=VECTOR('',#64937,10.);
#10094=VECTOR('',#64938,10.);
#10095=VECTOR('',#64939,10.);
#10096=VECTOR('',#64942,10.);
#10097=VECTOR('',#64943,10.);
#10098=VECTOR('',#64944,10.);
#10099=VECTOR('',#64947,10.);
#10100=VECTOR('',#64948,10.);
#10101=VECTOR('',#64949,10.);
#10102=VECTOR('',#64952,10.);
#10103=VECTOR('',#64953,10.);
#10104=VECTOR('',#64958,10.);
#10105=VECTOR('',#64959,10.);
#10106=VECTOR('',#64960,10.);
#10107=VECTOR('',#64961,10.);
#10108=VECTOR('',#64964,10.);
#10109=VECTOR('',#64965,10.);
#10110=VECTOR('',#64966,10.);
#10111=VECTOR('',#64969,10.);
#10112=VECTOR('',#64970,10.);
#10113=VECTOR('',#64971,10.);
#10114=VECTOR('',#64974,10.);
#10115=VECTOR('',#64975,10.);
#10116=VECTOR('',#64976,10.);
#10117=VECTOR('',#64979,10.);
#10118=VECTOR('',#64980,10.);
#10119=VECTOR('',#64981,10.);
#10120=VECTOR('',#64984,10.);
#10121=VECTOR('',#64985,10.);
#10122=VECTOR('',#64986,10.);
#10123=VECTOR('',#64989,10.);
#10124=VECTOR('',#64990,10.);
#10125=VECTOR('',#64991,10.);
#10126=VECTOR('',#64994,10.);
#10127=VECTOR('',#64995,10.);
#10128=VECTOR('',#64998,10.);
#10129=VECTOR('',#64999,10.);
#10130=VECTOR('',#65000,10.);
#10131=VECTOR('',#65003,10.);
#10132=VECTOR('',#65004,10.);
#10133=VECTOR('',#65005,10.);
#10134=VECTOR('',#65006,10.);
#10135=VECTOR('',#65007,10.);
#10136=VECTOR('',#65010,10.);
#10137=VECTOR('',#65011,10.);
#10138=VECTOR('',#65012,10.);
#10139=VECTOR('',#65015,10.);
#10140=VECTOR('',#65016,10.);
#10141=VECTOR('',#65017,10.);
#10142=VECTOR('',#65020,10.);
#10143=VECTOR('',#65021,10.);
#10144=VECTOR('',#65022,10.);
#10145=VECTOR('',#65025,10.);
#10146=VECTOR('',#65026,10.);
#10147=VECTOR('',#65029,10.);
#10148=VECTOR('',#65030,10.);
#10149=VECTOR('',#65031,10.);
#10150=VECTOR('',#65032,10.);
#10151=VECTOR('',#65033,10.);
#10152=VECTOR('',#65034,10.);
#10153=VECTOR('',#65035,10.);
#10154=VECTOR('',#65036,10.);
#10155=VECTOR('',#65037,10.);
#10156=VECTOR('',#65038,10.);
#10157=VECTOR('',#65039,10.);
#10158=VECTOR('',#65040,10.);
#10159=VECTOR('',#65043,10.);
#10160=VECTOR('',#65044,10.);
#10161=VECTOR('',#65045,10.);
#10162=VECTOR('',#65048,10.);
#10163=VECTOR('',#65049,10.);
#10164=VECTOR('',#65050,10.);
#10165=VECTOR('',#65051,10.);
#10166=VECTOR('',#65052,10.);
#10167=VECTOR('',#65055,10.);
#10168=VECTOR('',#65056,10.);
#10169=VECTOR('',#65057,10.);
#10170=VECTOR('',#65060,10.);
#10171=VECTOR('',#65061,10.);
#10172=VECTOR('',#65062,10.);
#10173=VECTOR('',#65065,10.);
#10174=VECTOR('',#65066,10.);
#10175=VECTOR('',#65067,10.);
#10176=VECTOR('',#65070,10.);
#10177=VECTOR('',#65071,10.);
#10178=VECTOR('',#65076,10.);
#10179=VECTOR('',#65077,10.);
#10180=VECTOR('',#65078,10.);
#10181=VECTOR('',#65079,10.);
#10182=VECTOR('',#65082,10.);
#10183=VECTOR('',#65083,10.);
#10184=VECTOR('',#65084,10.);
#10185=VECTOR('',#65087,10.);
#10186=VECTOR('',#65088,10.);
#10187=VECTOR('',#65089,10.);
#10188=VECTOR('',#65092,10.);
#10189=VECTOR('',#65093,10.);
#10190=VECTOR('',#65096,10.);
#10191=VECTOR('',#65097,10.);
#10192=VECTOR('',#65098,10.);
#10193=VECTOR('',#65099,10.);
#10194=VECTOR('',#65100,10.);
#10195=VECTOR('',#65101,10.);
#10196=VECTOR('',#65104,10.);
#10197=VECTOR('',#65105,10.);
#10198=VECTOR('',#65106,10.);
#10199=VECTOR('',#65109,10.);
#10200=VECTOR('',#65110,10.);
#10201=VECTOR('',#65111,10.);
#10202=VECTOR('',#65114,10.);
#10203=VECTOR('',#65115,10.);
#10204=VECTOR('',#65116,10.);
#10205=VECTOR('',#65119,10.);
#10206=VECTOR('',#65120,10.);
#10207=VECTOR('',#65121,10.);
#10208=VECTOR('',#65124,10.);
#10209=VECTOR('',#65125,10.);
#10210=VECTOR('',#65126,10.);
#10211=VECTOR('',#65129,10.);
#10212=VECTOR('',#65130,10.);
#10213=VECTOR('',#65131,10.);
#10214=VECTOR('',#65132,10.);
#10215=VECTOR('',#65133,10.);
#10216=VECTOR('',#65134,10.);
#10217=VECTOR('',#65135,10.);
#10218=VECTOR('',#65136,10.);
#10219=VECTOR('',#65137,10.);
#10220=VECTOR('',#65138,10.);
#10221=VECTOR('',#65139,10.);
#10222=VECTOR('',#65142,10.);
#10223=VECTOR('',#65143,10.);
#10224=VECTOR('',#65144,10.);
#10225=VECTOR('',#65145,10.);
#10226=VECTOR('',#65148,10.);
#10227=VECTOR('',#65149,10.);
#10228=VECTOR('',#65150,10.);
#10229=VECTOR('',#65151,10.);
#10230=VECTOR('',#65152,10.);
#10231=VECTOR('',#65153,10.);
#10232=VECTOR('',#65154,10.);
#10233=VECTOR('',#65155,10.);
#10234=VECTOR('',#65156,10.);
#10235=VECTOR('',#65157,10.);
#10236=VECTOR('',#65158,10.);
#10237=VECTOR('',#65161,10.);
#10238=VECTOR('',#65162,10.);
#10239=VECTOR('',#65163,10.);
#10240=VECTOR('',#65164,10.);
#10241=VECTOR('',#65165,10.);
#10242=VECTOR('',#65166,10.);
#10243=VECTOR('',#65167,10.);
#10244=VECTOR('',#65168,10.);
#10245=VECTOR('',#65169,10.);
#10246=VECTOR('',#65170,10.);
#10247=VECTOR('',#65171,10.);
#10248=VECTOR('',#65172,10.);
#10249=VECTOR('',#65175,10.);
#10250=VECTOR('',#65176,10.);
#10251=VECTOR('',#65177,10.);
#10252=VECTOR('',#65178,10.);
#10253=VECTOR('',#65179,10.);
#10254=VECTOR('',#65184,10.);
#10255=VECTOR('',#65185,10.);
#10256=VECTOR('',#65186,10.);
#10257=VECTOR('',#65187,10.);
#10258=VECTOR('',#65190,10.);
#10259=VECTOR('',#65191,10.);
#10260=VECTOR('',#65192,10.);
#10261=VECTOR('',#65195,10.);
#10262=VECTOR('',#65196,10.);
#10263=VECTOR('',#65197,10.);
#10264=VECTOR('',#65200,10.);
#10265=VECTOR('',#65201,10.);
#10266=VECTOR('',#65202,10.);
#10267=VECTOR('',#65205,10.);
#10268=VECTOR('',#65206,10.);
#10269=VECTOR('',#65207,10.);
#10270=VECTOR('',#65210,10.);
#10271=VECTOR('',#65211,10.);
#10272=VECTOR('',#65212,10.);
#10273=VECTOR('',#65215,10.);
#10274=VECTOR('',#65216,10.);
#10275=VECTOR('',#65217,10.);
#10276=VECTOR('',#65220,10.);
#10277=VECTOR('',#65221,10.);
#10278=VECTOR('',#65222,10.);
#10279=VECTOR('',#65225,10.);
#10280=VECTOR('',#65226,10.);
#10281=VECTOR('',#65227,10.);
#10282=VECTOR('',#65230,10.);
#10283=VECTOR('',#65231,10.);
#10284=VECTOR('',#65232,10.);
#10285=VECTOR('',#65235,10.);
#10286=VECTOR('',#65236,10.);
#10287=VECTOR('',#65237,10.);
#10288=VECTOR('',#65240,10.);
#10289=VECTOR('',#65241,10.);
#10290=VECTOR('',#65246,10.);
#10291=VECTOR('',#65247,10.);
#10292=VECTOR('',#65248,10.);
#10293=VECTOR('',#65249,10.);
#10294=VECTOR('',#65252,10.);
#10295=VECTOR('',#65253,10.);
#10296=VECTOR('',#65254,10.);
#10297=VECTOR('',#65257,10.);
#10298=VECTOR('',#65258,10.);
#10299=VECTOR('',#65259,10.);
#10300=VECTOR('',#65262,10.);
#10301=VECTOR('',#65263,10.);
#10302=VECTOR('',#65266,10.);
#10303=VECTOR('',#65267,10.);
#10304=VECTOR('',#65268,10.);
#10305=VECTOR('',#65269,10.);
#10306=VECTOR('',#65270,10.);
#10307=VECTOR('',#65271,10.);
#10308=VECTOR('',#65272,10.);
#10309=VECTOR('',#65273,10.);
#10310=VECTOR('',#65274,10.);
#10311=VECTOR('',#65275,10.);
#10312=VECTOR('',#65276,10.);
#10313=VECTOR('',#65281,10.);
#10314=VECTOR('',#65282,10.);
#10315=VECTOR('',#65283,10.);
#10316=VECTOR('',#65284,10.);
#10317=VECTOR('',#65287,10.);
#10318=VECTOR('',#65288,10.);
#10319=VECTOR('',#65289,10.);
#10320=VECTOR('',#65292,10.);
#10321=VECTOR('',#65293,10.);
#10322=VECTOR('',#65294,10.);
#10323=VECTOR('',#65297,10.);
#10324=VECTOR('',#65298,10.);
#10325=VECTOR('',#65299,10.);
#10326=VECTOR('',#65302,10.);
#10327=VECTOR('',#65303,10.);
#10328=VECTOR('',#65304,10.);
#10329=VECTOR('',#65307,10.);
#10330=VECTOR('',#65308,10.);
#10331=VECTOR('',#65309,10.);
#10332=VECTOR('',#65312,10.);
#10333=VECTOR('',#65313,10.);
#10334=VECTOR('',#65314,10.);
#10335=VECTOR('',#65317,10.);
#10336=VECTOR('',#65318,10.);
#10337=VECTOR('',#65319,10.);
#10338=VECTOR('',#65322,10.);
#10339=VECTOR('',#65323,10.);
#10340=VECTOR('',#65324,10.);
#10341=VECTOR('',#65327,10.);
#10342=VECTOR('',#65328,10.);
#10343=VECTOR('',#65329,10.);
#10344=VECTOR('',#65332,10.);
#10345=VECTOR('',#65333,10.);
#10346=VECTOR('',#65334,10.);
#10347=VECTOR('',#65337,10.);
#10348=VECTOR('',#65338,10.);
#10349=VECTOR('',#65343,10.);
#10350=VECTOR('',#65344,10.);
#10351=VECTOR('',#65345,10.);
#10352=VECTOR('',#65346,10.);
#10353=VECTOR('',#65349,10.);
#10354=VECTOR('',#65350,10.);
#10355=VECTOR('',#65351,10.);
#10356=VECTOR('',#65354,10.);
#10357=VECTOR('',#65355,10.);
#10358=VECTOR('',#65356,10.);
#10359=VECTOR('',#65359,10.);
#10360=VECTOR('',#65360,10.);
#10361=VECTOR('',#65361,10.);
#10362=VECTOR('',#65364,10.);
#10363=VECTOR('',#65365,10.);
#10364=VECTOR('',#65366,10.);
#10365=VECTOR('',#65369,10.);
#10366=VECTOR('',#65370,10.);
#10367=VECTOR('',#65373,10.);
#10368=VECTOR('',#65374,10.);
#10369=VECTOR('',#65375,10.);
#10370=VECTOR('',#65376,10.);
#10371=VECTOR('',#65377,10.);
#10372=VECTOR('',#65378,10.);
#10373=VECTOR('',#65379,10.);
#10374=VECTOR('',#65380,10.);
#10375=VECTOR('',#65381,10.);
#10376=VECTOR('',#65384,10.);
#10377=VECTOR('',#65385,10.);
#10378=VECTOR('',#65386,10.);
#10379=VECTOR('',#65389,10.);
#10380=VECTOR('',#65390,10.);
#10381=VECTOR('',#65391,10.);
#10382=VECTOR('',#65394,10.);
#10383=VECTOR('',#65395,10.);
#10384=VECTOR('',#65396,10.);
#10385=VECTOR('',#65401,10.);
#10386=VECTOR('',#65402,10.);
#10387=VECTOR('',#65403,10.);
#10388=VECTOR('',#65404,10.);
#10389=VECTOR('',#65405,10.);
#10390=VECTOR('',#65406,10.);
#10391=VECTOR('',#65407,10.);
#10392=VECTOR('',#65408,10.);
#10393=VECTOR('',#65411,10.);
#10394=VECTOR('',#65412,10.);
#10395=VECTOR('',#65413,10.);
#10396=VECTOR('',#65416,10.);
#10397=VECTOR('',#65417,10.);
#10398=VECTOR('',#65418,10.);
#10399=VECTOR('',#65421,10.);
#10400=VECTOR('',#65422,10.);
#10401=VECTOR('',#65423,10.);
#10402=VECTOR('',#65424,10.);
#10403=VECTOR('',#65425,10.);
#10404=VECTOR('',#65426,10.);
#10405=VECTOR('',#65427,10.);
#10406=VECTOR('',#65428,10.);
#10407=VECTOR('',#65429,10.);
#10408=VECTOR('',#65430,10.);
#10409=VECTOR('',#65433,10.);
#10410=VECTOR('',#65434,10.);
#10411=VECTOR('',#65435,10.);
#10412=VECTOR('',#65438,10.);
#10413=VECTOR('',#65439,10.);
#10414=VECTOR('',#65440,10.);
#10415=VECTOR('',#65443,10.);
#10416=VECTOR('',#65444,10.);
#10417=VECTOR('',#65445,10.);
#10418=VECTOR('',#65448,10.);
#10419=VECTOR('',#65449,10.);
#10420=VECTOR('',#65454,10.);
#10421=VECTOR('',#65455,10.);
#10422=VECTOR('',#65456,10.);
#10423=VECTOR('',#65457,10.);
#10424=VECTOR('',#65460,10.);
#10425=VECTOR('',#65461,10.);
#10426=VECTOR('',#65462,10.);
#10427=VECTOR('',#65465,10.);
#10428=VECTOR('',#65466,10.);
#10429=VECTOR('',#65467,10.);
#10430=VECTOR('',#65470,10.);
#10431=VECTOR('',#65471,10.);
#10432=VECTOR('',#65478,4.75);
#10433=VECTOR('',#65485,4.5);
#10434=VECTOR('',#65488,10.);
#10435=VECTOR('',#65491,10.);
#10436=VECTOR('',#65494,10.);
#10437=VECTOR('',#65497,10.);
#10438=VECTOR('',#65524,4.75);
#10439=VECTOR('',#65529,10.);
#10440=VECTOR('',#65532,10.);
#10441=VECTOR('',#65535,10.);
#10442=VECTOR('',#65538,10.);
#10443=VECTOR('',#65547,4.75);
#10444=VECTOR('',#65554,4.5);
#10445=VECTOR('',#65557,4.75);
#10446=VECTOR('',#65560,4.75);
#10447=VECTOR('',#65567,4.5);
#10448=VECTOR('',#65570,4.75);
#10449=VECTOR('',#65573,4.75);
#10450=VECTOR('',#65580,4.5);
#10451=VECTOR('',#65583,4.75);
#10452=VECTOR('',#65588,1.5);
#10453=VECTOR('',#65591,3.);
#10454=VECTOR('',#65596,1.5);
#10455=VECTOR('',#65599,3.);
#10456=VECTOR('',#65604,1.525);
#10457=VECTOR('',#65607,3.175);
#10458=VECTOR('',#65612,3.05);
#10459=VECTOR('',#65617,1.525);
#10460=VECTOR('',#65620,3.175);
#10461=VECTOR('',#65625,3.05);
#10462=VECTOR('',#65630,1.525);
#10463=VECTOR('',#65633,3.175);
#10464=VECTOR('',#65638,3.05);
#10465=VECTOR('',#65643,1.525);
#10466=VECTOR('',#65646,3.175);
#10467=VECTOR('',#65651,3.05);
#10468=VECTOR('',#65656,20.025);
#10469=VECTOR('',#65661,10.);
#10470=VECTOR('',#65664,10.);
#10471=VECTOR('',#65667,10.);
#10472=VECTOR('',#65668,10.);
#10473=VECTOR('',#65671,10.);
#10474=VECTOR('',#65676,10.);
#10475=VECTOR('',#65677,10.);
#10476=VECTOR('',#65680,10.);
#10477=VECTOR('',#65685,10.);
#10478=VECTOR('',#65686,10.);
#10479=VECTOR('',#65689,10.);
#10480=VECTOR('',#65694,10.);
#10481=VECTOR('',#65697,10.);
#10482=VECTOR('',#65698,10.);
#10483=VECTOR('',#65699,10.);
#10484=VECTOR('',#65702,10.);
#10485=VECTOR('',#65707,10.);
#10486=VECTOR('',#65708,10.);
#10487=VECTOR('',#65711,10.);
#10488=VECTOR('',#65716,10.);
#10489=VECTOR('',#65717,10.);
#10490=VECTOR('',#65720,10.);
#10491=VECTOR('',#65723,10.);
#10492=VECTOR('',#65726,10.);
#10493=VECTOR('',#65729,10.);
#10494=VECTOR('',#65730,10.);
#10495=VECTOR('',#65733,10.);
#10496=VECTOR('',#65738,10.);
#10497=VECTOR('',#65739,10.);
#10498=VECTOR('',#65746,10.);
#10499=VECTOR('',#65749,10.);
#10500=VECTOR('',#65752,10.);
#10501=VECTOR('',#65761,5.5);
#10502=VECTOR('',#65766,5.75);
#10503=VECTOR('',#65777,27.75);
#10504=VECTOR('',#65782,28.);
#10505=VECTOR('',#65787,27.5);
#10506=VECTOR('',#65794,5.75);
#10507=VECTOR('',#65799,5.);
#10508=VECTOR('',#65804,5.);
#10509=VECTOR('',#65807,5.);
#10510=VECTOR('',#65810,5.);
#10511=VECTOR('',#65813,5.);
#10512=VECTOR('',#65816,5.);
#10513=VECTOR('',#65819,5.);
#10514=VECTOR('',#65822,5.);
#10515=VECTOR('',#65825,5.);
#10516=VECTOR('',#65828,5.);
#10517=VECTOR('',#65831,5.);
#10518=VECTOR('',#65834,5.);
#10519=VECTOR('',#65837,5.);
#10520=VECTOR('',#65840,5.);
#10521=VECTOR('',#65843,5.);
#10522=VECTOR('',#65846,5.);
#10523=VECTOR('',#65849,4.0705);
#10524=VECTOR('',#65854,4.0705);
#10525=VECTOR('',#65859,4.0705);
#10526=VECTOR('',#65862,4.0705);
#10527=VECTOR('',#65865,4.0705);
#10528=VECTOR('',#65868,4.0705);
#10529=VECTOR('',#65871,4.0705);
#10530=VECTOR('',#65874,4.0705);
#10531=VECTOR('',#65877,4.0705);
#10532=VECTOR('',#65880,4.0705);
#10533=VECTOR('',#65883,4.0705);
#10534=VECTOR('',#65886,4.0705);
#10535=VECTOR('',#65889,4.0705);
#10536=VECTOR('',#65892,4.0705);
#10537=VECTOR('',#65895,4.0705);
#10538=VECTOR('',#65898,4.0705);
#10539=VECTOR('',#65931,10.);
#10540=VECTOR('',#65932,10.);
#10541=VECTOR('',#65933,10.);
#10542=VECTOR('',#65934,10.);
#10543=VECTOR('',#65939,10.);
#10544=VECTOR('',#65942,10.);
#10545=VECTOR('',#65943,10.);
#10546=VECTOR('',#65950,10.);
#10547=VECTOR('',#65951,10.);
#10548=VECTOR('',#65952,10.);
#10549=VECTOR('',#65953,10.);
#10550=VECTOR('',#65958,10.);
#10551=VECTOR('',#65961,10.);
#10552=VECTOR('',#65962,10.);
#10553=VECTOR('',#65969,10.);
#10554=VECTOR('',#65970,10.);
#10555=VECTOR('',#65971,10.);
#10556=VECTOR('',#65972,10.);
#10557=VECTOR('',#65977,10.);
#10558=VECTOR('',#65980,10.);
#10559=VECTOR('',#65981,10.);
#10560=VECTOR('',#65988,10.);
#10561=VECTOR('',#65989,10.);
#10562=VECTOR('',#65990,10.);
#10563=VECTOR('',#65991,10.);
#10564=VECTOR('',#65996,10.);
#10565=VECTOR('',#65999,10.);
#10566=VECTOR('',#66000,10.);
#10567=VECTOR('',#66007,10.);
#10568=VECTOR('',#66008,10.);
#10569=VECTOR('',#66009,10.);
#10570=VECTOR('',#66010,10.);
#10571=VECTOR('',#66015,10.);
#10572=VECTOR('',#66018,10.);
#10573=VECTOR('',#66019,10.);
#10574=VECTOR('',#66026,10.);
#10575=VECTOR('',#66027,10.);
#10576=VECTOR('',#66028,10.);
#10577=VECTOR('',#66029,10.);
#10578=VECTOR('',#66034,10.);
#10579=VECTOR('',#66037,10.);
#10580=VECTOR('',#66038,10.);
#10581=VECTOR('',#66045,10.);
#10582=VECTOR('',#66046,10.);
#10583=VECTOR('',#66047,10.);
#10584=VECTOR('',#66048,10.);
#10585=VECTOR('',#66053,10.);
#10586=VECTOR('',#66056,10.);
#10587=VECTOR('',#66057,10.);
#10588=VECTOR('',#66064,10.);
#10589=VECTOR('',#66065,10.);
#10590=VECTOR('',#66066,10.);
#10591=VECTOR('',#66067,10.);
#10592=VECTOR('',#66072,10.);
#10593=VECTOR('',#66075,10.);
#10594=VECTOR('',#66076,10.);
#10595=VECTOR('',#66083,10.);
#10596=VECTOR('',#66084,10.);
#10597=VECTOR('',#66085,10.);
#10598=VECTOR('',#66086,10.);
#10599=VECTOR('',#66091,10.);
#10600=VECTOR('',#66094,10.);
#10601=VECTOR('',#66095,10.);
#10602=VECTOR('',#66102,10.);
#10603=VECTOR('',#66103,10.);
#10604=VECTOR('',#66104,10.);
#10605=VECTOR('',#66105,10.);
#10606=VECTOR('',#66110,10.);
#10607=VECTOR('',#66113,10.);
#10608=VECTOR('',#66114,10.);
#10609=VECTOR('',#66121,10.);
#10610=VECTOR('',#66122,10.);
#10611=VECTOR('',#66123,10.);
#10612=VECTOR('',#66124,10.);
#10613=VECTOR('',#66129,10.);
#10614=VECTOR('',#66132,10.);
#10615=VECTOR('',#66133,10.);
#10616=VECTOR('',#66140,10.);
#10617=VECTOR('',#66141,10.);
#10618=VECTOR('',#66142,10.);
#10619=VECTOR('',#66143,10.);
#10620=VECTOR('',#66148,10.);
#10621=VECTOR('',#66151,10.);
#10622=VECTOR('',#66152,10.);
#10623=VECTOR('',#66159,10.);
#10624=VECTOR('',#66160,10.);
#10625=VECTOR('',#66161,10.);
#10626=VECTOR('',#66162,10.);
#10627=VECTOR('',#66167,10.);
#10628=VECTOR('',#66170,10.);
#10629=VECTOR('',#66171,10.);
#10630=VECTOR('',#66178,10.);
#10631=VECTOR('',#66179,10.);
#10632=VECTOR('',#66180,10.);
#10633=VECTOR('',#66181,10.);
#10634=VECTOR('',#66186,10.);
#10635=VECTOR('',#66189,10.);
#10636=VECTOR('',#66190,10.);
#10637=VECTOR('',#66197,10.);
#10638=VECTOR('',#66198,10.);
#10639=VECTOR('',#66199,10.);
#10640=VECTOR('',#66200,10.);
#10641=VECTOR('',#66205,10.);
#10642=VECTOR('',#66208,10.);
#10643=VECTOR('',#66209,10.);
#10644=VECTOR('',#66216,10.);
#10645=VECTOR('',#66217,10.);
#10646=VECTOR('',#66218,10.);
#10647=VECTOR('',#66219,10.);
#10648=VECTOR('',#66224,10.);
#10649=VECTOR('',#66227,10.);
#10650=VECTOR('',#66228,10.);
#10651=VECTOR('',#66235,10.);
#10652=VECTOR('',#66236,10.);
#10653=VECTOR('',#66237,10.);
#10654=VECTOR('',#66238,10.);
#10655=VECTOR('',#66243,10.);
#10656=VECTOR('',#66246,10.);
#10657=VECTOR('',#66247,10.);
#10658=VECTOR('',#66254,10.);
#10659=VECTOR('',#66255,10.);
#10660=VECTOR('',#66256,10.);
#10661=VECTOR('',#66257,10.);
#10662=VECTOR('',#66262,10.);
#10663=VECTOR('',#66267,10.);
#10664=VECTOR('',#66268,10.);
#10665=VECTOR('',#66277,10.);
#10666=VECTOR('',#66278,10.);
#10667=VECTOR('',#66279,10.);
#10668=VECTOR('',#66280,10.);
#10669=VECTOR('',#66285,10.);
#10670=VECTOR('',#66288,10.);
#10671=VECTOR('',#66289,10.);
#10672=VECTOR('',#66296,10.);
#10673=VECTOR('',#66297,10.);
#10674=VECTOR('',#66298,10.);
#10675=VECTOR('',#66299,10.);
#10676=VECTOR('',#66304,10.);
#10677=VECTOR('',#66307,10.);
#10678=VECTOR('',#66308,10.);
#10679=VECTOR('',#66315,10.);
#10680=VECTOR('',#66316,10.);
#10681=VECTOR('',#66317,10.);
#10682=VECTOR('',#66318,10.);
#10683=VECTOR('',#66323,10.);
#10684=VECTOR('',#66326,10.);
#10685=VECTOR('',#66327,10.);
#10686=VECTOR('',#66334,10.);
#10687=VECTOR('',#66335,10.);
#10688=VECTOR('',#66336,10.);
#10689=VECTOR('',#66337,10.);
#10690=VECTOR('',#66342,10.);
#10691=VECTOR('',#66345,10.);
#10692=VECTOR('',#66346,10.);
#10693=VECTOR('',#66353,10.);
#10694=VECTOR('',#66354,10.);
#10695=VECTOR('',#66355,10.);
#10696=VECTOR('',#66356,10.);
#10697=VECTOR('',#66361,10.);
#10698=VECTOR('',#66364,10.);
#10699=VECTOR('',#66365,10.);
#10700=VECTOR('',#66372,10.);
#10701=VECTOR('',#66373,10.);
#10702=VECTOR('',#66374,10.);
#10703=VECTOR('',#66375,10.);
#10704=VECTOR('',#66380,10.);
#10705=VECTOR('',#66383,10.);
#10706=VECTOR('',#66384,10.);
#10707=VECTOR('',#66391,10.);
#10708=VECTOR('',#66392,10.);
#10709=VECTOR('',#66393,10.);
#10710=VECTOR('',#66394,10.);
#10711=VECTOR('',#66399,10.);
#10712=VECTOR('',#66402,10.);
#10713=VECTOR('',#66403,10.);
#10714=VECTOR('',#66410,10.);
#10715=VECTOR('',#66411,10.);
#10716=VECTOR('',#66412,10.);
#10717=VECTOR('',#66413,10.);
#10718=VECTOR('',#66418,10.);
#10719=VECTOR('',#66421,10.);
#10720=VECTOR('',#66422,10.);
#10721=VECTOR('',#66429,10.);
#10722=VECTOR('',#66430,10.);
#10723=VECTOR('',#66431,10.);
#10724=VECTOR('',#66432,10.);
#10725=VECTOR('',#66437,10.);
#10726=VECTOR('',#66440,10.);
#10727=VECTOR('',#66441,10.);
#10728=VECTOR('',#66448,10.);
#10729=VECTOR('',#66449,10.);
#10730=VECTOR('',#66450,10.);
#10731=VECTOR('',#66451,10.);
#10732=VECTOR('',#66456,10.);
#10733=VECTOR('',#66459,10.);
#10734=VECTOR('',#66460,10.);
#10735=VECTOR('',#66467,10.);
#10736=VECTOR('',#66468,10.);
#10737=VECTOR('',#66469,10.);
#10738=VECTOR('',#66470,10.);
#10739=VECTOR('',#66475,10.);
#10740=VECTOR('',#66478,10.);
#10741=VECTOR('',#66479,10.);
#10742=VECTOR('',#66486,10.);
#10743=VECTOR('',#66487,10.);
#10744=VECTOR('',#66488,10.);
#10745=VECTOR('',#66489,10.);
#10746=VECTOR('',#66494,10.);
#10747=VECTOR('',#66497,10.);
#10748=VECTOR('',#66498,10.);
#10749=VECTOR('',#66505,10.);
#10750=VECTOR('',#66506,10.);
#10751=VECTOR('',#66507,10.);
#10752=VECTOR('',#66508,10.);
#10753=VECTOR('',#66513,10.);
#10754=VECTOR('',#66516,10.);
#10755=VECTOR('',#66517,10.);
#10756=VECTOR('',#66524,10.);
#10757=VECTOR('',#66525,10.);
#10758=VECTOR('',#66526,10.);
#10759=VECTOR('',#66527,10.);
#10760=VECTOR('',#66532,10.);
#10761=VECTOR('',#66535,10.);
#10762=VECTOR('',#66536,10.);
#10763=VECTOR('',#66543,10.);
#10764=VECTOR('',#66544,10.);
#10765=VECTOR('',#66545,10.);
#10766=VECTOR('',#66546,10.);
#10767=VECTOR('',#66551,10.);
#10768=VECTOR('',#66554,10.);
#10769=VECTOR('',#66555,10.);
#10770=VECTOR('',#66562,10.);
#10771=VECTOR('',#66563,10.);
#10772=VECTOR('',#66564,10.);
#10773=VECTOR('',#66565,10.);
#10774=VECTOR('',#66570,10.);
#10775=VECTOR('',#66573,10.);
#10776=VECTOR('',#66574,10.);
#10777=VECTOR('',#66581,10.);
#10778=VECTOR('',#66582,10.);
#10779=VECTOR('',#66583,10.);
#10780=VECTOR('',#66584,10.);
#10781=VECTOR('',#66589,10.);
#10782=VECTOR('',#66592,10.);
#10783=VECTOR('',#66593,10.);
#10784=VECTOR('',#66602,10.);
#10785=VECTOR('',#66603,10.);
#10786=VECTOR('',#66606,10.);
#10787=VECTOR('',#66607,10.);
#10788=VECTOR('',#66608,10.);
#10789=VECTOR('',#66611,10.);
#10790=VECTOR('',#66612,10.);
#10791=VECTOR('',#66619,2.);
#10792=VECTOR('',#66624,10.);
#10793=VECTOR('',#66625,10.);
#10794=VECTOR('',#66626,10.);
#10795=VECTOR('',#66627,10.);
#10796=VECTOR('',#66630,10.);
#10797=VECTOR('',#66631,10.);
#10798=VECTOR('',#66632,10.);
#10799=VECTOR('',#66635,10.);
#10800=VECTOR('',#66636,10.);
#10801=VECTOR('',#66637,10.);
#10802=VECTOR('',#66640,10.);
#10803=VECTOR('',#66641,10.);
#10804=VECTOR('',#66642,10.);
#10805=VECTOR('',#66645,10.);
#10806=VECTOR('',#66646,10.);
#10807=VECTOR('',#66647,10.);
#10808=VECTOR('',#66650,10.);
#10809=VECTOR('',#66651,10.);
#10810=VECTOR('',#66660,4.5);
#10811=VECTOR('',#66697,8.);
#10812=VECTOR('',#66740,7.5);
#10813=VECTOR('',#66749,9.9);
#10814=VECTOR('',#66756,10.);
#10815=VECTOR('',#66761,9.9);
#10816=VECTOR('',#66768,5.35);
#10817=VECTOR('',#66773,5.25);
#10818=VECTOR('',#66778,5.35);
#10819=VECTOR('',#66787,5.1);
#10820=VECTOR('',#66796,9.05);
#10821=VECTOR('',#66805,10.);
#10822=VECTOR('',#66808,10.);
#10823=VECTOR('',#66813,10.);
#10824=VECTOR('',#66814,10.);
#10825=VECTOR('',#66851,3.);
#10826=VECTOR('',#66856,3.);
#10827=VECTOR('',#66859,3.);
#10828=VECTOR('',#66862,3.);
#10829=VECTOR('',#66865,3.);
#10830=VECTOR('',#66868,3.);
#10831=VECTOR('',#66871,3.);
#10832=VECTOR('',#66874,3.);
#10833=VECTOR('',#66877,3.);
#10834=VECTOR('',#66880,3.);
#10835=VECTOR('',#66883,3.);
#10836=VECTOR('',#66886,3.);
#10837=VECTOR('',#66889,3.);
#10838=VECTOR('',#66892,3.);
#10839=VECTOR('',#66895,3.);
#10840=VECTOR('',#66898,3.);
#10841=VECTOR('',#66903,2.37175);
#10842=VECTOR('',#66908,2.37175);
#10843=VECTOR('',#66911,2.37175);
#10844=VECTOR('',#66914,2.37175);
#10845=VECTOR('',#66917,2.37175);
#10846=VECTOR('',#66920,2.37175);
#10847=VECTOR('',#66923,2.37175);
#10848=VECTOR('',#66926,2.37175);
#10849=VECTOR('',#66929,2.37175);
#10850=VECTOR('',#66932,2.37175);
#10851=VECTOR('',#66935,2.37175);
#10852=VECTOR('',#66938,2.37175);
#10853=VECTOR('',#66941,2.37175);
#10854=VECTOR('',#66944,2.37175);
#10855=VECTOR('',#66947,2.37175);
#10856=VECTOR('',#66980,10.);
#10857=VECTOR('',#66981,10.);
#10858=VECTOR('',#66982,10.);
#10859=VECTOR('',#66983,10.);
#10860=VECTOR('',#66988,10.);
#10861=VECTOR('',#66991,10.);
#10862=VECTOR('',#66992,10.);
#10863=VECTOR('',#66999,10.);
#10864=VECTOR('',#67000,10.);
#10865=VECTOR('',#67001,10.);
#10866=VECTOR('',#67002,10.);
#10867=VECTOR('',#67007,10.);
#10868=VECTOR('',#67010,10.);
#10869=VECTOR('',#67011,10.);
#10870=VECTOR('',#67018,10.);
#10871=VECTOR('',#67019,10.);
#10872=VECTOR('',#67020,10.);
#10873=VECTOR('',#67021,10.);
#10874=VECTOR('',#67026,10.);
#10875=VECTOR('',#67029,10.);
#10876=VECTOR('',#67030,10.);
#10877=VECTOR('',#67037,10.);
#10878=VECTOR('',#67038,10.);
#10879=VECTOR('',#67039,10.);
#10880=VECTOR('',#67040,10.);
#10881=VECTOR('',#67045,10.);
#10882=VECTOR('',#67048,10.);
#10883=VECTOR('',#67049,10.);
#10884=VECTOR('',#67056,10.);
#10885=VECTOR('',#67057,10.);
#10886=VECTOR('',#67058,10.);
#10887=VECTOR('',#67059,10.);
#10888=VECTOR('',#67064,10.);
#10889=VECTOR('',#67067,10.);
#10890=VECTOR('',#67068,10.);
#10891=VECTOR('',#67075,10.);
#10892=VECTOR('',#67076,10.);
#10893=VECTOR('',#67077,10.);
#10894=VECTOR('',#67078,10.);
#10895=VECTOR('',#67083,10.);
#10896=VECTOR('',#67086,10.);
#10897=VECTOR('',#67087,10.);
#10898=VECTOR('',#67094,10.);
#10899=VECTOR('',#67095,10.);
#10900=VECTOR('',#67096,10.);
#10901=VECTOR('',#67097,10.);
#10902=VECTOR('',#67102,10.);
#10903=VECTOR('',#67105,10.);
#10904=VECTOR('',#67106,10.);
#10905=VECTOR('',#67113,10.);
#10906=VECTOR('',#67114,10.);
#10907=VECTOR('',#67115,10.);
#10908=VECTOR('',#67116,10.);
#10909=VECTOR('',#67121,10.);
#10910=VECTOR('',#67124,10.);
#10911=VECTOR('',#67125,10.);
#10912=VECTOR('',#67132,10.);
#10913=VECTOR('',#67133,10.);
#10914=VECTOR('',#67134,10.);
#10915=VECTOR('',#67135,10.);
#10916=VECTOR('',#67140,10.);
#10917=VECTOR('',#67143,10.);
#10918=VECTOR('',#67144,10.);
#10919=VECTOR('',#67151,10.);
#10920=VECTOR('',#67152,10.);
#10921=VECTOR('',#67153,10.);
#10922=VECTOR('',#67154,10.);
#10923=VECTOR('',#67159,10.);
#10924=VECTOR('',#67162,10.);
#10925=VECTOR('',#67163,10.);
#10926=VECTOR('',#67170,10.);
#10927=VECTOR('',#67171,10.);
#10928=VECTOR('',#67172,10.);
#10929=VECTOR('',#67173,10.);
#10930=VECTOR('',#67178,10.);
#10931=VECTOR('',#67181,10.);
#10932=VECTOR('',#67182,10.);
#10933=VECTOR('',#67189,10.);
#10934=VECTOR('',#67190,10.);
#10935=VECTOR('',#67191,10.);
#10936=VECTOR('',#67192,10.);
#10937=VECTOR('',#67197,10.);
#10938=VECTOR('',#67200,10.);
#10939=VECTOR('',#67201,10.);
#10940=VECTOR('',#67208,10.);
#10941=VECTOR('',#67209,10.);
#10942=VECTOR('',#67210,10.);
#10943=VECTOR('',#67211,10.);
#10944=VECTOR('',#67216,10.);
#10945=VECTOR('',#67219,10.);
#10946=VECTOR('',#67220,10.);
#10947=VECTOR('',#67227,10.);
#10948=VECTOR('',#67228,10.);
#10949=VECTOR('',#67229,10.);
#10950=VECTOR('',#67230,10.);
#10951=VECTOR('',#67235,10.);
#10952=VECTOR('',#67238,10.);
#10953=VECTOR('',#67239,10.);
#10954=VECTOR('',#67246,10.);
#10955=VECTOR('',#67247,10.);
#10956=VECTOR('',#67248,10.);
#10957=VECTOR('',#67249,10.);
#10958=VECTOR('',#67254,10.);
#10959=VECTOR('',#67257,10.);
#10960=VECTOR('',#67258,10.);
#10961=VECTOR('',#67265,10.);
#10962=VECTOR('',#67266,10.);
#10963=VECTOR('',#67267,10.);
#10964=VECTOR('',#67268,10.);
#10965=VECTOR('',#67273,10.);
#10966=VECTOR('',#67276,10.);
#10967=VECTOR('',#67277,10.);
#10968=VECTOR('',#67284,10.);
#10969=VECTOR('',#67285,10.);
#10970=VECTOR('',#67286,10.);
#10971=VECTOR('',#67287,10.);
#10972=VECTOR('',#67292,10.);
#10973=VECTOR('',#67295,10.);
#10974=VECTOR('',#67296,10.);
#10975=VECTOR('',#67303,10.);
#10976=VECTOR('',#67304,10.);
#10977=VECTOR('',#67305,10.);
#10978=VECTOR('',#67306,10.);
#10979=VECTOR('',#67311,10.);
#10980=VECTOR('',#67316,10.);
#10981=VECTOR('',#67317,10.);
#10982=VECTOR('',#67326,10.);
#10983=VECTOR('',#67327,10.);
#10984=VECTOR('',#67328,10.);
#10985=VECTOR('',#67329,10.);
#10986=VECTOR('',#67334,10.);
#10987=VECTOR('',#67337,10.);
#10988=VECTOR('',#67338,10.);
#10989=VECTOR('',#67345,10.);
#10990=VECTOR('',#67346,10.);
#10991=VECTOR('',#67347,10.);
#10992=VECTOR('',#67348,10.);
#10993=VECTOR('',#67353,10.);
#10994=VECTOR('',#67356,10.);
#10995=VECTOR('',#67357,10.);
#10996=VECTOR('',#67364,10.);
#10997=VECTOR('',#67365,10.);
#10998=VECTOR('',#67366,10.);
#10999=VECTOR('',#67367,10.);
#11000=VECTOR('',#67372,10.);
#11001=VECTOR('',#67375,10.);
#11002=VECTOR('',#67376,10.);
#11003=VECTOR('',#67383,10.);
#11004=VECTOR('',#67384,10.);
#11005=VECTOR('',#67385,10.);
#11006=VECTOR('',#67386,10.);
#11007=VECTOR('',#67391,10.);
#11008=VECTOR('',#67394,10.);
#11009=VECTOR('',#67395,10.);
#11010=VECTOR('',#67402,10.);
#11011=VECTOR('',#67403,10.);
#11012=VECTOR('',#67404,10.);
#11013=VECTOR('',#67405,10.);
#11014=VECTOR('',#67410,10.);
#11015=VECTOR('',#67413,10.);
#11016=VECTOR('',#67414,10.);
#11017=VECTOR('',#67421,10.);
#11018=VECTOR('',#67422,10.);
#11019=VECTOR('',#67423,10.);
#11020=VECTOR('',#67424,10.);
#11021=VECTOR('',#67429,10.);
#11022=VECTOR('',#67432,10.);
#11023=VECTOR('',#67433,10.);
#11024=VECTOR('',#67440,10.);
#11025=VECTOR('',#67441,10.);
#11026=VECTOR('',#67442,10.);
#11027=VECTOR('',#67443,10.);
#11028=VECTOR('',#67448,10.);
#11029=VECTOR('',#67451,10.);
#11030=VECTOR('',#67452,10.);
#11031=VECTOR('',#67459,10.);
#11032=VECTOR('',#67460,10.);
#11033=VECTOR('',#67461,10.);
#11034=VECTOR('',#67462,10.);
#11035=VECTOR('',#67467,10.);
#11036=VECTOR('',#67470,10.);
#11037=VECTOR('',#67471,10.);
#11038=VECTOR('',#67478,10.);
#11039=VECTOR('',#67479,10.);
#11040=VECTOR('',#67480,10.);
#11041=VECTOR('',#67481,10.);
#11042=VECTOR('',#67486,10.);
#11043=VECTOR('',#67489,10.);
#11044=VECTOR('',#67490,10.);
#11045=VECTOR('',#67497,10.);
#11046=VECTOR('',#67498,10.);
#11047=VECTOR('',#67499,10.);
#11048=VECTOR('',#67500,10.);
#11049=VECTOR('',#67505,10.);
#11050=VECTOR('',#67508,10.);
#11051=VECTOR('',#67509,10.);
#11052=VECTOR('',#67516,10.);
#11053=VECTOR('',#67517,10.);
#11054=VECTOR('',#67518,10.);
#11055=VECTOR('',#67519,10.);
#11056=VECTOR('',#67524,10.);
#11057=VECTOR('',#67527,10.);
#11058=VECTOR('',#67528,10.);
#11059=VECTOR('',#67535,10.);
#11060=VECTOR('',#67536,10.);
#11061=VECTOR('',#67537,10.);
#11062=VECTOR('',#67538,10.);
#11063=VECTOR('',#67543,10.);
#11064=VECTOR('',#67546,10.);
#11065=VECTOR('',#67547,10.);
#11066=VECTOR('',#67554,10.);
#11067=VECTOR('',#67555,10.);
#11068=VECTOR('',#67556,10.);
#11069=VECTOR('',#67557,10.);
#11070=VECTOR('',#67562,10.);
#11071=VECTOR('',#67565,10.);
#11072=VECTOR('',#67566,10.);
#11073=VECTOR('',#67573,10.);
#11074=VECTOR('',#67574,10.);
#11075=VECTOR('',#67575,10.);
#11076=VECTOR('',#67576,10.);
#11077=VECTOR('',#67581,10.);
#11078=VECTOR('',#67584,10.);
#11079=VECTOR('',#67585,10.);
#11080=VECTOR('',#67592,10.);
#11081=VECTOR('',#67593,10.);
#11082=VECTOR('',#67594,10.);
#11083=VECTOR('',#67595,10.);
#11084=VECTOR('',#67600,10.);
#11085=VECTOR('',#67603,10.);
#11086=VECTOR('',#67604,10.);
#11087=VECTOR('',#67611,10.);
#11088=VECTOR('',#67612,10.);
#11089=VECTOR('',#67613,10.);
#11090=VECTOR('',#67614,10.);
#11091=VECTOR('',#67619,10.);
#11092=VECTOR('',#67622,10.);
#11093=VECTOR('',#67623,10.);
#11094=VECTOR('',#67630,10.);
#11095=VECTOR('',#67631,10.);
#11096=VECTOR('',#67632,10.);
#11097=VECTOR('',#67633,10.);
#11098=VECTOR('',#67638,10.);
#11099=VECTOR('',#67641,10.);
#11100=VECTOR('',#67642,10.);
#11101=VECTOR('',#67651,10.);
#11102=VECTOR('',#67652,10.);
#11103=VECTOR('',#67655,10.);
#11104=VECTOR('',#67656,10.);
#11105=VECTOR('',#67657,10.);
#11106=VECTOR('',#67660,10.);
#11107=VECTOR('',#67661,10.);
#11108=VECTOR('',#67668,1.25);
#11109=VECTOR('',#67673,10.);
#11110=VECTOR('',#67674,10.);
#11111=VECTOR('',#67675,10.);
#11112=VECTOR('',#67676,10.);
#11113=VECTOR('',#67679,10.);
#11114=VECTOR('',#67680,10.);
#11115=VECTOR('',#67681,10.);
#11116=VECTOR('',#67684,10.);
#11117=VECTOR('',#67685,10.);
#11118=VECTOR('',#67686,10.);
#11119=VECTOR('',#67689,10.);
#11120=VECTOR('',#67690,10.);
#11121=VECTOR('',#67691,10.);
#11122=VECTOR('',#67694,10.);
#11123=VECTOR('',#67695,10.);
#11124=VECTOR('',#67696,10.);
#11125=VECTOR('',#67699,10.);
#11126=VECTOR('',#67700,10.);
#11127=VECTOR('',#67709,2.7);
#11128=VECTOR('',#67746,5.);
#11129=VECTOR('',#67789,4.7);
#11130=VECTOR('',#67806,2.7);
#11131=VECTOR('',#67819,2.7);
#11132=VECTOR('',#67822,3.);
#11133=VECTOR('',#67827,4.);
#11134=VECTOR('',#67832,4.);
#11135=VECTOR('',#67835,4.);
#11136=VECTOR('',#67838,4.);
#11137=VECTOR('',#67841,4.);
#11138=VECTOR('',#67844,4.);
#11139=VECTOR('',#67847,4.);
#11140=VECTOR('',#67850,4.);
#11141=VECTOR('',#67853,4.);
#11142=VECTOR('',#67856,4.);
#11143=VECTOR('',#67859,4.);
#11144=VECTOR('',#67862,4.);
#11145=VECTOR('',#67865,4.);
#11146=VECTOR('',#67868,4.);
#11147=VECTOR('',#67871,4.);
#11148=VECTOR('',#67874,4.);
#11149=VECTOR('',#67877,4.);
#11150=VECTOR('',#67880,4.);
#11151=VECTOR('',#67883,4.);
#11152=VECTOR('',#67886,4.);
#11153=VECTOR('',#67889,4.);
#11154=VECTOR('',#67892,4.);
#11155=VECTOR('',#67895,4.);
#11156=VECTOR('',#67898,3.22275);
#11157=VECTOR('',#67903,3.22275);
#11158=VECTOR('',#67906,3.22275);
#11159=VECTOR('',#67909,3.22275);
#11160=VECTOR('',#67912,3.22275);
#11161=VECTOR('',#67915,3.22275);
#11162=VECTOR('',#67918,3.22275);
#11163=VECTOR('',#67921,3.22275);
#11164=VECTOR('',#67924,3.22275);
#11165=VECTOR('',#67927,3.22275);
#11166=VECTOR('',#67930,3.22275);
#11167=VECTOR('',#67933,3.22275);
#11168=VECTOR('',#67936,3.22275);
#11169=VECTOR('',#67939,3.22275);
#11170=VECTOR('',#67942,3.22275);
#11171=VECTOR('',#67945,3.22275);
#11172=VECTOR('',#67948,3.22275);
#11173=VECTOR('',#67951,3.22275);
#11174=VECTOR('',#67954,3.22275);
#11175=VECTOR('',#67957,3.22275);
#11176=VECTOR('',#67960,3.22275);
#11177=VECTOR('',#67963,3.22275);
#11178=VECTOR('',#67966,3.22275);
#11179=VECTOR('',#67999,7.09027674973257);
#11180=VECTOR('',#68004,10.);
#11181=VECTOR('',#68005,10.);
#11182=VECTOR('',#68006,10.);
#11183=VECTOR('',#68009,10.);
#11184=VECTOR('',#68010,10.);
#11185=VECTOR('',#68013,10.);
#11186=VECTOR('',#68014,10.);
#11187=VECTOR('',#68019,5.8);
#11188=VECTOR('',#68026,3.6);
#11189=VECTOR('',#68029,10.);
#11190=VECTOR('',#68030,10.);
#11191=VECTOR('',#68033,10.);
#11192=VECTOR('',#68034,10.);
#11193=VECTOR('',#68037,10.);
#11194=VECTOR('',#68048,7.9);
#11195=VECTOR('',#68055,8.);
#11196=VECTOR('',#68060,7.9);
#11197=VECTOR('',#68067,4.3);
#11198=VECTOR('',#68072,4.2);
#11199=VECTOR('',#68077,4.3);
#11200=VECTOR('',#68086,7.4);
#11201=VECTOR('',#68095,10.);
#11202=VECTOR('',#68098,10.);
#11203=VECTOR('',#68105,10.);
#11204=VECTOR('',#68106,10.);
#11205=VECTOR('',#68145,4.425);
#11206=VECTOR('',#68150,4.05);
#11207=VECTOR('',#68155,4.425);
#11208=VECTOR('',#68162,7.09027674973257);
#11209=VECTOR('',#68165,10.);
#11210=VECTOR('',#68166,10.);
#11211=VECTOR('',#68169,10.);
#11212=VECTOR('',#68172,10.);
#11213=VECTOR('',#68175,7.09027674973257);
#11214=VECTOR('',#68180,10.);
#11215=VECTOR('',#68183,10.);
#11216=PLANE('',#51261);
#11217=PLANE('',#51262);
#11218=PLANE('',#51264);
#11219=PLANE('',#51265);
#11220=PLANE('',#51267);
#11221=PLANE('',#51268);
#11222=PLANE('',#51270);
#11223=PLANE('',#51271);
#11224=PLANE('',#51273);
#11225=PLANE('',#51274);
#11226=PLANE('',#51276);
#11227=PLANE('',#51277);
#11228=PLANE('',#51279);
#11229=PLANE('',#51280);
#11230=PLANE('',#51282);
#11231=PLANE('',#51283);
#11232=PLANE('',#51285);
#11233=PLANE('',#51286);
#11234=PLANE('',#51288);
#11235=PLANE('',#51289);
#11236=PLANE('',#51291);
#11237=PLANE('',#51292);
#11238=PLANE('',#51294);
#11239=PLANE('',#51295);
#11240=PLANE('',#51297);
#11241=PLANE('',#51298);
#11242=PLANE('',#51300);
#11243=PLANE('',#51301);
#11244=PLANE('',#51303);
#11245=PLANE('',#51304);
#11246=PLANE('',#51306);
#11247=PLANE('',#51307);
#11248=PLANE('',#51309);
#11249=PLANE('',#51310);
#11250=PLANE('',#51312);
#11251=PLANE('',#51313);
#11252=PLANE('',#51315);
#11253=PLANE('',#51316);
#11254=PLANE('',#51318);
#11255=PLANE('',#51319);
#11256=PLANE('',#51321);
#11257=PLANE('',#51322);
#11258=PLANE('',#51324);
#11259=PLANE('',#51325);
#11260=PLANE('',#51327);
#11261=PLANE('',#51328);
#11262=PLANE('',#51330);
#11263=PLANE('',#51331);
#11264=PLANE('',#51333);
#11265=PLANE('',#51334);
#11266=PLANE('',#51336);
#11267=PLANE('',#51337);
#11268=PLANE('',#51339);
#11269=PLANE('',#51340);
#11270=PLANE('',#51342);
#11271=PLANE('',#51343);
#11272=PLANE('',#51345);
#11273=PLANE('',#51346);
#11274=PLANE('',#51348);
#11275=PLANE('',#51349);
#11276=PLANE('',#51351);
#11277=PLANE('',#51352);
#11278=PLANE('',#51354);
#11279=PLANE('',#51355);
#11280=PLANE('',#51357);
#11281=PLANE('',#51358);
#11282=PLANE('',#51360);
#11283=PLANE('',#51361);
#11284=PLANE('',#51363);
#11285=PLANE('',#51364);
#11286=PLANE('',#51366);
#11287=PLANE('',#51367);
#11288=PLANE('',#51441);
#11289=PLANE('',#51443);
#11290=PLANE('',#51445);
#11291=PLANE('',#51447);
#11292=PLANE('',#51449);
#11293=PLANE('',#51451);
#11294=PLANE('',#51453);
#11295=PLANE('',#51455);
#11296=PLANE('',#51457);
#11297=PLANE('',#51459);
#11298=PLANE('',#51461);
#11299=PLANE('',#51463);
#11300=PLANE('',#51465);
#11301=PLANE('',#51467);
#11302=PLANE('',#51469);
#11303=PLANE('',#51471);
#11304=PLANE('',#51473);
#11305=PLANE('',#51475);
#11306=PLANE('',#51477);
#11307=PLANE('',#51479);
#11308=PLANE('',#51481);
#11309=PLANE('',#51483);
#11310=PLANE('',#51485);
#11311=PLANE('',#51487);
#11312=PLANE('',#51489);
#11313=PLANE('',#51491);
#11314=PLANE('',#51493);
#11315=PLANE('',#51495);
#11316=PLANE('',#51497);
#11317=PLANE('',#51499);
#11318=PLANE('',#51501);
#11319=PLANE('',#51503);
#11320=PLANE('',#51505);
#11321=PLANE('',#51507);
#11322=PLANE('',#51509);
#11323=PLANE('',#51511);
#11324=PLANE('',#51513);
#11325=PLANE('',#51514);
#11326=PLANE('',#51515);
#11327=PLANE('',#51516);
#11328=PLANE('',#51517);
#11329=PLANE('',#51518);
#11330=PLANE('',#51519);
#11331=PLANE('',#51520);
#11332=PLANE('',#51521);
#11333=PLANE('',#51522);
#11334=PLANE('',#51523);
#11335=PLANE('',#51524);
#11336=PLANE('',#51525);
#11337=PLANE('',#51526);
#11338=PLANE('',#51527);
#11339=PLANE('',#51528);
#11340=PLANE('',#51529);
#11341=PLANE('',#51530);
#11342=PLANE('',#51531);
#11343=PLANE('',#51532);
#11344=PLANE('',#51533);
#11345=PLANE('',#51534);
#11346=PLANE('',#51535);
#11347=PLANE('',#51536);
#11348=PLANE('',#51537);
#11349=PLANE('',#51538);
#11350=PLANE('',#51539);
#11351=PLANE('',#51540);
#11352=PLANE('',#51541);
#11353=PLANE('',#51542);
#11354=PLANE('',#51543);
#11355=PLANE('',#51544);
#11356=PLANE('',#51545);
#11357=PLANE('',#51546);
#11358=PLANE('',#51547);
#11359=PLANE('',#51548);
#11360=PLANE('',#51549);
#11361=PLANE('',#51551);
#11362=PLANE('',#51553);
#11363=PLANE('',#51555);
#11364=PLANE('',#51557);
#11365=PLANE('',#51559);
#11366=PLANE('',#51561);
#11367=PLANE('',#51563);
#11368=PLANE('',#51565);
#11369=PLANE('',#51567);
#11370=PLANE('',#51569);
#11371=PLANE('',#51571);
#11372=PLANE('',#51573);
#11373=PLANE('',#51575);
#11374=PLANE('',#51577);
#11375=PLANE('',#51579);
#11376=PLANE('',#51581);
#11377=PLANE('',#51583);
#11378=PLANE('',#51585);
#11379=PLANE('',#51587);
#11380=PLANE('',#51589);
#11381=PLANE('',#51591);
#11382=PLANE('',#51593);
#11383=PLANE('',#51595);
#11384=PLANE('',#51597);
#11385=PLANE('',#51599);
#11386=PLANE('',#51601);
#11387=PLANE('',#51603);
#11388=PLANE('',#51605);
#11389=PLANE('',#51607);
#11390=PLANE('',#51609);
#11391=PLANE('',#51611);
#11392=PLANE('',#51613);
#11393=PLANE('',#51615);
#11394=PLANE('',#51617);
#11395=PLANE('',#51619);
#11396=PLANE('',#51620);
#11397=PLANE('',#51621);
#11398=PLANE('',#51622);
#11399=PLANE('',#51623);
#11400=PLANE('',#51624);
#11401=PLANE('',#51625);
#11402=PLANE('',#51626);
#11403=PLANE('',#51627);
#11404=PLANE('',#51628);
#11405=PLANE('',#51629);
#11406=PLANE('',#51630);
#11407=PLANE('',#51631);
#11408=PLANE('',#51632);
#11409=PLANE('',#51633);
#11410=PLANE('',#51634);
#11411=PLANE('',#51635);
#11412=PLANE('',#51636);
#11413=PLANE('',#51637);
#11414=PLANE('',#51638);
#11415=PLANE('',#51639);
#11416=PLANE('',#51640);
#11417=PLANE('',#51641);
#11418=PLANE('',#51642);
#11419=PLANE('',#51643);
#11420=PLANE('',#51644);
#11421=PLANE('',#51645);
#11422=PLANE('',#51646);
#11423=PLANE('',#51647);
#11424=PLANE('',#51648);
#11425=PLANE('',#51649);
#11426=PLANE('',#51650);
#11427=PLANE('',#51651);
#11428=PLANE('',#51652);
#11429=PLANE('',#51653);
#11430=PLANE('',#51654);
#11431=PLANE('',#51655);
#11432=PLANE('',#51656);
#11433=PLANE('',#51657);
#11434=PLANE('',#51658);
#11435=PLANE('',#51659);
#11436=PLANE('',#51660);
#11437=PLANE('',#51661);
#11438=PLANE('',#51662);
#11439=PLANE('',#51663);
#11440=PLANE('',#51664);
#11441=PLANE('',#51665);
#11442=PLANE('',#51666);
#11443=PLANE('',#51667);
#11444=PLANE('',#51668);
#11445=PLANE('',#51669);
#11446=PLANE('',#51670);
#11447=PLANE('',#51671);
#11448=PLANE('',#51672);
#11449=PLANE('',#51673);
#11450=PLANE('',#51674);
#11451=PLANE('',#51675);
#11452=PLANE('',#51676);
#11453=PLANE('',#51677);
#11454=PLANE('',#51678);
#11455=PLANE('',#51679);
#11456=PLANE('',#51680);
#11457=PLANE('',#51681);
#11458=PLANE('',#51682);
#11459=PLANE('',#51683);
#11460=PLANE('',#51684);
#11461=PLANE('',#51685);
#11462=PLANE('',#51686);
#11463=PLANE('',#51687);
#11464=PLANE('',#51688);
#11465=PLANE('',#51689);
#11466=PLANE('',#51690);
#11467=PLANE('',#51691);
#11468=PLANE('',#51692);
#11469=PLANE('',#51693);
#11470=PLANE('',#51695);
#11471=PLANE('',#51697);
#11472=PLANE('',#51699);
#11473=PLANE('',#51701);
#11474=PLANE('',#51703);
#11475=PLANE('',#51704);
#11476=PLANE('',#51706);
#11477=PLANE('',#51708);
#11478=PLANE('',#51710);
#11479=PLANE('',#51712);
#11480=PLANE('',#51714);
#11481=PLANE('',#51715);
#11482=PLANE('',#51717);
#11483=PLANE('',#51718);
#11484=PLANE('',#51720);
#11485=PLANE('',#51722);
#11486=PLANE('',#51724);
#11487=PLANE('',#51726);
#11488=PLANE('',#51728);
#11489=PLANE('',#51729);
#11490=PLANE('',#51731);
#11491=PLANE('',#51733);
#11492=PLANE('',#51735);
#11493=PLANE('',#51737);
#11494=PLANE('',#51739);
#11495=PLANE('',#51740);
#11496=PLANE('',#51792);
#11497=PLANE('',#51793);
#11498=PLANE('',#51794);
#11499=PLANE('',#51795);
#11500=PLANE('',#51796);
#11501=PLANE('',#51797);
#11502=PLANE('',#51798);
#11503=PLANE('',#51799);
#11504=PLANE('',#51800);
#11505=PLANE('',#51801);
#11506=PLANE('',#51802);
#11507=PLANE('',#51803);
#11508=PLANE('',#51804);
#11509=PLANE('',#51805);
#11510=PLANE('',#51806);
#11511=PLANE('',#51807);
#11512=PLANE('',#51809);
#11513=PLANE('',#51811);
#11514=PLANE('',#51813);
#11515=PLANE('',#51815);
#11516=PLANE('',#51817);
#11517=PLANE('',#51818);
#11518=PLANE('',#51820);
#11519=PLANE('',#51822);
#11520=PLANE('',#51824);
#11521=PLANE('',#51826);
#11522=PLANE('',#51828);
#11523=PLANE('',#51829);
#11524=PLANE('',#51843);
#11525=PLANE('',#51844);
#11526=PLANE('',#51845);
#11527=PLANE('',#51846);
#11528=PLANE('',#51847);
#11529=PLANE('',#51848);
#11530=PLANE('',#51849);
#11531=PLANE('',#51850);
#11532=PLANE('',#51851);
#11533=PLANE('',#51852);
#11534=PLANE('',#51853);
#11535=PLANE('',#51854);
#11536=PLANE('',#51855);
#11537=PLANE('',#51856);
#11538=PLANE('',#51857);
#11539=PLANE('',#51858);
#11540=PLANE('',#51860);
#11541=PLANE('',#51862);
#11542=PLANE('',#51864);
#11543=PLANE('',#51866);
#11544=PLANE('',#51868);
#11545=PLANE('',#51869);
#11546=PLANE('',#51871);
#11547=PLANE('',#51873);
#11548=PLANE('',#51875);
#11549=PLANE('',#51877);
#11550=PLANE('',#51879);
#11551=PLANE('',#51880);
#11552=PLANE('',#51894);
#11553=PLANE('',#51895);
#11554=PLANE('',#51896);
#11555=PLANE('',#51897);
#11556=PLANE('',#51898);
#11557=PLANE('',#51899);
#11558=PLANE('',#51900);
#11559=PLANE('',#51901);
#11560=PLANE('',#51902);
#11561=PLANE('',#51903);
#11562=PLANE('',#51904);
#11563=PLANE('',#51905);
#11564=PLANE('',#51906);
#11565=PLANE('',#51907);
#11566=PLANE('',#51908);
#11567=PLANE('',#51909);
#11568=PLANE('',#51911);
#11569=PLANE('',#51913);
#11570=PLANE('',#51915);
#11571=PLANE('',#51917);
#11572=PLANE('',#51919);
#11573=PLANE('',#51920);
#11574=PLANE('',#51922);
#11575=PLANE('',#51924);
#11576=PLANE('',#51926);
#11577=PLANE('',#51928);
#11578=PLANE('',#51930);
#11579=PLANE('',#51931);
#11580=PLANE('',#51945);
#11581=PLANE('',#51946);
#11582=PLANE('',#51947);
#11583=PLANE('',#51948);
#11584=PLANE('',#51949);
#11585=PLANE('',#51950);
#11586=PLANE('',#51951);
#11587=PLANE('',#51952);
#11588=PLANE('',#51953);
#11589=PLANE('',#51954);
#11590=PLANE('',#51955);
#11591=PLANE('',#51956);
#11592=PLANE('',#51957);
#11593=PLANE('',#51958);
#11594=PLANE('',#51959);
#11595=PLANE('',#51960);
#11596=PLANE('',#51962);
#11597=PLANE('',#51964);
#11598=PLANE('',#51966);
#11599=PLANE('',#51968);
#11600=PLANE('',#51970);
#11601=PLANE('',#51971);
#11602=PLANE('',#51973);
#11603=PLANE('',#51975);
#11604=PLANE('',#51977);
#11605=PLANE('',#51979);
#11606=PLANE('',#51981);
#11607=PLANE('',#51982);
#11608=PLANE('',#51996);
#11609=PLANE('',#51997);
#11610=PLANE('',#51998);
#11611=PLANE('',#51999);
#11612=PLANE('',#52000);
#11613=PLANE('',#52001);
#11614=PLANE('',#52002);
#11615=PLANE('',#52003);
#11616=PLANE('',#52004);
#11617=PLANE('',#52005);
#11618=PLANE('',#52006);
#11619=PLANE('',#52007);
#11620=PLANE('',#52008);
#11621=PLANE('',#52009);
#11622=PLANE('',#52010);
#11623=PLANE('',#52011);
#11624=PLANE('',#52013);
#11625=PLANE('',#52015);
#11626=PLANE('',#52017);
#11627=PLANE('',#52019);
#11628=PLANE('',#52021);
#11629=PLANE('',#52022);
#11630=PLANE('',#52024);
#11631=PLANE('',#52026);
#11632=PLANE('',#52028);
#11633=PLANE('',#52030);
#11634=PLANE('',#52032);
#11635=PLANE('',#52033);
#11636=PLANE('',#52047);
#11637=PLANE('',#52048);
#11638=PLANE('',#52049);
#11639=PLANE('',#52050);
#11640=PLANE('',#52051);
#11641=PLANE('',#52052);
#11642=PLANE('',#52053);
#11643=PLANE('',#52054);
#11644=PLANE('',#52055);
#11645=PLANE('',#52056);
#11646=PLANE('',#52057);
#11647=PLANE('',#52058);
#11648=PLANE('',#52059);
#11649=PLANE('',#52060);
#11650=PLANE('',#52061);
#11651=PLANE('',#52062);
#11652=PLANE('',#52064);
#11653=PLANE('',#52066);
#11654=PLANE('',#52068);
#11655=PLANE('',#52070);
#11656=PLANE('',#52072);
#11657=PLANE('',#52073);
#11658=PLANE('',#52075);
#11659=PLANE('',#52077);
#11660=PLANE('',#52079);
#11661=PLANE('',#52081);
#11662=PLANE('',#52083);
#11663=PLANE('',#52084);
#11664=PLANE('',#52098);
#11665=PLANE('',#52099);
#11666=PLANE('',#52100);
#11667=PLANE('',#52101);
#11668=PLANE('',#52102);
#11669=PLANE('',#52103);
#11670=PLANE('',#52104);
#11671=PLANE('',#52105);
#11672=PLANE('',#52106);
#11673=PLANE('',#52107);
#11674=PLANE('',#52108);
#11675=PLANE('',#52109);
#11676=PLANE('',#52110);
#11677=PLANE('',#52111);
#11678=PLANE('',#52112);
#11679=PLANE('',#52113);
#11680=PLANE('',#52115);
#11681=PLANE('',#52117);
#11682=PLANE('',#52119);
#11683=PLANE('',#52121);
#11684=PLANE('',#52123);
#11685=PLANE('',#52124);
#11686=PLANE('',#52126);
#11687=PLANE('',#52128);
#11688=PLANE('',#52130);
#11689=PLANE('',#52132);
#11690=PLANE('',#52134);
#11691=PLANE('',#52135);
#11692=PLANE('',#52149);
#11693=PLANE('',#52150);
#11694=PLANE('',#52151);
#11695=PLANE('',#52152);
#11696=PLANE('',#52153);
#11697=PLANE('',#52154);
#11698=PLANE('',#52155);
#11699=PLANE('',#52156);
#11700=PLANE('',#52157);
#11701=PLANE('',#52158);
#11702=PLANE('',#52159);
#11703=PLANE('',#52160);
#11704=PLANE('',#52161);
#11705=PLANE('',#52162);
#11706=PLANE('',#52163);
#11707=PLANE('',#52164);
#11708=PLANE('',#52166);
#11709=PLANE('',#52168);
#11710=PLANE('',#52170);
#11711=PLANE('',#52172);
#11712=PLANE('',#52174);
#11713=PLANE('',#52175);
#11714=PLANE('',#52177);
#11715=PLANE('',#52179);
#11716=PLANE('',#52181);
#11717=PLANE('',#52183);
#11718=PLANE('',#52185);
#11719=PLANE('',#52186);
#11720=PLANE('',#52200);
#11721=PLANE('',#52201);
#11722=PLANE('',#52202);
#11723=PLANE('',#52203);
#11724=PLANE('',#52204);
#11725=PLANE('',#52205);
#11726=PLANE('',#52206);
#11727=PLANE('',#52207);
#11728=PLANE('',#52208);
#11729=PLANE('',#52209);
#11730=PLANE('',#52210);
#11731=PLANE('',#52211);
#11732=PLANE('',#52212);
#11733=PLANE('',#52213);
#11734=PLANE('',#52214);
#11735=PLANE('',#52215);
#11736=PLANE('',#52217);
#11737=PLANE('',#52219);
#11738=PLANE('',#52221);
#11739=PLANE('',#52223);
#11740=PLANE('',#52225);
#11741=PLANE('',#52226);
#11742=PLANE('',#52228);
#11743=PLANE('',#52230);
#11744=PLANE('',#52232);
#11745=PLANE('',#52234);
#11746=PLANE('',#52236);
#11747=PLANE('',#52237);
#11748=PLANE('',#52251);
#11749=PLANE('',#52252);
#11750=PLANE('',#52253);
#11751=PLANE('',#52254);
#11752=PLANE('',#52255);
#11753=PLANE('',#52256);
#11754=PLANE('',#52257);
#11755=PLANE('',#52258);
#11756=PLANE('',#52259);
#11757=PLANE('',#52260);
#11758=PLANE('',#52261);
#11759=PLANE('',#52262);
#11760=PLANE('',#52263);
#11761=PLANE('',#52264);
#11762=PLANE('',#52265);
#11763=PLANE('',#52266);
#11764=PLANE('',#52268);
#11765=PLANE('',#52270);
#11766=PLANE('',#52272);
#11767=PLANE('',#52274);
#11768=PLANE('',#52276);
#11769=PLANE('',#52277);
#11770=PLANE('',#52279);
#11771=PLANE('',#52281);
#11772=PLANE('',#52283);
#11773=PLANE('',#52285);
#11774=PLANE('',#52287);
#11775=PLANE('',#52288);
#11776=PLANE('',#52302);
#11777=PLANE('',#52303);
#11778=PLANE('',#52304);
#11779=PLANE('',#52305);
#11780=PLANE('',#52306);
#11781=PLANE('',#52307);
#11782=PLANE('',#52308);
#11783=PLANE('',#52309);
#11784=PLANE('',#52310);
#11785=PLANE('',#52311);
#11786=PLANE('',#52312);
#11787=PLANE('',#52313);
#11788=PLANE('',#52314);
#11789=PLANE('',#52315);
#11790=PLANE('',#52316);
#11791=PLANE('',#52317);
#11792=PLANE('',#52319);
#11793=PLANE('',#52321);
#11794=PLANE('',#52323);
#11795=PLANE('',#52325);
#11796=PLANE('',#52327);
#11797=PLANE('',#52328);
#11798=PLANE('',#52330);
#11799=PLANE('',#52332);
#11800=PLANE('',#52334);
#11801=PLANE('',#52336);
#11802=PLANE('',#52338);
#11803=PLANE('',#52339);
#11804=PLANE('',#52353);
#11805=PLANE('',#52354);
#11806=PLANE('',#52355);
#11807=PLANE('',#52356);
#11808=PLANE('',#52357);
#11809=PLANE('',#52358);
#11810=PLANE('',#52359);
#11811=PLANE('',#52360);
#11812=PLANE('',#52361);
#11813=PLANE('',#52362);
#11814=PLANE('',#52363);
#11815=PLANE('',#52364);
#11816=PLANE('',#52365);
#11817=PLANE('',#52366);
#11818=PLANE('',#52367);
#11819=PLANE('',#52368);
#11820=PLANE('',#52370);
#11821=PLANE('',#52372);
#11822=PLANE('',#52374);
#11823=PLANE('',#52376);
#11824=PLANE('',#52378);
#11825=PLANE('',#52379);
#11826=PLANE('',#52381);
#11827=PLANE('',#52383);
#11828=PLANE('',#52385);
#11829=PLANE('',#52387);
#11830=PLANE('',#52389);
#11831=PLANE('',#52390);
#11832=PLANE('',#52404);
#11833=PLANE('',#52405);
#11834=PLANE('',#52406);
#11835=PLANE('',#52407);
#11836=PLANE('',#52408);
#11837=PLANE('',#52409);
#11838=PLANE('',#52410);
#11839=PLANE('',#52411);
#11840=PLANE('',#52412);
#11841=PLANE('',#52413);
#11842=PLANE('',#52414);
#11843=PLANE('',#52415);
#11844=PLANE('',#52416);
#11845=PLANE('',#52417);
#11846=PLANE('',#52418);
#11847=PLANE('',#52419);
#11848=PLANE('',#52421);
#11849=PLANE('',#52423);
#11850=PLANE('',#52425);
#11851=PLANE('',#52427);
#11852=PLANE('',#52429);
#11853=PLANE('',#52430);
#11854=PLANE('',#52432);
#11855=PLANE('',#52434);
#11856=PLANE('',#52436);
#11857=PLANE('',#52438);
#11858=PLANE('',#52440);
#11859=PLANE('',#52441);
#11860=PLANE('',#52455);
#11861=PLANE('',#52456);
#11862=PLANE('',#52457);
#11863=PLANE('',#52458);
#11864=PLANE('',#52459);
#11865=PLANE('',#52460);
#11866=PLANE('',#52461);
#11867=PLANE('',#52462);
#11868=PLANE('',#52463);
#11869=PLANE('',#52464);
#11870=PLANE('',#52465);
#11871=PLANE('',#52466);
#11872=PLANE('',#52467);
#11873=PLANE('',#52468);
#11874=PLANE('',#52469);
#11875=PLANE('',#52470);
#11876=PLANE('',#52472);
#11877=PLANE('',#52474);
#11878=PLANE('',#52476);
#11879=PLANE('',#52478);
#11880=PLANE('',#52480);
#11881=PLANE('',#52481);
#11882=PLANE('',#52483);
#11883=PLANE('',#52485);
#11884=PLANE('',#52487);
#11885=PLANE('',#52489);
#11886=PLANE('',#52491);
#11887=PLANE('',#52492);
#11888=PLANE('',#52506);
#11889=PLANE('',#52507);
#11890=PLANE('',#52508);
#11891=PLANE('',#52509);
#11892=PLANE('',#52510);
#11893=PLANE('',#52511);
#11894=PLANE('',#52512);
#11895=PLANE('',#52513);
#11896=PLANE('',#52514);
#11897=PLANE('',#52515);
#11898=PLANE('',#52516);
#11899=PLANE('',#52517);
#11900=PLANE('',#52518);
#11901=PLANE('',#52519);
#11902=PLANE('',#52520);
#11903=PLANE('',#52521);
#11904=PLANE('',#52523);
#11905=PLANE('',#52525);
#11906=PLANE('',#52527);
#11907=PLANE('',#52529);
#11908=PLANE('',#52531);
#11909=PLANE('',#52532);
#11910=PLANE('',#52534);
#11911=PLANE('',#52536);
#11912=PLANE('',#52538);
#11913=PLANE('',#52540);
#11914=PLANE('',#52542);
#11915=PLANE('',#52543);
#11916=PLANE('',#52557);
#11917=PLANE('',#52558);
#11918=PLANE('',#52559);
#11919=PLANE('',#52560);
#11920=PLANE('',#52561);
#11921=PLANE('',#52562);
#11922=PLANE('',#52563);
#11923=PLANE('',#52564);
#11924=PLANE('',#52565);
#11925=PLANE('',#52566);
#11926=PLANE('',#52567);
#11927=PLANE('',#52568);
#11928=PLANE('',#52569);
#11929=PLANE('',#52570);
#11930=PLANE('',#52571);
#11931=PLANE('',#52572);
#11932=PLANE('',#52574);
#11933=PLANE('',#52576);
#11934=PLANE('',#52578);
#11935=PLANE('',#52580);
#11936=PLANE('',#52582);
#11937=PLANE('',#52583);
#11938=PLANE('',#52585);
#11939=PLANE('',#52587);
#11940=PLANE('',#52589);
#11941=PLANE('',#52591);
#11942=PLANE('',#52593);
#11943=PLANE('',#52594);
#11944=PLANE('',#52608);
#11945=PLANE('',#52609);
#11946=PLANE('',#52610);
#11947=PLANE('',#52611);
#11948=PLANE('',#52612);
#11949=PLANE('',#52613);
#11950=PLANE('',#52614);
#11951=PLANE('',#52615);
#11952=PLANE('',#52616);
#11953=PLANE('',#52617);
#11954=PLANE('',#52618);
#11955=PLANE('',#52619);
#11956=PLANE('',#52620);
#11957=PLANE('',#52621);
#11958=PLANE('',#52622);
#11959=PLANE('',#52623);
#11960=PLANE('',#52625);
#11961=PLANE('',#52627);
#11962=PLANE('',#52629);
#11963=PLANE('',#52631);
#11964=PLANE('',#52633);
#11965=PLANE('',#52634);
#11966=PLANE('',#52636);
#11967=PLANE('',#52638);
#11968=PLANE('',#52640);
#11969=PLANE('',#52642);
#11970=PLANE('',#52644);
#11971=PLANE('',#52645);
#11972=PLANE('',#52659);
#11973=PLANE('',#52660);
#11974=PLANE('',#52661);
#11975=PLANE('',#52662);
#11976=PLANE('',#52663);
#11977=PLANE('',#52664);
#11978=PLANE('',#52665);
#11979=PLANE('',#52666);
#11980=PLANE('',#52667);
#11981=PLANE('',#52668);
#11982=PLANE('',#52669);
#11983=PLANE('',#52670);
#11984=PLANE('',#52671);
#11985=PLANE('',#52672);
#11986=PLANE('',#52673);
#11987=PLANE('',#52674);
#11988=PLANE('',#52676);
#11989=PLANE('',#52678);
#11990=PLANE('',#52680);
#11991=PLANE('',#52682);
#11992=PLANE('',#52684);
#11993=PLANE('',#52685);
#11994=PLANE('',#52687);
#11995=PLANE('',#52689);
#11996=PLANE('',#52691);
#11997=PLANE('',#52693);
#11998=PLANE('',#52695);
#11999=PLANE('',#52696);
#12000=PLANE('',#52710);
#12001=PLANE('',#52711);
#12002=PLANE('',#52712);
#12003=PLANE('',#52713);
#12004=PLANE('',#52714);
#12005=PLANE('',#52715);
#12006=PLANE('',#52716);
#12007=PLANE('',#52717);
#12008=PLANE('',#52718);
#12009=PLANE('',#52719);
#12010=PLANE('',#52720);
#12011=PLANE('',#52721);
#12012=PLANE('',#52722);
#12013=PLANE('',#52723);
#12014=PLANE('',#52724);
#12015=PLANE('',#52725);
#12016=PLANE('',#52727);
#12017=PLANE('',#52729);
#12018=PLANE('',#52731);
#12019=PLANE('',#52733);
#12020=PLANE('',#52735);
#12021=PLANE('',#52736);
#12022=PLANE('',#52738);
#12023=PLANE('',#52740);
#12024=PLANE('',#52742);
#12025=PLANE('',#52744);
#12026=PLANE('',#52746);
#12027=PLANE('',#52747);
#12028=PLANE('',#52761);
#12029=PLANE('',#52762);
#12030=PLANE('',#52763);
#12031=PLANE('',#52764);
#12032=PLANE('',#52765);
#12033=PLANE('',#52766);
#12034=PLANE('',#52767);
#12035=PLANE('',#52768);
#12036=PLANE('',#52769);
#12037=PLANE('',#52770);
#12038=PLANE('',#52771);
#12039=PLANE('',#52772);
#12040=PLANE('',#52773);
#12041=PLANE('',#52774);
#12042=PLANE('',#52775);
#12043=PLANE('',#52776);
#12044=PLANE('',#52778);
#12045=PLANE('',#52780);
#12046=PLANE('',#52782);
#12047=PLANE('',#52784);
#12048=PLANE('',#52786);
#12049=PLANE('',#52787);
#12050=PLANE('',#52789);
#12051=PLANE('',#52791);
#12052=PLANE('',#52793);
#12053=PLANE('',#52795);
#12054=PLANE('',#52797);
#12055=PLANE('',#52798);
#12056=PLANE('',#52812);
#12057=PLANE('',#52813);
#12058=PLANE('',#52814);
#12059=PLANE('',#52815);
#12060=PLANE('',#52816);
#12061=PLANE('',#52817);
#12062=PLANE('',#52818);
#12063=PLANE('',#52819);
#12064=PLANE('',#52820);
#12065=PLANE('',#52821);
#12066=PLANE('',#52822);
#12067=PLANE('',#52823);
#12068=PLANE('',#52824);
#12069=PLANE('',#52825);
#12070=PLANE('',#52826);
#12071=PLANE('',#52827);
#12072=PLANE('',#52829);
#12073=PLANE('',#52831);
#12074=PLANE('',#52833);
#12075=PLANE('',#52835);
#12076=PLANE('',#52837);
#12077=PLANE('',#52838);
#12078=PLANE('',#52840);
#12079=PLANE('',#52842);
#12080=PLANE('',#52844);
#12081=PLANE('',#52846);
#12082=PLANE('',#52848);
#12083=PLANE('',#52849);
#12084=PLANE('',#52863);
#12085=PLANE('',#52864);
#12086=PLANE('',#52865);
#12087=PLANE('',#52866);
#12088=PLANE('',#52867);
#12089=PLANE('',#52868);
#12090=PLANE('',#52869);
#12091=PLANE('',#52870);
#12092=PLANE('',#52871);
#12093=PLANE('',#52872);
#12094=PLANE('',#52873);
#12095=PLANE('',#52874);
#12096=PLANE('',#52875);
#12097=PLANE('',#52876);
#12098=PLANE('',#52877);
#12099=PLANE('',#52878);
#12100=PLANE('',#52880);
#12101=PLANE('',#52882);
#12102=PLANE('',#52884);
#12103=PLANE('',#52886);
#12104=PLANE('',#52888);
#12105=PLANE('',#52889);
#12106=PLANE('',#52891);
#12107=PLANE('',#52893);
#12108=PLANE('',#52895);
#12109=PLANE('',#52897);
#12110=PLANE('',#52899);
#12111=PLANE('',#52900);
#12112=PLANE('',#52914);
#12113=PLANE('',#52915);
#12114=PLANE('',#52916);
#12115=PLANE('',#52917);
#12116=PLANE('',#52918);
#12117=PLANE('',#52919);
#12118=PLANE('',#52920);
#12119=PLANE('',#52921);
#12120=PLANE('',#52922);
#12121=PLANE('',#52923);
#12122=PLANE('',#52924);
#12123=PLANE('',#52925);
#12124=PLANE('',#52926);
#12125=PLANE('',#52927);
#12126=PLANE('',#52928);
#12127=PLANE('',#52929);
#12128=PLANE('',#52931);
#12129=PLANE('',#52933);
#12130=PLANE('',#52935);
#12131=PLANE('',#52937);
#12132=PLANE('',#52939);
#12133=PLANE('',#52940);
#12134=PLANE('',#52942);
#12135=PLANE('',#52944);
#12136=PLANE('',#52946);
#12137=PLANE('',#52948);
#12138=PLANE('',#52950);
#12139=PLANE('',#52951);
#12140=PLANE('',#52965);
#12141=PLANE('',#52966);
#12142=PLANE('',#52967);
#12143=PLANE('',#52968);
#12144=PLANE('',#52969);
#12145=PLANE('',#52970);
#12146=PLANE('',#52971);
#12147=PLANE('',#52972);
#12148=PLANE('',#52973);
#12149=PLANE('',#52974);
#12150=PLANE('',#52975);
#12151=PLANE('',#52976);
#12152=PLANE('',#52977);
#12153=PLANE('',#52978);
#12154=PLANE('',#52979);
#12155=PLANE('',#52980);
#12156=PLANE('',#52982);
#12157=PLANE('',#52984);
#12158=PLANE('',#52986);
#12159=PLANE('',#52988);
#12160=PLANE('',#52990);
#12161=PLANE('',#52991);
#12162=PLANE('',#52993);
#12163=PLANE('',#52995);
#12164=PLANE('',#52997);
#12165=PLANE('',#52999);
#12166=PLANE('',#53001);
#12167=PLANE('',#53002);
#12168=PLANE('',#53016);
#12169=PLANE('',#53017);
#12170=PLANE('',#53018);
#12171=PLANE('',#53019);
#12172=PLANE('',#53020);
#12173=PLANE('',#53021);
#12174=PLANE('',#53022);
#12175=PLANE('',#53023);
#12176=PLANE('',#53024);
#12177=PLANE('',#53025);
#12178=PLANE('',#53026);
#12179=PLANE('',#53027);
#12180=PLANE('',#53028);
#12181=PLANE('',#53029);
#12182=PLANE('',#53030);
#12183=PLANE('',#53031);
#12184=PLANE('',#53033);
#12185=PLANE('',#53035);
#12186=PLANE('',#53037);
#12187=PLANE('',#53039);
#12188=PLANE('',#53041);
#12189=PLANE('',#53042);
#12190=PLANE('',#53044);
#12191=PLANE('',#53046);
#12192=PLANE('',#53048);
#12193=PLANE('',#53050);
#12194=PLANE('',#53052);
#12195=PLANE('',#53053);
#12196=PLANE('',#53067);
#12197=PLANE('',#53068);
#12198=PLANE('',#53069);
#12199=PLANE('',#53070);
#12200=PLANE('',#53071);
#12201=PLANE('',#53072);
#12202=PLANE('',#53073);
#12203=PLANE('',#53074);
#12204=PLANE('',#53075);
#12205=PLANE('',#53076);
#12206=PLANE('',#53077);
#12207=PLANE('',#53078);
#12208=PLANE('',#53079);
#12209=PLANE('',#53080);
#12210=PLANE('',#53081);
#12211=PLANE('',#53082);
#12212=PLANE('',#53084);
#12213=PLANE('',#53086);
#12214=PLANE('',#53088);
#12215=PLANE('',#53090);
#12216=PLANE('',#53092);
#12217=PLANE('',#53093);
#12218=PLANE('',#53095);
#12219=PLANE('',#53097);
#12220=PLANE('',#53099);
#12221=PLANE('',#53101);
#12222=PLANE('',#53103);
#12223=PLANE('',#53104);
#12224=PLANE('',#53118);
#12225=PLANE('',#53119);
#12226=PLANE('',#53120);
#12227=PLANE('',#53121);
#12228=PLANE('',#53122);
#12229=PLANE('',#53123);
#12230=PLANE('',#53124);
#12231=PLANE('',#53125);
#12232=PLANE('',#53126);
#12233=PLANE('',#53127);
#12234=PLANE('',#53128);
#12235=PLANE('',#53129);
#12236=PLANE('',#53130);
#12237=PLANE('',#53131);
#12238=PLANE('',#53132);
#12239=PLANE('',#53133);
#12240=PLANE('',#53135);
#12241=PLANE('',#53137);
#12242=PLANE('',#53139);
#12243=PLANE('',#53141);
#12244=PLANE('',#53143);
#12245=PLANE('',#53144);
#12246=PLANE('',#53146);
#12247=PLANE('',#53148);
#12248=PLANE('',#53150);
#12249=PLANE('',#53152);
#12250=PLANE('',#53154);
#12251=PLANE('',#53155);
#12252=PLANE('',#53169);
#12253=PLANE('',#53170);
#12254=PLANE('',#53171);
#12255=PLANE('',#53172);
#12256=PLANE('',#53173);
#12257=PLANE('',#53174);
#12258=PLANE('',#53175);
#12259=PLANE('',#53176);
#12260=PLANE('',#53177);
#12261=PLANE('',#53178);
#12262=PLANE('',#53179);
#12263=PLANE('',#53180);
#12264=PLANE('',#53181);
#12265=PLANE('',#53182);
#12266=PLANE('',#53183);
#12267=PLANE('',#53184);
#12268=PLANE('',#53186);
#12269=PLANE('',#53188);
#12270=PLANE('',#53190);
#12271=PLANE('',#53192);
#12272=PLANE('',#53194);
#12273=PLANE('',#53195);
#12274=PLANE('',#53197);
#12275=PLANE('',#53199);
#12276=PLANE('',#53201);
#12277=PLANE('',#53203);
#12278=PLANE('',#53205);
#12279=PLANE('',#53206);
#12280=PLANE('',#53220);
#12281=PLANE('',#53221);
#12282=PLANE('',#53222);
#12283=PLANE('',#53223);
#12284=PLANE('',#53224);
#12285=PLANE('',#53225);
#12286=PLANE('',#53226);
#12287=PLANE('',#53227);
#12288=PLANE('',#53228);
#12289=PLANE('',#53229);
#12290=PLANE('',#53230);
#12291=PLANE('',#53231);
#12292=PLANE('',#53232);
#12293=PLANE('',#53233);
#12294=PLANE('',#53234);
#12295=PLANE('',#53235);
#12296=PLANE('',#53237);
#12297=PLANE('',#53239);
#12298=PLANE('',#53241);
#12299=PLANE('',#53243);
#12300=PLANE('',#53245);
#12301=PLANE('',#53246);
#12302=PLANE('',#53248);
#12303=PLANE('',#53250);
#12304=PLANE('',#53252);
#12305=PLANE('',#53254);
#12306=PLANE('',#53256);
#12307=PLANE('',#53257);
#12308=PLANE('',#53271);
#12309=PLANE('',#53272);
#12310=PLANE('',#53273);
#12311=PLANE('',#53274);
#12312=PLANE('',#53275);
#12313=PLANE('',#53276);
#12314=PLANE('',#53277);
#12315=PLANE('',#53278);
#12316=PLANE('',#53279);
#12317=PLANE('',#53280);
#12318=PLANE('',#53281);
#12319=PLANE('',#53282);
#12320=PLANE('',#53283);
#12321=PLANE('',#53284);
#12322=PLANE('',#53285);
#12323=PLANE('',#53286);
#12324=PLANE('',#53288);
#12325=PLANE('',#53290);
#12326=PLANE('',#53292);
#12327=PLANE('',#53294);
#12328=PLANE('',#53296);
#12329=PLANE('',#53297);
#12330=PLANE('',#53299);
#12331=PLANE('',#53301);
#12332=PLANE('',#53303);
#12333=PLANE('',#53305);
#12334=PLANE('',#53307);
#12335=PLANE('',#53308);
#12336=PLANE('',#53322);
#12337=PLANE('',#53323);
#12338=PLANE('',#53324);
#12339=PLANE('',#53325);
#12340=PLANE('',#53326);
#12341=PLANE('',#53327);
#12342=PLANE('',#53328);
#12343=PLANE('',#53329);
#12344=PLANE('',#53330);
#12345=PLANE('',#53331);
#12346=PLANE('',#53332);
#12347=PLANE('',#53333);
#12348=PLANE('',#53334);
#12349=PLANE('',#53335);
#12350=PLANE('',#53336);
#12351=PLANE('',#53337);
#12352=PLANE('',#53339);
#12353=PLANE('',#53341);
#12354=PLANE('',#53343);
#12355=PLANE('',#53345);
#12356=PLANE('',#53347);
#12357=PLANE('',#53348);
#12358=PLANE('',#53350);
#12359=PLANE('',#53352);
#12360=PLANE('',#53354);
#12361=PLANE('',#53356);
#12362=PLANE('',#53358);
#12363=PLANE('',#53359);
#12364=PLANE('',#53373);
#12365=PLANE('',#53374);
#12366=PLANE('',#53375);
#12367=PLANE('',#53376);
#12368=PLANE('',#53377);
#12369=PLANE('',#53378);
#12370=PLANE('',#53379);
#12371=PLANE('',#53380);
#12372=PLANE('',#53381);
#12373=PLANE('',#53382);
#12374=PLANE('',#53383);
#12375=PLANE('',#53384);
#12376=PLANE('',#53385);
#12377=PLANE('',#53386);
#12378=PLANE('',#53387);
#12379=PLANE('',#53388);
#12380=PLANE('',#53390);
#12381=PLANE('',#53392);
#12382=PLANE('',#53394);
#12383=PLANE('',#53396);
#12384=PLANE('',#53398);
#12385=PLANE('',#53399);
#12386=PLANE('',#53401);
#12387=PLANE('',#53403);
#12388=PLANE('',#53405);
#12389=PLANE('',#53407);
#12390=PLANE('',#53409);
#12391=PLANE('',#53410);
#12392=PLANE('',#53424);
#12393=PLANE('',#53425);
#12394=PLANE('',#53426);
#12395=PLANE('',#53427);
#12396=PLANE('',#53428);
#12397=PLANE('',#53429);
#12398=PLANE('',#53430);
#12399=PLANE('',#53431);
#12400=PLANE('',#53432);
#12401=PLANE('',#53433);
#12402=PLANE('',#53434);
#12403=PLANE('',#53435);
#12404=PLANE('',#53436);
#12405=PLANE('',#53437);
#12406=PLANE('',#53438);
#12407=PLANE('',#53439);
#12408=PLANE('',#53441);
#12409=PLANE('',#53443);
#12410=PLANE('',#53445);
#12411=PLANE('',#53447);
#12412=PLANE('',#53449);
#12413=PLANE('',#53450);
#12414=PLANE('',#53452);
#12415=PLANE('',#53454);
#12416=PLANE('',#53456);
#12417=PLANE('',#53458);
#12418=PLANE('',#53460);
#12419=PLANE('',#53461);
#12420=PLANE('',#53475);
#12421=PLANE('',#53476);
#12422=PLANE('',#53477);
#12423=PLANE('',#53478);
#12424=PLANE('',#53479);
#12425=PLANE('',#53480);
#12426=PLANE('',#53481);
#12427=PLANE('',#53482);
#12428=PLANE('',#53483);
#12429=PLANE('',#53484);
#12430=PLANE('',#53485);
#12431=PLANE('',#53486);
#12432=PLANE('',#53487);
#12433=PLANE('',#53488);
#12434=PLANE('',#53489);
#12435=PLANE('',#53490);
#12436=PLANE('',#53492);
#12437=PLANE('',#53494);
#12438=PLANE('',#53496);
#12439=PLANE('',#53498);
#12440=PLANE('',#53500);
#12441=PLANE('',#53501);
#12442=PLANE('',#53503);
#12443=PLANE('',#53505);
#12444=PLANE('',#53507);
#12445=PLANE('',#53509);
#12446=PLANE('',#53511);
#12447=PLANE('',#53512);
#12448=PLANE('',#53526);
#12449=PLANE('',#53527);
#12450=PLANE('',#53529);
#12451=PLANE('',#53531);
#12452=PLANE('',#53533);
#12453=PLANE('',#53535);
#12454=PLANE('',#53537);
#12455=PLANE('',#53538);
#12456=PLANE('',#53540);
#12457=PLANE('',#53542);
#12458=PLANE('',#53544);
#12459=PLANE('',#53546);
#12460=PLANE('',#53548);
#12461=PLANE('',#53549);
#12462=PLANE('',#53551);
#12463=PLANE('',#53552);
#12464=PLANE('',#53553);
#12465=PLANE('',#53554);
#12466=PLANE('',#53555);
#12467=PLANE('',#53556);
#12468=PLANE('',#53557);
#12469=PLANE('',#53558);
#12470=PLANE('',#53559);
#12471=PLANE('',#53560);
#12472=PLANE('',#53561);
#12473=PLANE('',#53562);
#12474=PLANE('',#53563);
#12475=PLANE('',#53564);
#12476=PLANE('',#53575);
#12477=PLANE('',#53590);
#12478=PLANE('',#53595);
#12479=PLANE('',#53598);
#12480=PLANE('',#53609);
#12481=PLANE('',#53610);
#12482=PLANE('',#53611);
#12483=PLANE('',#53629);
#12484=PLANE('',#53659);
#12485=PLANE('',#53660);
#12486=PLANE('',#53661);
#12487=PLANE('',#53703);
#12488=PLANE('',#53704);
#12489=PLANE('',#53705);
#12490=PLANE('',#53773);
#12491=PLANE('',#53774);
#12492=PLANE('',#53775);
#12493=PLANE('',#53776);
#12494=PLANE('',#53777);
#12495=PLANE('',#53778);
#12496=PLANE('',#53779);
#12497=PLANE('',#53780);
#12498=PLANE('',#53781);
#12499=PLANE('',#53782);
#12500=PLANE('',#53783);
#12501=PLANE('',#53784);
#12502=PLANE('',#53785);
#12503=PLANE('',#53786);
#12504=PLANE('',#53787);
#12505=PLANE('',#53788);
#12506=PLANE('',#53789);
#12507=PLANE('',#53790);
#12508=PLANE('',#53791);
#12509=PLANE('',#53792);
#12510=PLANE('',#53793);
#12511=PLANE('',#53794);
#12512=PLANE('',#53795);
#12513=PLANE('',#53796);
#12514=PLANE('',#53797);
#12515=PLANE('',#53798);
#12516=PLANE('',#53799);
#12517=PLANE('',#53800);
#12518=PLANE('',#53801);
#12519=PLANE('',#53802);
#12520=PLANE('',#53803);
#12521=PLANE('',#53804);
#12522=PLANE('',#53805);
#12523=PLANE('',#53806);
#12524=PLANE('',#53807);
#12525=PLANE('',#53808);
#12526=PLANE('',#53809);
#12527=PLANE('',#53810);
#12528=PLANE('',#53811);
#12529=PLANE('',#53812);
#12530=PLANE('',#53813);
#12531=PLANE('',#53814);
#12532=PLANE('',#53815);
#12533=PLANE('',#53816);
#12534=PLANE('',#53817);
#12535=PLANE('',#53818);
#12536=PLANE('',#53819);
#12537=PLANE('',#53820);
#12538=PLANE('',#53821);
#12539=PLANE('',#53822);
#12540=PLANE('',#53823);
#12541=PLANE('',#53824);
#12542=PLANE('',#53825);
#12543=PLANE('',#53826);
#12544=PLANE('',#53827);
#12545=PLANE('',#53828);
#12546=PLANE('',#53829);
#12547=PLANE('',#53830);
#12548=PLANE('',#53831);
#12549=PLANE('',#53832);
#12550=PLANE('',#53833);
#12551=PLANE('',#53834);
#12552=PLANE('',#53835);
#12553=PLANE('',#53836);
#12554=PLANE('',#53837);
#12555=PLANE('',#53838);
#12556=PLANE('',#53905);
#12557=PLANE('',#53906);
#12558=PLANE('',#53907);
#12559=PLANE('',#53908);
#12560=PLANE('',#53909);
#12561=PLANE('',#53910);
#12562=PLANE('',#53911);
#12563=PLANE('',#53912);
#12564=PLANE('',#53913);
#12565=PLANE('',#53914);
#12566=PLANE('',#53915);
#12567=PLANE('',#53916);
#12568=PLANE('',#53917);
#12569=PLANE('',#53918);
#12570=PLANE('',#53919);
#12571=PLANE('',#53920);
#12572=PLANE('',#53921);
#12573=PLANE('',#53922);
#12574=PLANE('',#53923);
#12575=PLANE('',#53924);
#12576=PLANE('',#53925);
#12577=PLANE('',#53926);
#12578=PLANE('',#53927);
#12579=PLANE('',#53928);
#12580=PLANE('',#53929);
#12581=PLANE('',#53930);
#12582=PLANE('',#53931);
#12583=PLANE('',#53932);
#12584=PLANE('',#53933);
#12585=PLANE('',#53934);
#12586=PLANE('',#53935);
#12587=PLANE('',#53936);
#12588=PLANE('',#53937);
#12589=PLANE('',#53938);
#12590=PLANE('',#53939);
#12591=PLANE('',#53940);
#12592=PLANE('',#53941);
#12593=PLANE('',#53944);
#12594=PLANE('',#53945);
#12595=PLANE('',#53946);
#12596=PLANE('',#53947);
#12597=PLANE('',#53949);
#12598=PLANE('',#53950);
#12599=PLANE('',#53951);
#12600=PLANE('',#53952);
#12601=PLANE('',#53954);
#12602=PLANE('',#53955);
#12603=PLANE('',#53956);
#12604=PLANE('',#53957);
#12605=PLANE('',#53959);
#12606=PLANE('',#53960);
#12607=PLANE('',#53961);
#12608=PLANE('',#53962);
#12609=PLANE('',#53964);
#12610=PLANE('',#53965);
#12611=PLANE('',#53966);
#12612=PLANE('',#53967);
#12613=PLANE('',#53969);
#12614=PLANE('',#53970);
#12615=PLANE('',#53971);
#12616=PLANE('',#53972);
#12617=PLANE('',#53974);
#12618=PLANE('',#53975);
#12619=PLANE('',#53976);
#12620=PLANE('',#53977);
#12621=PLANE('',#53979);
#12622=PLANE('',#53980);
#12623=PLANE('',#53981);
#12624=PLANE('',#53982);
#12625=PLANE('',#53984);
#12626=PLANE('',#53985);
#12627=PLANE('',#53986);
#12628=PLANE('',#53987);
#12629=PLANE('',#53989);
#12630=PLANE('',#53990);
#12631=PLANE('',#53991);
#12632=PLANE('',#53992);
#12633=PLANE('',#53994);
#12634=PLANE('',#53995);
#12635=PLANE('',#53996);
#12636=PLANE('',#53997);
#12637=PLANE('',#53999);
#12638=PLANE('',#54000);
#12639=PLANE('',#54001);
#12640=PLANE('',#54002);
#12641=PLANE('',#54004);
#12642=PLANE('',#54005);
#12643=PLANE('',#54006);
#12644=PLANE('',#54007);
#12645=PLANE('',#54009);
#12646=PLANE('',#54010);
#12647=PLANE('',#54011);
#12648=PLANE('',#54012);
#12649=PLANE('',#54014);
#12650=PLANE('',#54015);
#12651=PLANE('',#54016);
#12652=PLANE('',#54017);
#12653=PLANE('',#54019);
#12654=PLANE('',#54020);
#12655=PLANE('',#54021);
#12656=PLANE('',#54022);
#12657=PLANE('',#54024);
#12658=PLANE('',#54025);
#12659=PLANE('',#54026);
#12660=PLANE('',#54027);
#12661=PLANE('',#54029);
#12662=PLANE('',#54030);
#12663=PLANE('',#54031);
#12664=PLANE('',#54032);
#12665=PLANE('',#54034);
#12666=PLANE('',#54035);
#12667=PLANE('',#54036);
#12668=PLANE('',#54037);
#12669=PLANE('',#54039);
#12670=PLANE('',#54040);
#12671=PLANE('',#54041);
#12672=PLANE('',#54042);
#12673=PLANE('',#54044);
#12674=PLANE('',#54045);
#12675=PLANE('',#54046);
#12676=PLANE('',#54047);
#12677=PLANE('',#54049);
#12678=PLANE('',#54050);
#12679=PLANE('',#54051);
#12680=PLANE('',#54052);
#12681=PLANE('',#54054);
#12682=PLANE('',#54055);
#12683=PLANE('',#54056);
#12684=PLANE('',#54057);
#12685=PLANE('',#54059);
#12686=PLANE('',#54060);
#12687=PLANE('',#54061);
#12688=PLANE('',#54062);
#12689=PLANE('',#54064);
#12690=PLANE('',#54065);
#12691=PLANE('',#54066);
#12692=PLANE('',#54067);
#12693=PLANE('',#54069);
#12694=PLANE('',#54070);
#12695=PLANE('',#54071);
#12696=PLANE('',#54072);
#12697=PLANE('',#54074);
#12698=PLANE('',#54075);
#12699=PLANE('',#54076);
#12700=PLANE('',#54077);
#12701=PLANE('',#54079);
#12702=PLANE('',#54080);
#12703=PLANE('',#54081);
#12704=PLANE('',#54082);
#12705=PLANE('',#54084);
#12706=PLANE('',#54085);
#12707=PLANE('',#54086);
#12708=PLANE('',#54087);
#12709=PLANE('',#54089);
#12710=PLANE('',#54090);
#12711=PLANE('',#54091);
#12712=PLANE('',#54092);
#12713=PLANE('',#54094);
#12714=PLANE('',#54095);
#12715=PLANE('',#54096);
#12716=PLANE('',#54097);
#12717=PLANE('',#54099);
#12718=PLANE('',#54100);
#12719=PLANE('',#54101);
#12720=PLANE('',#54102);
#12721=PLANE('',#54108);
#12722=PLANE('',#54117);
#12723=PLANE('',#54137);
#12724=PLANE('',#54138);
#12725=PLANE('',#54139);
#12726=PLANE('',#54146);
#12727=PLANE('',#54174);
#12728=PLANE('',#54177);
#12729=PLANE('',#54180);
#12730=PLANE('',#54183);
#12731=PLANE('',#54196);
#12732=PLANE('',#54202);
#12733=PLANE('',#54209);
#12734=PLANE('',#54215);
#12735=PLANE('',#54217);
#12736=PLANE('',#54218);
#12737=PLANE('',#54219);
#12738=PLANE('',#54220);
#12739=PLANE('',#54221);
#12740=PLANE('',#54222);
#12741=PLANE('',#54223);
#12742=PLANE('',#54224);
#12743=PLANE('',#54225);
#12744=PLANE('',#54226);
#12745=PLANE('',#54227);
#12746=PLANE('',#54228);
#12747=PLANE('',#54229);
#12748=PLANE('',#54230);
#12749=PLANE('',#54231);
#12750=PLANE('',#54232);
#12751=PLANE('',#54233);
#12752=PLANE('',#54234);
#12753=PLANE('',#54235);
#12754=PLANE('',#54236);
#12755=PLANE('',#54237);
#12756=PLANE('',#54238);
#12757=PLANE('',#54239);
#12758=PLANE('',#54240);
#12759=PLANE('',#54241);
#12760=PLANE('',#54242);
#12761=PLANE('',#54243);
#12762=PLANE('',#54244);
#12763=PLANE('',#54245);
#12764=PLANE('',#54246);
#12765=PLANE('',#54247);
#12766=PLANE('',#54248);
#12767=PLANE('',#54249);
#12768=PLANE('',#54250);
#12769=PLANE('',#54251);
#12770=PLANE('',#54252);
#12771=PLANE('',#54253);
#12772=PLANE('',#54254);
#12773=PLANE('',#54255);
#12774=PLANE('',#54256);
#12775=PLANE('',#54257);
#12776=PLANE('',#54258);
#12777=PLANE('',#54259);
#12778=PLANE('',#54260);
#12779=PLANE('',#54261);
#12780=PLANE('',#54262);
#12781=PLANE('',#54263);
#12782=PLANE('',#54264);
#12783=PLANE('',#54265);
#12784=PLANE('',#54266);
#12785=PLANE('',#54267);
#12786=PLANE('',#54268);
#12787=PLANE('',#54269);
#12788=PLANE('',#54270);
#12789=PLANE('',#54271);
#12790=PLANE('',#54272);
#12791=PLANE('',#54273);
#12792=PLANE('',#54274);
#12793=PLANE('',#54275);
#12794=PLANE('',#54276);
#12795=PLANE('',#54277);
#12796=PLANE('',#54278);
#12797=PLANE('',#54279);
#12798=PLANE('',#54280);
#12799=PLANE('',#54281);
#12800=PLANE('',#54282);
#12801=PLANE('',#54283);
#12802=PLANE('',#54284);
#12803=PLANE('',#54285);
#12804=PLANE('',#54286);
#12805=PLANE('',#54287);
#12806=PLANE('',#54288);
#12807=PLANE('',#54289);
#12808=PLANE('',#54290);
#12809=PLANE('',#54291);
#12810=PLANE('',#54292);
#12811=PLANE('',#54293);
#12812=PLANE('',#54294);
#12813=PLANE('',#54295);
#12814=PLANE('',#54296);
#12815=PLANE('',#54297);
#12816=PLANE('',#54298);
#12817=PLANE('',#54299);
#12818=PLANE('',#54300);
#12819=PLANE('',#54301);
#12820=PLANE('',#54302);
#12821=PLANE('',#54303);
#12822=PLANE('',#54304);
#12823=PLANE('',#54305);
#12824=PLANE('',#54306);
#12825=PLANE('',#54307);
#12826=PLANE('',#54308);
#12827=PLANE('',#54309);
#12828=PLANE('',#54310);
#12829=PLANE('',#54311);
#12830=PLANE('',#54312);
#12831=PLANE('',#54313);
#12832=PLANE('',#54314);
#12833=PLANE('',#54315);
#12834=PLANE('',#54316);
#12835=PLANE('',#54317);
#12836=PLANE('',#54318);
#12837=PLANE('',#54319);
#12838=PLANE('',#54320);
#12839=PLANE('',#54321);
#12840=PLANE('',#54322);
#12841=PLANE('',#54323);
#12842=PLANE('',#54324);
#12843=PLANE('',#54325);
#12844=PLANE('',#54326);
#12845=PLANE('',#54327);
#12846=PLANE('',#54328);
#12847=PLANE('',#54329);
#12848=PLANE('',#54330);
#12849=PLANE('',#54331);
#12850=PLANE('',#54332);
#12851=PLANE('',#54333);
#12852=PLANE('',#54334);
#12853=PLANE('',#54335);
#12854=PLANE('',#54336);
#12855=PLANE('',#54337);
#12856=PLANE('',#54338);
#12857=PLANE('',#54339);
#12858=PLANE('',#54340);
#12859=PLANE('',#54341);
#12860=PLANE('',#54342);
#12861=PLANE('',#54343);
#12862=PLANE('',#54344);
#12863=PLANE('',#54345);
#12864=PLANE('',#54346);
#12865=PLANE('',#54347);
#12866=PLANE('',#54348);
#12867=PLANE('',#54349);
#12868=PLANE('',#54350);
#12869=PLANE('',#54351);
#12870=PLANE('',#54352);
#12871=PLANE('',#54353);
#12872=PLANE('',#54354);
#12873=PLANE('',#54355);
#12874=PLANE('',#54356);
#12875=PLANE('',#54357);
#12876=PLANE('',#54358);
#12877=PLANE('',#54359);
#12878=PLANE('',#54360);
#12879=PLANE('',#54361);
#12880=PLANE('',#54362);
#12881=PLANE('',#54363);
#12882=PLANE('',#54364);
#12883=PLANE('',#54365);
#12884=PLANE('',#54366);
#12885=PLANE('',#54367);
#12886=PLANE('',#54373);
#12887=PLANE('',#54390);
#12888=PLANE('',#54441);
#12889=PLANE('',#54444);
#12890=PLANE('',#54447);
#12891=PLANE('',#54450);
#12892=PLANE('',#54453);
#12893=PLANE('',#54454);
#12894=PLANE('',#54457);
#12895=PLANE('',#54460);
#12896=PLANE('',#54462);
#12897=PLANE('',#54464);
#12898=PLANE('',#54467);
#12899=PLANE('',#54471);
#12900=PLANE('',#54473);
#12901=PLANE('',#54480);
#12902=PLANE('',#54488);
#12903=PLANE('',#54527);
#12904=PLANE('',#54530);
#12905=PLANE('',#54540);
#12906=PLANE('',#54542);
#12907=PLANE('',#54543);
#12908=PLANE('',#54545);
#12909=PLANE('',#54546);
#12910=PLANE('',#54548);
#12911=PLANE('',#54549);
#12912=PLANE('',#54551);
#12913=PLANE('',#54552);
#12914=PLANE('',#54554);
#12915=PLANE('',#54555);
#12916=PLANE('',#54557);
#12917=PLANE('',#54558);
#12918=PLANE('',#54560);
#12919=PLANE('',#54561);
#12920=PLANE('',#54563);
#12921=PLANE('',#54564);
#12922=PLANE('',#54566);
#12923=PLANE('',#54567);
#12924=PLANE('',#54569);
#12925=PLANE('',#54570);
#12926=PLANE('',#54572);
#12927=PLANE('',#54573);
#12928=PLANE('',#54575);
#12929=PLANE('',#54576);
#12930=PLANE('',#54578);
#12931=PLANE('',#54579);
#12932=PLANE('',#54581);
#12933=PLANE('',#54582);
#12934=PLANE('',#54584);
#12935=PLANE('',#54585);
#12936=PLANE('',#54587);
#12937=PLANE('',#54588);
#12938=PLANE('',#54590);
#12939=PLANE('',#54591);
#12940=PLANE('',#54593);
#12941=PLANE('',#54594);
#12942=PLANE('',#54596);
#12943=PLANE('',#54597);
#12944=PLANE('',#54599);
#12945=PLANE('',#54600);
#12946=PLANE('',#54602);
#12947=PLANE('',#54603);
#12948=PLANE('',#54605);
#12949=PLANE('',#54606);
#12950=PLANE('',#54608);
#12951=PLANE('',#54609);
#12952=PLANE('',#54611);
#12953=PLANE('',#54612);
#12954=PLANE('',#54614);
#12955=PLANE('',#54615);
#12956=PLANE('',#54617);
#12957=PLANE('',#54618);
#12958=PLANE('',#54620);
#12959=PLANE('',#54621);
#12960=PLANE('',#54623);
#12961=PLANE('',#54624);
#12962=PLANE('',#54626);
#12963=PLANE('',#54627);
#12964=PLANE('',#54629);
#12965=PLANE('',#54630);
#12966=PLANE('',#54632);
#12967=PLANE('',#54633);
#12968=PLANE('',#54635);
#12969=PLANE('',#54636);
#12970=PLANE('',#54638);
#12971=PLANE('',#54639);
#12972=PLANE('',#54641);
#12973=PLANE('',#54642);
#12974=PLANE('',#54644);
#12975=PLANE('',#54645);
#12976=PLANE('',#54648);
#12977=PLANE('',#54649);
#12978=PLANE('',#54652);
#12979=PLANE('',#54653);
#12980=PLANE('',#54655);
#12981=PLANE('',#54656);
#12982=PLANE('',#54658);
#12983=PLANE('',#54659);
#12984=PLANE('',#54661);
#12985=PLANE('',#54662);
#12986=PLANE('',#54664);
#12987=PLANE('',#54665);
#12988=PLANE('',#54667);
#12989=PLANE('',#54668);
#12990=PLANE('',#54670);
#12991=PLANE('',#54671);
#12992=PLANE('',#54673);
#12993=PLANE('',#54674);
#12994=PLANE('',#54676);
#12995=PLANE('',#54677);
#12996=PLANE('',#54679);
#12997=PLANE('',#54680);
#12998=PLANE('',#54682);
#12999=PLANE('',#54683);
#13000=PLANE('',#54685);
#13001=PLANE('',#54686);
#13002=PLANE('',#54688);
#13003=PLANE('',#54689);
#13004=PLANE('',#54691);
#13005=PLANE('',#54692);
#13006=PLANE('',#54694);
#13007=PLANE('',#54695);
#13008=PLANE('',#54697);
#13009=PLANE('',#54698);
#13010=PLANE('',#54700);
#13011=PLANE('',#54701);
#13012=PLANE('',#54703);
#13013=PLANE('',#54704);
#13014=PLANE('',#54706);
#13015=PLANE('',#54707);
#13016=PLANE('',#54709);
#13017=PLANE('',#54710);
#13018=PLANE('',#54712);
#13019=PLANE('',#54713);
#13020=PLANE('',#54715);
#13021=PLANE('',#54716);
#13022=PLANE('',#54718);
#13023=PLANE('',#54719);
#13024=PLANE('',#54721);
#13025=PLANE('',#54722);
#13026=PLANE('',#54724);
#13027=PLANE('',#54725);
#13028=PLANE('',#54727);
#13029=PLANE('',#54728);
#13030=PLANE('',#54730);
#13031=PLANE('',#54731);
#13032=PLANE('',#54733);
#13033=PLANE('',#54734);
#13034=PLANE('',#54736);
#13035=PLANE('',#54737);
#13036=PLANE('',#54739);
#13037=PLANE('',#54740);
#13038=PLANE('',#54742);
#13039=PLANE('',#54743);
#13040=PLANE('',#54745);
#13041=PLANE('',#54746);
#13042=PLANE('',#54748);
#13043=PLANE('',#54749);
#13044=PLANE('',#54751);
#13045=PLANE('',#54752);
#13046=PLANE('',#54754);
#13047=PLANE('',#54756);
#13048=PLANE('',#54757);
#13049=PLANE('',#54758);
#13050=PLANE('',#54762);
#13051=PLANE('',#54763);
#13052=PLANE('',#54764);
#13053=PLANE('',#54765);
#13054=PLANE('',#54766);
#13055=PLANE('',#54767);
#13056=PLANE('',#54768);
#13057=PLANE('',#54769);
#13058=PLANE('',#54811);
#13059=PLANE('',#54820);
#13060=PLANE('',#54828);
#13061=PLANE('',#54838);
#13062=PLANE('',#54840);
#13063=PLANE('',#54849);
#13064=PLANE('',#54857);
#13065=PLANE('',#54893);
#13066=PLANE('',#54896);
#13067=PLANE('',#54906);
#13068=PLANE('',#54908);
#13069=PLANE('',#54909);
#13070=PLANE('',#54911);
#13071=PLANE('',#54912);
#13072=PLANE('',#54914);
#13073=PLANE('',#54915);
#13074=PLANE('',#54917);
#13075=PLANE('',#54918);
#13076=PLANE('',#54920);
#13077=PLANE('',#54921);
#13078=PLANE('',#54923);
#13079=PLANE('',#54924);
#13080=PLANE('',#54926);
#13081=PLANE('',#54927);
#13082=PLANE('',#54929);
#13083=PLANE('',#54930);
#13084=PLANE('',#54932);
#13085=PLANE('',#54933);
#13086=PLANE('',#54935);
#13087=PLANE('',#54936);
#13088=PLANE('',#54938);
#13089=PLANE('',#54939);
#13090=PLANE('',#54941);
#13091=PLANE('',#54942);
#13092=PLANE('',#54944);
#13093=PLANE('',#54945);
#13094=PLANE('',#54947);
#13095=PLANE('',#54948);
#13096=PLANE('',#54950);
#13097=PLANE('',#54951);
#13098=PLANE('',#54953);
#13099=PLANE('',#54954);
#13100=PLANE('',#54956);
#13101=PLANE('',#54957);
#13102=PLANE('',#54959);
#13103=PLANE('',#54960);
#13104=PLANE('',#54962);
#13105=PLANE('',#54963);
#13106=PLANE('',#54965);
#13107=PLANE('',#54966);
#13108=PLANE('',#54968);
#13109=PLANE('',#54969);
#13110=PLANE('',#54971);
#13111=PLANE('',#54972);
#13112=PLANE('',#54974);
#13113=PLANE('',#54975);
#13114=PLANE('',#54977);
#13115=PLANE('',#54978);
#13116=PLANE('',#54980);
#13117=PLANE('',#54981);
#13118=PLANE('',#54983);
#13119=PLANE('',#54984);
#13120=PLANE('',#54986);
#13121=PLANE('',#54987);
#13122=PLANE('',#54989);
#13123=PLANE('',#54990);
#13124=PLANE('',#54992);
#13125=PLANE('',#54993);
#13126=PLANE('',#54995);
#13127=PLANE('',#54996);
#13128=PLANE('',#54998);
#13129=PLANE('',#54999);
#13130=PLANE('',#55001);
#13131=PLANE('',#55002);
#13132=PLANE('',#55004);
#13133=PLANE('',#55005);
#13134=PLANE('',#55007);
#13135=PLANE('',#55008);
#13136=PLANE('',#55010);
#13137=PLANE('',#55011);
#13138=PLANE('',#55014);
#13139=PLANE('',#55015);
#13140=PLANE('',#55018);
#13141=PLANE('',#55019);
#13142=PLANE('',#55021);
#13143=PLANE('',#55022);
#13144=PLANE('',#55024);
#13145=PLANE('',#55025);
#13146=PLANE('',#55027);
#13147=PLANE('',#55028);
#13148=PLANE('',#55030);
#13149=PLANE('',#55031);
#13150=PLANE('',#55033);
#13151=PLANE('',#55034);
#13152=PLANE('',#55036);
#13153=PLANE('',#55037);
#13154=PLANE('',#55039);
#13155=PLANE('',#55040);
#13156=PLANE('',#55042);
#13157=PLANE('',#55043);
#13158=PLANE('',#55045);
#13159=PLANE('',#55046);
#13160=PLANE('',#55048);
#13161=PLANE('',#55049);
#13162=PLANE('',#55051);
#13163=PLANE('',#55052);
#13164=PLANE('',#55054);
#13165=PLANE('',#55055);
#13166=PLANE('',#55057);
#13167=PLANE('',#55058);
#13168=PLANE('',#55060);
#13169=PLANE('',#55061);
#13170=PLANE('',#55063);
#13171=PLANE('',#55064);
#13172=PLANE('',#55066);
#13173=PLANE('',#55067);
#13174=PLANE('',#55069);
#13175=PLANE('',#55070);
#13176=PLANE('',#55072);
#13177=PLANE('',#55073);
#13178=PLANE('',#55075);
#13179=PLANE('',#55076);
#13180=PLANE('',#55078);
#13181=PLANE('',#55079);
#13182=PLANE('',#55081);
#13183=PLANE('',#55082);
#13184=PLANE('',#55084);
#13185=PLANE('',#55085);
#13186=PLANE('',#55087);
#13187=PLANE('',#55088);
#13188=PLANE('',#55090);
#13189=PLANE('',#55091);
#13190=PLANE('',#55093);
#13191=PLANE('',#55094);
#13192=PLANE('',#55096);
#13193=PLANE('',#55097);
#13194=PLANE('',#55099);
#13195=PLANE('',#55100);
#13196=PLANE('',#55102);
#13197=PLANE('',#55103);
#13198=PLANE('',#55105);
#13199=PLANE('',#55106);
#13200=PLANE('',#55108);
#13201=PLANE('',#55109);
#13202=PLANE('',#55111);
#13203=PLANE('',#55112);
#13204=PLANE('',#55114);
#13205=PLANE('',#55115);
#13206=PLANE('',#55117);
#13207=PLANE('',#55118);
#13208=PLANE('',#55120);
#13209=PLANE('',#55122);
#13210=PLANE('',#55123);
#13211=PLANE('',#55124);
#13212=PLANE('',#55128);
#13213=PLANE('',#55129);
#13214=PLANE('',#55130);
#13215=PLANE('',#55131);
#13216=PLANE('',#55132);
#13217=PLANE('',#55133);
#13218=PLANE('',#55134);
#13219=PLANE('',#55135);
#13220=PLANE('',#55177);
#13221=PLANE('',#55186);
#13222=PLANE('',#55187);
#13223=PLANE('',#55241);
#13224=PLANE('',#55244);
#13225=PLANE('',#55254);
#13226=PLANE('',#55258);
#13227=PLANE('',#55259);
#13228=PLANE('',#55260);
#13229=PLANE('',#55263);
#13230=PLANE('',#55266);
#13231=PLANE('',#55267);
#13232=PLANE('',#55268);
#13233=PLANE('',#55269);
#13234=PLANE('',#55270);
#13235=PLANE('',#55279);
#13236=PLANE('',#55287);
#13237=PLANE('',#55293);
#13238=PLANE('',#55296);
#13239=PLANE('',#55305);
#13240=PLANE('',#55313);
#13241=PLANE('',#55324);
#13242=PLANE('',#55325);
#13243=PLANE('',#55326);
#13244=PLANE('',#55329);
#13245=PLANE('',#55330);
#13246=PLANE('',#55331);
#13247=PLANE('',#55332);
#13248=PLANE('',#55333);
#13249=FACE_OUTER_BOUND('',#15931,.T.);
#13250=FACE_OUTER_BOUND('',#15932,.T.);
#13251=FACE_OUTER_BOUND('',#15933,.T.);
#13252=FACE_OUTER_BOUND('',#15934,.T.);
#13253=FACE_OUTER_BOUND('',#15935,.T.);
#13254=FACE_OUTER_BOUND('',#15936,.T.);
#13255=FACE_OUTER_BOUND('',#15937,.T.);
#13256=FACE_OUTER_BOUND('',#15938,.T.);
#13257=FACE_OUTER_BOUND('',#15939,.T.);
#13258=FACE_OUTER_BOUND('',#15940,.T.);
#13259=FACE_OUTER_BOUND('',#15941,.T.);
#13260=FACE_OUTER_BOUND('',#15942,.T.);
#13261=FACE_OUTER_BOUND('',#15943,.T.);
#13262=FACE_OUTER_BOUND('',#15944,.T.);
#13263=FACE_OUTER_BOUND('',#15945,.T.);
#13264=FACE_OUTER_BOUND('',#15946,.T.);
#13265=FACE_OUTER_BOUND('',#15947,.T.);
#13266=FACE_OUTER_BOUND('',#15948,.T.);
#13267=FACE_OUTER_BOUND('',#15949,.T.);
#13268=FACE_OUTER_BOUND('',#15950,.T.);
#13269=FACE_OUTER_BOUND('',#15951,.T.);
#13270=FACE_OUTER_BOUND('',#15952,.T.);
#13271=FACE_OUTER_BOUND('',#15953,.T.);
#13272=FACE_OUTER_BOUND('',#15954,.T.);
#13273=FACE_OUTER_BOUND('',#15955,.T.);
#13274=FACE_OUTER_BOUND('',#15956,.T.);
#13275=FACE_OUTER_BOUND('',#15957,.T.);
#13276=FACE_OUTER_BOUND('',#15958,.T.);
#13277=FACE_OUTER_BOUND('',#15959,.T.);
#13278=FACE_OUTER_BOUND('',#15960,.T.);
#13279=FACE_OUTER_BOUND('',#15961,.T.);
#13280=FACE_OUTER_BOUND('',#15962,.T.);
#13281=FACE_OUTER_BOUND('',#15963,.T.);
#13282=FACE_OUTER_BOUND('',#15964,.T.);
#13283=FACE_OUTER_BOUND('',#15965,.T.);
#13284=FACE_OUTER_BOUND('',#15966,.T.);
#13285=FACE_OUTER_BOUND('',#15967,.T.);
#13286=FACE_OUTER_BOUND('',#15968,.T.);
#13287=FACE_OUTER_BOUND('',#15969,.T.);
#13288=FACE_OUTER_BOUND('',#15970,.T.);
#13289=FACE_OUTER_BOUND('',#15971,.T.);
#13290=FACE_OUTER_BOUND('',#15972,.T.);
#13291=FACE_OUTER_BOUND('',#15973,.T.);
#13292=FACE_OUTER_BOUND('',#15974,.T.);
#13293=FACE_OUTER_BOUND('',#15975,.T.);
#13294=FACE_OUTER_BOUND('',#15976,.T.);
#13295=FACE_OUTER_BOUND('',#15977,.T.);
#13296=FACE_OUTER_BOUND('',#15978,.T.);
#13297=FACE_OUTER_BOUND('',#15979,.T.);
#13298=FACE_OUTER_BOUND('',#15980,.T.);
#13299=FACE_OUTER_BOUND('',#15981,.T.);
#13300=FACE_OUTER_BOUND('',#15982,.T.);
#13301=FACE_OUTER_BOUND('',#15983,.T.);
#13302=FACE_OUTER_BOUND('',#15984,.T.);
#13303=FACE_OUTER_BOUND('',#15985,.T.);
#13304=FACE_OUTER_BOUND('',#15986,.T.);
#13305=FACE_OUTER_BOUND('',#15987,.T.);
#13306=FACE_OUTER_BOUND('',#15988,.T.);
#13307=FACE_OUTER_BOUND('',#15989,.T.);
#13308=FACE_OUTER_BOUND('',#15990,.T.);
#13309=FACE_OUTER_BOUND('',#15991,.T.);
#13310=FACE_OUTER_BOUND('',#15992,.T.);
#13311=FACE_OUTER_BOUND('',#15993,.T.);
#13312=FACE_OUTER_BOUND('',#15994,.T.);
#13313=FACE_OUTER_BOUND('',#15995,.T.);
#13314=FACE_OUTER_BOUND('',#15996,.T.);
#13315=FACE_OUTER_BOUND('',#15997,.T.);
#13316=FACE_OUTER_BOUND('',#15998,.T.);
#13317=FACE_OUTER_BOUND('',#15999,.T.);
#13318=FACE_OUTER_BOUND('',#16000,.T.);
#13319=FACE_OUTER_BOUND('',#16001,.T.);
#13320=FACE_OUTER_BOUND('',#16002,.T.);
#13321=FACE_OUTER_BOUND('',#16003,.T.);
#13322=FACE_OUTER_BOUND('',#16004,.T.);
#13323=FACE_OUTER_BOUND('',#16005,.T.);
#13324=FACE_OUTER_BOUND('',#16006,.T.);
#13325=FACE_OUTER_BOUND('',#16007,.T.);
#13326=FACE_OUTER_BOUND('',#16008,.T.);
#13327=FACE_OUTER_BOUND('',#16009,.T.);
#13328=FACE_OUTER_BOUND('',#16010,.T.);
#13329=FACE_OUTER_BOUND('',#16011,.T.);
#13330=FACE_OUTER_BOUND('',#16012,.T.);
#13331=FACE_OUTER_BOUND('',#16013,.T.);
#13332=FACE_OUTER_BOUND('',#16014,.T.);
#13333=FACE_OUTER_BOUND('',#16015,.T.);
#13334=FACE_OUTER_BOUND('',#16016,.T.);
#13335=FACE_OUTER_BOUND('',#16017,.T.);
#13336=FACE_OUTER_BOUND('',#16018,.T.);
#13337=FACE_OUTER_BOUND('',#16019,.T.);
#13338=FACE_OUTER_BOUND('',#16020,.T.);
#13339=FACE_OUTER_BOUND('',#16021,.T.);
#13340=FACE_OUTER_BOUND('',#16022,.T.);
#13341=FACE_OUTER_BOUND('',#16023,.T.);
#13342=FACE_OUTER_BOUND('',#16024,.T.);
#13343=FACE_OUTER_BOUND('',#16025,.T.);
#13344=FACE_OUTER_BOUND('',#16026,.T.);
#13345=FACE_OUTER_BOUND('',#16027,.T.);
#13346=FACE_OUTER_BOUND('',#16028,.T.);
#13347=FACE_OUTER_BOUND('',#16029,.T.);
#13348=FACE_OUTER_BOUND('',#16030,.T.);
#13349=FACE_OUTER_BOUND('',#16031,.T.);
#13350=FACE_OUTER_BOUND('',#16032,.T.);
#13351=FACE_OUTER_BOUND('',#16033,.T.);
#13352=FACE_OUTER_BOUND('',#16034,.T.);
#13353=FACE_OUTER_BOUND('',#16035,.T.);
#13354=FACE_OUTER_BOUND('',#16036,.T.);
#13355=FACE_OUTER_BOUND('',#16037,.T.);
#13356=FACE_OUTER_BOUND('',#16038,.T.);
#13357=FACE_OUTER_BOUND('',#16039,.T.);
#13358=FACE_OUTER_BOUND('',#16040,.T.);
#13359=FACE_OUTER_BOUND('',#16041,.T.);
#13360=FACE_OUTER_BOUND('',#16042,.T.);
#13361=FACE_OUTER_BOUND('',#16043,.T.);
#13362=FACE_OUTER_BOUND('',#16044,.T.);
#13363=FACE_OUTER_BOUND('',#16045,.T.);
#13364=FACE_OUTER_BOUND('',#16046,.T.);
#13365=FACE_OUTER_BOUND('',#16047,.T.);
#13366=FACE_OUTER_BOUND('',#16048,.T.);
#13367=FACE_OUTER_BOUND('',#16049,.T.);
#13368=FACE_OUTER_BOUND('',#16050,.T.);
#13369=FACE_OUTER_BOUND('',#16051,.T.);
#13370=FACE_OUTER_BOUND('',#16052,.T.);
#13371=FACE_OUTER_BOUND('',#16053,.T.);
#13372=FACE_OUTER_BOUND('',#16054,.T.);
#13373=FACE_OUTER_BOUND('',#16055,.T.);
#13374=FACE_OUTER_BOUND('',#16056,.T.);
#13375=FACE_OUTER_BOUND('',#16057,.T.);
#13376=FACE_OUTER_BOUND('',#16058,.T.);
#13377=FACE_OUTER_BOUND('',#16059,.T.);
#13378=FACE_OUTER_BOUND('',#16060,.T.);
#13379=FACE_OUTER_BOUND('',#16061,.T.);
#13380=FACE_OUTER_BOUND('',#16062,.T.);
#13381=FACE_OUTER_BOUND('',#16063,.T.);
#13382=FACE_OUTER_BOUND('',#16064,.T.);
#13383=FACE_OUTER_BOUND('',#16065,.T.);
#13384=FACE_OUTER_BOUND('',#16066,.T.);
#13385=FACE_OUTER_BOUND('',#16067,.T.);
#13386=FACE_OUTER_BOUND('',#16068,.T.);
#13387=FACE_OUTER_BOUND('',#16069,.T.);
#13388=FACE_OUTER_BOUND('',#16070,.T.);
#13389=FACE_OUTER_BOUND('',#16071,.T.);
#13390=FACE_OUTER_BOUND('',#16072,.T.);
#13391=FACE_OUTER_BOUND('',#16073,.T.);
#13392=FACE_OUTER_BOUND('',#16074,.T.);
#13393=FACE_OUTER_BOUND('',#16075,.T.);
#13394=FACE_OUTER_BOUND('',#16076,.T.);
#13395=FACE_OUTER_BOUND('',#16077,.T.);
#13396=FACE_OUTER_BOUND('',#16078,.T.);
#13397=FACE_OUTER_BOUND('',#16079,.T.);
#13398=FACE_OUTER_BOUND('',#16080,.T.);
#13399=FACE_OUTER_BOUND('',#16081,.T.);
#13400=FACE_OUTER_BOUND('',#16082,.T.);
#13401=FACE_OUTER_BOUND('',#16083,.T.);
#13402=FACE_OUTER_BOUND('',#16084,.T.);
#13403=FACE_OUTER_BOUND('',#16085,.T.);
#13404=FACE_OUTER_BOUND('',#16086,.T.);
#13405=FACE_OUTER_BOUND('',#16087,.T.);
#13406=FACE_OUTER_BOUND('',#16088,.T.);
#13407=FACE_OUTER_BOUND('',#16089,.T.);
#13408=FACE_OUTER_BOUND('',#16090,.T.);
#13409=FACE_OUTER_BOUND('',#16091,.T.);
#13410=FACE_OUTER_BOUND('',#16092,.T.);
#13411=FACE_OUTER_BOUND('',#16093,.T.);
#13412=FACE_OUTER_BOUND('',#16094,.T.);
#13413=FACE_OUTER_BOUND('',#16095,.T.);
#13414=FACE_OUTER_BOUND('',#16096,.T.);
#13415=FACE_OUTER_BOUND('',#16097,.T.);
#13416=FACE_OUTER_BOUND('',#16098,.T.);
#13417=FACE_OUTER_BOUND('',#16099,.T.);
#13418=FACE_OUTER_BOUND('',#16100,.T.);
#13419=FACE_OUTER_BOUND('',#16101,.T.);
#13420=FACE_OUTER_BOUND('',#16102,.T.);
#13421=FACE_OUTER_BOUND('',#16103,.T.);
#13422=FACE_OUTER_BOUND('',#16104,.T.);
#13423=FACE_OUTER_BOUND('',#16105,.T.);
#13424=FACE_OUTER_BOUND('',#16106,.T.);
#13425=FACE_OUTER_BOUND('',#16107,.T.);
#13426=FACE_OUTER_BOUND('',#16108,.T.);
#13427=FACE_OUTER_BOUND('',#16109,.T.);
#13428=FACE_OUTER_BOUND('',#16110,.T.);
#13429=FACE_OUTER_BOUND('',#16111,.T.);
#13430=FACE_OUTER_BOUND('',#16112,.T.);
#13431=FACE_OUTER_BOUND('',#16113,.T.);
#13432=FACE_OUTER_BOUND('',#16114,.T.);
#13433=FACE_OUTER_BOUND('',#16115,.T.);
#13434=FACE_OUTER_BOUND('',#16116,.T.);
#13435=FACE_OUTER_BOUND('',#16117,.T.);
#13436=FACE_OUTER_BOUND('',#16118,.T.);
#13437=FACE_OUTER_BOUND('',#16119,.T.);
#13438=FACE_OUTER_BOUND('',#16120,.T.);
#13439=FACE_OUTER_BOUND('',#16121,.T.);
#13440=FACE_OUTER_BOUND('',#16122,.T.);
#13441=FACE_OUTER_BOUND('',#16123,.T.);
#13442=FACE_OUTER_BOUND('',#16124,.T.);
#13443=FACE_OUTER_BOUND('',#16125,.T.);
#13444=FACE_OUTER_BOUND('',#16126,.T.);
#13445=FACE_OUTER_BOUND('',#16127,.T.);
#13446=FACE_OUTER_BOUND('',#16128,.T.);
#13447=FACE_OUTER_BOUND('',#16129,.T.);
#13448=FACE_OUTER_BOUND('',#16130,.T.);
#13449=FACE_OUTER_BOUND('',#16131,.T.);
#13450=FACE_OUTER_BOUND('',#16132,.T.);
#13451=FACE_OUTER_BOUND('',#16133,.T.);
#13452=FACE_OUTER_BOUND('',#16134,.T.);
#13453=FACE_OUTER_BOUND('',#16135,.T.);
#13454=FACE_OUTER_BOUND('',#16136,.T.);
#13455=FACE_OUTER_BOUND('',#16137,.T.);
#13456=FACE_OUTER_BOUND('',#16138,.T.);
#13457=FACE_OUTER_BOUND('',#16139,.T.);
#13458=FACE_OUTER_BOUND('',#16140,.T.);
#13459=FACE_OUTER_BOUND('',#16141,.T.);
#13460=FACE_OUTER_BOUND('',#16142,.T.);
#13461=FACE_OUTER_BOUND('',#16143,.T.);
#13462=FACE_OUTER_BOUND('',#16144,.T.);
#13463=FACE_OUTER_BOUND('',#16145,.T.);
#13464=FACE_OUTER_BOUND('',#16146,.T.);
#13465=FACE_OUTER_BOUND('',#16147,.T.);
#13466=FACE_OUTER_BOUND('',#16148,.T.);
#13467=FACE_OUTER_BOUND('',#16149,.T.);
#13468=FACE_OUTER_BOUND('',#16150,.T.);
#13469=FACE_OUTER_BOUND('',#16151,.T.);
#13470=FACE_OUTER_BOUND('',#16152,.T.);
#13471=FACE_OUTER_BOUND('',#16153,.T.);
#13472=FACE_OUTER_BOUND('',#16154,.T.);
#13473=FACE_OUTER_BOUND('',#16155,.T.);
#13474=FACE_OUTER_BOUND('',#16156,.T.);
#13475=FACE_OUTER_BOUND('',#16157,.T.);
#13476=FACE_OUTER_BOUND('',#16158,.T.);
#13477=FACE_OUTER_BOUND('',#16159,.T.);
#13478=FACE_OUTER_BOUND('',#16160,.T.);
#13479=FACE_OUTER_BOUND('',#16161,.T.);
#13480=FACE_OUTER_BOUND('',#16162,.T.);
#13481=FACE_OUTER_BOUND('',#16163,.T.);
#13482=FACE_OUTER_BOUND('',#16164,.T.);
#13483=FACE_OUTER_BOUND('',#16165,.T.);
#13484=FACE_OUTER_BOUND('',#16166,.T.);
#13485=FACE_OUTER_BOUND('',#16167,.T.);
#13486=FACE_OUTER_BOUND('',#16168,.T.);
#13487=FACE_OUTER_BOUND('',#16169,.T.);
#13488=FACE_OUTER_BOUND('',#16170,.T.);
#13489=FACE_OUTER_BOUND('',#16171,.T.);
#13490=FACE_OUTER_BOUND('',#16172,.T.);
#13491=FACE_OUTER_BOUND('',#16173,.T.);
#13492=FACE_OUTER_BOUND('',#16174,.T.);
#13493=FACE_OUTER_BOUND('',#16175,.T.);
#13494=FACE_OUTER_BOUND('',#16176,.T.);
#13495=FACE_OUTER_BOUND('',#16177,.T.);
#13496=FACE_OUTER_BOUND('',#16178,.T.);
#13497=FACE_OUTER_BOUND('',#16179,.T.);
#13498=FACE_OUTER_BOUND('',#16180,.T.);
#13499=FACE_OUTER_BOUND('',#16181,.T.);
#13500=FACE_OUTER_BOUND('',#16182,.T.);
#13501=FACE_OUTER_BOUND('',#16183,.T.);
#13502=FACE_OUTER_BOUND('',#16184,.T.);
#13503=FACE_OUTER_BOUND('',#16185,.T.);
#13504=FACE_OUTER_BOUND('',#16186,.T.);
#13505=FACE_OUTER_BOUND('',#16187,.T.);
#13506=FACE_OUTER_BOUND('',#16188,.T.);
#13507=FACE_OUTER_BOUND('',#16189,.T.);
#13508=FACE_OUTER_BOUND('',#16190,.T.);
#13509=FACE_OUTER_BOUND('',#16191,.T.);
#13510=FACE_OUTER_BOUND('',#16192,.T.);
#13511=FACE_OUTER_BOUND('',#16193,.T.);
#13512=FACE_OUTER_BOUND('',#16194,.T.);
#13513=FACE_OUTER_BOUND('',#16195,.T.);
#13514=FACE_OUTER_BOUND('',#16196,.T.);
#13515=FACE_OUTER_BOUND('',#16197,.T.);
#13516=FACE_OUTER_BOUND('',#16198,.T.);
#13517=FACE_OUTER_BOUND('',#16199,.T.);
#13518=FACE_OUTER_BOUND('',#16200,.T.);
#13519=FACE_OUTER_BOUND('',#16201,.T.);
#13520=FACE_OUTER_BOUND('',#16202,.T.);
#13521=FACE_OUTER_BOUND('',#16203,.T.);
#13522=FACE_OUTER_BOUND('',#16204,.T.);
#13523=FACE_OUTER_BOUND('',#16205,.T.);
#13524=FACE_OUTER_BOUND('',#16206,.T.);
#13525=FACE_OUTER_BOUND('',#16207,.T.);
#13526=FACE_OUTER_BOUND('',#16208,.T.);
#13527=FACE_OUTER_BOUND('',#16209,.T.);
#13528=FACE_OUTER_BOUND('',#16210,.T.);
#13529=FACE_OUTER_BOUND('',#16211,.T.);
#13530=FACE_OUTER_BOUND('',#16212,.T.);
#13531=FACE_OUTER_BOUND('',#16213,.T.);
#13532=FACE_OUTER_BOUND('',#16214,.T.);
#13533=FACE_OUTER_BOUND('',#16215,.T.);
#13534=FACE_OUTER_BOUND('',#16216,.T.);
#13535=FACE_OUTER_BOUND('',#16217,.T.);
#13536=FACE_OUTER_BOUND('',#16218,.T.);
#13537=FACE_OUTER_BOUND('',#16219,.T.);
#13538=FACE_OUTER_BOUND('',#16220,.T.);
#13539=FACE_OUTER_BOUND('',#16221,.T.);
#13540=FACE_OUTER_BOUND('',#16222,.T.);
#13541=FACE_OUTER_BOUND('',#16223,.T.);
#13542=FACE_OUTER_BOUND('',#16224,.T.);
#13543=FACE_OUTER_BOUND('',#16225,.T.);
#13544=FACE_OUTER_BOUND('',#16226,.T.);
#13545=FACE_OUTER_BOUND('',#16227,.T.);
#13546=FACE_OUTER_BOUND('',#16228,.T.);
#13547=FACE_OUTER_BOUND('',#16229,.T.);
#13548=FACE_OUTER_BOUND('',#16230,.T.);
#13549=FACE_OUTER_BOUND('',#16231,.T.);
#13550=FACE_OUTER_BOUND('',#16232,.T.);
#13551=FACE_OUTER_BOUND('',#16233,.T.);
#13552=FACE_OUTER_BOUND('',#16234,.T.);
#13553=FACE_OUTER_BOUND('',#16235,.T.);
#13554=FACE_OUTER_BOUND('',#16236,.T.);
#13555=FACE_OUTER_BOUND('',#16237,.T.);
#13556=FACE_OUTER_BOUND('',#16238,.T.);
#13557=FACE_OUTER_BOUND('',#16239,.T.);
#13558=FACE_OUTER_BOUND('',#16240,.T.);
#13559=FACE_OUTER_BOUND('',#16241,.T.);
#13560=FACE_OUTER_BOUND('',#16242,.T.);
#13561=FACE_OUTER_BOUND('',#16243,.T.);
#13562=FACE_OUTER_BOUND('',#16244,.T.);
#13563=FACE_OUTER_BOUND('',#16245,.T.);
#13564=FACE_OUTER_BOUND('',#16246,.T.);
#13565=FACE_OUTER_BOUND('',#16247,.T.);
#13566=FACE_OUTER_BOUND('',#16248,.T.);
#13567=FACE_OUTER_BOUND('',#16249,.T.);
#13568=FACE_OUTER_BOUND('',#16250,.T.);
#13569=FACE_OUTER_BOUND('',#16251,.T.);
#13570=FACE_OUTER_BOUND('',#16252,.T.);
#13571=FACE_OUTER_BOUND('',#16253,.T.);
#13572=FACE_OUTER_BOUND('',#16254,.T.);
#13573=FACE_OUTER_BOUND('',#16255,.T.);
#13574=FACE_OUTER_BOUND('',#16256,.T.);
#13575=FACE_OUTER_BOUND('',#16257,.T.);
#13576=FACE_OUTER_BOUND('',#16258,.T.);
#13577=FACE_OUTER_BOUND('',#16259,.T.);
#13578=FACE_OUTER_BOUND('',#16260,.T.);
#13579=FACE_OUTER_BOUND('',#16261,.T.);
#13580=FACE_OUTER_BOUND('',#16262,.T.);
#13581=FACE_OUTER_BOUND('',#16263,.T.);
#13582=FACE_OUTER_BOUND('',#16264,.T.);
#13583=FACE_OUTER_BOUND('',#16265,.T.);
#13584=FACE_OUTER_BOUND('',#16266,.T.);
#13585=FACE_OUTER_BOUND('',#16267,.T.);
#13586=FACE_OUTER_BOUND('',#16268,.T.);
#13587=FACE_OUTER_BOUND('',#16269,.T.);
#13588=FACE_OUTER_BOUND('',#16270,.T.);
#13589=FACE_OUTER_BOUND('',#16271,.T.);
#13590=FACE_OUTER_BOUND('',#16272,.T.);
#13591=FACE_OUTER_BOUND('',#16273,.T.);
#13592=FACE_OUTER_BOUND('',#16274,.T.);
#13593=FACE_OUTER_BOUND('',#16275,.T.);
#13594=FACE_OUTER_BOUND('',#16276,.T.);
#13595=FACE_OUTER_BOUND('',#16277,.T.);
#13596=FACE_OUTER_BOUND('',#16278,.T.);
#13597=FACE_OUTER_BOUND('',#16279,.T.);
#13598=FACE_OUTER_BOUND('',#16280,.T.);
#13599=FACE_OUTER_BOUND('',#16281,.T.);
#13600=FACE_OUTER_BOUND('',#16282,.T.);
#13601=FACE_OUTER_BOUND('',#16283,.T.);
#13602=FACE_OUTER_BOUND('',#16284,.T.);
#13603=FACE_OUTER_BOUND('',#16285,.T.);
#13604=FACE_OUTER_BOUND('',#16286,.T.);
#13605=FACE_OUTER_BOUND('',#16287,.T.);
#13606=FACE_OUTER_BOUND('',#16288,.T.);
#13607=FACE_OUTER_BOUND('',#16289,.T.);
#13608=FACE_OUTER_BOUND('',#16290,.T.);
#13609=FACE_OUTER_BOUND('',#16291,.T.);
#13610=FACE_OUTER_BOUND('',#16292,.T.);
#13611=FACE_OUTER_BOUND('',#16293,.T.);
#13612=FACE_OUTER_BOUND('',#16294,.T.);
#13613=FACE_OUTER_BOUND('',#16295,.T.);
#13614=FACE_OUTER_BOUND('',#16296,.T.);
#13615=FACE_OUTER_BOUND('',#16297,.T.);
#13616=FACE_OUTER_BOUND('',#16298,.T.);
#13617=FACE_OUTER_BOUND('',#16299,.T.);
#13618=FACE_OUTER_BOUND('',#16300,.T.);
#13619=FACE_OUTER_BOUND('',#16301,.T.);
#13620=FACE_OUTER_BOUND('',#16302,.T.);
#13621=FACE_OUTER_BOUND('',#16303,.T.);
#13622=FACE_OUTER_BOUND('',#16304,.T.);
#13623=FACE_OUTER_BOUND('',#16305,.T.);
#13624=FACE_OUTER_BOUND('',#16306,.T.);
#13625=FACE_OUTER_BOUND('',#16307,.T.);
#13626=FACE_OUTER_BOUND('',#16308,.T.);
#13627=FACE_OUTER_BOUND('',#16309,.T.);
#13628=FACE_OUTER_BOUND('',#16310,.T.);
#13629=FACE_OUTER_BOUND('',#16311,.T.);
#13630=FACE_OUTER_BOUND('',#16312,.T.);
#13631=FACE_OUTER_BOUND('',#16313,.T.);
#13632=FACE_OUTER_BOUND('',#16314,.T.);
#13633=FACE_OUTER_BOUND('',#16315,.T.);
#13634=FACE_OUTER_BOUND('',#16316,.T.);
#13635=FACE_OUTER_BOUND('',#16317,.T.);
#13636=FACE_OUTER_BOUND('',#16318,.T.);
#13637=FACE_OUTER_BOUND('',#16319,.T.);
#13638=FACE_OUTER_BOUND('',#16320,.T.);
#13639=FACE_OUTER_BOUND('',#16321,.T.);
#13640=FACE_OUTER_BOUND('',#16322,.T.);
#13641=FACE_OUTER_BOUND('',#16323,.T.);
#13642=FACE_OUTER_BOUND('',#16324,.T.);
#13643=FACE_OUTER_BOUND('',#16325,.T.);
#13644=FACE_OUTER_BOUND('',#16326,.T.);
#13645=FACE_OUTER_BOUND('',#16327,.T.);
#13646=FACE_OUTER_BOUND('',#16328,.T.);
#13647=FACE_OUTER_BOUND('',#16329,.T.);
#13648=FACE_OUTER_BOUND('',#16330,.T.);
#13649=FACE_OUTER_BOUND('',#16331,.T.);
#13650=FACE_OUTER_BOUND('',#16332,.T.);
#13651=FACE_OUTER_BOUND('',#16333,.T.);
#13652=FACE_OUTER_BOUND('',#16334,.T.);
#13653=FACE_OUTER_BOUND('',#16335,.T.);
#13654=FACE_OUTER_BOUND('',#16336,.T.);
#13655=FACE_OUTER_BOUND('',#16337,.T.);
#13656=FACE_OUTER_BOUND('',#16338,.T.);
#13657=FACE_OUTER_BOUND('',#16339,.T.);
#13658=FACE_OUTER_BOUND('',#16340,.T.);
#13659=FACE_OUTER_BOUND('',#16341,.T.);
#13660=FACE_OUTER_BOUND('',#16342,.T.);
#13661=FACE_OUTER_BOUND('',#16343,.T.);
#13662=FACE_OUTER_BOUND('',#16344,.T.);
#13663=FACE_OUTER_BOUND('',#16345,.T.);
#13664=FACE_OUTER_BOUND('',#16346,.T.);
#13665=FACE_OUTER_BOUND('',#16347,.T.);
#13666=FACE_OUTER_BOUND('',#16348,.T.);
#13667=FACE_OUTER_BOUND('',#16349,.T.);
#13668=FACE_OUTER_BOUND('',#16350,.T.);
#13669=FACE_OUTER_BOUND('',#16351,.T.);
#13670=FACE_OUTER_BOUND('',#16352,.T.);
#13671=FACE_OUTER_BOUND('',#16353,.T.);
#13672=FACE_OUTER_BOUND('',#16354,.T.);
#13673=FACE_OUTER_BOUND('',#16355,.T.);
#13674=FACE_OUTER_BOUND('',#16356,.T.);
#13675=FACE_OUTER_BOUND('',#16357,.T.);
#13676=FACE_OUTER_BOUND('',#16358,.T.);
#13677=FACE_OUTER_BOUND('',#16359,.T.);
#13678=FACE_OUTER_BOUND('',#16360,.T.);
#13679=FACE_OUTER_BOUND('',#16361,.T.);
#13680=FACE_OUTER_BOUND('',#16362,.T.);
#13681=FACE_OUTER_BOUND('',#16363,.T.);
#13682=FACE_OUTER_BOUND('',#16364,.T.);
#13683=FACE_OUTER_BOUND('',#16365,.T.);
#13684=FACE_OUTER_BOUND('',#16366,.T.);
#13685=FACE_OUTER_BOUND('',#16367,.T.);
#13686=FACE_OUTER_BOUND('',#16368,.T.);
#13687=FACE_OUTER_BOUND('',#16369,.T.);
#13688=FACE_OUTER_BOUND('',#16370,.T.);
#13689=FACE_OUTER_BOUND('',#16371,.T.);
#13690=FACE_OUTER_BOUND('',#16372,.T.);
#13691=FACE_OUTER_BOUND('',#16373,.T.);
#13692=FACE_OUTER_BOUND('',#16374,.T.);
#13693=FACE_OUTER_BOUND('',#16375,.T.);
#13694=FACE_OUTER_BOUND('',#16376,.T.);
#13695=FACE_OUTER_BOUND('',#16377,.T.);
#13696=FACE_OUTER_BOUND('',#16378,.T.);
#13697=FACE_OUTER_BOUND('',#16379,.T.);
#13698=FACE_OUTER_BOUND('',#16380,.T.);
#13699=FACE_OUTER_BOUND('',#16381,.T.);
#13700=FACE_OUTER_BOUND('',#16382,.T.);
#13701=FACE_OUTER_BOUND('',#16383,.T.);
#13702=FACE_OUTER_BOUND('',#16384,.T.);
#13703=FACE_OUTER_BOUND('',#16385,.T.);
#13704=FACE_OUTER_BOUND('',#16386,.T.);
#13705=FACE_OUTER_BOUND('',#16387,.T.);
#13706=FACE_OUTER_BOUND('',#16388,.T.);
#13707=FACE_OUTER_BOUND('',#16389,.T.);
#13708=FACE_OUTER_BOUND('',#16390,.T.);
#13709=FACE_OUTER_BOUND('',#16391,.T.);
#13710=FACE_OUTER_BOUND('',#16392,.T.);
#13711=FACE_OUTER_BOUND('',#16393,.T.);
#13712=FACE_OUTER_BOUND('',#16394,.T.);
#13713=FACE_OUTER_BOUND('',#16395,.T.);
#13714=FACE_OUTER_BOUND('',#16396,.T.);
#13715=FACE_OUTER_BOUND('',#16397,.T.);
#13716=FACE_OUTER_BOUND('',#16398,.T.);
#13717=FACE_OUTER_BOUND('',#16399,.T.);
#13718=FACE_OUTER_BOUND('',#16400,.T.);
#13719=FACE_OUTER_BOUND('',#16401,.T.);
#13720=FACE_OUTER_BOUND('',#16402,.T.);
#13721=FACE_OUTER_BOUND('',#16403,.T.);
#13722=FACE_OUTER_BOUND('',#16404,.T.);
#13723=FACE_OUTER_BOUND('',#16405,.T.);
#13724=FACE_OUTER_BOUND('',#16406,.T.);
#13725=FACE_OUTER_BOUND('',#16407,.T.);
#13726=FACE_OUTER_BOUND('',#16408,.T.);
#13727=FACE_OUTER_BOUND('',#16409,.T.);
#13728=FACE_OUTER_BOUND('',#16410,.T.);
#13729=FACE_OUTER_BOUND('',#16411,.T.);
#13730=FACE_OUTER_BOUND('',#16412,.T.);
#13731=FACE_OUTER_BOUND('',#16413,.T.);
#13732=FACE_OUTER_BOUND('',#16414,.T.);
#13733=FACE_OUTER_BOUND('',#16415,.T.);
#13734=FACE_OUTER_BOUND('',#16416,.T.);
#13735=FACE_OUTER_BOUND('',#16417,.T.);
#13736=FACE_OUTER_BOUND('',#16418,.T.);
#13737=FACE_OUTER_BOUND('',#16419,.T.);
#13738=FACE_OUTER_BOUND('',#16420,.T.);
#13739=FACE_OUTER_BOUND('',#16421,.T.);
#13740=FACE_OUTER_BOUND('',#16422,.T.);
#13741=FACE_OUTER_BOUND('',#16423,.T.);
#13742=FACE_OUTER_BOUND('',#16424,.T.);
#13743=FACE_OUTER_BOUND('',#16425,.T.);
#13744=FACE_OUTER_BOUND('',#16426,.T.);
#13745=FACE_OUTER_BOUND('',#16427,.T.);
#13746=FACE_OUTER_BOUND('',#16428,.T.);
#13747=FACE_OUTER_BOUND('',#16429,.T.);
#13748=FACE_OUTER_BOUND('',#16430,.T.);
#13749=FACE_OUTER_BOUND('',#16431,.T.);
#13750=FACE_OUTER_BOUND('',#16432,.T.);
#13751=FACE_OUTER_BOUND('',#16433,.T.);
#13752=FACE_OUTER_BOUND('',#16434,.T.);
#13753=FACE_OUTER_BOUND('',#16435,.T.);
#13754=FACE_OUTER_BOUND('',#16436,.T.);
#13755=FACE_OUTER_BOUND('',#16437,.T.);
#13756=FACE_OUTER_BOUND('',#16438,.T.);
#13757=FACE_OUTER_BOUND('',#16439,.T.);
#13758=FACE_OUTER_BOUND('',#16440,.T.);
#13759=FACE_OUTER_BOUND('',#16441,.T.);
#13760=FACE_OUTER_BOUND('',#16442,.T.);
#13761=FACE_OUTER_BOUND('',#16443,.T.);
#13762=FACE_OUTER_BOUND('',#16444,.T.);
#13763=FACE_OUTER_BOUND('',#16445,.T.);
#13764=FACE_OUTER_BOUND('',#16446,.T.);
#13765=FACE_OUTER_BOUND('',#16447,.T.);
#13766=FACE_OUTER_BOUND('',#16448,.T.);
#13767=FACE_OUTER_BOUND('',#16449,.T.);
#13768=FACE_OUTER_BOUND('',#16450,.T.);
#13769=FACE_OUTER_BOUND('',#16451,.T.);
#13770=FACE_OUTER_BOUND('',#16452,.T.);
#13771=FACE_OUTER_BOUND('',#16453,.T.);
#13772=FACE_OUTER_BOUND('',#16454,.T.);
#13773=FACE_OUTER_BOUND('',#16455,.T.);
#13774=FACE_OUTER_BOUND('',#16456,.T.);
#13775=FACE_OUTER_BOUND('',#16457,.T.);
#13776=FACE_OUTER_BOUND('',#16458,.T.);
#13777=FACE_OUTER_BOUND('',#16459,.T.);
#13778=FACE_OUTER_BOUND('',#16460,.T.);
#13779=FACE_OUTER_BOUND('',#16461,.T.);
#13780=FACE_OUTER_BOUND('',#16462,.T.);
#13781=FACE_OUTER_BOUND('',#16463,.T.);
#13782=FACE_OUTER_BOUND('',#16464,.T.);
#13783=FACE_OUTER_BOUND('',#16465,.T.);
#13784=FACE_OUTER_BOUND('',#16466,.T.);
#13785=FACE_OUTER_BOUND('',#16467,.T.);
#13786=FACE_OUTER_BOUND('',#16468,.T.);
#13787=FACE_OUTER_BOUND('',#16469,.T.);
#13788=FACE_OUTER_BOUND('',#16470,.T.);
#13789=FACE_OUTER_BOUND('',#16471,.T.);
#13790=FACE_OUTER_BOUND('',#16472,.T.);
#13791=FACE_OUTER_BOUND('',#16473,.T.);
#13792=FACE_OUTER_BOUND('',#16474,.T.);
#13793=FACE_OUTER_BOUND('',#16475,.T.);
#13794=FACE_OUTER_BOUND('',#16476,.T.);
#13795=FACE_OUTER_BOUND('',#16477,.T.);
#13796=FACE_OUTER_BOUND('',#16478,.T.);
#13797=FACE_OUTER_BOUND('',#16479,.T.);
#13798=FACE_OUTER_BOUND('',#16480,.T.);
#13799=FACE_OUTER_BOUND('',#16481,.T.);
#13800=FACE_OUTER_BOUND('',#16482,.T.);
#13801=FACE_OUTER_BOUND('',#16483,.T.);
#13802=FACE_OUTER_BOUND('',#16484,.T.);
#13803=FACE_OUTER_BOUND('',#16485,.T.);
#13804=FACE_OUTER_BOUND('',#16486,.T.);
#13805=FACE_OUTER_BOUND('',#16487,.T.);
#13806=FACE_OUTER_BOUND('',#16488,.T.);
#13807=FACE_OUTER_BOUND('',#16489,.T.);
#13808=FACE_OUTER_BOUND('',#16490,.T.);
#13809=FACE_OUTER_BOUND('',#16491,.T.);
#13810=FACE_OUTER_BOUND('',#16492,.T.);
#13811=FACE_OUTER_BOUND('',#16493,.T.);
#13812=FACE_OUTER_BOUND('',#16494,.T.);
#13813=FACE_OUTER_BOUND('',#16495,.T.);
#13814=FACE_OUTER_BOUND('',#16496,.T.);
#13815=FACE_OUTER_BOUND('',#16497,.T.);
#13816=FACE_OUTER_BOUND('',#16498,.T.);
#13817=FACE_OUTER_BOUND('',#16499,.T.);
#13818=FACE_OUTER_BOUND('',#16500,.T.);
#13819=FACE_OUTER_BOUND('',#16501,.T.);
#13820=FACE_OUTER_BOUND('',#16502,.T.);
#13821=FACE_OUTER_BOUND('',#16503,.T.);
#13822=FACE_OUTER_BOUND('',#16504,.T.);
#13823=FACE_OUTER_BOUND('',#16505,.T.);
#13824=FACE_OUTER_BOUND('',#16506,.T.);
#13825=FACE_OUTER_BOUND('',#16507,.T.);
#13826=FACE_OUTER_BOUND('',#16508,.T.);
#13827=FACE_OUTER_BOUND('',#16509,.T.);
#13828=FACE_OUTER_BOUND('',#16510,.T.);
#13829=FACE_OUTER_BOUND('',#16511,.T.);
#13830=FACE_OUTER_BOUND('',#16512,.T.);
#13831=FACE_OUTER_BOUND('',#16513,.T.);
#13832=FACE_OUTER_BOUND('',#16514,.T.);
#13833=FACE_OUTER_BOUND('',#16515,.T.);
#13834=FACE_OUTER_BOUND('',#16516,.T.);
#13835=FACE_OUTER_BOUND('',#16517,.T.);
#13836=FACE_OUTER_BOUND('',#16518,.T.);
#13837=FACE_OUTER_BOUND('',#16519,.T.);
#13838=FACE_OUTER_BOUND('',#16520,.T.);
#13839=FACE_OUTER_BOUND('',#16521,.T.);
#13840=FACE_OUTER_BOUND('',#16522,.T.);
#13841=FACE_OUTER_BOUND('',#16523,.T.);
#13842=FACE_OUTER_BOUND('',#16524,.T.);
#13843=FACE_OUTER_BOUND('',#16525,.T.);
#13844=FACE_OUTER_BOUND('',#16526,.T.);
#13845=FACE_OUTER_BOUND('',#16527,.T.);
#13846=FACE_OUTER_BOUND('',#16528,.T.);
#13847=FACE_OUTER_BOUND('',#16529,.T.);
#13848=FACE_OUTER_BOUND('',#16530,.T.);
#13849=FACE_OUTER_BOUND('',#16531,.T.);
#13850=FACE_OUTER_BOUND('',#16532,.T.);
#13851=FACE_OUTER_BOUND('',#16533,.T.);
#13852=FACE_OUTER_BOUND('',#16534,.T.);
#13853=FACE_OUTER_BOUND('',#16535,.T.);
#13854=FACE_OUTER_BOUND('',#16536,.T.);
#13855=FACE_OUTER_BOUND('',#16537,.T.);
#13856=FACE_OUTER_BOUND('',#16538,.T.);
#13857=FACE_OUTER_BOUND('',#16539,.T.);
#13858=FACE_OUTER_BOUND('',#16540,.T.);
#13859=FACE_OUTER_BOUND('',#16541,.T.);
#13860=FACE_OUTER_BOUND('',#16542,.T.);
#13861=FACE_OUTER_BOUND('',#16543,.T.);
#13862=FACE_OUTER_BOUND('',#16544,.T.);
#13863=FACE_OUTER_BOUND('',#16545,.T.);
#13864=FACE_OUTER_BOUND('',#16546,.T.);
#13865=FACE_OUTER_BOUND('',#16547,.T.);
#13866=FACE_OUTER_BOUND('',#16548,.T.);
#13867=FACE_OUTER_BOUND('',#16549,.T.);
#13868=FACE_OUTER_BOUND('',#16550,.T.);
#13869=FACE_OUTER_BOUND('',#16551,.T.);
#13870=FACE_OUTER_BOUND('',#16552,.T.);
#13871=FACE_OUTER_BOUND('',#16553,.T.);
#13872=FACE_OUTER_BOUND('',#16554,.T.);
#13873=FACE_OUTER_BOUND('',#16555,.T.);
#13874=FACE_OUTER_BOUND('',#16556,.T.);
#13875=FACE_OUTER_BOUND('',#16557,.T.);
#13876=FACE_OUTER_BOUND('',#16558,.T.);
#13877=FACE_OUTER_BOUND('',#16559,.T.);
#13878=FACE_OUTER_BOUND('',#16560,.T.);
#13879=FACE_OUTER_BOUND('',#16561,.T.);
#13880=FACE_OUTER_BOUND('',#16562,.T.);
#13881=FACE_OUTER_BOUND('',#16563,.T.);
#13882=FACE_OUTER_BOUND('',#16564,.T.);
#13883=FACE_OUTER_BOUND('',#16565,.T.);
#13884=FACE_OUTER_BOUND('',#16566,.T.);
#13885=FACE_OUTER_BOUND('',#16567,.T.);
#13886=FACE_OUTER_BOUND('',#16568,.T.);
#13887=FACE_OUTER_BOUND('',#16569,.T.);
#13888=FACE_OUTER_BOUND('',#16570,.T.);
#13889=FACE_OUTER_BOUND('',#16571,.T.);
#13890=FACE_OUTER_BOUND('',#16572,.T.);
#13891=FACE_OUTER_BOUND('',#16573,.T.);
#13892=FACE_OUTER_BOUND('',#16574,.T.);
#13893=FACE_OUTER_BOUND('',#16575,.T.);
#13894=FACE_OUTER_BOUND('',#16576,.T.);
#13895=FACE_OUTER_BOUND('',#16577,.T.);
#13896=FACE_OUTER_BOUND('',#16578,.T.);
#13897=FACE_OUTER_BOUND('',#16579,.T.);
#13898=FACE_OUTER_BOUND('',#16580,.T.);
#13899=FACE_OUTER_BOUND('',#16581,.T.);
#13900=FACE_OUTER_BOUND('',#16582,.T.);
#13901=FACE_OUTER_BOUND('',#16583,.T.);
#13902=FACE_OUTER_BOUND('',#16584,.T.);
#13903=FACE_OUTER_BOUND('',#16585,.T.);
#13904=FACE_OUTER_BOUND('',#16586,.T.);
#13905=FACE_OUTER_BOUND('',#16587,.T.);
#13906=FACE_OUTER_BOUND('',#16588,.T.);
#13907=FACE_OUTER_BOUND('',#16589,.T.);
#13908=FACE_OUTER_BOUND('',#16590,.T.);
#13909=FACE_OUTER_BOUND('',#16591,.T.);
#13910=FACE_OUTER_BOUND('',#16592,.T.);
#13911=FACE_OUTER_BOUND('',#16593,.T.);
#13912=FACE_OUTER_BOUND('',#16594,.T.);
#13913=FACE_OUTER_BOUND('',#16595,.T.);
#13914=FACE_OUTER_BOUND('',#16596,.T.);
#13915=FACE_OUTER_BOUND('',#16597,.T.);
#13916=FACE_OUTER_BOUND('',#16598,.T.);
#13917=FACE_OUTER_BOUND('',#16599,.T.);
#13918=FACE_OUTER_BOUND('',#16600,.T.);
#13919=FACE_OUTER_BOUND('',#16601,.T.);
#13920=FACE_OUTER_BOUND('',#16602,.T.);
#13921=FACE_OUTER_BOUND('',#16603,.T.);
#13922=FACE_OUTER_BOUND('',#16604,.T.);
#13923=FACE_OUTER_BOUND('',#16605,.T.);
#13924=FACE_OUTER_BOUND('',#16606,.T.);
#13925=FACE_OUTER_BOUND('',#16607,.T.);
#13926=FACE_OUTER_BOUND('',#16608,.T.);
#13927=FACE_OUTER_BOUND('',#16609,.T.);
#13928=FACE_OUTER_BOUND('',#16610,.T.);
#13929=FACE_OUTER_BOUND('',#16611,.T.);
#13930=FACE_OUTER_BOUND('',#16612,.T.);
#13931=FACE_OUTER_BOUND('',#16613,.T.);
#13932=FACE_OUTER_BOUND('',#16614,.T.);
#13933=FACE_OUTER_BOUND('',#16615,.T.);
#13934=FACE_OUTER_BOUND('',#16616,.T.);
#13935=FACE_OUTER_BOUND('',#16617,.T.);
#13936=FACE_OUTER_BOUND('',#16618,.T.);
#13937=FACE_OUTER_BOUND('',#16619,.T.);
#13938=FACE_OUTER_BOUND('',#16620,.T.);
#13939=FACE_OUTER_BOUND('',#16621,.T.);
#13940=FACE_OUTER_BOUND('',#16622,.T.);
#13941=FACE_OUTER_BOUND('',#16623,.T.);
#13942=FACE_OUTER_BOUND('',#16624,.T.);
#13943=FACE_OUTER_BOUND('',#16625,.T.);
#13944=FACE_OUTER_BOUND('',#16626,.T.);
#13945=FACE_OUTER_BOUND('',#16627,.T.);
#13946=FACE_OUTER_BOUND('',#16628,.T.);
#13947=FACE_OUTER_BOUND('',#16629,.T.);
#13948=FACE_OUTER_BOUND('',#16630,.T.);
#13949=FACE_OUTER_BOUND('',#16631,.T.);
#13950=FACE_OUTER_BOUND('',#16632,.T.);
#13951=FACE_OUTER_BOUND('',#16633,.T.);
#13952=FACE_OUTER_BOUND('',#16634,.T.);
#13953=FACE_OUTER_BOUND('',#16635,.T.);
#13954=FACE_OUTER_BOUND('',#16636,.T.);
#13955=FACE_OUTER_BOUND('',#16637,.T.);
#13956=FACE_OUTER_BOUND('',#16638,.T.);
#13957=FACE_OUTER_BOUND('',#16639,.T.);
#13958=FACE_OUTER_BOUND('',#16640,.T.);
#13959=FACE_OUTER_BOUND('',#16641,.T.);
#13960=FACE_OUTER_BOUND('',#16642,.T.);
#13961=FACE_OUTER_BOUND('',#16643,.T.);
#13962=FACE_OUTER_BOUND('',#16644,.T.);
#13963=FACE_OUTER_BOUND('',#16645,.T.);
#13964=FACE_OUTER_BOUND('',#16646,.T.);
#13965=FACE_OUTER_BOUND('',#16647,.T.);
#13966=FACE_OUTER_BOUND('',#16648,.T.);
#13967=FACE_OUTER_BOUND('',#16649,.T.);
#13968=FACE_OUTER_BOUND('',#16650,.T.);
#13969=FACE_OUTER_BOUND('',#16651,.T.);
#13970=FACE_OUTER_BOUND('',#16652,.T.);
#13971=FACE_OUTER_BOUND('',#16653,.T.);
#13972=FACE_OUTER_BOUND('',#16654,.T.);
#13973=FACE_OUTER_BOUND('',#16655,.T.);
#13974=FACE_OUTER_BOUND('',#16656,.T.);
#13975=FACE_OUTER_BOUND('',#16657,.T.);
#13976=FACE_OUTER_BOUND('',#16658,.T.);
#13977=FACE_OUTER_BOUND('',#16659,.T.);
#13978=FACE_OUTER_BOUND('',#16660,.T.);
#13979=FACE_OUTER_BOUND('',#16661,.T.);
#13980=FACE_OUTER_BOUND('',#16662,.T.);
#13981=FACE_OUTER_BOUND('',#16663,.T.);
#13982=FACE_OUTER_BOUND('',#16664,.T.);
#13983=FACE_OUTER_BOUND('',#16665,.T.);
#13984=FACE_OUTER_BOUND('',#16666,.T.);
#13985=FACE_OUTER_BOUND('',#16667,.T.);
#13986=FACE_OUTER_BOUND('',#16668,.T.);
#13987=FACE_OUTER_BOUND('',#16669,.T.);
#13988=FACE_OUTER_BOUND('',#16670,.T.);
#13989=FACE_OUTER_BOUND('',#16671,.T.);
#13990=FACE_OUTER_BOUND('',#16672,.T.);
#13991=FACE_OUTER_BOUND('',#16673,.T.);
#13992=FACE_OUTER_BOUND('',#16674,.T.);
#13993=FACE_OUTER_BOUND('',#16675,.T.);
#13994=FACE_OUTER_BOUND('',#16676,.T.);
#13995=FACE_OUTER_BOUND('',#16677,.T.);
#13996=FACE_OUTER_BOUND('',#16678,.T.);
#13997=FACE_OUTER_BOUND('',#16679,.T.);
#13998=FACE_OUTER_BOUND('',#16680,.T.);
#13999=FACE_OUTER_BOUND('',#16681,.T.);
#14000=FACE_OUTER_BOUND('',#16682,.T.);
#14001=FACE_OUTER_BOUND('',#16683,.T.);
#14002=FACE_OUTER_BOUND('',#16684,.T.);
#14003=FACE_OUTER_BOUND('',#16685,.T.);
#14004=FACE_OUTER_BOUND('',#16686,.T.);
#14005=FACE_OUTER_BOUND('',#16687,.T.);
#14006=FACE_OUTER_BOUND('',#16688,.T.);
#14007=FACE_OUTER_BOUND('',#16689,.T.);
#14008=FACE_OUTER_BOUND('',#16690,.T.);
#14009=FACE_OUTER_BOUND('',#16691,.T.);
#14010=FACE_OUTER_BOUND('',#16692,.T.);
#14011=FACE_OUTER_BOUND('',#16693,.T.);
#14012=FACE_OUTER_BOUND('',#16694,.T.);
#14013=FACE_OUTER_BOUND('',#16695,.T.);
#14014=FACE_OUTER_BOUND('',#16696,.T.);
#14015=FACE_OUTER_BOUND('',#16697,.T.);
#14016=FACE_OUTER_BOUND('',#16698,.T.);
#14017=FACE_OUTER_BOUND('',#16699,.T.);
#14018=FACE_OUTER_BOUND('',#16700,.T.);
#14019=FACE_OUTER_BOUND('',#16701,.T.);
#14020=FACE_OUTER_BOUND('',#16702,.T.);
#14021=FACE_OUTER_BOUND('',#16703,.T.);
#14022=FACE_OUTER_BOUND('',#16704,.T.);
#14023=FACE_OUTER_BOUND('',#16705,.T.);
#14024=FACE_OUTER_BOUND('',#16706,.T.);
#14025=FACE_OUTER_BOUND('',#16707,.T.);
#14026=FACE_OUTER_BOUND('',#16708,.T.);
#14027=FACE_OUTER_BOUND('',#16709,.T.);
#14028=FACE_OUTER_BOUND('',#16710,.T.);
#14029=FACE_OUTER_BOUND('',#16711,.T.);
#14030=FACE_OUTER_BOUND('',#16712,.T.);
#14031=FACE_OUTER_BOUND('',#16713,.T.);
#14032=FACE_OUTER_BOUND('',#16714,.T.);
#14033=FACE_OUTER_BOUND('',#16715,.T.);
#14034=FACE_OUTER_BOUND('',#16716,.T.);
#14035=FACE_OUTER_BOUND('',#16717,.T.);
#14036=FACE_OUTER_BOUND('',#16718,.T.);
#14037=FACE_OUTER_BOUND('',#16719,.T.);
#14038=FACE_OUTER_BOUND('',#16720,.T.);
#14039=FACE_OUTER_BOUND('',#16721,.T.);
#14040=FACE_OUTER_BOUND('',#16722,.T.);
#14041=FACE_OUTER_BOUND('',#16723,.T.);
#14042=FACE_OUTER_BOUND('',#16724,.T.);
#14043=FACE_OUTER_BOUND('',#16725,.T.);
#14044=FACE_OUTER_BOUND('',#16726,.T.);
#14045=FACE_OUTER_BOUND('',#16727,.T.);
#14046=FACE_OUTER_BOUND('',#16728,.T.);
#14047=FACE_OUTER_BOUND('',#16729,.T.);
#14048=FACE_OUTER_BOUND('',#16730,.T.);
#14049=FACE_OUTER_BOUND('',#16731,.T.);
#14050=FACE_OUTER_BOUND('',#16732,.T.);
#14051=FACE_OUTER_BOUND('',#16733,.T.);
#14052=FACE_OUTER_BOUND('',#16734,.T.);
#14053=FACE_OUTER_BOUND('',#16735,.T.);
#14054=FACE_OUTER_BOUND('',#16736,.T.);
#14055=FACE_OUTER_BOUND('',#16737,.T.);
#14056=FACE_OUTER_BOUND('',#16738,.T.);
#14057=FACE_OUTER_BOUND('',#16739,.T.);
#14058=FACE_OUTER_BOUND('',#16740,.T.);
#14059=FACE_OUTER_BOUND('',#16741,.T.);
#14060=FACE_OUTER_BOUND('',#16742,.T.);
#14061=FACE_OUTER_BOUND('',#16743,.T.);
#14062=FACE_OUTER_BOUND('',#16744,.T.);
#14063=FACE_OUTER_BOUND('',#16745,.T.);
#14064=FACE_OUTER_BOUND('',#16746,.T.);
#14065=FACE_OUTER_BOUND('',#16747,.T.);
#14066=FACE_OUTER_BOUND('',#16748,.T.);
#14067=FACE_OUTER_BOUND('',#16749,.T.);
#14068=FACE_OUTER_BOUND('',#16750,.T.);
#14069=FACE_OUTER_BOUND('',#16751,.T.);
#14070=FACE_OUTER_BOUND('',#16752,.T.);
#14071=FACE_OUTER_BOUND('',#16753,.T.);
#14072=FACE_OUTER_BOUND('',#16754,.T.);
#14073=FACE_OUTER_BOUND('',#16755,.T.);
#14074=FACE_OUTER_BOUND('',#16756,.T.);
#14075=FACE_OUTER_BOUND('',#16757,.T.);
#14076=FACE_OUTER_BOUND('',#16758,.T.);
#14077=FACE_OUTER_BOUND('',#16759,.T.);
#14078=FACE_OUTER_BOUND('',#16760,.T.);
#14079=FACE_OUTER_BOUND('',#16761,.T.);
#14080=FACE_OUTER_BOUND('',#16762,.T.);
#14081=FACE_OUTER_BOUND('',#16763,.T.);
#14082=FACE_OUTER_BOUND('',#16764,.T.);
#14083=FACE_OUTER_BOUND('',#16765,.T.);
#14084=FACE_OUTER_BOUND('',#16766,.T.);
#14085=FACE_OUTER_BOUND('',#16767,.T.);
#14086=FACE_OUTER_BOUND('',#16768,.T.);
#14087=FACE_OUTER_BOUND('',#16769,.T.);
#14088=FACE_OUTER_BOUND('',#16770,.T.);
#14089=FACE_OUTER_BOUND('',#16771,.T.);
#14090=FACE_OUTER_BOUND('',#16772,.T.);
#14091=FACE_OUTER_BOUND('',#16773,.T.);
#14092=FACE_OUTER_BOUND('',#16774,.T.);
#14093=FACE_OUTER_BOUND('',#16775,.T.);
#14094=FACE_OUTER_BOUND('',#16776,.T.);
#14095=FACE_OUTER_BOUND('',#16777,.T.);
#14096=FACE_OUTER_BOUND('',#16778,.T.);
#14097=FACE_OUTER_BOUND('',#16779,.T.);
#14098=FACE_OUTER_BOUND('',#16780,.T.);
#14099=FACE_OUTER_BOUND('',#16781,.T.);
#14100=FACE_OUTER_BOUND('',#16782,.T.);
#14101=FACE_OUTER_BOUND('',#16783,.T.);
#14102=FACE_OUTER_BOUND('',#16784,.T.);
#14103=FACE_OUTER_BOUND('',#16785,.T.);
#14104=FACE_OUTER_BOUND('',#16786,.T.);
#14105=FACE_OUTER_BOUND('',#16787,.T.);
#14106=FACE_OUTER_BOUND('',#16788,.T.);
#14107=FACE_OUTER_BOUND('',#16789,.T.);
#14108=FACE_OUTER_BOUND('',#16790,.T.);
#14109=FACE_OUTER_BOUND('',#16791,.T.);
#14110=FACE_OUTER_BOUND('',#16792,.T.);
#14111=FACE_OUTER_BOUND('',#16793,.T.);
#14112=FACE_OUTER_BOUND('',#16794,.T.);
#14113=FACE_OUTER_BOUND('',#16795,.T.);
#14114=FACE_OUTER_BOUND('',#16796,.T.);
#14115=FACE_OUTER_BOUND('',#16797,.T.);
#14116=FACE_OUTER_BOUND('',#16798,.T.);
#14117=FACE_OUTER_BOUND('',#16799,.T.);
#14118=FACE_OUTER_BOUND('',#16800,.T.);
#14119=FACE_OUTER_BOUND('',#16801,.T.);
#14120=FACE_OUTER_BOUND('',#16802,.T.);
#14121=FACE_OUTER_BOUND('',#16803,.T.);
#14122=FACE_OUTER_BOUND('',#16804,.T.);
#14123=FACE_OUTER_BOUND('',#16805,.T.);
#14124=FACE_OUTER_BOUND('',#16806,.T.);
#14125=FACE_OUTER_BOUND('',#16807,.T.);
#14126=FACE_OUTER_BOUND('',#16808,.T.);
#14127=FACE_OUTER_BOUND('',#16809,.T.);
#14128=FACE_OUTER_BOUND('',#16810,.T.);
#14129=FACE_OUTER_BOUND('',#16811,.T.);
#14130=FACE_OUTER_BOUND('',#16812,.T.);
#14131=FACE_OUTER_BOUND('',#16813,.T.);
#14132=FACE_OUTER_BOUND('',#16814,.T.);
#14133=FACE_OUTER_BOUND('',#16815,.T.);
#14134=FACE_OUTER_BOUND('',#16816,.T.);
#14135=FACE_OUTER_BOUND('',#16817,.T.);
#14136=FACE_OUTER_BOUND('',#16818,.T.);
#14137=FACE_OUTER_BOUND('',#16819,.T.);
#14138=FACE_OUTER_BOUND('',#16820,.T.);
#14139=FACE_OUTER_BOUND('',#16821,.T.);
#14140=FACE_OUTER_BOUND('',#16822,.T.);
#14141=FACE_OUTER_BOUND('',#16823,.T.);
#14142=FACE_OUTER_BOUND('',#16824,.T.);
#14143=FACE_OUTER_BOUND('',#16825,.T.);
#14144=FACE_OUTER_BOUND('',#16826,.T.);
#14145=FACE_OUTER_BOUND('',#16827,.T.);
#14146=FACE_OUTER_BOUND('',#16828,.T.);
#14147=FACE_OUTER_BOUND('',#16829,.T.);
#14148=FACE_OUTER_BOUND('',#16830,.T.);
#14149=FACE_OUTER_BOUND('',#16831,.T.);
#14150=FACE_OUTER_BOUND('',#16832,.T.);
#14151=FACE_OUTER_BOUND('',#16833,.T.);
#14152=FACE_OUTER_BOUND('',#16834,.T.);
#14153=FACE_OUTER_BOUND('',#16835,.T.);
#14154=FACE_OUTER_BOUND('',#16836,.T.);
#14155=FACE_OUTER_BOUND('',#16837,.T.);
#14156=FACE_OUTER_BOUND('',#16838,.T.);
#14157=FACE_OUTER_BOUND('',#16839,.T.);
#14158=FACE_OUTER_BOUND('',#16840,.T.);
#14159=FACE_OUTER_BOUND('',#16841,.T.);
#14160=FACE_OUTER_BOUND('',#16842,.T.);
#14161=FACE_OUTER_BOUND('',#16843,.T.);
#14162=FACE_OUTER_BOUND('',#16844,.T.);
#14163=FACE_OUTER_BOUND('',#16845,.T.);
#14164=FACE_OUTER_BOUND('',#16846,.T.);
#14165=FACE_OUTER_BOUND('',#16847,.T.);
#14166=FACE_OUTER_BOUND('',#16848,.T.);
#14167=FACE_OUTER_BOUND('',#16849,.T.);
#14168=FACE_OUTER_BOUND('',#16850,.T.);
#14169=FACE_OUTER_BOUND('',#16851,.T.);
#14170=FACE_OUTER_BOUND('',#16852,.T.);
#14171=FACE_OUTER_BOUND('',#16853,.T.);
#14172=FACE_OUTER_BOUND('',#16854,.T.);
#14173=FACE_OUTER_BOUND('',#16855,.T.);
#14174=FACE_OUTER_BOUND('',#16856,.T.);
#14175=FACE_OUTER_BOUND('',#16857,.T.);
#14176=FACE_OUTER_BOUND('',#16858,.T.);
#14177=FACE_OUTER_BOUND('',#16859,.T.);
#14178=FACE_OUTER_BOUND('',#16860,.T.);
#14179=FACE_OUTER_BOUND('',#16861,.T.);
#14180=FACE_OUTER_BOUND('',#16862,.T.);
#14181=FACE_OUTER_BOUND('',#16863,.T.);
#14182=FACE_OUTER_BOUND('',#16864,.T.);
#14183=FACE_OUTER_BOUND('',#16865,.T.);
#14184=FACE_OUTER_BOUND('',#16866,.T.);
#14185=FACE_OUTER_BOUND('',#16867,.T.);
#14186=FACE_OUTER_BOUND('',#16868,.T.);
#14187=FACE_OUTER_BOUND('',#16869,.T.);
#14188=FACE_OUTER_BOUND('',#16870,.T.);
#14189=FACE_OUTER_BOUND('',#16871,.T.);
#14190=FACE_OUTER_BOUND('',#16872,.T.);
#14191=FACE_OUTER_BOUND('',#16873,.T.);
#14192=FACE_OUTER_BOUND('',#16874,.T.);
#14193=FACE_OUTER_BOUND('',#16875,.T.);
#14194=FACE_OUTER_BOUND('',#16876,.T.);
#14195=FACE_OUTER_BOUND('',#16877,.T.);
#14196=FACE_OUTER_BOUND('',#16878,.T.);
#14197=FACE_OUTER_BOUND('',#16879,.T.);
#14198=FACE_OUTER_BOUND('',#16880,.T.);
#14199=FACE_OUTER_BOUND('',#16881,.T.);
#14200=FACE_OUTER_BOUND('',#16882,.T.);
#14201=FACE_OUTER_BOUND('',#16883,.T.);
#14202=FACE_OUTER_BOUND('',#16884,.T.);
#14203=FACE_OUTER_BOUND('',#16885,.T.);
#14204=FACE_OUTER_BOUND('',#16886,.T.);
#14205=FACE_OUTER_BOUND('',#16887,.T.);
#14206=FACE_OUTER_BOUND('',#16888,.T.);
#14207=FACE_OUTER_BOUND('',#16889,.T.);
#14208=FACE_OUTER_BOUND('',#16890,.T.);
#14209=FACE_OUTER_BOUND('',#16891,.T.);
#14210=FACE_OUTER_BOUND('',#16892,.T.);
#14211=FACE_OUTER_BOUND('',#16893,.T.);
#14212=FACE_OUTER_BOUND('',#16894,.T.);
#14213=FACE_OUTER_BOUND('',#16895,.T.);
#14214=FACE_OUTER_BOUND('',#16896,.T.);
#14215=FACE_OUTER_BOUND('',#16897,.T.);
#14216=FACE_OUTER_BOUND('',#16898,.T.);
#14217=FACE_OUTER_BOUND('',#16899,.T.);
#14218=FACE_OUTER_BOUND('',#16900,.T.);
#14219=FACE_OUTER_BOUND('',#16901,.T.);
#14220=FACE_OUTER_BOUND('',#16902,.T.);
#14221=FACE_OUTER_BOUND('',#16903,.T.);
#14222=FACE_OUTER_BOUND('',#16904,.T.);
#14223=FACE_OUTER_BOUND('',#16905,.T.);
#14224=FACE_OUTER_BOUND('',#16906,.T.);
#14225=FACE_OUTER_BOUND('',#16907,.T.);
#14226=FACE_OUTER_BOUND('',#16908,.T.);
#14227=FACE_OUTER_BOUND('',#16909,.T.);
#14228=FACE_OUTER_BOUND('',#16910,.T.);
#14229=FACE_OUTER_BOUND('',#16911,.T.);
#14230=FACE_OUTER_BOUND('',#16912,.T.);
#14231=FACE_OUTER_BOUND('',#16913,.T.);
#14232=FACE_OUTER_BOUND('',#16914,.T.);
#14233=FACE_OUTER_BOUND('',#16915,.T.);
#14234=FACE_OUTER_BOUND('',#16916,.T.);
#14235=FACE_OUTER_BOUND('',#16917,.T.);
#14236=FACE_OUTER_BOUND('',#16918,.T.);
#14237=FACE_OUTER_BOUND('',#16919,.T.);
#14238=FACE_OUTER_BOUND('',#16920,.T.);
#14239=FACE_OUTER_BOUND('',#16921,.T.);
#14240=FACE_OUTER_BOUND('',#16922,.T.);
#14241=FACE_OUTER_BOUND('',#16923,.T.);
#14242=FACE_OUTER_BOUND('',#16924,.T.);
#14243=FACE_OUTER_BOUND('',#16925,.T.);
#14244=FACE_OUTER_BOUND('',#16926,.T.);
#14245=FACE_OUTER_BOUND('',#16927,.T.);
#14246=FACE_OUTER_BOUND('',#16928,.T.);
#14247=FACE_OUTER_BOUND('',#16929,.T.);
#14248=FACE_OUTER_BOUND('',#16930,.T.);
#14249=FACE_OUTER_BOUND('',#16931,.T.);
#14250=FACE_OUTER_BOUND('',#16932,.T.);
#14251=FACE_OUTER_BOUND('',#16933,.T.);
#14252=FACE_OUTER_BOUND('',#16934,.T.);
#14253=FACE_OUTER_BOUND('',#16935,.T.);
#14254=FACE_OUTER_BOUND('',#16936,.T.);
#14255=FACE_OUTER_BOUND('',#16937,.T.);
#14256=FACE_OUTER_BOUND('',#16938,.T.);
#14257=FACE_OUTER_BOUND('',#16939,.T.);
#14258=FACE_OUTER_BOUND('',#16940,.T.);
#14259=FACE_OUTER_BOUND('',#16941,.T.);
#14260=FACE_OUTER_BOUND('',#16942,.T.);
#14261=FACE_OUTER_BOUND('',#16943,.T.);
#14262=FACE_OUTER_BOUND('',#16944,.T.);
#14263=FACE_OUTER_BOUND('',#16945,.T.);
#14264=FACE_OUTER_BOUND('',#16946,.T.);
#14265=FACE_OUTER_BOUND('',#16947,.T.);
#14266=FACE_OUTER_BOUND('',#16948,.T.);
#14267=FACE_OUTER_BOUND('',#16949,.T.);
#14268=FACE_OUTER_BOUND('',#16950,.T.);
#14269=FACE_OUTER_BOUND('',#16951,.T.);
#14270=FACE_OUTER_BOUND('',#16952,.T.);
#14271=FACE_OUTER_BOUND('',#16953,.T.);
#14272=FACE_OUTER_BOUND('',#16954,.T.);
#14273=FACE_OUTER_BOUND('',#16955,.T.);
#14274=FACE_OUTER_BOUND('',#16956,.T.);
#14275=FACE_OUTER_BOUND('',#16957,.T.);
#14276=FACE_OUTER_BOUND('',#16958,.T.);
#14277=FACE_OUTER_BOUND('',#16959,.T.);
#14278=FACE_OUTER_BOUND('',#16960,.T.);
#14279=FACE_OUTER_BOUND('',#16961,.T.);
#14280=FACE_OUTER_BOUND('',#16962,.T.);
#14281=FACE_OUTER_BOUND('',#16963,.T.);
#14282=FACE_OUTER_BOUND('',#16964,.T.);
#14283=FACE_OUTER_BOUND('',#16965,.T.);
#14284=FACE_OUTER_BOUND('',#16966,.T.);
#14285=FACE_OUTER_BOUND('',#16967,.T.);
#14286=FACE_OUTER_BOUND('',#16968,.T.);
#14287=FACE_OUTER_BOUND('',#16969,.T.);
#14288=FACE_OUTER_BOUND('',#16970,.T.);
#14289=FACE_OUTER_BOUND('',#16971,.T.);
#14290=FACE_OUTER_BOUND('',#16972,.T.);
#14291=FACE_OUTER_BOUND('',#16973,.T.);
#14292=FACE_OUTER_BOUND('',#16974,.T.);
#14293=FACE_OUTER_BOUND('',#16975,.T.);
#14294=FACE_OUTER_BOUND('',#16976,.T.);
#14295=FACE_OUTER_BOUND('',#16977,.T.);
#14296=FACE_OUTER_BOUND('',#16978,.T.);
#14297=FACE_OUTER_BOUND('',#16979,.T.);
#14298=FACE_OUTER_BOUND('',#16980,.T.);
#14299=FACE_OUTER_BOUND('',#16981,.T.);
#14300=FACE_OUTER_BOUND('',#16982,.T.);
#14301=FACE_OUTER_BOUND('',#16983,.T.);
#14302=FACE_OUTER_BOUND('',#16984,.T.);
#14303=FACE_OUTER_BOUND('',#16985,.T.);
#14304=FACE_OUTER_BOUND('',#16986,.T.);
#14305=FACE_OUTER_BOUND('',#16987,.T.);
#14306=FACE_OUTER_BOUND('',#16988,.T.);
#14307=FACE_OUTER_BOUND('',#16989,.T.);
#14308=FACE_OUTER_BOUND('',#16990,.T.);
#14309=FACE_OUTER_BOUND('',#16991,.T.);
#14310=FACE_OUTER_BOUND('',#16992,.T.);
#14311=FACE_OUTER_BOUND('',#16993,.T.);
#14312=FACE_OUTER_BOUND('',#16994,.T.);
#14313=FACE_OUTER_BOUND('',#16995,.T.);
#14314=FACE_OUTER_BOUND('',#16996,.T.);
#14315=FACE_OUTER_BOUND('',#16997,.T.);
#14316=FACE_OUTER_BOUND('',#16998,.T.);
#14317=FACE_OUTER_BOUND('',#16999,.T.);
#14318=FACE_OUTER_BOUND('',#17000,.T.);
#14319=FACE_OUTER_BOUND('',#17001,.T.);
#14320=FACE_OUTER_BOUND('',#17002,.T.);
#14321=FACE_OUTER_BOUND('',#17003,.T.);
#14322=FACE_OUTER_BOUND('',#17004,.T.);
#14323=FACE_OUTER_BOUND('',#17005,.T.);
#14324=FACE_OUTER_BOUND('',#17006,.T.);
#14325=FACE_OUTER_BOUND('',#17007,.T.);
#14326=FACE_OUTER_BOUND('',#17008,.T.);
#14327=FACE_OUTER_BOUND('',#17009,.T.);
#14328=FACE_OUTER_BOUND('',#17010,.T.);
#14329=FACE_OUTER_BOUND('',#17011,.T.);
#14330=FACE_OUTER_BOUND('',#17012,.T.);
#14331=FACE_OUTER_BOUND('',#17013,.T.);
#14332=FACE_OUTER_BOUND('',#17014,.T.);
#14333=FACE_OUTER_BOUND('',#17015,.T.);
#14334=FACE_OUTER_BOUND('',#17016,.T.);
#14335=FACE_OUTER_BOUND('',#17017,.T.);
#14336=FACE_OUTER_BOUND('',#17018,.T.);
#14337=FACE_OUTER_BOUND('',#17019,.T.);
#14338=FACE_OUTER_BOUND('',#17020,.T.);
#14339=FACE_OUTER_BOUND('',#17021,.T.);
#14340=FACE_OUTER_BOUND('',#17022,.T.);
#14341=FACE_OUTER_BOUND('',#17023,.T.);
#14342=FACE_OUTER_BOUND('',#17024,.T.);
#14343=FACE_OUTER_BOUND('',#17025,.T.);
#14344=FACE_OUTER_BOUND('',#17026,.T.);
#14345=FACE_OUTER_BOUND('',#17027,.T.);
#14346=FACE_OUTER_BOUND('',#17028,.T.);
#14347=FACE_OUTER_BOUND('',#17029,.T.);
#14348=FACE_OUTER_BOUND('',#17030,.T.);
#14349=FACE_OUTER_BOUND('',#17031,.T.);
#14350=FACE_OUTER_BOUND('',#17032,.T.);
#14351=FACE_OUTER_BOUND('',#17033,.T.);
#14352=FACE_OUTER_BOUND('',#17034,.T.);
#14353=FACE_OUTER_BOUND('',#17035,.T.);
#14354=FACE_OUTER_BOUND('',#17036,.T.);
#14355=FACE_OUTER_BOUND('',#17037,.T.);
#14356=FACE_OUTER_BOUND('',#17038,.T.);
#14357=FACE_OUTER_BOUND('',#17039,.T.);
#14358=FACE_OUTER_BOUND('',#17040,.T.);
#14359=FACE_OUTER_BOUND('',#17041,.T.);
#14360=FACE_OUTER_BOUND('',#17042,.T.);
#14361=FACE_OUTER_BOUND('',#17043,.T.);
#14362=FACE_OUTER_BOUND('',#17044,.T.);
#14363=FACE_OUTER_BOUND('',#17045,.T.);
#14364=FACE_OUTER_BOUND('',#17046,.T.);
#14365=FACE_OUTER_BOUND('',#17047,.T.);
#14366=FACE_OUTER_BOUND('',#17048,.T.);
#14367=FACE_OUTER_BOUND('',#17049,.T.);
#14368=FACE_OUTER_BOUND('',#17050,.T.);
#14369=FACE_OUTER_BOUND('',#17051,.T.);
#14370=FACE_OUTER_BOUND('',#17052,.T.);
#14371=FACE_OUTER_BOUND('',#17053,.T.);
#14372=FACE_OUTER_BOUND('',#17054,.T.);
#14373=FACE_OUTER_BOUND('',#17055,.T.);
#14374=FACE_OUTER_BOUND('',#17056,.T.);
#14375=FACE_OUTER_BOUND('',#17057,.T.);
#14376=FACE_OUTER_BOUND('',#17058,.T.);
#14377=FACE_OUTER_BOUND('',#17059,.T.);
#14378=FACE_OUTER_BOUND('',#17060,.T.);
#14379=FACE_OUTER_BOUND('',#17061,.T.);
#14380=FACE_OUTER_BOUND('',#17062,.T.);
#14381=FACE_OUTER_BOUND('',#17063,.T.);
#14382=FACE_OUTER_BOUND('',#17064,.T.);
#14383=FACE_OUTER_BOUND('',#17065,.T.);
#14384=FACE_OUTER_BOUND('',#17066,.T.);
#14385=FACE_OUTER_BOUND('',#17067,.T.);
#14386=FACE_OUTER_BOUND('',#17068,.T.);
#14387=FACE_OUTER_BOUND('',#17069,.T.);
#14388=FACE_OUTER_BOUND('',#17070,.T.);
#14389=FACE_OUTER_BOUND('',#17071,.T.);
#14390=FACE_OUTER_BOUND('',#17072,.T.);
#14391=FACE_OUTER_BOUND('',#17073,.T.);
#14392=FACE_OUTER_BOUND('',#17074,.T.);
#14393=FACE_OUTER_BOUND('',#17075,.T.);
#14394=FACE_OUTER_BOUND('',#17076,.T.);
#14395=FACE_OUTER_BOUND('',#17077,.T.);
#14396=FACE_OUTER_BOUND('',#17078,.T.);
#14397=FACE_OUTER_BOUND('',#17079,.T.);
#14398=FACE_OUTER_BOUND('',#17080,.T.);
#14399=FACE_OUTER_BOUND('',#17081,.T.);
#14400=FACE_OUTER_BOUND('',#17082,.T.);
#14401=FACE_OUTER_BOUND('',#17083,.T.);
#14402=FACE_OUTER_BOUND('',#17084,.T.);
#14403=FACE_OUTER_BOUND('',#17085,.T.);
#14404=FACE_OUTER_BOUND('',#17086,.T.);
#14405=FACE_OUTER_BOUND('',#17087,.T.);
#14406=FACE_OUTER_BOUND('',#17088,.T.);
#14407=FACE_OUTER_BOUND('',#17089,.T.);
#14408=FACE_OUTER_BOUND('',#17090,.T.);
#14409=FACE_OUTER_BOUND('',#17091,.T.);
#14410=FACE_OUTER_BOUND('',#17092,.T.);
#14411=FACE_OUTER_BOUND('',#17093,.T.);
#14412=FACE_OUTER_BOUND('',#17094,.T.);
#14413=FACE_OUTER_BOUND('',#17095,.T.);
#14414=FACE_OUTER_BOUND('',#17096,.T.);
#14415=FACE_OUTER_BOUND('',#17097,.T.);
#14416=FACE_OUTER_BOUND('',#17098,.T.);
#14417=FACE_OUTER_BOUND('',#17099,.T.);
#14418=FACE_OUTER_BOUND('',#17100,.T.);
#14419=FACE_OUTER_BOUND('',#17101,.T.);
#14420=FACE_OUTER_BOUND('',#17102,.T.);
#14421=FACE_OUTER_BOUND('',#17103,.T.);
#14422=FACE_OUTER_BOUND('',#17104,.T.);
#14423=FACE_OUTER_BOUND('',#17105,.T.);
#14424=FACE_OUTER_BOUND('',#17106,.T.);
#14425=FACE_OUTER_BOUND('',#17107,.T.);
#14426=FACE_OUTER_BOUND('',#17108,.T.);
#14427=FACE_OUTER_BOUND('',#17109,.T.);
#14428=FACE_OUTER_BOUND('',#17110,.T.);
#14429=FACE_OUTER_BOUND('',#17111,.T.);
#14430=FACE_OUTER_BOUND('',#17112,.T.);
#14431=FACE_OUTER_BOUND('',#17113,.T.);
#14432=FACE_OUTER_BOUND('',#17114,.T.);
#14433=FACE_OUTER_BOUND('',#17115,.T.);
#14434=FACE_OUTER_BOUND('',#17116,.T.);
#14435=FACE_OUTER_BOUND('',#17117,.T.);
#14436=FACE_OUTER_BOUND('',#17118,.T.);
#14437=FACE_OUTER_BOUND('',#17119,.T.);
#14438=FACE_OUTER_BOUND('',#17120,.T.);
#14439=FACE_OUTER_BOUND('',#17121,.T.);
#14440=FACE_OUTER_BOUND('',#17122,.T.);
#14441=FACE_OUTER_BOUND('',#17123,.T.);
#14442=FACE_OUTER_BOUND('',#17124,.T.);
#14443=FACE_OUTER_BOUND('',#17125,.T.);
#14444=FACE_OUTER_BOUND('',#17126,.T.);
#14445=FACE_OUTER_BOUND('',#17127,.T.);
#14446=FACE_OUTER_BOUND('',#17128,.T.);
#14447=FACE_OUTER_BOUND('',#17129,.T.);
#14448=FACE_OUTER_BOUND('',#17130,.T.);
#14449=FACE_OUTER_BOUND('',#17131,.T.);
#14450=FACE_OUTER_BOUND('',#17132,.T.);
#14451=FACE_OUTER_BOUND('',#17133,.T.);
#14452=FACE_OUTER_BOUND('',#17134,.T.);
#14453=FACE_OUTER_BOUND('',#17135,.T.);
#14454=FACE_OUTER_BOUND('',#17136,.T.);
#14455=FACE_OUTER_BOUND('',#17137,.T.);
#14456=FACE_OUTER_BOUND('',#17138,.T.);
#14457=FACE_OUTER_BOUND('',#17139,.T.);
#14458=FACE_OUTER_BOUND('',#17140,.T.);
#14459=FACE_OUTER_BOUND('',#17141,.T.);
#14460=FACE_OUTER_BOUND('',#17142,.T.);
#14461=FACE_OUTER_BOUND('',#17143,.T.);
#14462=FACE_OUTER_BOUND('',#17144,.T.);
#14463=FACE_OUTER_BOUND('',#17145,.T.);
#14464=FACE_OUTER_BOUND('',#17146,.T.);
#14465=FACE_OUTER_BOUND('',#17147,.T.);
#14466=FACE_OUTER_BOUND('',#17148,.T.);
#14467=FACE_OUTER_BOUND('',#17149,.T.);
#14468=FACE_OUTER_BOUND('',#17150,.T.);
#14469=FACE_OUTER_BOUND('',#17151,.T.);
#14470=FACE_OUTER_BOUND('',#17152,.T.);
#14471=FACE_OUTER_BOUND('',#17153,.T.);
#14472=FACE_OUTER_BOUND('',#17154,.T.);
#14473=FACE_OUTER_BOUND('',#17155,.T.);
#14474=FACE_OUTER_BOUND('',#17156,.T.);
#14475=FACE_OUTER_BOUND('',#17157,.T.);
#14476=FACE_OUTER_BOUND('',#17158,.T.);
#14477=FACE_OUTER_BOUND('',#17159,.T.);
#14478=FACE_OUTER_BOUND('',#17160,.T.);
#14479=FACE_OUTER_BOUND('',#17161,.T.);
#14480=FACE_OUTER_BOUND('',#17162,.T.);
#14481=FACE_OUTER_BOUND('',#17163,.T.);
#14482=FACE_OUTER_BOUND('',#17164,.T.);
#14483=FACE_OUTER_BOUND('',#17165,.T.);
#14484=FACE_OUTER_BOUND('',#17166,.T.);
#14485=FACE_OUTER_BOUND('',#17167,.T.);
#14486=FACE_OUTER_BOUND('',#17168,.T.);
#14487=FACE_OUTER_BOUND('',#17169,.T.);
#14488=FACE_OUTER_BOUND('',#17170,.T.);
#14489=FACE_OUTER_BOUND('',#17171,.T.);
#14490=FACE_OUTER_BOUND('',#17172,.T.);
#14491=FACE_OUTER_BOUND('',#17173,.T.);
#14492=FACE_OUTER_BOUND('',#17174,.T.);
#14493=FACE_OUTER_BOUND('',#17175,.T.);
#14494=FACE_OUTER_BOUND('',#17176,.T.);
#14495=FACE_OUTER_BOUND('',#17177,.T.);
#14496=FACE_OUTER_BOUND('',#17178,.T.);
#14497=FACE_OUTER_BOUND('',#17179,.T.);
#14498=FACE_OUTER_BOUND('',#17180,.T.);
#14499=FACE_OUTER_BOUND('',#17181,.T.);
#14500=FACE_OUTER_BOUND('',#17182,.T.);
#14501=FACE_OUTER_BOUND('',#17183,.T.);
#14502=FACE_OUTER_BOUND('',#17184,.T.);
#14503=FACE_OUTER_BOUND('',#17185,.T.);
#14504=FACE_OUTER_BOUND('',#17186,.T.);
#14505=FACE_OUTER_BOUND('',#17187,.T.);
#14506=FACE_OUTER_BOUND('',#17188,.T.);
#14507=FACE_OUTER_BOUND('',#17189,.T.);
#14508=FACE_OUTER_BOUND('',#17190,.T.);
#14509=FACE_OUTER_BOUND('',#17191,.T.);
#14510=FACE_OUTER_BOUND('',#17192,.T.);
#14511=FACE_OUTER_BOUND('',#17193,.T.);
#14512=FACE_OUTER_BOUND('',#17194,.T.);
#14513=FACE_OUTER_BOUND('',#17195,.T.);
#14514=FACE_OUTER_BOUND('',#17196,.T.);
#14515=FACE_OUTER_BOUND('',#17197,.T.);
#14516=FACE_OUTER_BOUND('',#17198,.T.);
#14517=FACE_OUTER_BOUND('',#17199,.T.);
#14518=FACE_OUTER_BOUND('',#17200,.T.);
#14519=FACE_OUTER_BOUND('',#17201,.T.);
#14520=FACE_OUTER_BOUND('',#17202,.T.);
#14521=FACE_OUTER_BOUND('',#17203,.T.);
#14522=FACE_OUTER_BOUND('',#17204,.T.);
#14523=FACE_OUTER_BOUND('',#17205,.T.);
#14524=FACE_OUTER_BOUND('',#17206,.T.);
#14525=FACE_OUTER_BOUND('',#17207,.T.);
#14526=FACE_OUTER_BOUND('',#17208,.T.);
#14527=FACE_OUTER_BOUND('',#17209,.T.);
#14528=FACE_OUTER_BOUND('',#17210,.T.);
#14529=FACE_OUTER_BOUND('',#17211,.T.);
#14530=FACE_OUTER_BOUND('',#17212,.T.);
#14531=FACE_OUTER_BOUND('',#17213,.T.);
#14532=FACE_OUTER_BOUND('',#17214,.T.);
#14533=FACE_OUTER_BOUND('',#17215,.T.);
#14534=FACE_OUTER_BOUND('',#17216,.T.);
#14535=FACE_OUTER_BOUND('',#17217,.T.);
#14536=FACE_OUTER_BOUND('',#17218,.T.);
#14537=FACE_OUTER_BOUND('',#17219,.T.);
#14538=FACE_OUTER_BOUND('',#17220,.T.);
#14539=FACE_OUTER_BOUND('',#17221,.T.);
#14540=FACE_OUTER_BOUND('',#17222,.T.);
#14541=FACE_OUTER_BOUND('',#17223,.T.);
#14542=FACE_OUTER_BOUND('',#17224,.T.);
#14543=FACE_OUTER_BOUND('',#17225,.T.);
#14544=FACE_OUTER_BOUND('',#17226,.T.);
#14545=FACE_OUTER_BOUND('',#17227,.T.);
#14546=FACE_OUTER_BOUND('',#17228,.T.);
#14547=FACE_OUTER_BOUND('',#17229,.T.);
#14548=FACE_OUTER_BOUND('',#17230,.T.);
#14549=FACE_OUTER_BOUND('',#17231,.T.);
#14550=FACE_OUTER_BOUND('',#17232,.T.);
#14551=FACE_OUTER_BOUND('',#17233,.T.);
#14552=FACE_OUTER_BOUND('',#17234,.T.);
#14553=FACE_OUTER_BOUND('',#17235,.T.);
#14554=FACE_OUTER_BOUND('',#17236,.T.);
#14555=FACE_OUTER_BOUND('',#17237,.T.);
#14556=FACE_OUTER_BOUND('',#17238,.T.);
#14557=FACE_OUTER_BOUND('',#17239,.T.);
#14558=FACE_OUTER_BOUND('',#17240,.T.);
#14559=FACE_OUTER_BOUND('',#17241,.T.);
#14560=FACE_OUTER_BOUND('',#17242,.T.);
#14561=FACE_OUTER_BOUND('',#17243,.T.);
#14562=FACE_OUTER_BOUND('',#17244,.T.);
#14563=FACE_OUTER_BOUND('',#17245,.T.);
#14564=FACE_OUTER_BOUND('',#17246,.T.);
#14565=FACE_OUTER_BOUND('',#17247,.T.);
#14566=FACE_OUTER_BOUND('',#17248,.T.);
#14567=FACE_OUTER_BOUND('',#17249,.T.);
#14568=FACE_OUTER_BOUND('',#17250,.T.);
#14569=FACE_OUTER_BOUND('',#17251,.T.);
#14570=FACE_OUTER_BOUND('',#17252,.T.);
#14571=FACE_OUTER_BOUND('',#17253,.T.);
#14572=FACE_OUTER_BOUND('',#17254,.T.);
#14573=FACE_OUTER_BOUND('',#17255,.T.);
#14574=FACE_OUTER_BOUND('',#17256,.T.);
#14575=FACE_OUTER_BOUND('',#17257,.T.);
#14576=FACE_OUTER_BOUND('',#17258,.T.);
#14577=FACE_OUTER_BOUND('',#17259,.T.);
#14578=FACE_OUTER_BOUND('',#17260,.T.);
#14579=FACE_OUTER_BOUND('',#17261,.T.);
#14580=FACE_OUTER_BOUND('',#17262,.T.);
#14581=FACE_OUTER_BOUND('',#17263,.T.);
#14582=FACE_OUTER_BOUND('',#17264,.T.);
#14583=FACE_OUTER_BOUND('',#17265,.T.);
#14584=FACE_OUTER_BOUND('',#17266,.T.);
#14585=FACE_OUTER_BOUND('',#17267,.T.);
#14586=FACE_OUTER_BOUND('',#17268,.T.);
#14587=FACE_OUTER_BOUND('',#17269,.T.);
#14588=FACE_OUTER_BOUND('',#17270,.T.);
#14589=FACE_OUTER_BOUND('',#17271,.T.);
#14590=FACE_OUTER_BOUND('',#17272,.T.);
#14591=FACE_OUTER_BOUND('',#17273,.T.);
#14592=FACE_OUTER_BOUND('',#17274,.T.);
#14593=FACE_OUTER_BOUND('',#17275,.T.);
#14594=FACE_OUTER_BOUND('',#17276,.T.);
#14595=FACE_OUTER_BOUND('',#17277,.T.);
#14596=FACE_OUTER_BOUND('',#17278,.T.);
#14597=FACE_OUTER_BOUND('',#17279,.T.);
#14598=FACE_OUTER_BOUND('',#17280,.T.);
#14599=FACE_OUTER_BOUND('',#17281,.T.);
#14600=FACE_OUTER_BOUND('',#17282,.T.);
#14601=FACE_OUTER_BOUND('',#17283,.T.);
#14602=FACE_OUTER_BOUND('',#17284,.T.);
#14603=FACE_OUTER_BOUND('',#17285,.T.);
#14604=FACE_OUTER_BOUND('',#17286,.T.);
#14605=FACE_OUTER_BOUND('',#17287,.T.);
#14606=FACE_OUTER_BOUND('',#17288,.T.);
#14607=FACE_OUTER_BOUND('',#17289,.T.);
#14608=FACE_OUTER_BOUND('',#17290,.T.);
#14609=FACE_OUTER_BOUND('',#17291,.T.);
#14610=FACE_OUTER_BOUND('',#17292,.T.);
#14611=FACE_OUTER_BOUND('',#17293,.T.);
#14612=FACE_OUTER_BOUND('',#17294,.T.);
#14613=FACE_OUTER_BOUND('',#17295,.T.);
#14614=FACE_OUTER_BOUND('',#17296,.T.);
#14615=FACE_OUTER_BOUND('',#17297,.T.);
#14616=FACE_OUTER_BOUND('',#17298,.T.);
#14617=FACE_OUTER_BOUND('',#17299,.T.);
#14618=FACE_OUTER_BOUND('',#17300,.T.);
#14619=FACE_OUTER_BOUND('',#17301,.T.);
#14620=FACE_OUTER_BOUND('',#17302,.T.);
#14621=FACE_OUTER_BOUND('',#17304,.T.);
#14622=FACE_OUTER_BOUND('',#17305,.T.);
#14623=FACE_OUTER_BOUND('',#17306,.T.);
#14624=FACE_OUTER_BOUND('',#17307,.T.);
#14625=FACE_OUTER_BOUND('',#17308,.T.);
#14626=FACE_OUTER_BOUND('',#17310,.T.);
#14627=FACE_OUTER_BOUND('',#17311,.T.);
#14628=FACE_OUTER_BOUND('',#17313,.T.);
#14629=FACE_OUTER_BOUND('',#17314,.T.);
#14630=FACE_OUTER_BOUND('',#17316,.T.);
#14631=FACE_OUTER_BOUND('',#17317,.T.);
#14632=FACE_OUTER_BOUND('',#17318,.T.);
#14633=FACE_OUTER_BOUND('',#17319,.T.);
#14634=FACE_OUTER_BOUND('',#17320,.T.);
#14635=FACE_OUTER_BOUND('',#17321,.T.);
#14636=FACE_OUTER_BOUND('',#17322,.T.);
#14637=FACE_OUTER_BOUND('',#17323,.T.);
#14638=FACE_OUTER_BOUND('',#17324,.T.);
#14639=FACE_OUTER_BOUND('',#17325,.T.);
#14640=FACE_OUTER_BOUND('',#17326,.T.);
#14641=FACE_OUTER_BOUND('',#17328,.T.);
#14642=FACE_OUTER_BOUND('',#17329,.T.);
#14643=FACE_OUTER_BOUND('',#17330,.T.);
#14644=FACE_OUTER_BOUND('',#17331,.T.);
#14645=FACE_OUTER_BOUND('',#17332,.T.);
#14646=FACE_OUTER_BOUND('',#17333,.T.);
#14647=FACE_OUTER_BOUND('',#17334,.T.);
#14648=FACE_OUTER_BOUND('',#17335,.T.);
#14649=FACE_OUTER_BOUND('',#17336,.T.);
#14650=FACE_OUTER_BOUND('',#17337,.T.);
#14651=FACE_OUTER_BOUND('',#17338,.T.);
#14652=FACE_OUTER_BOUND('',#17339,.T.);
#14653=FACE_OUTER_BOUND('',#17340,.T.);
#14654=FACE_OUTER_BOUND('',#17341,.T.);
#14655=FACE_OUTER_BOUND('',#17342,.T.);
#14656=FACE_OUTER_BOUND('',#17343,.T.);
#14657=FACE_OUTER_BOUND('',#17344,.T.);
#14658=FACE_OUTER_BOUND('',#17345,.T.);
#14659=FACE_OUTER_BOUND('',#17346,.T.);
#14660=FACE_OUTER_BOUND('',#17347,.T.);
#14661=FACE_OUTER_BOUND('',#17348,.T.);
#14662=FACE_OUTER_BOUND('',#17349,.T.);
#14663=FACE_OUTER_BOUND('',#17350,.T.);
#14664=FACE_OUTER_BOUND('',#17351,.T.);
#14665=FACE_OUTER_BOUND('',#17352,.T.);
#14666=FACE_OUTER_BOUND('',#17353,.T.);
#14667=FACE_OUTER_BOUND('',#17354,.T.);
#14668=FACE_OUTER_BOUND('',#17355,.T.);
#14669=FACE_OUTER_BOUND('',#17356,.T.);
#14670=FACE_OUTER_BOUND('',#17357,.T.);
#14671=FACE_OUTER_BOUND('',#17358,.T.);
#14672=FACE_OUTER_BOUND('',#17359,.T.);
#14673=FACE_OUTER_BOUND('',#17360,.T.);
#14674=FACE_OUTER_BOUND('',#17361,.T.);
#14675=FACE_OUTER_BOUND('',#17362,.T.);
#14676=FACE_OUTER_BOUND('',#17363,.T.);
#14677=FACE_OUTER_BOUND('',#17364,.T.);
#14678=FACE_OUTER_BOUND('',#17365,.T.);
#14679=FACE_OUTER_BOUND('',#17366,.T.);
#14680=FACE_OUTER_BOUND('',#17367,.T.);
#14681=FACE_OUTER_BOUND('',#17368,.T.);
#14682=FACE_OUTER_BOUND('',#17369,.T.);
#14683=FACE_OUTER_BOUND('',#17370,.T.);
#14684=FACE_OUTER_BOUND('',#17371,.T.);
#14685=FACE_OUTER_BOUND('',#17372,.T.);
#14686=FACE_OUTER_BOUND('',#17373,.T.);
#14687=FACE_OUTER_BOUND('',#17374,.T.);
#14688=FACE_OUTER_BOUND('',#17375,.T.);
#14689=FACE_OUTER_BOUND('',#17376,.T.);
#14690=FACE_OUTER_BOUND('',#17377,.T.);
#14691=FACE_OUTER_BOUND('',#17378,.T.);
#14692=FACE_OUTER_BOUND('',#17379,.T.);
#14693=FACE_OUTER_BOUND('',#17380,.T.);
#14694=FACE_OUTER_BOUND('',#17381,.T.);
#14695=FACE_OUTER_BOUND('',#17382,.T.);
#14696=FACE_OUTER_BOUND('',#17383,.T.);
#14697=FACE_OUTER_BOUND('',#17384,.T.);
#14698=FACE_OUTER_BOUND('',#17385,.T.);
#14699=FACE_OUTER_BOUND('',#17386,.T.);
#14700=FACE_OUTER_BOUND('',#17387,.T.);
#14701=FACE_OUTER_BOUND('',#17388,.T.);
#14702=FACE_OUTER_BOUND('',#17389,.T.);
#14703=FACE_OUTER_BOUND('',#17390,.T.);
#14704=FACE_OUTER_BOUND('',#17391,.T.);
#14705=FACE_OUTER_BOUND('',#17392,.T.);
#14706=FACE_OUTER_BOUND('',#17393,.T.);
#14707=FACE_OUTER_BOUND('',#17394,.T.);
#14708=FACE_OUTER_BOUND('',#17395,.T.);
#14709=FACE_OUTER_BOUND('',#17396,.T.);
#14710=FACE_OUTER_BOUND('',#17397,.T.);
#14711=FACE_OUTER_BOUND('',#17398,.T.);
#14712=FACE_OUTER_BOUND('',#17399,.T.);
#14713=FACE_OUTER_BOUND('',#17400,.T.);
#14714=FACE_OUTER_BOUND('',#17401,.T.);
#14715=FACE_OUTER_BOUND('',#17402,.T.);
#14716=FACE_OUTER_BOUND('',#17403,.T.);
#14717=FACE_OUTER_BOUND('',#17404,.T.);
#14718=FACE_OUTER_BOUND('',#17405,.T.);
#14719=FACE_OUTER_BOUND('',#17406,.T.);
#14720=FACE_OUTER_BOUND('',#17407,.T.);
#14721=FACE_OUTER_BOUND('',#17408,.T.);
#14722=FACE_OUTER_BOUND('',#17409,.T.);
#14723=FACE_OUTER_BOUND('',#17410,.T.);
#14724=FACE_OUTER_BOUND('',#17411,.T.);
#14725=FACE_OUTER_BOUND('',#17412,.T.);
#14726=FACE_OUTER_BOUND('',#17413,.T.);
#14727=FACE_OUTER_BOUND('',#17414,.T.);
#14728=FACE_OUTER_BOUND('',#17415,.T.);
#14729=FACE_OUTER_BOUND('',#17416,.T.);
#14730=FACE_OUTER_BOUND('',#17417,.T.);
#14731=FACE_OUTER_BOUND('',#17418,.T.);
#14732=FACE_OUTER_BOUND('',#17419,.T.);
#14733=FACE_OUTER_BOUND('',#17420,.T.);
#14734=FACE_OUTER_BOUND('',#17421,.T.);
#14735=FACE_OUTER_BOUND('',#17422,.T.);
#14736=FACE_OUTER_BOUND('',#17423,.T.);
#14737=FACE_OUTER_BOUND('',#17424,.T.);
#14738=FACE_OUTER_BOUND('',#17425,.T.);
#14739=FACE_OUTER_BOUND('',#17426,.T.);
#14740=FACE_OUTER_BOUND('',#17427,.T.);
#14741=FACE_OUTER_BOUND('',#17428,.T.);
#14742=FACE_OUTER_BOUND('',#17429,.T.);
#14743=FACE_OUTER_BOUND('',#17430,.T.);
#14744=FACE_OUTER_BOUND('',#17431,.T.);
#14745=FACE_OUTER_BOUND('',#17432,.T.);
#14746=FACE_OUTER_BOUND('',#17433,.T.);
#14747=FACE_OUTER_BOUND('',#17434,.T.);
#14748=FACE_OUTER_BOUND('',#17435,.T.);
#14749=FACE_OUTER_BOUND('',#17436,.T.);
#14750=FACE_OUTER_BOUND('',#17437,.T.);
#14751=FACE_OUTER_BOUND('',#17438,.T.);
#14752=FACE_OUTER_BOUND('',#17439,.T.);
#14753=FACE_OUTER_BOUND('',#17440,.T.);
#14754=FACE_OUTER_BOUND('',#17441,.T.);
#14755=FACE_OUTER_BOUND('',#17442,.T.);
#14756=FACE_OUTER_BOUND('',#17443,.T.);
#14757=FACE_OUTER_BOUND('',#17444,.T.);
#14758=FACE_OUTER_BOUND('',#17445,.T.);
#14759=FACE_OUTER_BOUND('',#17446,.T.);
#14760=FACE_OUTER_BOUND('',#17447,.T.);
#14761=FACE_OUTER_BOUND('',#17448,.T.);
#14762=FACE_OUTER_BOUND('',#17449,.T.);
#14763=FACE_OUTER_BOUND('',#17450,.T.);
#14764=FACE_OUTER_BOUND('',#17451,.T.);
#14765=FACE_OUTER_BOUND('',#17452,.T.);
#14766=FACE_OUTER_BOUND('',#17453,.T.);
#14767=FACE_OUTER_BOUND('',#17454,.T.);
#14768=FACE_OUTER_BOUND('',#17455,.T.);
#14769=FACE_OUTER_BOUND('',#17456,.T.);
#14770=FACE_OUTER_BOUND('',#17457,.T.);
#14771=FACE_OUTER_BOUND('',#17458,.T.);
#14772=FACE_OUTER_BOUND('',#17459,.T.);
#14773=FACE_OUTER_BOUND('',#17460,.T.);
#14774=FACE_OUTER_BOUND('',#17461,.T.);
#14775=FACE_OUTER_BOUND('',#17462,.T.);
#14776=FACE_OUTER_BOUND('',#17463,.T.);
#14777=FACE_OUTER_BOUND('',#17464,.T.);
#14778=FACE_OUTER_BOUND('',#17465,.T.);
#14779=FACE_OUTER_BOUND('',#17466,.T.);
#14780=FACE_OUTER_BOUND('',#17467,.T.);
#14781=FACE_OUTER_BOUND('',#17468,.T.);
#14782=FACE_OUTER_BOUND('',#17469,.T.);
#14783=FACE_OUTER_BOUND('',#17470,.T.);
#14784=FACE_OUTER_BOUND('',#17471,.T.);
#14785=FACE_OUTER_BOUND('',#17472,.T.);
#14786=FACE_OUTER_BOUND('',#17473,.T.);
#14787=FACE_OUTER_BOUND('',#17474,.T.);
#14788=FACE_OUTER_BOUND('',#17475,.T.);
#14789=FACE_OUTER_BOUND('',#17476,.T.);
#14790=FACE_OUTER_BOUND('',#17477,.T.);
#14791=FACE_OUTER_BOUND('',#17478,.T.);
#14792=FACE_OUTER_BOUND('',#17479,.T.);
#14793=FACE_OUTER_BOUND('',#17480,.T.);
#14794=FACE_OUTER_BOUND('',#17481,.T.);
#14795=FACE_OUTER_BOUND('',#17482,.T.);
#14796=FACE_OUTER_BOUND('',#17483,.T.);
#14797=FACE_OUTER_BOUND('',#17484,.T.);
#14798=FACE_OUTER_BOUND('',#17485,.T.);
#14799=FACE_OUTER_BOUND('',#17486,.T.);
#14800=FACE_OUTER_BOUND('',#17487,.T.);
#14801=FACE_OUTER_BOUND('',#17488,.T.);
#14802=FACE_OUTER_BOUND('',#17489,.T.);
#14803=FACE_OUTER_BOUND('',#17490,.T.);
#14804=FACE_OUTER_BOUND('',#17491,.T.);
#14805=FACE_OUTER_BOUND('',#17492,.T.);
#14806=FACE_OUTER_BOUND('',#17493,.T.);
#14807=FACE_OUTER_BOUND('',#17494,.T.);
#14808=FACE_OUTER_BOUND('',#17495,.T.);
#14809=FACE_OUTER_BOUND('',#17496,.T.);
#14810=FACE_OUTER_BOUND('',#17497,.T.);
#14811=FACE_OUTER_BOUND('',#17498,.T.);
#14812=FACE_OUTER_BOUND('',#17499,.T.);
#14813=FACE_OUTER_BOUND('',#17500,.T.);
#14814=FACE_OUTER_BOUND('',#17501,.T.);
#14815=FACE_OUTER_BOUND('',#17502,.T.);
#14816=FACE_OUTER_BOUND('',#17503,.T.);
#14817=FACE_OUTER_BOUND('',#17504,.T.);
#14818=FACE_OUTER_BOUND('',#17505,.T.);
#14819=FACE_OUTER_BOUND('',#17506,.T.);
#14820=FACE_OUTER_BOUND('',#17507,.T.);
#14821=FACE_OUTER_BOUND('',#17508,.T.);
#14822=FACE_OUTER_BOUND('',#17509,.T.);
#14823=FACE_OUTER_BOUND('',#17510,.T.);
#14824=FACE_OUTER_BOUND('',#17511,.T.);
#14825=FACE_OUTER_BOUND('',#17512,.T.);
#14826=FACE_OUTER_BOUND('',#17513,.T.);
#14827=FACE_OUTER_BOUND('',#17514,.T.);
#14828=FACE_OUTER_BOUND('',#17515,.T.);
#14829=FACE_OUTER_BOUND('',#17516,.T.);
#14830=FACE_OUTER_BOUND('',#17517,.T.);
#14831=FACE_OUTER_BOUND('',#17518,.T.);
#14832=FACE_OUTER_BOUND('',#17519,.T.);
#14833=FACE_OUTER_BOUND('',#17520,.T.);
#14834=FACE_OUTER_BOUND('',#17521,.T.);
#14835=FACE_OUTER_BOUND('',#17522,.T.);
#14836=FACE_OUTER_BOUND('',#17523,.T.);
#14837=FACE_OUTER_BOUND('',#17524,.T.);
#14838=FACE_OUTER_BOUND('',#17525,.T.);
#14839=FACE_OUTER_BOUND('',#17526,.T.);
#14840=FACE_OUTER_BOUND('',#17527,.T.);
#14841=FACE_OUTER_BOUND('',#17528,.T.);
#14842=FACE_OUTER_BOUND('',#17529,.T.);
#14843=FACE_OUTER_BOUND('',#17530,.T.);
#14844=FACE_OUTER_BOUND('',#17531,.T.);
#14845=FACE_OUTER_BOUND('',#17532,.T.);
#14846=FACE_OUTER_BOUND('',#17533,.T.);
#14847=FACE_OUTER_BOUND('',#17534,.T.);
#14848=FACE_OUTER_BOUND('',#17535,.T.);
#14849=FACE_OUTER_BOUND('',#17536,.T.);
#14850=FACE_OUTER_BOUND('',#17537,.T.);
#14851=FACE_OUTER_BOUND('',#17538,.T.);
#14852=FACE_OUTER_BOUND('',#17539,.T.);
#14853=FACE_OUTER_BOUND('',#17540,.T.);
#14854=FACE_OUTER_BOUND('',#17541,.T.);
#14855=FACE_OUTER_BOUND('',#17542,.T.);
#14856=FACE_OUTER_BOUND('',#17543,.T.);
#14857=FACE_OUTER_BOUND('',#17544,.T.);
#14858=FACE_OUTER_BOUND('',#17545,.T.);
#14859=FACE_OUTER_BOUND('',#17546,.T.);
#14860=FACE_OUTER_BOUND('',#17547,.T.);
#14861=FACE_OUTER_BOUND('',#17548,.T.);
#14862=FACE_OUTER_BOUND('',#17549,.T.);
#14863=FACE_OUTER_BOUND('',#17550,.T.);
#14864=FACE_OUTER_BOUND('',#17551,.T.);
#14865=FACE_OUTER_BOUND('',#17552,.T.);
#14866=FACE_OUTER_BOUND('',#17553,.T.);
#14867=FACE_OUTER_BOUND('',#17554,.T.);
#14868=FACE_OUTER_BOUND('',#17555,.T.);
#14869=FACE_OUTER_BOUND('',#17556,.T.);
#14870=FACE_OUTER_BOUND('',#17557,.T.);
#14871=FACE_OUTER_BOUND('',#17558,.T.);
#14872=FACE_OUTER_BOUND('',#17559,.T.);
#14873=FACE_OUTER_BOUND('',#17560,.T.);
#14874=FACE_OUTER_BOUND('',#17561,.T.);
#14875=FACE_OUTER_BOUND('',#17562,.T.);
#14876=FACE_OUTER_BOUND('',#17563,.T.);
#14877=FACE_OUTER_BOUND('',#17564,.T.);
#14878=FACE_OUTER_BOUND('',#17565,.T.);
#14879=FACE_OUTER_BOUND('',#17566,.T.);
#14880=FACE_OUTER_BOUND('',#17567,.T.);
#14881=FACE_OUTER_BOUND('',#17568,.T.);
#14882=FACE_OUTER_BOUND('',#17569,.T.);
#14883=FACE_OUTER_BOUND('',#17570,.T.);
#14884=FACE_OUTER_BOUND('',#17571,.T.);
#14885=FACE_OUTER_BOUND('',#17572,.T.);
#14886=FACE_OUTER_BOUND('',#17573,.T.);
#14887=FACE_OUTER_BOUND('',#17574,.T.);
#14888=FACE_OUTER_BOUND('',#17575,.T.);
#14889=FACE_OUTER_BOUND('',#17576,.T.);
#14890=FACE_OUTER_BOUND('',#17577,.T.);
#14891=FACE_OUTER_BOUND('',#17578,.T.);
#14892=FACE_OUTER_BOUND('',#17579,.T.);
#14893=FACE_OUTER_BOUND('',#17580,.T.);
#14894=FACE_OUTER_BOUND('',#17581,.T.);
#14895=FACE_OUTER_BOUND('',#17582,.T.);
#14896=FACE_OUTER_BOUND('',#17583,.T.);
#14897=FACE_OUTER_BOUND('',#17584,.T.);
#14898=FACE_OUTER_BOUND('',#17585,.T.);
#14899=FACE_OUTER_BOUND('',#17586,.T.);
#14900=FACE_OUTER_BOUND('',#17587,.T.);
#14901=FACE_OUTER_BOUND('',#17588,.T.);
#14902=FACE_OUTER_BOUND('',#17589,.T.);
#14903=FACE_OUTER_BOUND('',#17590,.T.);
#14904=FACE_OUTER_BOUND('',#17591,.T.);
#14905=FACE_OUTER_BOUND('',#17592,.T.);
#14906=FACE_OUTER_BOUND('',#17593,.T.);
#14907=FACE_OUTER_BOUND('',#17594,.T.);
#14908=FACE_OUTER_BOUND('',#17595,.T.);
#14909=FACE_OUTER_BOUND('',#17596,.T.);
#14910=FACE_OUTER_BOUND('',#17597,.T.);
#14911=FACE_OUTER_BOUND('',#17598,.T.);
#14912=FACE_OUTER_BOUND('',#17599,.T.);
#14913=FACE_OUTER_BOUND('',#17600,.T.);
#14914=FACE_OUTER_BOUND('',#17601,.T.);
#14915=FACE_OUTER_BOUND('',#17602,.T.);
#14916=FACE_OUTER_BOUND('',#17603,.T.);
#14917=FACE_OUTER_BOUND('',#17604,.T.);
#14918=FACE_OUTER_BOUND('',#17605,.T.);
#14919=FACE_OUTER_BOUND('',#17606,.T.);
#14920=FACE_OUTER_BOUND('',#17607,.T.);
#14921=FACE_OUTER_BOUND('',#17608,.T.);
#14922=FACE_OUTER_BOUND('',#17609,.T.);
#14923=FACE_OUTER_BOUND('',#17610,.T.);
#14924=FACE_OUTER_BOUND('',#17611,.T.);
#14925=FACE_OUTER_BOUND('',#17612,.T.);
#14926=FACE_OUTER_BOUND('',#17613,.T.);
#14927=FACE_OUTER_BOUND('',#17614,.T.);
#14928=FACE_OUTER_BOUND('',#17615,.T.);
#14929=FACE_OUTER_BOUND('',#17616,.T.);
#14930=FACE_OUTER_BOUND('',#17617,.T.);
#14931=FACE_OUTER_BOUND('',#17618,.T.);
#14932=FACE_OUTER_BOUND('',#17619,.T.);
#14933=FACE_OUTER_BOUND('',#17620,.T.);
#14934=FACE_OUTER_BOUND('',#17621,.T.);
#14935=FACE_OUTER_BOUND('',#17622,.T.);
#14936=FACE_OUTER_BOUND('',#17623,.T.);
#14937=FACE_OUTER_BOUND('',#17624,.T.);
#14938=FACE_OUTER_BOUND('',#17625,.T.);
#14939=FACE_OUTER_BOUND('',#17626,.T.);
#14940=FACE_OUTER_BOUND('',#17627,.T.);
#14941=FACE_OUTER_BOUND('',#17628,.T.);
#14942=FACE_OUTER_BOUND('',#17629,.T.);
#14943=FACE_OUTER_BOUND('',#17630,.T.);
#14944=FACE_OUTER_BOUND('',#17631,.T.);
#14945=FACE_OUTER_BOUND('',#17632,.T.);
#14946=FACE_OUTER_BOUND('',#17633,.T.);
#14947=FACE_OUTER_BOUND('',#17634,.T.);
#14948=FACE_OUTER_BOUND('',#17635,.T.);
#14949=FACE_OUTER_BOUND('',#17636,.T.);
#14950=FACE_OUTER_BOUND('',#17637,.T.);
#14951=FACE_OUTER_BOUND('',#17638,.T.);
#14952=FACE_OUTER_BOUND('',#17639,.T.);
#14953=FACE_OUTER_BOUND('',#17640,.T.);
#14954=FACE_OUTER_BOUND('',#17641,.T.);
#14955=FACE_OUTER_BOUND('',#17642,.T.);
#14956=FACE_OUTER_BOUND('',#17643,.T.);
#14957=FACE_OUTER_BOUND('',#17644,.T.);
#14958=FACE_OUTER_BOUND('',#17645,.T.);
#14959=FACE_OUTER_BOUND('',#17646,.T.);
#14960=FACE_OUTER_BOUND('',#17647,.T.);
#14961=FACE_OUTER_BOUND('',#17648,.T.);
#14962=FACE_OUTER_BOUND('',#17649,.T.);
#14963=FACE_OUTER_BOUND('',#17650,.T.);
#14964=FACE_OUTER_BOUND('',#17651,.T.);
#14965=FACE_OUTER_BOUND('',#17652,.T.);
#14966=FACE_OUTER_BOUND('',#17653,.T.);
#14967=FACE_OUTER_BOUND('',#17654,.T.);
#14968=FACE_OUTER_BOUND('',#17655,.T.);
#14969=FACE_OUTER_BOUND('',#17656,.T.);
#14970=FACE_OUTER_BOUND('',#17657,.T.);
#14971=FACE_OUTER_BOUND('',#17658,.T.);
#14972=FACE_OUTER_BOUND('',#17659,.T.);
#14973=FACE_OUTER_BOUND('',#17660,.T.);
#14974=FACE_OUTER_BOUND('',#17661,.T.);
#14975=FACE_OUTER_BOUND('',#17662,.T.);
#14976=FACE_OUTER_BOUND('',#17663,.T.);
#14977=FACE_OUTER_BOUND('',#17664,.T.);
#14978=FACE_OUTER_BOUND('',#17665,.T.);
#14979=FACE_OUTER_BOUND('',#17666,.T.);
#14980=FACE_OUTER_BOUND('',#17667,.T.);
#14981=FACE_OUTER_BOUND('',#17668,.T.);
#14982=FACE_OUTER_BOUND('',#17669,.T.);
#14983=FACE_OUTER_BOUND('',#17670,.T.);
#14984=FACE_OUTER_BOUND('',#17671,.T.);
#14985=FACE_OUTER_BOUND('',#17672,.T.);
#14986=FACE_OUTER_BOUND('',#17674,.T.);
#14987=FACE_OUTER_BOUND('',#17675,.T.);
#14988=FACE_OUTER_BOUND('',#17676,.T.);
#14989=FACE_OUTER_BOUND('',#17678,.T.);
#14990=FACE_OUTER_BOUND('',#17679,.T.);
#14991=FACE_OUTER_BOUND('',#17680,.T.);
#14992=FACE_OUTER_BOUND('',#17681,.T.);
#14993=FACE_OUTER_BOUND('',#17682,.T.);
#14994=FACE_OUTER_BOUND('',#17683,.T.);
#14995=FACE_OUTER_BOUND('',#17684,.T.);
#14996=FACE_OUTER_BOUND('',#17685,.T.);
#14997=FACE_OUTER_BOUND('',#17687,.T.);
#14998=FACE_OUTER_BOUND('',#17689,.T.);
#14999=FACE_OUTER_BOUND('',#17691,.T.);
#15000=FACE_OUTER_BOUND('',#17692,.T.);
#15001=FACE_OUTER_BOUND('',#17693,.T.);
#15002=FACE_OUTER_BOUND('',#17701,.T.);
#15003=FACE_OUTER_BOUND('',#17702,.T.);
#15004=FACE_OUTER_BOUND('',#17703,.T.);
#15005=FACE_OUTER_BOUND('',#17704,.T.);
#15006=FACE_OUTER_BOUND('',#17705,.T.);
#15007=FACE_OUTER_BOUND('',#17706,.T.);
#15008=FACE_OUTER_BOUND('',#17707,.T.);
#15009=FACE_OUTER_BOUND('',#17708,.T.);
#15010=FACE_OUTER_BOUND('',#17709,.T.);
#15011=FACE_OUTER_BOUND('',#17711,.T.);
#15012=FACE_OUTER_BOUND('',#17712,.T.);
#15013=FACE_OUTER_BOUND('',#17714,.T.);
#15014=FACE_OUTER_BOUND('',#17715,.T.);
#15015=FACE_OUTER_BOUND('',#17717,.T.);
#15016=FACE_OUTER_BOUND('',#17718,.T.);
#15017=FACE_OUTER_BOUND('',#17720,.T.);
#15018=FACE_OUTER_BOUND('',#17721,.T.);
#15019=FACE_OUTER_BOUND('',#17722,.T.);
#15020=FACE_OUTER_BOUND('',#17723,.T.);
#15021=FACE_OUTER_BOUND('',#17724,.T.);
#15022=FACE_OUTER_BOUND('',#17725,.T.);
#15023=FACE_OUTER_BOUND('',#17726,.T.);
#15024=FACE_OUTER_BOUND('',#17727,.T.);
#15025=FACE_OUTER_BOUND('',#17728,.T.);
#15026=FACE_OUTER_BOUND('',#17736,.T.);
#15027=FACE_OUTER_BOUND('',#17737,.T.);
#15028=FACE_OUTER_BOUND('',#17738,.T.);
#15029=FACE_OUTER_BOUND('',#17739,.T.);
#15030=FACE_OUTER_BOUND('',#17741,.T.);
#15031=FACE_OUTER_BOUND('',#17742,.T.);
#15032=FACE_OUTER_BOUND('',#17743,.T.);
#15033=FACE_OUTER_BOUND('',#17745,.T.);
#15034=FACE_OUTER_BOUND('',#17746,.T.);
#15035=FACE_OUTER_BOUND('',#17747,.T.);
#15036=FACE_OUTER_BOUND('',#17748,.T.);
#15037=FACE_OUTER_BOUND('',#17749,.T.);
#15038=FACE_OUTER_BOUND('',#17750,.T.);
#15039=FACE_OUTER_BOUND('',#17751,.T.);
#15040=FACE_OUTER_BOUND('',#17752,.T.);
#15041=FACE_OUTER_BOUND('',#17753,.T.);
#15042=FACE_OUTER_BOUND('',#17754,.T.);
#15043=FACE_OUTER_BOUND('',#17755,.T.);
#15044=FACE_OUTER_BOUND('',#17756,.T.);
#15045=FACE_OUTER_BOUND('',#17757,.T.);
#15046=FACE_OUTER_BOUND('',#17758,.T.);
#15047=FACE_OUTER_BOUND('',#17759,.T.);
#15048=FACE_OUTER_BOUND('',#17760,.T.);
#15049=FACE_OUTER_BOUND('',#17761,.T.);
#15050=FACE_OUTER_BOUND('',#17762,.T.);
#15051=FACE_OUTER_BOUND('',#17763,.T.);
#15052=FACE_OUTER_BOUND('',#17764,.T.);
#15053=FACE_OUTER_BOUND('',#17765,.T.);
#15054=FACE_OUTER_BOUND('',#17766,.T.);
#15055=FACE_OUTER_BOUND('',#17767,.T.);
#15056=FACE_OUTER_BOUND('',#17768,.T.);
#15057=FACE_OUTER_BOUND('',#17769,.T.);
#15058=FACE_OUTER_BOUND('',#17770,.T.);
#15059=FACE_OUTER_BOUND('',#17771,.T.);
#15060=FACE_OUTER_BOUND('',#17772,.T.);
#15061=FACE_OUTER_BOUND('',#17773,.T.);
#15062=FACE_OUTER_BOUND('',#17774,.T.);
#15063=FACE_OUTER_BOUND('',#17775,.T.);
#15064=FACE_OUTER_BOUND('',#17776,.T.);
#15065=FACE_OUTER_BOUND('',#17777,.T.);
#15066=FACE_OUTER_BOUND('',#17778,.T.);
#15067=FACE_OUTER_BOUND('',#17779,.T.);
#15068=FACE_OUTER_BOUND('',#17780,.T.);
#15069=FACE_OUTER_BOUND('',#17781,.T.);
#15070=FACE_OUTER_BOUND('',#17782,.T.);
#15071=FACE_OUTER_BOUND('',#17783,.T.);
#15072=FACE_OUTER_BOUND('',#17784,.T.);
#15073=FACE_OUTER_BOUND('',#17785,.T.);
#15074=FACE_OUTER_BOUND('',#17786,.T.);
#15075=FACE_OUTER_BOUND('',#17787,.T.);
#15076=FACE_OUTER_BOUND('',#17788,.T.);
#15077=FACE_OUTER_BOUND('',#17789,.T.);
#15078=FACE_OUTER_BOUND('',#17790,.T.);
#15079=FACE_OUTER_BOUND('',#17791,.T.);
#15080=FACE_OUTER_BOUND('',#17792,.T.);
#15081=FACE_OUTER_BOUND('',#17793,.T.);
#15082=FACE_OUTER_BOUND('',#17794,.T.);
#15083=FACE_OUTER_BOUND('',#17795,.T.);
#15084=FACE_OUTER_BOUND('',#17796,.T.);
#15085=FACE_OUTER_BOUND('',#17797,.T.);
#15086=FACE_OUTER_BOUND('',#17798,.T.);
#15087=FACE_OUTER_BOUND('',#17799,.T.);
#15088=FACE_OUTER_BOUND('',#17800,.T.);
#15089=FACE_OUTER_BOUND('',#17801,.T.);
#15090=FACE_OUTER_BOUND('',#17802,.T.);
#15091=FACE_OUTER_BOUND('',#17803,.T.);
#15092=FACE_OUTER_BOUND('',#17804,.T.);
#15093=FACE_OUTER_BOUND('',#17805,.T.);
#15094=FACE_OUTER_BOUND('',#17806,.T.);
#15095=FACE_OUTER_BOUND('',#17807,.T.);
#15096=FACE_OUTER_BOUND('',#17808,.T.);
#15097=FACE_OUTER_BOUND('',#17809,.T.);
#15098=FACE_OUTER_BOUND('',#17810,.T.);
#15099=FACE_OUTER_BOUND('',#17811,.T.);
#15100=FACE_OUTER_BOUND('',#17812,.T.);
#15101=FACE_OUTER_BOUND('',#17813,.T.);
#15102=FACE_OUTER_BOUND('',#17814,.T.);
#15103=FACE_OUTER_BOUND('',#17815,.T.);
#15104=FACE_OUTER_BOUND('',#17816,.T.);
#15105=FACE_OUTER_BOUND('',#17817,.T.);
#15106=FACE_OUTER_BOUND('',#17818,.T.);
#15107=FACE_OUTER_BOUND('',#17819,.T.);
#15108=FACE_OUTER_BOUND('',#17820,.T.);
#15109=FACE_OUTER_BOUND('',#17821,.T.);
#15110=FACE_OUTER_BOUND('',#17822,.T.);
#15111=FACE_OUTER_BOUND('',#17823,.T.);
#15112=FACE_OUTER_BOUND('',#17824,.T.);
#15113=FACE_OUTER_BOUND('',#17825,.T.);
#15114=FACE_OUTER_BOUND('',#17826,.T.);
#15115=FACE_OUTER_BOUND('',#17827,.T.);
#15116=FACE_OUTER_BOUND('',#17828,.T.);
#15117=FACE_OUTER_BOUND('',#17829,.T.);
#15118=FACE_OUTER_BOUND('',#17830,.T.);
#15119=FACE_OUTER_BOUND('',#17831,.T.);
#15120=FACE_OUTER_BOUND('',#17832,.T.);
#15121=FACE_OUTER_BOUND('',#17833,.T.);
#15122=FACE_OUTER_BOUND('',#17834,.T.);
#15123=FACE_OUTER_BOUND('',#17835,.T.);
#15124=FACE_OUTER_BOUND('',#17836,.T.);
#15125=FACE_OUTER_BOUND('',#17837,.T.);
#15126=FACE_OUTER_BOUND('',#17838,.T.);
#15127=FACE_OUTER_BOUND('',#17839,.T.);
#15128=FACE_OUTER_BOUND('',#17840,.T.);
#15129=FACE_OUTER_BOUND('',#17841,.T.);
#15130=FACE_OUTER_BOUND('',#17842,.T.);
#15131=FACE_OUTER_BOUND('',#17843,.T.);
#15132=FACE_OUTER_BOUND('',#17844,.T.);
#15133=FACE_OUTER_BOUND('',#17845,.T.);
#15134=FACE_OUTER_BOUND('',#17846,.T.);
#15135=FACE_OUTER_BOUND('',#17847,.T.);
#15136=FACE_OUTER_BOUND('',#17848,.T.);
#15137=FACE_OUTER_BOUND('',#17849,.T.);
#15138=FACE_OUTER_BOUND('',#17850,.T.);
#15139=FACE_OUTER_BOUND('',#17851,.T.);
#15140=FACE_OUTER_BOUND('',#17852,.T.);
#15141=FACE_OUTER_BOUND('',#17853,.T.);
#15142=FACE_OUTER_BOUND('',#17854,.T.);
#15143=FACE_OUTER_BOUND('',#17855,.T.);
#15144=FACE_OUTER_BOUND('',#17856,.T.);
#15145=FACE_OUTER_BOUND('',#17857,.T.);
#15146=FACE_OUTER_BOUND('',#17858,.T.);
#15147=FACE_OUTER_BOUND('',#17859,.T.);
#15148=FACE_OUTER_BOUND('',#17860,.T.);
#15149=FACE_OUTER_BOUND('',#17861,.T.);
#15150=FACE_OUTER_BOUND('',#17862,.T.);
#15151=FACE_OUTER_BOUND('',#17863,.T.);
#15152=FACE_OUTER_BOUND('',#17864,.T.);
#15153=FACE_OUTER_BOUND('',#17865,.T.);
#15154=FACE_OUTER_BOUND('',#17866,.T.);
#15155=FACE_OUTER_BOUND('',#17867,.T.);
#15156=FACE_OUTER_BOUND('',#17868,.T.);
#15157=FACE_OUTER_BOUND('',#17869,.T.);
#15158=FACE_OUTER_BOUND('',#17870,.T.);
#15159=FACE_OUTER_BOUND('',#17871,.T.);
#15160=FACE_OUTER_BOUND('',#17872,.T.);
#15161=FACE_OUTER_BOUND('',#17873,.T.);
#15162=FACE_OUTER_BOUND('',#17874,.T.);
#15163=FACE_OUTER_BOUND('',#17875,.T.);
#15164=FACE_OUTER_BOUND('',#17876,.T.);
#15165=FACE_OUTER_BOUND('',#17877,.T.);
#15166=FACE_OUTER_BOUND('',#17878,.T.);
#15167=FACE_OUTER_BOUND('',#17879,.T.);
#15168=FACE_OUTER_BOUND('',#17880,.T.);
#15169=FACE_OUTER_BOUND('',#17881,.T.);
#15170=FACE_OUTER_BOUND('',#17882,.T.);
#15171=FACE_OUTER_BOUND('',#17883,.T.);
#15172=FACE_OUTER_BOUND('',#17884,.T.);
#15173=FACE_OUTER_BOUND('',#17885,.T.);
#15174=FACE_OUTER_BOUND('',#17886,.T.);
#15175=FACE_OUTER_BOUND('',#17887,.T.);
#15176=FACE_OUTER_BOUND('',#17888,.T.);
#15177=FACE_OUTER_BOUND('',#17889,.T.);
#15178=FACE_OUTER_BOUND('',#17890,.T.);
#15179=FACE_OUTER_BOUND('',#17891,.T.);
#15180=FACE_OUTER_BOUND('',#17892,.T.);
#15181=FACE_OUTER_BOUND('',#17893,.T.);
#15182=FACE_OUTER_BOUND('',#17894,.T.);
#15183=FACE_OUTER_BOUND('',#17895,.T.);
#15184=FACE_OUTER_BOUND('',#17896,.T.);
#15185=FACE_OUTER_BOUND('',#17897,.T.);
#15186=FACE_OUTER_BOUND('',#17898,.T.);
#15187=FACE_OUTER_BOUND('',#17899,.T.);
#15188=FACE_OUTER_BOUND('',#17900,.T.);
#15189=FACE_OUTER_BOUND('',#17901,.T.);
#15190=FACE_OUTER_BOUND('',#17902,.T.);
#15191=FACE_OUTER_BOUND('',#17903,.T.);
#15192=FACE_OUTER_BOUND('',#17904,.T.);
#15193=FACE_OUTER_BOUND('',#17905,.T.);
#15194=FACE_OUTER_BOUND('',#17906,.T.);
#15195=FACE_OUTER_BOUND('',#17907,.T.);
#15196=FACE_OUTER_BOUND('',#17908,.T.);
#15197=FACE_OUTER_BOUND('',#17909,.T.);
#15198=FACE_OUTER_BOUND('',#17910,.T.);
#15199=FACE_OUTER_BOUND('',#17911,.T.);
#15200=FACE_OUTER_BOUND('',#17912,.T.);
#15201=FACE_OUTER_BOUND('',#17913,.T.);
#15202=FACE_OUTER_BOUND('',#17914,.T.);
#15203=FACE_OUTER_BOUND('',#17915,.T.);
#15204=FACE_OUTER_BOUND('',#17916,.T.);
#15205=FACE_OUTER_BOUND('',#17917,.T.);
#15206=FACE_OUTER_BOUND('',#17918,.T.);
#15207=FACE_OUTER_BOUND('',#17919,.T.);
#15208=FACE_OUTER_BOUND('',#17920,.T.);
#15209=FACE_OUTER_BOUND('',#17921,.T.);
#15210=FACE_OUTER_BOUND('',#17922,.T.);
#15211=FACE_OUTER_BOUND('',#17923,.T.);
#15212=FACE_OUTER_BOUND('',#17924,.T.);
#15213=FACE_OUTER_BOUND('',#17925,.T.);
#15214=FACE_OUTER_BOUND('',#17926,.T.);
#15215=FACE_OUTER_BOUND('',#17927,.T.);
#15216=FACE_OUTER_BOUND('',#17928,.T.);
#15217=FACE_OUTER_BOUND('',#17929,.T.);
#15218=FACE_OUTER_BOUND('',#17930,.T.);
#15219=FACE_OUTER_BOUND('',#17931,.T.);
#15220=FACE_OUTER_BOUND('',#17932,.T.);
#15221=FACE_OUTER_BOUND('',#17933,.T.);
#15222=FACE_OUTER_BOUND('',#17934,.T.);
#15223=FACE_OUTER_BOUND('',#17935,.T.);
#15224=FACE_OUTER_BOUND('',#17936,.T.);
#15225=FACE_OUTER_BOUND('',#17937,.T.);
#15226=FACE_OUTER_BOUND('',#17938,.T.);
#15227=FACE_OUTER_BOUND('',#17939,.T.);
#15228=FACE_OUTER_BOUND('',#17940,.T.);
#15229=FACE_OUTER_BOUND('',#17941,.T.);
#15230=FACE_OUTER_BOUND('',#17942,.T.);
#15231=FACE_OUTER_BOUND('',#17943,.T.);
#15232=FACE_OUTER_BOUND('',#17944,.T.);
#15233=FACE_OUTER_BOUND('',#17945,.T.);
#15234=FACE_OUTER_BOUND('',#17946,.T.);
#15235=FACE_OUTER_BOUND('',#17947,.T.);
#15236=FACE_OUTER_BOUND('',#17948,.T.);
#15237=FACE_OUTER_BOUND('',#17949,.T.);
#15238=FACE_OUTER_BOUND('',#17950,.T.);
#15239=FACE_OUTER_BOUND('',#17951,.T.);
#15240=FACE_OUTER_BOUND('',#17952,.T.);
#15241=FACE_OUTER_BOUND('',#17953,.T.);
#15242=FACE_OUTER_BOUND('',#17954,.T.);
#15243=FACE_OUTER_BOUND('',#17955,.T.);
#15244=FACE_OUTER_BOUND('',#17956,.T.);
#15245=FACE_OUTER_BOUND('',#17957,.T.);
#15246=FACE_OUTER_BOUND('',#17958,.T.);
#15247=FACE_OUTER_BOUND('',#17959,.T.);
#15248=FACE_OUTER_BOUND('',#17960,.T.);
#15249=FACE_OUTER_BOUND('',#17961,.T.);
#15250=FACE_OUTER_BOUND('',#17962,.T.);
#15251=FACE_OUTER_BOUND('',#17963,.T.);
#15252=FACE_OUTER_BOUND('',#17964,.T.);
#15253=FACE_OUTER_BOUND('',#17965,.T.);
#15254=FACE_OUTER_BOUND('',#17966,.T.);
#15255=FACE_OUTER_BOUND('',#17967,.T.);
#15256=FACE_OUTER_BOUND('',#17968,.T.);
#15257=FACE_OUTER_BOUND('',#17969,.T.);
#15258=FACE_OUTER_BOUND('',#17970,.T.);
#15259=FACE_OUTER_BOUND('',#17971,.T.);
#15260=FACE_OUTER_BOUND('',#17972,.T.);
#15261=FACE_OUTER_BOUND('',#17973,.T.);
#15262=FACE_OUTER_BOUND('',#17974,.T.);
#15263=FACE_OUTER_BOUND('',#17975,.T.);
#15264=FACE_OUTER_BOUND('',#17976,.T.);
#15265=FACE_OUTER_BOUND('',#17977,.T.);
#15266=FACE_OUTER_BOUND('',#17978,.T.);
#15267=FACE_OUTER_BOUND('',#17979,.T.);
#15268=FACE_OUTER_BOUND('',#17980,.T.);
#15269=FACE_OUTER_BOUND('',#17981,.T.);
#15270=FACE_OUTER_BOUND('',#17982,.T.);
#15271=FACE_OUTER_BOUND('',#17983,.T.);
#15272=FACE_OUTER_BOUND('',#17984,.T.);
#15273=FACE_OUTER_BOUND('',#17985,.T.);
#15274=FACE_OUTER_BOUND('',#17986,.T.);
#15275=FACE_OUTER_BOUND('',#17987,.T.);
#15276=FACE_OUTER_BOUND('',#17988,.T.);
#15277=FACE_OUTER_BOUND('',#17989,.T.);
#15278=FACE_OUTER_BOUND('',#17990,.T.);
#15279=FACE_OUTER_BOUND('',#17991,.T.);
#15280=FACE_OUTER_BOUND('',#17992,.T.);
#15281=FACE_OUTER_BOUND('',#17993,.T.);
#15282=FACE_OUTER_BOUND('',#17994,.T.);
#15283=FACE_OUTER_BOUND('',#17995,.T.);
#15284=FACE_OUTER_BOUND('',#17996,.T.);
#15285=FACE_OUTER_BOUND('',#17997,.T.);
#15286=FACE_OUTER_BOUND('',#17998,.T.);
#15287=FACE_OUTER_BOUND('',#17999,.T.);
#15288=FACE_OUTER_BOUND('',#18000,.T.);
#15289=FACE_OUTER_BOUND('',#18001,.T.);
#15290=FACE_OUTER_BOUND('',#18002,.T.);
#15291=FACE_OUTER_BOUND('',#18003,.T.);
#15292=FACE_OUTER_BOUND('',#18004,.T.);
#15293=FACE_OUTER_BOUND('',#18005,.T.);
#15294=FACE_OUTER_BOUND('',#18006,.T.);
#15295=FACE_OUTER_BOUND('',#18007,.T.);
#15296=FACE_OUTER_BOUND('',#18008,.T.);
#15297=FACE_OUTER_BOUND('',#18009,.T.);
#15298=FACE_OUTER_BOUND('',#18010,.T.);
#15299=FACE_OUTER_BOUND('',#18011,.T.);
#15300=FACE_OUTER_BOUND('',#18012,.T.);
#15301=FACE_OUTER_BOUND('',#18013,.T.);
#15302=FACE_OUTER_BOUND('',#18014,.T.);
#15303=FACE_OUTER_BOUND('',#18015,.T.);
#15304=FACE_OUTER_BOUND('',#18016,.T.);
#15305=FACE_OUTER_BOUND('',#18017,.T.);
#15306=FACE_OUTER_BOUND('',#18018,.T.);
#15307=FACE_OUTER_BOUND('',#18019,.T.);
#15308=FACE_OUTER_BOUND('',#18020,.T.);
#15309=FACE_OUTER_BOUND('',#18021,.T.);
#15310=FACE_OUTER_BOUND('',#18022,.T.);
#15311=FACE_OUTER_BOUND('',#18023,.T.);
#15312=FACE_OUTER_BOUND('',#18024,.T.);
#15313=FACE_OUTER_BOUND('',#18025,.T.);
#15314=FACE_OUTER_BOUND('',#18026,.T.);
#15315=FACE_OUTER_BOUND('',#18027,.T.);
#15316=FACE_OUTER_BOUND('',#18028,.T.);
#15317=FACE_OUTER_BOUND('',#18029,.T.);
#15318=FACE_OUTER_BOUND('',#18030,.T.);
#15319=FACE_OUTER_BOUND('',#18031,.T.);
#15320=FACE_OUTER_BOUND('',#18032,.T.);
#15321=FACE_OUTER_BOUND('',#18033,.T.);
#15322=FACE_OUTER_BOUND('',#18034,.T.);
#15323=FACE_OUTER_BOUND('',#18035,.T.);
#15324=FACE_OUTER_BOUND('',#18036,.T.);
#15325=FACE_OUTER_BOUND('',#18037,.T.);
#15326=FACE_OUTER_BOUND('',#18038,.T.);
#15327=FACE_OUTER_BOUND('',#18039,.T.);
#15328=FACE_OUTER_BOUND('',#18040,.T.);
#15329=FACE_OUTER_BOUND('',#18041,.T.);
#15330=FACE_OUTER_BOUND('',#18042,.T.);
#15331=FACE_OUTER_BOUND('',#18043,.T.);
#15332=FACE_OUTER_BOUND('',#18044,.T.);
#15333=FACE_OUTER_BOUND('',#18045,.T.);
#15334=FACE_OUTER_BOUND('',#18046,.T.);
#15335=FACE_OUTER_BOUND('',#18047,.T.);
#15336=FACE_OUTER_BOUND('',#18048,.T.);
#15337=FACE_OUTER_BOUND('',#18049,.T.);
#15338=FACE_OUTER_BOUND('',#18050,.T.);
#15339=FACE_OUTER_BOUND('',#18051,.T.);
#15340=FACE_OUTER_BOUND('',#18052,.T.);
#15341=FACE_OUTER_BOUND('',#18053,.T.);
#15342=FACE_OUTER_BOUND('',#18054,.T.);
#15343=FACE_OUTER_BOUND('',#18055,.T.);
#15344=FACE_OUTER_BOUND('',#18056,.T.);
#15345=FACE_OUTER_BOUND('',#18057,.T.);
#15346=FACE_OUTER_BOUND('',#18058,.T.);
#15347=FACE_OUTER_BOUND('',#18059,.T.);
#15348=FACE_OUTER_BOUND('',#18060,.T.);
#15349=FACE_OUTER_BOUND('',#18061,.T.);
#15350=FACE_OUTER_BOUND('',#18085,.T.);
#15351=FACE_OUTER_BOUND('',#18086,.T.);
#15352=FACE_OUTER_BOUND('',#18087,.T.);
#15353=FACE_OUTER_BOUND('',#18100,.T.);
#15354=FACE_OUTER_BOUND('',#18101,.T.);
#15355=FACE_OUTER_BOUND('',#18106,.T.);
#15356=FACE_OUTER_BOUND('',#18107,.T.);
#15357=FACE_OUTER_BOUND('',#18108,.T.);
#15358=FACE_OUTER_BOUND('',#18109,.T.);
#15359=FACE_OUTER_BOUND('',#18110,.T.);
#15360=FACE_OUTER_BOUND('',#18111,.T.);
#15361=FACE_OUTER_BOUND('',#18112,.T.);
#15362=FACE_OUTER_BOUND('',#18113,.T.);
#15363=FACE_OUTER_BOUND('',#18114,.T.);
#15364=FACE_OUTER_BOUND('',#18115,.T.);
#15365=FACE_OUTER_BOUND('',#18116,.T.);
#15366=FACE_OUTER_BOUND('',#18117,.T.);
#15367=FACE_OUTER_BOUND('',#18118,.T.);
#15368=FACE_OUTER_BOUND('',#18119,.T.);
#15369=FACE_OUTER_BOUND('',#18120,.T.);
#15370=FACE_OUTER_BOUND('',#18121,.T.);
#15371=FACE_OUTER_BOUND('',#18122,.T.);
#15372=FACE_OUTER_BOUND('',#18123,.T.);
#15373=FACE_OUTER_BOUND('',#18124,.T.);
#15374=FACE_OUTER_BOUND('',#18125,.T.);
#15375=FACE_OUTER_BOUND('',#18126,.T.);
#15376=FACE_OUTER_BOUND('',#18127,.T.);
#15377=FACE_OUTER_BOUND('',#18128,.T.);
#15378=FACE_OUTER_BOUND('',#18129,.T.);
#15379=FACE_OUTER_BOUND('',#18130,.T.);
#15380=FACE_OUTER_BOUND('',#18131,.T.);
#15381=FACE_OUTER_BOUND('',#18132,.T.);
#15382=FACE_OUTER_BOUND('',#18133,.T.);
#15383=FACE_OUTER_BOUND('',#18134,.T.);
#15384=FACE_OUTER_BOUND('',#18135,.T.);
#15385=FACE_OUTER_BOUND('',#18136,.T.);
#15386=FACE_OUTER_BOUND('',#18137,.T.);
#15387=FACE_OUTER_BOUND('',#18138,.T.);
#15388=FACE_OUTER_BOUND('',#18139,.T.);
#15389=FACE_OUTER_BOUND('',#18140,.T.);
#15390=FACE_OUTER_BOUND('',#18141,.T.);
#15391=FACE_OUTER_BOUND('',#18142,.T.);
#15392=FACE_OUTER_BOUND('',#18143,.T.);
#15393=FACE_OUTER_BOUND('',#18144,.T.);
#15394=FACE_OUTER_BOUND('',#18145,.T.);
#15395=FACE_OUTER_BOUND('',#18146,.T.);
#15396=FACE_OUTER_BOUND('',#18147,.T.);
#15397=FACE_OUTER_BOUND('',#18148,.T.);
#15398=FACE_OUTER_BOUND('',#18149,.T.);
#15399=FACE_OUTER_BOUND('',#18150,.T.);
#15400=FACE_OUTER_BOUND('',#18151,.T.);
#15401=FACE_OUTER_BOUND('',#18152,.T.);
#15402=FACE_OUTER_BOUND('',#18153,.T.);
#15403=FACE_OUTER_BOUND('',#18154,.T.);
#15404=FACE_OUTER_BOUND('',#18155,.T.);
#15405=FACE_OUTER_BOUND('',#18156,.T.);
#15406=FACE_OUTER_BOUND('',#18157,.T.);
#15407=FACE_OUTER_BOUND('',#18158,.T.);
#15408=FACE_OUTER_BOUND('',#18159,.T.);
#15409=FACE_OUTER_BOUND('',#18161,.T.);
#15410=FACE_OUTER_BOUND('',#18162,.T.);
#15411=FACE_OUTER_BOUND('',#18163,.T.);
#15412=FACE_OUTER_BOUND('',#18164,.T.);
#15413=FACE_OUTER_BOUND('',#18166,.T.);
#15414=FACE_OUTER_BOUND('',#18167,.T.);
#15415=FACE_OUTER_BOUND('',#18168,.T.);
#15416=FACE_OUTER_BOUND('',#18169,.T.);
#15417=FACE_OUTER_BOUND('',#18170,.T.);
#15418=FACE_OUTER_BOUND('',#18171,.T.);
#15419=FACE_OUTER_BOUND('',#18172,.T.);
#15420=FACE_OUTER_BOUND('',#18173,.T.);
#15421=FACE_OUTER_BOUND('',#18174,.T.);
#15422=FACE_OUTER_BOUND('',#18175,.T.);
#15423=FACE_OUTER_BOUND('',#18176,.T.);
#15424=FACE_OUTER_BOUND('',#18177,.T.);
#15425=FACE_OUTER_BOUND('',#18178,.T.);
#15426=FACE_OUTER_BOUND('',#18179,.T.);
#15427=FACE_OUTER_BOUND('',#18180,.T.);
#15428=FACE_OUTER_BOUND('',#18181,.T.);
#15429=FACE_OUTER_BOUND('',#18182,.T.);
#15430=FACE_OUTER_BOUND('',#18183,.T.);
#15431=FACE_OUTER_BOUND('',#18184,.T.);
#15432=FACE_OUTER_BOUND('',#18185,.T.);
#15433=FACE_OUTER_BOUND('',#18186,.T.);
#15434=FACE_OUTER_BOUND('',#18187,.T.);
#15435=FACE_OUTER_BOUND('',#18188,.T.);
#15436=FACE_OUTER_BOUND('',#18189,.T.);
#15437=FACE_OUTER_BOUND('',#18190,.T.);
#15438=FACE_OUTER_BOUND('',#18191,.T.);
#15439=FACE_OUTER_BOUND('',#18192,.T.);
#15440=FACE_OUTER_BOUND('',#18193,.T.);
#15441=FACE_OUTER_BOUND('',#18194,.T.);
#15442=FACE_OUTER_BOUND('',#18195,.T.);
#15443=FACE_OUTER_BOUND('',#18196,.T.);
#15444=FACE_OUTER_BOUND('',#18197,.T.);
#15445=FACE_OUTER_BOUND('',#18198,.T.);
#15446=FACE_OUTER_BOUND('',#18199,.T.);
#15447=FACE_OUTER_BOUND('',#18200,.T.);
#15448=FACE_OUTER_BOUND('',#18201,.T.);
#15449=FACE_OUTER_BOUND('',#18202,.T.);
#15450=FACE_OUTER_BOUND('',#18203,.T.);
#15451=FACE_OUTER_BOUND('',#18204,.T.);
#15452=FACE_OUTER_BOUND('',#18205,.T.);
#15453=FACE_OUTER_BOUND('',#18206,.T.);
#15454=FACE_OUTER_BOUND('',#18208,.T.);
#15455=FACE_OUTER_BOUND('',#18209,.T.);
#15456=FACE_OUTER_BOUND('',#18210,.T.);
#15457=FACE_OUTER_BOUND('',#18211,.T.);
#15458=FACE_OUTER_BOUND('',#18212,.T.);
#15459=FACE_OUTER_BOUND('',#18213,.T.);
#15460=FACE_OUTER_BOUND('',#18214,.T.);
#15461=FACE_OUTER_BOUND('',#18215,.T.);
#15462=FACE_OUTER_BOUND('',#18216,.T.);
#15463=FACE_OUTER_BOUND('',#18217,.T.);
#15464=FACE_OUTER_BOUND('',#18218,.T.);
#15465=FACE_OUTER_BOUND('',#18219,.T.);
#15466=FACE_OUTER_BOUND('',#18220,.T.);
#15467=FACE_OUTER_BOUND('',#18221,.T.);
#15468=FACE_OUTER_BOUND('',#18222,.T.);
#15469=FACE_OUTER_BOUND('',#18223,.T.);
#15470=FACE_OUTER_BOUND('',#18224,.T.);
#15471=FACE_OUTER_BOUND('',#18225,.T.);
#15472=FACE_OUTER_BOUND('',#18226,.T.);
#15473=FACE_OUTER_BOUND('',#18227,.T.);
#15474=FACE_OUTER_BOUND('',#18228,.T.);
#15475=FACE_OUTER_BOUND('',#18229,.T.);
#15476=FACE_OUTER_BOUND('',#18230,.T.);
#15477=FACE_OUTER_BOUND('',#18231,.T.);
#15478=FACE_OUTER_BOUND('',#18232,.T.);
#15479=FACE_OUTER_BOUND('',#18233,.T.);
#15480=FACE_OUTER_BOUND('',#18234,.T.);
#15481=FACE_OUTER_BOUND('',#18235,.T.);
#15482=FACE_OUTER_BOUND('',#18236,.T.);
#15483=FACE_OUTER_BOUND('',#18237,.T.);
#15484=FACE_OUTER_BOUND('',#18238,.T.);
#15485=FACE_OUTER_BOUND('',#18239,.T.);
#15486=FACE_OUTER_BOUND('',#18240,.T.);
#15487=FACE_OUTER_BOUND('',#18241,.T.);
#15488=FACE_OUTER_BOUND('',#18242,.T.);
#15489=FACE_OUTER_BOUND('',#18243,.T.);
#15490=FACE_OUTER_BOUND('',#18244,.T.);
#15491=FACE_OUTER_BOUND('',#18245,.T.);
#15492=FACE_OUTER_BOUND('',#18246,.T.);
#15493=FACE_OUTER_BOUND('',#18247,.T.);
#15494=FACE_OUTER_BOUND('',#18248,.T.);
#15495=FACE_OUTER_BOUND('',#18249,.T.);
#15496=FACE_OUTER_BOUND('',#18250,.T.);
#15497=FACE_OUTER_BOUND('',#18251,.T.);
#15498=FACE_OUTER_BOUND('',#18252,.T.);
#15499=FACE_OUTER_BOUND('',#18253,.T.);
#15500=FACE_OUTER_BOUND('',#18254,.T.);
#15501=FACE_OUTER_BOUND('',#18255,.T.);
#15502=FACE_OUTER_BOUND('',#18256,.T.);
#15503=FACE_OUTER_BOUND('',#18257,.T.);
#15504=FACE_OUTER_BOUND('',#18258,.T.);
#15505=FACE_OUTER_BOUND('',#18259,.T.);
#15506=FACE_OUTER_BOUND('',#18260,.T.);
#15507=FACE_OUTER_BOUND('',#18261,.T.);
#15508=FACE_OUTER_BOUND('',#18262,.T.);
#15509=FACE_OUTER_BOUND('',#18263,.T.);
#15510=FACE_OUTER_BOUND('',#18264,.T.);
#15511=FACE_OUTER_BOUND('',#18265,.T.);
#15512=FACE_OUTER_BOUND('',#18266,.T.);
#15513=FACE_OUTER_BOUND('',#18267,.T.);
#15514=FACE_OUTER_BOUND('',#18268,.T.);
#15515=FACE_OUTER_BOUND('',#18269,.T.);
#15516=FACE_OUTER_BOUND('',#18270,.T.);
#15517=FACE_OUTER_BOUND('',#18271,.T.);
#15518=FACE_OUTER_BOUND('',#18272,.T.);
#15519=FACE_OUTER_BOUND('',#18273,.T.);
#15520=FACE_OUTER_BOUND('',#18274,.T.);
#15521=FACE_OUTER_BOUND('',#18275,.T.);
#15522=FACE_OUTER_BOUND('',#18276,.T.);
#15523=FACE_OUTER_BOUND('',#18277,.T.);
#15524=FACE_OUTER_BOUND('',#18278,.T.);
#15525=FACE_OUTER_BOUND('',#18279,.T.);
#15526=FACE_OUTER_BOUND('',#18280,.T.);
#15527=FACE_OUTER_BOUND('',#18281,.T.);
#15528=FACE_OUTER_BOUND('',#18282,.T.);
#15529=FACE_OUTER_BOUND('',#18283,.T.);
#15530=FACE_OUTER_BOUND('',#18284,.T.);
#15531=FACE_OUTER_BOUND('',#18285,.T.);
#15532=FACE_OUTER_BOUND('',#18286,.T.);
#15533=FACE_OUTER_BOUND('',#18287,.T.);
#15534=FACE_OUTER_BOUND('',#18288,.T.);
#15535=FACE_OUTER_BOUND('',#18289,.T.);
#15536=FACE_OUTER_BOUND('',#18290,.T.);
#15537=FACE_OUTER_BOUND('',#18291,.T.);
#15538=FACE_OUTER_BOUND('',#18292,.T.);
#15539=FACE_OUTER_BOUND('',#18293,.T.);
#15540=FACE_OUTER_BOUND('',#18294,.T.);
#15541=FACE_OUTER_BOUND('',#18295,.T.);
#15542=FACE_OUTER_BOUND('',#18296,.T.);
#15543=FACE_OUTER_BOUND('',#18297,.T.);
#15544=FACE_OUTER_BOUND('',#18298,.T.);
#15545=FACE_OUTER_BOUND('',#18299,.T.);
#15546=FACE_OUTER_BOUND('',#18300,.T.);
#15547=FACE_OUTER_BOUND('',#18301,.T.);
#15548=FACE_OUTER_BOUND('',#18302,.T.);
#15549=FACE_OUTER_BOUND('',#18303,.T.);
#15550=FACE_OUTER_BOUND('',#18304,.T.);
#15551=FACE_OUTER_BOUND('',#18305,.T.);
#15552=FACE_OUTER_BOUND('',#18306,.T.);
#15553=FACE_OUTER_BOUND('',#18307,.T.);
#15554=FACE_OUTER_BOUND('',#18308,.T.);
#15555=FACE_OUTER_BOUND('',#18309,.T.);
#15556=FACE_OUTER_BOUND('',#18310,.T.);
#15557=FACE_OUTER_BOUND('',#18311,.T.);
#15558=FACE_OUTER_BOUND('',#18312,.T.);
#15559=FACE_OUTER_BOUND('',#18313,.T.);
#15560=FACE_OUTER_BOUND('',#18314,.T.);
#15561=FACE_OUTER_BOUND('',#18315,.T.);
#15562=FACE_OUTER_BOUND('',#18316,.T.);
#15563=FACE_OUTER_BOUND('',#18317,.T.);
#15564=FACE_OUTER_BOUND('',#18318,.T.);
#15565=FACE_OUTER_BOUND('',#18319,.T.);
#15566=FACE_OUTER_BOUND('',#18320,.T.);
#15567=FACE_OUTER_BOUND('',#18321,.T.);
#15568=FACE_OUTER_BOUND('',#18322,.T.);
#15569=FACE_OUTER_BOUND('',#18323,.T.);
#15570=FACE_OUTER_BOUND('',#18324,.T.);
#15571=FACE_OUTER_BOUND('',#18325,.T.);
#15572=FACE_OUTER_BOUND('',#18326,.T.);
#15573=FACE_OUTER_BOUND('',#18327,.T.);
#15574=FACE_OUTER_BOUND('',#18328,.T.);
#15575=FACE_OUTER_BOUND('',#18329,.T.);
#15576=FACE_OUTER_BOUND('',#18330,.T.);
#15577=FACE_OUTER_BOUND('',#18331,.T.);
#15578=FACE_OUTER_BOUND('',#18332,.T.);
#15579=FACE_OUTER_BOUND('',#18333,.T.);
#15580=FACE_OUTER_BOUND('',#18334,.T.);
#15581=FACE_OUTER_BOUND('',#18335,.T.);
#15582=FACE_OUTER_BOUND('',#18336,.T.);
#15583=FACE_OUTER_BOUND('',#18337,.T.);
#15584=FACE_OUTER_BOUND('',#18338,.T.);
#15585=FACE_OUTER_BOUND('',#18339,.T.);
#15586=FACE_OUTER_BOUND('',#18340,.T.);
#15587=FACE_OUTER_BOUND('',#18341,.T.);
#15588=FACE_OUTER_BOUND('',#18342,.T.);
#15589=FACE_OUTER_BOUND('',#18343,.T.);
#15590=FACE_OUTER_BOUND('',#18344,.T.);
#15591=FACE_OUTER_BOUND('',#18345,.T.);
#15592=FACE_OUTER_BOUND('',#18346,.T.);
#15593=FACE_OUTER_BOUND('',#18347,.T.);
#15594=FACE_OUTER_BOUND('',#18348,.T.);
#15595=FACE_OUTER_BOUND('',#18349,.T.);
#15596=FACE_OUTER_BOUND('',#18350,.T.);
#15597=FACE_OUTER_BOUND('',#18351,.T.);
#15598=FACE_OUTER_BOUND('',#18352,.T.);
#15599=FACE_OUTER_BOUND('',#18353,.T.);
#15600=FACE_OUTER_BOUND('',#18354,.T.);
#15601=FACE_OUTER_BOUND('',#18355,.T.);
#15602=FACE_OUTER_BOUND('',#18356,.T.);
#15603=FACE_OUTER_BOUND('',#18357,.T.);
#15604=FACE_OUTER_BOUND('',#18358,.T.);
#15605=FACE_OUTER_BOUND('',#18359,.T.);
#15606=FACE_OUTER_BOUND('',#18361,.T.);
#15607=FACE_OUTER_BOUND('',#18362,.T.);
#15608=FACE_OUTER_BOUND('',#18363,.T.);
#15609=FACE_OUTER_BOUND('',#18364,.T.);
#15610=FACE_OUTER_BOUND('',#18365,.T.);
#15611=FACE_OUTER_BOUND('',#18367,.T.);
#15612=FACE_OUTER_BOUND('',#18368,.T.);
#15613=FACE_OUTER_BOUND('',#18369,.T.);
#15614=FACE_OUTER_BOUND('',#18370,.T.);
#15615=FACE_OUTER_BOUND('',#18372,.T.);
#15616=FACE_OUTER_BOUND('',#18373,.T.);
#15617=FACE_OUTER_BOUND('',#18374,.T.);
#15618=FACE_OUTER_BOUND('',#18375,.T.);
#15619=FACE_OUTER_BOUND('',#18377,.T.);
#15620=FACE_OUTER_BOUND('',#18378,.T.);
#15621=FACE_OUTER_BOUND('',#18379,.T.);
#15622=FACE_OUTER_BOUND('',#18380,.T.);
#15623=FACE_OUTER_BOUND('',#18381,.T.);
#15624=FACE_OUTER_BOUND('',#18382,.T.);
#15625=FACE_OUTER_BOUND('',#18383,.T.);
#15626=FACE_OUTER_BOUND('',#18384,.T.);
#15627=FACE_OUTER_BOUND('',#18385,.T.);
#15628=FACE_OUTER_BOUND('',#18386,.T.);
#15629=FACE_OUTER_BOUND('',#18387,.T.);
#15630=FACE_OUTER_BOUND('',#18388,.T.);
#15631=FACE_OUTER_BOUND('',#18389,.T.);
#15632=FACE_OUTER_BOUND('',#18390,.T.);
#15633=FACE_OUTER_BOUND('',#18391,.T.);
#15634=FACE_OUTER_BOUND('',#18392,.T.);
#15635=FACE_OUTER_BOUND('',#18393,.T.);
#15636=FACE_OUTER_BOUND('',#18394,.T.);
#15637=FACE_OUTER_BOUND('',#18395,.T.);
#15638=FACE_OUTER_BOUND('',#18396,.T.);
#15639=FACE_OUTER_BOUND('',#18397,.T.);
#15640=FACE_OUTER_BOUND('',#18398,.T.);
#15641=FACE_OUTER_BOUND('',#18399,.T.);
#15642=FACE_OUTER_BOUND('',#18400,.T.);
#15643=FACE_OUTER_BOUND('',#18401,.T.);
#15644=FACE_OUTER_BOUND('',#18402,.T.);
#15645=FACE_OUTER_BOUND('',#18403,.T.);
#15646=FACE_OUTER_BOUND('',#18404,.T.);
#15647=FACE_OUTER_BOUND('',#18405,.T.);
#15648=FACE_OUTER_BOUND('',#18406,.T.);
#15649=FACE_OUTER_BOUND('',#18407,.T.);
#15650=FACE_OUTER_BOUND('',#18408,.T.);
#15651=FACE_OUTER_BOUND('',#18409,.T.);
#15652=FACE_OUTER_BOUND('',#18410,.T.);
#15653=FACE_OUTER_BOUND('',#18411,.T.);
#15654=FACE_OUTER_BOUND('',#18412,.T.);
#15655=FACE_OUTER_BOUND('',#18413,.T.);
#15656=FACE_OUTER_BOUND('',#18414,.T.);
#15657=FACE_OUTER_BOUND('',#18415,.T.);
#15658=FACE_OUTER_BOUND('',#18416,.T.);
#15659=FACE_OUTER_BOUND('',#18417,.T.);
#15660=FACE_OUTER_BOUND('',#18418,.T.);
#15661=FACE_OUTER_BOUND('',#18419,.T.);
#15662=FACE_OUTER_BOUND('',#18420,.T.);
#15663=FACE_OUTER_BOUND('',#18421,.T.);
#15664=FACE_OUTER_BOUND('',#18422,.T.);
#15665=FACE_OUTER_BOUND('',#18423,.T.);
#15666=FACE_OUTER_BOUND('',#18424,.T.);
#15667=FACE_OUTER_BOUND('',#18425,.T.);
#15668=FACE_OUTER_BOUND('',#18426,.T.);
#15669=FACE_OUTER_BOUND('',#18427,.T.);
#15670=FACE_OUTER_BOUND('',#18429,.T.);
#15671=FACE_OUTER_BOUND('',#18430,.T.);
#15672=FACE_OUTER_BOUND('',#18431,.T.);
#15673=FACE_OUTER_BOUND('',#18432,.T.);
#15674=FACE_OUTER_BOUND('',#18433,.T.);
#15675=FACE_OUTER_BOUND('',#18434,.T.);
#15676=FACE_OUTER_BOUND('',#18435,.T.);
#15677=FACE_OUTER_BOUND('',#18436,.T.);
#15678=FACE_OUTER_BOUND('',#18437,.T.);
#15679=FACE_OUTER_BOUND('',#18438,.T.);
#15680=FACE_OUTER_BOUND('',#18439,.T.);
#15681=FACE_OUTER_BOUND('',#18440,.T.);
#15682=FACE_OUTER_BOUND('',#18441,.T.);
#15683=FACE_OUTER_BOUND('',#18442,.T.);
#15684=FACE_OUTER_BOUND('',#18443,.T.);
#15685=FACE_OUTER_BOUND('',#18444,.T.);
#15686=FACE_OUTER_BOUND('',#18445,.T.);
#15687=FACE_OUTER_BOUND('',#18446,.T.);
#15688=FACE_OUTER_BOUND('',#18447,.T.);
#15689=FACE_OUTER_BOUND('',#18448,.T.);
#15690=FACE_OUTER_BOUND('',#18449,.T.);
#15691=FACE_OUTER_BOUND('',#18450,.T.);
#15692=FACE_OUTER_BOUND('',#18451,.T.);
#15693=FACE_OUTER_BOUND('',#18452,.T.);
#15694=FACE_OUTER_BOUND('',#18453,.T.);
#15695=FACE_OUTER_BOUND('',#18454,.T.);
#15696=FACE_OUTER_BOUND('',#18455,.T.);
#15697=FACE_OUTER_BOUND('',#18456,.T.);
#15698=FACE_OUTER_BOUND('',#18457,.T.);
#15699=FACE_OUTER_BOUND('',#18458,.T.);
#15700=FACE_OUTER_BOUND('',#18459,.T.);
#15701=FACE_OUTER_BOUND('',#18460,.T.);
#15702=FACE_OUTER_BOUND('',#18461,.T.);
#15703=FACE_OUTER_BOUND('',#18462,.T.);
#15704=FACE_OUTER_BOUND('',#18463,.T.);
#15705=FACE_OUTER_BOUND('',#18464,.T.);
#15706=FACE_OUTER_BOUND('',#18465,.T.);
#15707=FACE_OUTER_BOUND('',#18466,.T.);
#15708=FACE_OUTER_BOUND('',#18467,.T.);
#15709=FACE_OUTER_BOUND('',#18468,.T.);
#15710=FACE_OUTER_BOUND('',#18469,.T.);
#15711=FACE_OUTER_BOUND('',#18470,.T.);
#15712=FACE_OUTER_BOUND('',#18471,.T.);
#15713=FACE_OUTER_BOUND('',#18472,.T.);
#15714=FACE_OUTER_BOUND('',#18473,.T.);
#15715=FACE_OUTER_BOUND('',#18474,.T.);
#15716=FACE_OUTER_BOUND('',#18475,.T.);
#15717=FACE_OUTER_BOUND('',#18476,.T.);
#15718=FACE_OUTER_BOUND('',#18477,.T.);
#15719=FACE_OUTER_BOUND('',#18478,.T.);
#15720=FACE_OUTER_BOUND('',#18479,.T.);
#15721=FACE_OUTER_BOUND('',#18480,.T.);
#15722=FACE_OUTER_BOUND('',#18481,.T.);
#15723=FACE_OUTER_BOUND('',#18482,.T.);
#15724=FACE_OUTER_BOUND('',#18483,.T.);
#15725=FACE_OUTER_BOUND('',#18484,.T.);
#15726=FACE_OUTER_BOUND('',#18485,.T.);
#15727=FACE_OUTER_BOUND('',#18486,.T.);
#15728=FACE_OUTER_BOUND('',#18487,.T.);
#15729=FACE_OUTER_BOUND('',#18488,.T.);
#15730=FACE_OUTER_BOUND('',#18489,.T.);
#15731=FACE_OUTER_BOUND('',#18490,.T.);
#15732=FACE_OUTER_BOUND('',#18491,.T.);
#15733=FACE_OUTER_BOUND('',#18492,.T.);
#15734=FACE_OUTER_BOUND('',#18493,.T.);
#15735=FACE_OUTER_BOUND('',#18494,.T.);
#15736=FACE_OUTER_BOUND('',#18495,.T.);
#15737=FACE_OUTER_BOUND('',#18496,.T.);
#15738=FACE_OUTER_BOUND('',#18497,.T.);
#15739=FACE_OUTER_BOUND('',#18498,.T.);
#15740=FACE_OUTER_BOUND('',#18499,.T.);
#15741=FACE_OUTER_BOUND('',#18500,.T.);
#15742=FACE_OUTER_BOUND('',#18501,.T.);
#15743=FACE_OUTER_BOUND('',#18502,.T.);
#15744=FACE_OUTER_BOUND('',#18503,.T.);
#15745=FACE_OUTER_BOUND('',#18504,.T.);
#15746=FACE_OUTER_BOUND('',#18505,.T.);
#15747=FACE_OUTER_BOUND('',#18506,.T.);
#15748=FACE_OUTER_BOUND('',#18507,.T.);
#15749=FACE_OUTER_BOUND('',#18508,.T.);
#15750=FACE_OUTER_BOUND('',#18509,.T.);
#15751=FACE_OUTER_BOUND('',#18510,.T.);
#15752=FACE_OUTER_BOUND('',#18511,.T.);
#15753=FACE_OUTER_BOUND('',#18512,.T.);
#15754=FACE_OUTER_BOUND('',#18513,.T.);
#15755=FACE_OUTER_BOUND('',#18514,.T.);
#15756=FACE_OUTER_BOUND('',#18515,.T.);
#15757=FACE_OUTER_BOUND('',#18516,.T.);
#15758=FACE_OUTER_BOUND('',#18517,.T.);
#15759=FACE_OUTER_BOUND('',#18518,.T.);
#15760=FACE_OUTER_BOUND('',#18519,.T.);
#15761=FACE_OUTER_BOUND('',#18520,.T.);
#15762=FACE_OUTER_BOUND('',#18521,.T.);
#15763=FACE_OUTER_BOUND('',#18522,.T.);
#15764=FACE_OUTER_BOUND('',#18523,.T.);
#15765=FACE_OUTER_BOUND('',#18524,.T.);
#15766=FACE_OUTER_BOUND('',#18525,.T.);
#15767=FACE_OUTER_BOUND('',#18526,.T.);
#15768=FACE_OUTER_BOUND('',#18527,.T.);
#15769=FACE_OUTER_BOUND('',#18528,.T.);
#15770=FACE_OUTER_BOUND('',#18529,.T.);
#15771=FACE_OUTER_BOUND('',#18530,.T.);
#15772=FACE_OUTER_BOUND('',#18531,.T.);
#15773=FACE_OUTER_BOUND('',#18532,.T.);
#15774=FACE_OUTER_BOUND('',#18533,.T.);
#15775=FACE_OUTER_BOUND('',#18534,.T.);
#15776=FACE_OUTER_BOUND('',#18535,.T.);
#15777=FACE_OUTER_BOUND('',#18536,.T.);
#15778=FACE_OUTER_BOUND('',#18537,.T.);
#15779=FACE_OUTER_BOUND('',#18538,.T.);
#15780=FACE_OUTER_BOUND('',#18539,.T.);
#15781=FACE_OUTER_BOUND('',#18540,.T.);
#15782=FACE_OUTER_BOUND('',#18541,.T.);
#15783=FACE_OUTER_BOUND('',#18542,.T.);
#15784=FACE_OUTER_BOUND('',#18543,.T.);
#15785=FACE_OUTER_BOUND('',#18544,.T.);
#15786=FACE_OUTER_BOUND('',#18545,.T.);
#15787=FACE_OUTER_BOUND('',#18546,.T.);
#15788=FACE_OUTER_BOUND('',#18547,.T.);
#15789=FACE_OUTER_BOUND('',#18548,.T.);
#15790=FACE_OUTER_BOUND('',#18549,.T.);
#15791=FACE_OUTER_BOUND('',#18550,.T.);
#15792=FACE_OUTER_BOUND('',#18551,.T.);
#15793=FACE_OUTER_BOUND('',#18552,.T.);
#15794=FACE_OUTER_BOUND('',#18553,.T.);
#15795=FACE_OUTER_BOUND('',#18554,.T.);
#15796=FACE_OUTER_BOUND('',#18555,.T.);
#15797=FACE_OUTER_BOUND('',#18556,.T.);
#15798=FACE_OUTER_BOUND('',#18557,.T.);
#15799=FACE_OUTER_BOUND('',#18558,.T.);
#15800=FACE_OUTER_BOUND('',#18559,.T.);
#15801=FACE_OUTER_BOUND('',#18560,.T.);
#15802=FACE_OUTER_BOUND('',#18561,.T.);
#15803=FACE_OUTER_BOUND('',#18562,.T.);
#15804=FACE_OUTER_BOUND('',#18563,.T.);
#15805=FACE_OUTER_BOUND('',#18564,.T.);
#15806=FACE_OUTER_BOUND('',#18565,.T.);
#15807=FACE_OUTER_BOUND('',#18566,.T.);
#15808=FACE_OUTER_BOUND('',#18567,.T.);
#15809=FACE_OUTER_BOUND('',#18568,.T.);
#15810=FACE_OUTER_BOUND('',#18569,.T.);
#15811=FACE_OUTER_BOUND('',#18570,.T.);
#15812=FACE_OUTER_BOUND('',#18571,.T.);
#15813=FACE_OUTER_BOUND('',#18572,.T.);
#15814=FACE_OUTER_BOUND('',#18573,.T.);
#15815=FACE_OUTER_BOUND('',#18574,.T.);
#15816=FACE_OUTER_BOUND('',#18575,.T.);
#15817=FACE_OUTER_BOUND('',#18576,.T.);
#15818=FACE_OUTER_BOUND('',#18577,.T.);
#15819=FACE_OUTER_BOUND('',#18578,.T.);
#15820=FACE_OUTER_BOUND('',#18579,.T.);
#15821=FACE_OUTER_BOUND('',#18580,.T.);
#15822=FACE_OUTER_BOUND('',#18582,.T.);
#15823=FACE_OUTER_BOUND('',#18583,.T.);
#15824=FACE_OUTER_BOUND('',#18584,.T.);
#15825=FACE_OUTER_BOUND('',#18585,.T.);
#15826=FACE_OUTER_BOUND('',#18586,.T.);
#15827=FACE_OUTER_BOUND('',#18588,.T.);
#15828=FACE_OUTER_BOUND('',#18589,.T.);
#15829=FACE_OUTER_BOUND('',#18590,.T.);
#15830=FACE_OUTER_BOUND('',#18591,.T.);
#15831=FACE_OUTER_BOUND('',#18592,.T.);
#15832=FACE_OUTER_BOUND('',#18593,.T.);
#15833=FACE_OUTER_BOUND('',#18594,.T.);
#15834=FACE_OUTER_BOUND('',#18595,.T.);
#15835=FACE_OUTER_BOUND('',#18596,.T.);
#15836=FACE_OUTER_BOUND('',#18597,.T.);
#15837=FACE_OUTER_BOUND('',#18598,.T.);
#15838=FACE_OUTER_BOUND('',#18599,.T.);
#15839=FACE_OUTER_BOUND('',#18600,.T.);
#15840=FACE_OUTER_BOUND('',#18601,.T.);
#15841=FACE_OUTER_BOUND('',#18602,.T.);
#15842=FACE_OUTER_BOUND('',#18603,.T.);
#15843=FACE_OUTER_BOUND('',#18604,.T.);
#15844=FACE_OUTER_BOUND('',#18605,.T.);
#15845=FACE_OUTER_BOUND('',#18606,.T.);
#15846=FACE_OUTER_BOUND('',#18607,.T.);
#15847=FACE_OUTER_BOUND('',#18608,.T.);
#15848=FACE_OUTER_BOUND('',#18609,.T.);
#15849=FACE_OUTER_BOUND('',#18610,.T.);
#15850=FACE_OUTER_BOUND('',#18611,.T.);
#15851=FACE_OUTER_BOUND('',#18612,.T.);
#15852=FACE_OUTER_BOUND('',#18613,.T.);
#15853=FACE_OUTER_BOUND('',#18614,.T.);
#15854=FACE_OUTER_BOUND('',#18615,.T.);
#15855=FACE_OUTER_BOUND('',#18616,.T.);
#15856=FACE_OUTER_BOUND('',#18617,.T.);
#15857=FACE_OUTER_BOUND('',#18618,.T.);
#15858=FACE_OUTER_BOUND('',#18619,.T.);
#15859=FACE_OUTER_BOUND('',#18620,.T.);
#15860=FACE_OUTER_BOUND('',#18621,.T.);
#15861=FACE_OUTER_BOUND('',#18622,.T.);
#15862=FACE_OUTER_BOUND('',#18623,.T.);
#15863=FACE_OUTER_BOUND('',#18624,.T.);
#15864=FACE_OUTER_BOUND('',#18625,.T.);
#15865=FACE_OUTER_BOUND('',#18626,.T.);
#15866=FACE_OUTER_BOUND('',#18627,.T.);
#15867=FACE_OUTER_BOUND('',#18628,.T.);
#15868=FACE_OUTER_BOUND('',#18629,.T.);
#15869=FACE_OUTER_BOUND('',#18630,.T.);
#15870=FACE_OUTER_BOUND('',#18631,.T.);
#15871=FACE_OUTER_BOUND('',#18632,.T.);
#15872=FACE_OUTER_BOUND('',#18633,.T.);
#15873=FACE_OUTER_BOUND('',#18634,.T.);
#15874=FACE_OUTER_BOUND('',#18635,.T.);
#15875=FACE_OUTER_BOUND('',#18636,.T.);
#15876=FACE_OUTER_BOUND('',#18637,.T.);
#15877=FACE_OUTER_BOUND('',#18638,.T.);
#15878=FACE_OUTER_BOUND('',#18639,.T.);
#15879=FACE_OUTER_BOUND('',#18640,.T.);
#15880=FACE_OUTER_BOUND('',#18641,.T.);
#15881=FACE_OUTER_BOUND('',#18642,.T.);
#15882=FACE_OUTER_BOUND('',#18643,.T.);
#15883=FACE_OUTER_BOUND('',#18644,.T.);
#15884=FACE_OUTER_BOUND('',#18645,.T.);
#15885=FACE_OUTER_BOUND('',#18646,.T.);
#15886=FACE_OUTER_BOUND('',#18647,.T.);
#15887=FACE_OUTER_BOUND('',#18649,.T.);
#15888=FACE_OUTER_BOUND('',#18650,.T.);
#15889=FACE_OUTER_BOUND('',#18651,.T.);
#15890=FACE_OUTER_BOUND('',#18652,.T.);
#15891=FACE_OUTER_BOUND('',#18653,.T.);
#15892=FACE_OUTER_BOUND('',#18654,.T.);
#15893=FACE_OUTER_BOUND('',#18655,.T.);
#15894=FACE_OUTER_BOUND('',#18656,.T.);
#15895=FACE_OUTER_BOUND('',#18657,.T.);
#15896=FACE_OUTER_BOUND('',#18658,.T.);
#15897=FACE_OUTER_BOUND('',#18659,.T.);
#15898=FACE_OUTER_BOUND('',#18660,.T.);
#15899=FACE_OUTER_BOUND('',#18662,.T.);
#15900=FACE_OUTER_BOUND('',#18663,.T.);
#15901=FACE_OUTER_BOUND('',#18664,.T.);
#15902=FACE_OUTER_BOUND('',#18665,.T.);
#15903=FACE_OUTER_BOUND('',#18667,.T.);
#15904=FACE_OUTER_BOUND('',#18668,.T.);
#15905=FACE_OUTER_BOUND('',#18669,.T.);
#15906=FACE_OUTER_BOUND('',#18670,.T.);
#15907=FACE_OUTER_BOUND('',#18672,.T.);
#15908=FACE_OUTER_BOUND('',#18673,.T.);
#15909=FACE_OUTER_BOUND('',#18674,.T.);
#15910=FACE_OUTER_BOUND('',#18675,.T.);
#15911=FACE_OUTER_BOUND('',#18676,.T.);
#15912=FACE_OUTER_BOUND('',#18677,.T.);
#15913=FACE_OUTER_BOUND('',#18678,.T.);
#15914=FACE_OUTER_BOUND('',#18679,.T.);
#15915=FACE_OUTER_BOUND('',#18680,.T.);
#15916=FACE_OUTER_BOUND('',#18681,.T.);
#15917=FACE_OUTER_BOUND('',#18682,.T.);
#15918=FACE_OUTER_BOUND('',#18683,.T.);
#15919=FACE_OUTER_BOUND('',#18684,.T.);
#15920=FACE_OUTER_BOUND('',#18685,.T.);
#15921=FACE_OUTER_BOUND('',#18686,.T.);
#15922=FACE_OUTER_BOUND('',#18687,.T.);
#15923=FACE_OUTER_BOUND('',#18688,.T.);
#15924=FACE_OUTER_BOUND('',#18689,.T.);
#15925=FACE_OUTER_BOUND('',#18690,.T.);
#15926=FACE_OUTER_BOUND('',#18691,.T.);
#15927=FACE_OUTER_BOUND('',#18692,.T.);
#15928=FACE_OUTER_BOUND('',#18693,.T.);
#15929=FACE_OUTER_BOUND('',#18694,.T.);
#15930=FACE_OUTER_BOUND('',#18696,.T.);
#15931=EDGE_LOOP('',(#32919,#32920,#32921,#32922));
#15932=EDGE_LOOP('',(#32923,#32924,#32925,#32926));
#15933=EDGE_LOOP('',(#32927,#32928,#32929,#32930));
#15934=EDGE_LOOP('',(#32931,#32932,#32933,#32934));
#15935=EDGE_LOOP('',(#32935,#32936,#32937,#32938));
#15936=EDGE_LOOP('',(#32939,#32940,#32941,#32942));
#15937=EDGE_LOOP('',(#32943,#32944,#32945,#32946));
#15938=EDGE_LOOP('',(#32947,#32948,#32949,#32950));
#15939=EDGE_LOOP('',(#32951,#32952,#32953,#32954));
#15940=EDGE_LOOP('',(#32955,#32956,#32957,#32958));
#15941=EDGE_LOOP('',(#32959,#32960,#32961,#32962));
#15942=EDGE_LOOP('',(#32963,#32964,#32965,#32966));
#15943=EDGE_LOOP('',(#32967,#32968,#32969,#32970));
#15944=EDGE_LOOP('',(#32971,#32972,#32973,#32974));
#15945=EDGE_LOOP('',(#32975,#32976,#32977,#32978));
#15946=EDGE_LOOP('',(#32979,#32980,#32981,#32982));
#15947=EDGE_LOOP('',(#32983,#32984,#32985,#32986));
#15948=EDGE_LOOP('',(#32987,#32988,#32989,#32990));
#15949=EDGE_LOOP('',(#32991,#32992,#32993,#32994));
#15950=EDGE_LOOP('',(#32995,#32996,#32997,#32998));
#15951=EDGE_LOOP('',(#32999,#33000,#33001,#33002));
#15952=EDGE_LOOP('',(#33003,#33004,#33005,#33006));
#15953=EDGE_LOOP('',(#33007,#33008,#33009,#33010));
#15954=EDGE_LOOP('',(#33011,#33012,#33013,#33014));
#15955=EDGE_LOOP('',(#33015,#33016,#33017,#33018));
#15956=EDGE_LOOP('',(#33019,#33020,#33021,#33022));
#15957=EDGE_LOOP('',(#33023,#33024,#33025,#33026));
#15958=EDGE_LOOP('',(#33027,#33028,#33029,#33030));
#15959=EDGE_LOOP('',(#33031,#33032,#33033,#33034));
#15960=EDGE_LOOP('',(#33035,#33036,#33037,#33038));
#15961=EDGE_LOOP('',(#33039,#33040,#33041,#33042));
#15962=EDGE_LOOP('',(#33043,#33044,#33045,#33046));
#15963=EDGE_LOOP('',(#33047,#33048,#33049,#33050));
#15964=EDGE_LOOP('',(#33051,#33052,#33053,#33054));
#15965=EDGE_LOOP('',(#33055,#33056,#33057,#33058));
#15966=EDGE_LOOP('',(#33059,#33060,#33061,#33062));
#15967=EDGE_LOOP('',(#33063,#33064,#33065,#33066,#33067,#33068,#33069,#33070,
#33071,#33072,#33073,#33074,#33075,#33076,#33077,#33078,#33079,#33080,#33081,
#33082,#33083,#33084,#33085,#33086,#33087,#33088,#33089,#33090,#33091,#33092,
#33093,#33094));
#15968=EDGE_LOOP('',(#33095,#33096,#33097,#33098,#33099,#33100,#33101));
#15969=EDGE_LOOP('',(#33102,#33103,#33104,#33105,#33106,#33107,#33108,#33109,
#33110,#33111,#33112,#33113,#33114,#33115,#33116,#33117,#33118,#33119,#33120,
#33121,#33122,#33123,#33124,#33125,#33126,#33127,#33128,#33129,#33130,#33131,
#33132,#33133));
#15970=EDGE_LOOP('',(#33134,#33135,#33136,#33137,#33138,#33139,#33140));
#15971=EDGE_LOOP('',(#33141,#33142,#33143,#33144,#33145,#33146,#33147,#33148,
#33149,#33150,#33151,#33152,#33153,#33154,#33155,#33156,#33157,#33158,#33159,
#33160,#33161,#33162,#33163,#33164,#33165,#33166,#33167,#33168,#33169,#33170,
#33171,#33172));
#15972=EDGE_LOOP('',(#33173,#33174,#33175,#33176,#33177,#33178,#33179));
#15973=EDGE_LOOP('',(#33180,#33181,#33182,#33183,#33184,#33185,#33186,#33187,
#33188,#33189,#33190,#33191,#33192,#33193,#33194,#33195,#33196,#33197,#33198,
#33199,#33200,#33201,#33202,#33203,#33204,#33205,#33206,#33207,#33208,#33209,
#33210,#33211));
#15974=EDGE_LOOP('',(#33212,#33213,#33214,#33215,#33216,#33217,#33218));
#15975=EDGE_LOOP('',(#33219,#33220,#33221,#33222,#33223,#33224,#33225,#33226,
#33227,#33228,#33229,#33230,#33231,#33232,#33233,#33234,#33235,#33236,#33237,
#33238,#33239,#33240,#33241,#33242,#33243,#33244,#33245,#33246,#33247,#33248,
#33249,#33250));
#15976=EDGE_LOOP('',(#33251,#33252,#33253,#33254,#33255,#33256,#33257));
#15977=EDGE_LOOP('',(#33258,#33259,#33260,#33261,#33262,#33263,#33264,#33265,
#33266,#33267,#33268,#33269,#33270,#33271,#33272,#33273,#33274,#33275,#33276,
#33277,#33278,#33279,#33280,#33281,#33282,#33283,#33284,#33285,#33286,#33287,
#33288,#33289));
#15978=EDGE_LOOP('',(#33290,#33291,#33292,#33293,#33294,#33295,#33296));
#15979=EDGE_LOOP('',(#33297,#33298,#33299,#33300,#33301,#33302,#33303,#33304,
#33305,#33306,#33307,#33308,#33309,#33310,#33311,#33312,#33313,#33314,#33315,
#33316,#33317,#33318,#33319,#33320,#33321,#33322,#33323,#33324,#33325,#33326,
#33327,#33328));
#15980=EDGE_LOOP('',(#33329,#33330,#33331,#33332,#33333,#33334,#33335));
#15981=EDGE_LOOP('',(#33336,#33337,#33338,#33339,#33340,#33341,#33342,#33343,
#33344,#33345,#33346,#33347,#33348,#33349,#33350,#33351,#33352,#33353,#33354,
#33355,#33356,#33357,#33358,#33359,#33360,#33361,#33362,#33363,#33364,#33365,
#33366,#33367));
#15982=EDGE_LOOP('',(#33368,#33369,#33370,#33371,#33372,#33373,#33374));
#15983=EDGE_LOOP('',(#33375,#33376,#33377,#33378,#33379,#33380,#33381,#33382,
#33383,#33384,#33385,#33386,#33387,#33388,#33389,#33390,#33391,#33392,#33393,
#33394,#33395,#33396,#33397,#33398,#33399,#33400,#33401,#33402,#33403,#33404,
#33405,#33406));
#15984=EDGE_LOOP('',(#33407,#33408,#33409,#33410,#33411,#33412,#33413));
#15985=EDGE_LOOP('',(#33414,#33415,#33416,#33417,#33418,#33419,#33420,#33421,
#33422,#33423,#33424,#33425,#33426,#33427,#33428,#33429,#33430,#33431,#33432,
#33433,#33434,#33435,#33436,#33437,#33438,#33439,#33440,#33441,#33442,#33443,
#33444,#33445));
#15986=EDGE_LOOP('',(#33446,#33447,#33448,#33449,#33450,#33451,#33452));
#15987=EDGE_LOOP('',(#33453,#33454,#33455,#33456,#33457,#33458,#33459,#33460,
#33461,#33462,#33463,#33464,#33465,#33466,#33467,#33468,#33469,#33470,#33471,
#33472,#33473,#33474,#33475,#33476,#33477,#33478,#33479,#33480,#33481,#33482,
#33483,#33484));
#15988=EDGE_LOOP('',(#33485,#33486,#33487,#33488,#33489,#33490,#33491));
#15989=EDGE_LOOP('',(#33492,#33493,#33494,#33495,#33496,#33497,#33498,#33499,
#33500,#33501,#33502,#33503,#33504,#33505,#33506,#33507,#33508,#33509,#33510,
#33511,#33512,#33513,#33514,#33515,#33516,#33517,#33518,#33519,#33520,#33521,
#33522,#33523));
#15990=EDGE_LOOP('',(#33524,#33525,#33526,#33527,#33528,#33529,#33530));
#15991=EDGE_LOOP('',(#33531,#33532,#33533,#33534,#33535,#33536,#33537,#33538,
#33539,#33540,#33541,#33542,#33543,#33544,#33545,#33546,#33547,#33548,#33549,
#33550,#33551,#33552,#33553,#33554,#33555,#33556,#33557,#33558,#33559,#33560,
#33561,#33562));
#15992=EDGE_LOOP('',(#33563,#33564,#33565,#33566,#33567,#33568,#33569));
#15993=EDGE_LOOP('',(#33570,#33571,#33572,#33573,#33574,#33575,#33576,#33577,
#33578,#33579,#33580,#33581,#33582,#33583,#33584,#33585,#33586,#33587,#33588,
#33589,#33590,#33591,#33592,#33593,#33594,#33595,#33596,#33597,#33598,#33599,
#33600,#33601));
#15994=EDGE_LOOP('',(#33602,#33603,#33604,#33605,#33606,#33607,#33608));
#15995=EDGE_LOOP('',(#33609,#33610,#33611,#33612,#33613,#33614,#33615,#33616,
#33617,#33618,#33619,#33620,#33621,#33622,#33623,#33624,#33625,#33626,#33627,
#33628,#33629,#33630,#33631,#33632,#33633,#33634,#33635,#33636,#33637,#33638,
#33639,#33640));
#15996=EDGE_LOOP('',(#33641,#33642,#33643,#33644,#33645,#33646,#33647));
#15997=EDGE_LOOP('',(#33648,#33649,#33650,#33651,#33652,#33653,#33654,#33655,
#33656,#33657,#33658,#33659,#33660,#33661,#33662,#33663,#33664,#33665,#33666,
#33667,#33668,#33669,#33670,#33671,#33672,#33673,#33674,#33675,#33676,#33677,
#33678,#33679));
#15998=EDGE_LOOP('',(#33680,#33681,#33682,#33683,#33684,#33685,#33686));
#15999=EDGE_LOOP('',(#33687,#33688,#33689,#33690,#33691,#33692,#33693,#33694,
#33695,#33696,#33697,#33698,#33699,#33700,#33701,#33702,#33703,#33704,#33705,
#33706,#33707,#33708,#33709,#33710,#33711,#33712,#33713,#33714,#33715,#33716,
#33717,#33718));
#16000=EDGE_LOOP('',(#33719,#33720,#33721,#33722,#33723,#33724,#33725));
#16001=EDGE_LOOP('',(#33726,#33727,#33728,#33729,#33730,#33731,#33732,#33733,
#33734,#33735,#33736,#33737,#33738,#33739,#33740,#33741,#33742,#33743,#33744,
#33745,#33746,#33747,#33748,#33749,#33750,#33751,#33752,#33753,#33754,#33755,
#33756,#33757));
#16002=EDGE_LOOP('',(#33758,#33759,#33760,#33761,#33762,#33763,#33764));
#16003=EDGE_LOOP('',(#33765,#33766,#33767,#33768,#33769,#33770,#33771,#33772,
#33773,#33774,#33775,#33776,#33777,#33778,#33779,#33780,#33781,#33782,#33783,
#33784,#33785,#33786,#33787,#33788,#33789,#33790,#33791,#33792,#33793,#33794,
#33795,#33796));
#16004=EDGE_LOOP('',(#33797,#33798,#33799,#33800,#33801,#33802,#33803));
#16005=EDGE_LOOP('',(#33804,#33805,#33806,#33807,#33808,#33809,#33810,#33811,
#33812,#33813,#33814,#33815,#33816,#33817,#33818,#33819,#33820,#33821,#33822,
#33823,#33824,#33825,#33826,#33827,#33828,#33829,#33830,#33831,#33832,#33833,
#33834,#33835));
#16006=EDGE_LOOP('',(#33836,#33837,#33838,#33839,#33840,#33841,#33842));
#16007=EDGE_LOOP('',(#33843,#33844,#33845,#33846,#33847,#33848,#33849,#33850,
#33851,#33852,#33853,#33854,#33855,#33856,#33857,#33858,#33859,#33860,#33861,
#33862,#33863,#33864,#33865,#33866,#33867,#33868,#33869,#33870,#33871,#33872,
#33873,#33874));
#16008=EDGE_LOOP('',(#33875,#33876,#33877,#33878,#33879,#33880,#33881));
#16009=EDGE_LOOP('',(#33882,#33883,#33884,#33885,#33886,#33887,#33888,#33889,
#33890,#33891,#33892,#33893,#33894,#33895,#33896,#33897,#33898,#33899,#33900,
#33901,#33902,#33903,#33904,#33905,#33906,#33907,#33908,#33909,#33910,#33911,
#33912,#33913));
#16010=EDGE_LOOP('',(#33914,#33915,#33916,#33917,#33918,#33919,#33920));
#16011=EDGE_LOOP('',(#33921,#33922,#33923,#33924,#33925,#33926,#33927,#33928,
#33929,#33930,#33931,#33932,#33933,#33934,#33935,#33936,#33937,#33938,#33939,
#33940,#33941,#33942,#33943,#33944,#33945,#33946,#33947,#33948,#33949,#33950,
#33951,#33952));
#16012=EDGE_LOOP('',(#33953,#33954,#33955,#33956,#33957,#33958,#33959));
#16013=EDGE_LOOP('',(#33960,#33961,#33962,#33963,#33964,#33965,#33966,#33967,
#33968,#33969,#33970,#33971,#33972,#33973,#33974,#33975,#33976,#33977,#33978,
#33979,#33980,#33981,#33982,#33983,#33984,#33985,#33986,#33987,#33988,#33989,
#33990,#33991));
#16014=EDGE_LOOP('',(#33992,#33993,#33994,#33995,#33996,#33997,#33998));
#16015=EDGE_LOOP('',(#33999,#34000,#34001,#34002,#34003,#34004,#34005,#34006,
#34007,#34008,#34009,#34010,#34011,#34012,#34013,#34014,#34015,#34016,#34017,
#34018,#34019,#34020,#34021,#34022,#34023,#34024,#34025,#34026,#34027,#34028,
#34029,#34030));
#16016=EDGE_LOOP('',(#34031,#34032,#34033,#34034,#34035,#34036,#34037));
#16017=EDGE_LOOP('',(#34038,#34039,#34040,#34041,#34042,#34043,#34044,#34045,
#34046,#34047,#34048,#34049,#34050,#34051,#34052,#34053,#34054,#34055,#34056,
#34057,#34058,#34059,#34060,#34061,#34062,#34063,#34064,#34065,#34066,#34067,
#34068,#34069));
#16018=EDGE_LOOP('',(#34070,#34071,#34072,#34073,#34074,#34075,#34076));
#16019=EDGE_LOOP('',(#34077,#34078,#34079,#34080,#34081,#34082,#34083,#34084,
#34085,#34086,#34087,#34088,#34089,#34090,#34091,#34092,#34093,#34094,#34095,
#34096,#34097,#34098,#34099,#34100,#34101,#34102,#34103,#34104,#34105,#34106,
#34107,#34108));
#16020=EDGE_LOOP('',(#34109,#34110,#34111,#34112,#34113,#34114,#34115));
#16021=EDGE_LOOP('',(#34116,#34117,#34118,#34119,#34120,#34121,#34122,#34123,
#34124,#34125,#34126,#34127,#34128,#34129,#34130,#34131,#34132,#34133,#34134,
#34135,#34136,#34137,#34138,#34139,#34140,#34141,#34142,#34143,#34144,#34145,
#34146,#34147));
#16022=EDGE_LOOP('',(#34148,#34149,#34150,#34151,#34152,#34153,#34154));
#16023=EDGE_LOOP('',(#34155,#34156,#34157,#34158,#34159,#34160,#34161,#34162,
#34163,#34164,#34165,#34166,#34167,#34168,#34169,#34170,#34171,#34172,#34173,
#34174,#34175,#34176,#34177,#34178,#34179,#34180,#34181,#34182,#34183,#34184,
#34185,#34186));
#16024=EDGE_LOOP('',(#34187,#34188,#34189,#34190,#34191,#34192,#34193));
#16025=EDGE_LOOP('',(#34194,#34195,#34196,#34197,#34198,#34199,#34200,#34201,
#34202,#34203,#34204,#34205,#34206,#34207,#34208,#34209,#34210,#34211,#34212,
#34213,#34214,#34215,#34216,#34217,#34218,#34219,#34220,#34221,#34222,#34223,
#34224,#34225));
#16026=EDGE_LOOP('',(#34226,#34227,#34228,#34229,#34230,#34231,#34232));
#16027=EDGE_LOOP('',(#34233,#34234,#34235,#34236,#34237,#34238,#34239,#34240,
#34241,#34242,#34243,#34244,#34245,#34246,#34247,#34248,#34249,#34250,#34251,
#34252,#34253,#34254,#34255,#34256,#34257,#34258,#34259,#34260,#34261,#34262,
#34263,#34264));
#16028=EDGE_LOOP('',(#34265,#34266,#34267,#34268,#34269,#34270,#34271));
#16029=EDGE_LOOP('',(#34272,#34273,#34274,#34275,#34276,#34277,#34278,#34279,
#34280,#34281,#34282,#34283,#34284,#34285,#34286,#34287,#34288,#34289,#34290,
#34291,#34292,#34293,#34294,#34295,#34296,#34297,#34298,#34299,#34300,#34301,
#34302,#34303));
#16030=EDGE_LOOP('',(#34304,#34305,#34306,#34307,#34308,#34309,#34310));
#16031=EDGE_LOOP('',(#34311,#34312,#34313,#34314,#34315,#34316,#34317,#34318,
#34319,#34320,#34321,#34322,#34323,#34324,#34325,#34326,#34327,#34328,#34329,
#34330,#34331,#34332,#34333,#34334,#34335,#34336,#34337,#34338,#34339,#34340,
#34341,#34342));
#16032=EDGE_LOOP('',(#34343,#34344,#34345,#34346,#34347,#34348,#34349));
#16033=EDGE_LOOP('',(#34350,#34351,#34352,#34353,#34354,#34355,#34356,#34357,
#34358,#34359,#34360,#34361,#34362,#34363,#34364,#34365,#34366,#34367,#34368,
#34369,#34370,#34371,#34372,#34373,#34374,#34375,#34376,#34377,#34378,#34379,
#34380,#34381));
#16034=EDGE_LOOP('',(#34382,#34383,#34384,#34385,#34386,#34387,#34388));
#16035=EDGE_LOOP('',(#34389,#34390,#34391,#34392,#34393,#34394,#34395,#34396,
#34397,#34398,#34399,#34400,#34401,#34402,#34403,#34404,#34405,#34406,#34407,
#34408,#34409,#34410,#34411,#34412,#34413,#34414,#34415,#34416,#34417,#34418,
#34419,#34420));
#16036=EDGE_LOOP('',(#34421,#34422,#34423,#34424,#34425,#34426,#34427));
#16037=EDGE_LOOP('',(#34428,#34429,#34430,#34431,#34432,#34433,#34434,#34435,
#34436,#34437,#34438,#34439,#34440,#34441,#34442,#34443,#34444,#34445,#34446,
#34447,#34448,#34449,#34450,#34451,#34452,#34453,#34454,#34455,#34456,#34457,
#34458,#34459));
#16038=EDGE_LOOP('',(#34460,#34461,#34462,#34463,#34464,#34465,#34466));
#16039=EDGE_LOOP('',(#34467,#34468,#34469,#34470));
#16040=EDGE_LOOP('',(#34471,#34472,#34473,#34474));
#16041=EDGE_LOOP('',(#34475,#34476,#34477,#34478));
#16042=EDGE_LOOP('',(#34479,#34480,#34481,#34482));
#16043=EDGE_LOOP('',(#34483,#34484,#34485,#34486));
#16044=EDGE_LOOP('',(#34487,#34488,#34489,#34490));
#16045=EDGE_LOOP('',(#34491,#34492,#34493,#34494));
#16046=EDGE_LOOP('',(#34495,#34496,#34497,#34498));
#16047=EDGE_LOOP('',(#34499,#34500,#34501,#34502));
#16048=EDGE_LOOP('',(#34503,#34504,#34505,#34506));
#16049=EDGE_LOOP('',(#34507,#34508,#34509,#34510));
#16050=EDGE_LOOP('',(#34511,#34512,#34513,#34514));
#16051=EDGE_LOOP('',(#34515,#34516,#34517,#34518));
#16052=EDGE_LOOP('',(#34519,#34520,#34521,#34522));
#16053=EDGE_LOOP('',(#34523,#34524,#34525,#34526));
#16054=EDGE_LOOP('',(#34527,#34528,#34529,#34530));
#16055=EDGE_LOOP('',(#34531,#34532,#34533,#34534));
#16056=EDGE_LOOP('',(#34535,#34536,#34537,#34538));
#16057=EDGE_LOOP('',(#34539,#34540,#34541,#34542));
#16058=EDGE_LOOP('',(#34543,#34544,#34545,#34546));
#16059=EDGE_LOOP('',(#34547,#34548,#34549,#34550));
#16060=EDGE_LOOP('',(#34551,#34552,#34553,#34554));
#16061=EDGE_LOOP('',(#34555,#34556,#34557,#34558));
#16062=EDGE_LOOP('',(#34559,#34560,#34561,#34562));
#16063=EDGE_LOOP('',(#34563,#34564,#34565,#34566));
#16064=EDGE_LOOP('',(#34567,#34568,#34569,#34570));
#16065=EDGE_LOOP('',(#34571,#34572,#34573,#34574));
#16066=EDGE_LOOP('',(#34575,#34576,#34577,#34578));
#16067=EDGE_LOOP('',(#34579,#34580,#34581,#34582));
#16068=EDGE_LOOP('',(#34583,#34584,#34585,#34586));
#16069=EDGE_LOOP('',(#34587,#34588,#34589,#34590));
#16070=EDGE_LOOP('',(#34591,#34592,#34593,#34594));
#16071=EDGE_LOOP('',(#34595,#34596,#34597,#34598));
#16072=EDGE_LOOP('',(#34599,#34600,#34601,#34602));
#16073=EDGE_LOOP('',(#34603,#34604,#34605,#34606));
#16074=EDGE_LOOP('',(#34607,#34608,#34609,#34610));
#16075=EDGE_LOOP('',(#34611,#34612,#34613,#34614,#34615,#34616,#34617));
#16076=EDGE_LOOP('',(#34618,#34619,#34620,#34621,#34622,#34623,#34624));
#16077=EDGE_LOOP('',(#34625,#34626,#34627,#34628,#34629,#34630,#34631));
#16078=EDGE_LOOP('',(#34632,#34633,#34634,#34635,#34636,#34637,#34638));
#16079=EDGE_LOOP('',(#34639,#34640,#34641,#34642,#34643,#34644,#34645));
#16080=EDGE_LOOP('',(#34646,#34647,#34648,#34649,#34650,#34651,#34652));
#16081=EDGE_LOOP('',(#34653,#34654,#34655,#34656,#34657,#34658,#34659));
#16082=EDGE_LOOP('',(#34660,#34661,#34662,#34663,#34664,#34665,#34666));
#16083=EDGE_LOOP('',(#34667,#34668,#34669,#34670,#34671,#34672,#34673));
#16084=EDGE_LOOP('',(#34674,#34675,#34676,#34677,#34678,#34679,#34680));
#16085=EDGE_LOOP('',(#34681,#34682,#34683,#34684,#34685,#34686,#34687));
#16086=EDGE_LOOP('',(#34688,#34689,#34690,#34691,#34692,#34693,#34694));
#16087=EDGE_LOOP('',(#34695,#34696,#34697,#34698,#34699,#34700,#34701));
#16088=EDGE_LOOP('',(#34702,#34703,#34704,#34705,#34706,#34707,#34708));
#16089=EDGE_LOOP('',(#34709,#34710,#34711,#34712,#34713,#34714,#34715));
#16090=EDGE_LOOP('',(#34716,#34717,#34718,#34719,#34720,#34721,#34722));
#16091=EDGE_LOOP('',(#34723,#34724,#34725,#34726,#34727,#34728,#34729));
#16092=EDGE_LOOP('',(#34730,#34731,#34732,#34733,#34734,#34735,#34736));
#16093=EDGE_LOOP('',(#34737,#34738,#34739,#34740,#34741,#34742,#34743));
#16094=EDGE_LOOP('',(#34744,#34745,#34746,#34747,#34748,#34749,#34750));
#16095=EDGE_LOOP('',(#34751,#34752,#34753,#34754,#34755,#34756,#34757));
#16096=EDGE_LOOP('',(#34758,#34759,#34760,#34761,#34762,#34763,#34764));
#16097=EDGE_LOOP('',(#34765,#34766,#34767,#34768,#34769,#34770,#34771));
#16098=EDGE_LOOP('',(#34772,#34773,#34774,#34775,#34776,#34777,#34778));
#16099=EDGE_LOOP('',(#34779,#34780,#34781,#34782,#34783,#34784,#34785));
#16100=EDGE_LOOP('',(#34786,#34787,#34788,#34789,#34790,#34791,#34792));
#16101=EDGE_LOOP('',(#34793,#34794,#34795,#34796,#34797,#34798,#34799));
#16102=EDGE_LOOP('',(#34800,#34801,#34802,#34803,#34804,#34805,#34806));
#16103=EDGE_LOOP('',(#34807,#34808,#34809,#34810,#34811,#34812,#34813));
#16104=EDGE_LOOP('',(#34814,#34815,#34816,#34817,#34818,#34819,#34820));
#16105=EDGE_LOOP('',(#34821,#34822,#34823,#34824,#34825,#34826,#34827));
#16106=EDGE_LOOP('',(#34828,#34829,#34830,#34831,#34832,#34833,#34834));
#16107=EDGE_LOOP('',(#34835,#34836,#34837,#34838,#34839,#34840,#34841));
#16108=EDGE_LOOP('',(#34842,#34843,#34844,#34845,#34846,#34847,#34848));
#16109=EDGE_LOOP('',(#34849,#34850,#34851,#34852,#34853,#34854,#34855));
#16110=EDGE_LOOP('',(#34856,#34857,#34858,#34859,#34860,#34861,#34862));
#16111=EDGE_LOOP('',(#34863,#34864,#34865,#34866));
#16112=EDGE_LOOP('',(#34867,#34868,#34869,#34870));
#16113=EDGE_LOOP('',(#34871,#34872,#34873,#34874));
#16114=EDGE_LOOP('',(#34875,#34876,#34877,#34878));
#16115=EDGE_LOOP('',(#34879,#34880,#34881,#34882));
#16116=EDGE_LOOP('',(#34883,#34884,#34885,#34886));
#16117=EDGE_LOOP('',(#34887,#34888,#34889,#34890));
#16118=EDGE_LOOP('',(#34891,#34892,#34893,#34894));
#16119=EDGE_LOOP('',(#34895,#34896,#34897,#34898));
#16120=EDGE_LOOP('',(#34899,#34900,#34901,#34902));
#16121=EDGE_LOOP('',(#34903,#34904,#34905,#34906));
#16122=EDGE_LOOP('',(#34907,#34908,#34909,#34910));
#16123=EDGE_LOOP('',(#34911,#34912,#34913,#34914));
#16124=EDGE_LOOP('',(#34915,#34916,#34917,#34918));
#16125=EDGE_LOOP('',(#34919,#34920,#34921,#34922));
#16126=EDGE_LOOP('',(#34923,#34924,#34925,#34926));
#16127=EDGE_LOOP('',(#34927,#34928,#34929,#34930));
#16128=EDGE_LOOP('',(#34931,#34932,#34933,#34934));
#16129=EDGE_LOOP('',(#34935,#34936,#34937,#34938));
#16130=EDGE_LOOP('',(#34939,#34940,#34941,#34942));
#16131=EDGE_LOOP('',(#34943,#34944,#34945,#34946));
#16132=EDGE_LOOP('',(#34947,#34948,#34949,#34950));
#16133=EDGE_LOOP('',(#34951,#34952,#34953,#34954));
#16134=EDGE_LOOP('',(#34955,#34956,#34957,#34958));
#16135=EDGE_LOOP('',(#34959,#34960,#34961,#34962));
#16136=EDGE_LOOP('',(#34963,#34964,#34965,#34966));
#16137=EDGE_LOOP('',(#34967,#34968,#34969,#34970));
#16138=EDGE_LOOP('',(#34971,#34972,#34973,#34974));
#16139=EDGE_LOOP('',(#34975,#34976,#34977,#34978));
#16140=EDGE_LOOP('',(#34979,#34980,#34981,#34982));
#16141=EDGE_LOOP('',(#34983,#34984,#34985,#34986));
#16142=EDGE_LOOP('',(#34987,#34988,#34989,#34990));
#16143=EDGE_LOOP('',(#34991,#34992,#34993,#34994));
#16144=EDGE_LOOP('',(#34995,#34996,#34997,#34998));
#16145=EDGE_LOOP('',(#34999,#35000,#35001,#35002));
#16146=EDGE_LOOP('',(#35003,#35004,#35005,#35006));
#16147=EDGE_LOOP('',(#35007,#35008,#35009,#35010,#35011,#35012,#35013));
#16148=EDGE_LOOP('',(#35014,#35015,#35016,#35017,#35018,#35019,#35020));
#16149=EDGE_LOOP('',(#35021,#35022,#35023,#35024,#35025,#35026,#35027));
#16150=EDGE_LOOP('',(#35028,#35029,#35030,#35031,#35032,#35033,#35034));
#16151=EDGE_LOOP('',(#35035,#35036,#35037,#35038,#35039,#35040,#35041));
#16152=EDGE_LOOP('',(#35042,#35043,#35044,#35045,#35046,#35047,#35048));
#16153=EDGE_LOOP('',(#35049,#35050,#35051,#35052,#35053,#35054,#35055));
#16154=EDGE_LOOP('',(#35056,#35057,#35058,#35059,#35060,#35061,#35062));
#16155=EDGE_LOOP('',(#35063,#35064,#35065,#35066,#35067,#35068,#35069));
#16156=EDGE_LOOP('',(#35070,#35071,#35072,#35073,#35074,#35075,#35076));
#16157=EDGE_LOOP('',(#35077,#35078,#35079,#35080,#35081,#35082,#35083));
#16158=EDGE_LOOP('',(#35084,#35085,#35086,#35087,#35088,#35089,#35090));
#16159=EDGE_LOOP('',(#35091,#35092,#35093,#35094,#35095,#35096,#35097));
#16160=EDGE_LOOP('',(#35098,#35099,#35100,#35101,#35102,#35103,#35104));
#16161=EDGE_LOOP('',(#35105,#35106,#35107,#35108,#35109,#35110,#35111));
#16162=EDGE_LOOP('',(#35112,#35113,#35114,#35115,#35116,#35117,#35118));
#16163=EDGE_LOOP('',(#35119,#35120,#35121,#35122,#35123,#35124,#35125));
#16164=EDGE_LOOP('',(#35126,#35127,#35128,#35129,#35130,#35131,#35132));
#16165=EDGE_LOOP('',(#35133,#35134,#35135,#35136,#35137,#35138,#35139));
#16166=EDGE_LOOP('',(#35140,#35141,#35142,#35143,#35144,#35145,#35146));
#16167=EDGE_LOOP('',(#35147,#35148,#35149,#35150,#35151,#35152,#35153));
#16168=EDGE_LOOP('',(#35154,#35155,#35156,#35157,#35158,#35159,#35160));
#16169=EDGE_LOOP('',(#35161,#35162,#35163,#35164,#35165,#35166,#35167));
#16170=EDGE_LOOP('',(#35168,#35169,#35170,#35171,#35172,#35173,#35174));
#16171=EDGE_LOOP('',(#35175,#35176,#35177,#35178,#35179,#35180,#35181));
#16172=EDGE_LOOP('',(#35182,#35183,#35184,#35185,#35186,#35187,#35188));
#16173=EDGE_LOOP('',(#35189,#35190,#35191,#35192,#35193,#35194,#35195));
#16174=EDGE_LOOP('',(#35196,#35197,#35198,#35199,#35200,#35201,#35202));
#16175=EDGE_LOOP('',(#35203,#35204,#35205,#35206,#35207,#35208,#35209));
#16176=EDGE_LOOP('',(#35210,#35211,#35212,#35213,#35214,#35215,#35216));
#16177=EDGE_LOOP('',(#35217,#35218,#35219,#35220,#35221,#35222,#35223));
#16178=EDGE_LOOP('',(#35224,#35225,#35226,#35227,#35228,#35229,#35230));
#16179=EDGE_LOOP('',(#35231,#35232,#35233,#35234,#35235,#35236,#35237));
#16180=EDGE_LOOP('',(#35238,#35239,#35240,#35241,#35242,#35243,#35244));
#16181=EDGE_LOOP('',(#35245,#35246,#35247,#35248,#35249,#35250,#35251));
#16182=EDGE_LOOP('',(#35252,#35253,#35254,#35255));
#16183=EDGE_LOOP('',(#35256,#35257,#35258,#35259));
#16184=EDGE_LOOP('',(#35260,#35261,#35262,#35263));
#16185=EDGE_LOOP('',(#35264,#35265,#35266,#35267));
#16186=EDGE_LOOP('',(#35268,#35269,#35270,#35271));
#16187=EDGE_LOOP('',(#35272,#35273,#35274,#35275));
#16188=EDGE_LOOP('',(#35276,#35277,#35278,#35279));
#16189=EDGE_LOOP('',(#35280,#35281,#35282,#35283));
#16190=EDGE_LOOP('',(#35284,#35285,#35286,#35287));
#16191=EDGE_LOOP('',(#35288,#35289,#35290,#35291));
#16192=EDGE_LOOP('',(#35292,#35293,#35294,#35295));
#16193=EDGE_LOOP('',(#35296,#35297,#35298,#35299));
#16194=EDGE_LOOP('',(#35300,#35301,#35302,#35303));
#16195=EDGE_LOOP('',(#35304,#35305,#35306,#35307));
#16196=EDGE_LOOP('',(#35308,#35309,#35310,#35311));
#16197=EDGE_LOOP('',(#35312,#35313,#35314,#35315));
#16198=EDGE_LOOP('',(#35316,#35317,#35318,#35319));
#16199=EDGE_LOOP('',(#35320,#35321,#35322,#35323));
#16200=EDGE_LOOP('',(#35324,#35325,#35326,#35327));
#16201=EDGE_LOOP('',(#35328,#35329,#35330,#35331));
#16202=EDGE_LOOP('',(#35332,#35333,#35334,#35335));
#16203=EDGE_LOOP('',(#35336,#35337,#35338,#35339));
#16204=EDGE_LOOP('',(#35340,#35341,#35342,#35343));
#16205=EDGE_LOOP('',(#35344,#35345,#35346,#35347));
#16206=EDGE_LOOP('',(#35348,#35349,#35350,#35351));
#16207=EDGE_LOOP('',(#35352,#35353,#35354,#35355));
#16208=EDGE_LOOP('',(#35356,#35357,#35358,#35359));
#16209=EDGE_LOOP('',(#35360,#35361,#35362,#35363));
#16210=EDGE_LOOP('',(#35364,#35365,#35366,#35367));
#16211=EDGE_LOOP('',(#35368,#35369,#35370,#35371));
#16212=EDGE_LOOP('',(#35372,#35373,#35374,#35375));
#16213=EDGE_LOOP('',(#35376,#35377,#35378,#35379));
#16214=EDGE_LOOP('',(#35380,#35381,#35382,#35383));
#16215=EDGE_LOOP('',(#35384,#35385,#35386,#35387));
#16216=EDGE_LOOP('',(#35388,#35389,#35390,#35391));
#16217=EDGE_LOOP('',(#35392,#35393,#35394,#35395));
#16218=EDGE_LOOP('',(#35396,#35397,#35398,#35399));
#16219=EDGE_LOOP('',(#35400,#35401,#35402,#35403));
#16220=EDGE_LOOP('',(#35404,#35405,#35406,#35407));
#16221=EDGE_LOOP('',(#35408,#35409,#35410,#35411));
#16222=EDGE_LOOP('',(#35412,#35413,#35414,#35415));
#16223=EDGE_LOOP('',(#35416,#35417,#35418,#35419));
#16224=EDGE_LOOP('',(#35420,#35421,#35422,#35423));
#16225=EDGE_LOOP('',(#35424,#35425,#35426,#35427));
#16226=EDGE_LOOP('',(#35428,#35429,#35430,#35431));
#16227=EDGE_LOOP('',(#35432,#35433,#35434,#35435));
#16228=EDGE_LOOP('',(#35436,#35437,#35438,#35439));
#16229=EDGE_LOOP('',(#35440,#35441,#35442,#35443));
#16230=EDGE_LOOP('',(#35444,#35445,#35446,#35447));
#16231=EDGE_LOOP('',(#35448,#35449,#35450,#35451));
#16232=EDGE_LOOP('',(#35452,#35453,#35454,#35455));
#16233=EDGE_LOOP('',(#35456,#35457,#35458,#35459));
#16234=EDGE_LOOP('',(#35460,#35461,#35462,#35463));
#16235=EDGE_LOOP('',(#35464,#35465,#35466,#35467));
#16236=EDGE_LOOP('',(#35468,#35469,#35470,#35471,#35472));
#16237=EDGE_LOOP('',(#35473,#35474,#35475,#35476));
#16238=EDGE_LOOP('',(#35477,#35478,#35479,#35480));
#16239=EDGE_LOOP('',(#35481,#35482,#35483,#35484));
#16240=EDGE_LOOP('',(#35485,#35486,#35487,#35488));
#16241=EDGE_LOOP('',(#35489,#35490,#35491,#35492));
#16242=EDGE_LOOP('',(#35493,#35494,#35495,#35496));
#16243=EDGE_LOOP('',(#35497,#35498,#35499,#35500));
#16244=EDGE_LOOP('',(#35501,#35502,#35503,#35504));
#16245=EDGE_LOOP('',(#35505,#35506,#35507,#35508));
#16246=EDGE_LOOP('',(#35509,#35510,#35511,#35512));
#16247=EDGE_LOOP('',(#35513,#35514,#35515,#35516));
#16248=EDGE_LOOP('',(#35517,#35518,#35519,#35520));
#16249=EDGE_LOOP('',(#35521,#35522,#35523,#35524));
#16250=EDGE_LOOP('',(#35525,#35526,#35527,#35528));
#16251=EDGE_LOOP('',(#35529,#35530,#35531,#35532));
#16252=EDGE_LOOP('',(#35533,#35534,#35535,#35536));
#16253=EDGE_LOOP('',(#35537,#35538,#35539,#35540));
#16254=EDGE_LOOP('',(#35541,#35542,#35543,#35544));
#16255=EDGE_LOOP('',(#35545,#35546,#35547,#35548));
#16256=EDGE_LOOP('',(#35549,#35550,#35551,#35552));
#16257=EDGE_LOOP('',(#35553,#35554,#35555,#35556));
#16258=EDGE_LOOP('',(#35557,#35558,#35559,#35560));
#16259=EDGE_LOOP('',(#35561,#35562,#35563,#35564));
#16260=EDGE_LOOP('',(#35565,#35566,#35567,#35568));
#16261=EDGE_LOOP('',(#35569,#35570,#35571,#35572));
#16262=EDGE_LOOP('',(#35573,#35574,#35575,#35576));
#16263=EDGE_LOOP('',(#35577,#35578,#35579,#35580));
#16264=EDGE_LOOP('',(#35581,#35582,#35583,#35584));
#16265=EDGE_LOOP('',(#35585,#35586,#35587,#35588));
#16266=EDGE_LOOP('',(#35589,#35590,#35591,#35592));
#16267=EDGE_LOOP('',(#35593,#35594,#35595,#35596));
#16268=EDGE_LOOP('',(#35597,#35598,#35599,#35600,#35601,#35602,#35603));
#16269=EDGE_LOOP('',(#35604,#35605,#35606,#35607));
#16270=EDGE_LOOP('',(#35608,#35609,#35610,#35611));
#16271=EDGE_LOOP('',(#35612,#35613,#35614,#35615));
#16272=EDGE_LOOP('',(#35616,#35617,#35618,#35619));
#16273=EDGE_LOOP('',(#35620,#35621,#35622,#35623));
#16274=EDGE_LOOP('',(#35624,#35625,#35626,#35627));
#16275=EDGE_LOOP('',(#35628,#35629,#35630,#35631));
#16276=EDGE_LOOP('',(#35632,#35633,#35634,#35635));
#16277=EDGE_LOOP('',(#35636,#35637,#35638,#35639));
#16278=EDGE_LOOP('',(#35640,#35641,#35642,#35643));
#16279=EDGE_LOOP('',(#35644,#35645,#35646,#35647));
#16280=EDGE_LOOP('',(#35648,#35649,#35650,#35651));
#16281=EDGE_LOOP('',(#35652,#35653,#35654,#35655));
#16282=EDGE_LOOP('',(#35656,#35657,#35658,#35659));
#16283=EDGE_LOOP('',(#35660,#35661,#35662,#35663,#35664,#35665,#35666,#35667,
#35668,#35669,#35670,#35671,#35672,#35673,#35674,#35675,#35676,#35677,#35678,
#35679,#35680,#35681,#35682,#35683,#35684,#35685,#35686,#35687,#35688,#35689,
#35690,#35691,#35692,#35693,#35694,#35695,#35696,#35697,#35698,#35699,#35700,
#35701,#35702,#35703,#35704,#35705,#35706,#35707,#35708,#35709,#35710,#35711,
#35712,#35713,#35714,#35715,#35716,#35717,#35718,#35719,#35720,#35721,#35722,
#35723,#35724,#35725,#35726,#35727,#35728,#35729,#35730,#35731,#35732,#35733,
#35734,#35735,#35736,#35737,#35738,#35739,#35740,#35741,#35742,#35743,#35744,
#35745,#35746,#35747,#35748,#35749,#35750,#35751,#35752,#35753,#35754,#35755,
#35756,#35757,#35758,#35759,#35760,#35761,#35762,#35763,#35764,#35765,#35766,
#35767,#35768,#35769,#35770,#35771,#35772,#35773,#35774,#35775,#35776,#35777,
#35778,#35779,#35780,#35781,#35782,#35783,#35784,#35785,#35786,#35787,#35788,
#35789,#35790,#35791,#35792,#35793,#35794,#35795,#35796,#35797,#35798,#35799,
#35800,#35801,#35802,#35803,#35804,#35805,#35806,#35807));
#16284=EDGE_LOOP('',(#35808,#35809,#35810,#35811,#35812,#35813,#35814,#35815,
#35816,#35817,#35818,#35819,#35820,#35821,#35822,#35823,#35824,#35825,#35826,
#35827,#35828,#35829,#35830,#35831,#35832,#35833,#35834,#35835,#35836,#35837,
#35838,#35839));
#16285=EDGE_LOOP('',(#35840,#35841,#35842,#35843));
#16286=EDGE_LOOP('',(#35844,#35845,#35846,#35847));
#16287=EDGE_LOOP('',(#35848,#35849,#35850,#35851));
#16288=EDGE_LOOP('',(#35852,#35853,#35854,#35855));
#16289=EDGE_LOOP('',(#35856,#35857,#35858,#35859));
#16290=EDGE_LOOP('',(#35860,#35861,#35862,#35863));
#16291=EDGE_LOOP('',(#35864,#35865,#35866,#35867));
#16292=EDGE_LOOP('',(#35868,#35869,#35870,#35871));
#16293=EDGE_LOOP('',(#35872,#35873,#35874,#35875));
#16294=EDGE_LOOP('',(#35876,#35877,#35878,#35879));
#16295=EDGE_LOOP('',(#35880,#35881,#35882,#35883));
#16296=EDGE_LOOP('',(#35884,#35885,#35886,#35887));
#16297=EDGE_LOOP('',(#35888,#35889,#35890,#35891));
#16298=EDGE_LOOP('',(#35892,#35893,#35894,#35895,#35896,#35897,#35898));
#16299=EDGE_LOOP('',(#35899,#35900,#35901,#35902));
#16300=EDGE_LOOP('',(#35903,#35904,#35905,#35906));
#16301=EDGE_LOOP('',(#35907,#35908,#35909,#35910));
#16302=EDGE_LOOP('',(#35911,#35912,#35913,#35914));
#16303=EDGE_LOOP('',(#35915,#35916,#35917,#35918));
#16304=EDGE_LOOP('',(#35919,#35920,#35921,#35922));
#16305=EDGE_LOOP('',(#35923,#35924,#35925,#35926));
#16306=EDGE_LOOP('',(#35927,#35928,#35929,#35930));
#16307=EDGE_LOOP('',(#35931,#35932,#35933,#35934));
#16308=EDGE_LOOP('',(#35935,#35936,#35937,#35938));
#16309=EDGE_LOOP('',(#35939,#35940,#35941,#35942));
#16310=EDGE_LOOP('',(#35943,#35944,#35945,#35946));
#16311=EDGE_LOOP('',(#35947,#35948,#35949,#35950));
#16312=EDGE_LOOP('',(#35951,#35952,#35953,#35954));
#16313=EDGE_LOOP('',(#35955,#35956,#35957,#35958,#35959,#35960,#35961,#35962,
#35963,#35964,#35965,#35966,#35967,#35968,#35969,#35970,#35971,#35972,#35973,
#35974,#35975,#35976,#35977,#35978,#35979,#35980,#35981,#35982,#35983,#35984,
#35985,#35986));
#16314=EDGE_LOOP('',(#35987,#35988,#35989,#35990));
#16315=EDGE_LOOP('',(#35991,#35992,#35993,#35994));
#16316=EDGE_LOOP('',(#35995,#35996,#35997,#35998));
#16317=EDGE_LOOP('',(#35999,#36000,#36001,#36002));
#16318=EDGE_LOOP('',(#36003,#36004,#36005,#36006));
#16319=EDGE_LOOP('',(#36007,#36008,#36009,#36010));
#16320=EDGE_LOOP('',(#36011,#36012,#36013,#36014));
#16321=EDGE_LOOP('',(#36015,#36016,#36017,#36018));
#16322=EDGE_LOOP('',(#36019,#36020,#36021,#36022));
#16323=EDGE_LOOP('',(#36023,#36024,#36025,#36026));
#16324=EDGE_LOOP('',(#36027,#36028,#36029,#36030));
#16325=EDGE_LOOP('',(#36031,#36032,#36033,#36034));
#16326=EDGE_LOOP('',(#36035,#36036,#36037,#36038));
#16327=EDGE_LOOP('',(#36039,#36040,#36041,#36042,#36043,#36044,#36045));
#16328=EDGE_LOOP('',(#36046,#36047,#36048,#36049));
#16329=EDGE_LOOP('',(#36050,#36051,#36052,#36053));
#16330=EDGE_LOOP('',(#36054,#36055,#36056,#36057));
#16331=EDGE_LOOP('',(#36058,#36059,#36060,#36061));
#16332=EDGE_LOOP('',(#36062,#36063,#36064,#36065));
#16333=EDGE_LOOP('',(#36066,#36067,#36068,#36069));
#16334=EDGE_LOOP('',(#36070,#36071,#36072,#36073));
#16335=EDGE_LOOP('',(#36074,#36075,#36076,#36077));
#16336=EDGE_LOOP('',(#36078,#36079,#36080,#36081));
#16337=EDGE_LOOP('',(#36082,#36083,#36084,#36085));
#16338=EDGE_LOOP('',(#36086,#36087,#36088,#36089));
#16339=EDGE_LOOP('',(#36090,#36091,#36092,#36093));
#16340=EDGE_LOOP('',(#36094,#36095,#36096,#36097));
#16341=EDGE_LOOP('',(#36098,#36099,#36100,#36101));
#16342=EDGE_LOOP('',(#36102,#36103,#36104,#36105,#36106,#36107,#36108,#36109,
#36110,#36111,#36112,#36113,#36114,#36115,#36116,#36117,#36118,#36119,#36120,
#36121,#36122,#36123,#36124,#36125,#36126,#36127,#36128,#36129,#36130,#36131,
#36132,#36133));
#16343=EDGE_LOOP('',(#36134,#36135,#36136,#36137));
#16344=EDGE_LOOP('',(#36138,#36139,#36140,#36141));
#16345=EDGE_LOOP('',(#36142,#36143,#36144,#36145));
#16346=EDGE_LOOP('',(#36146,#36147,#36148,#36149));
#16347=EDGE_LOOP('',(#36150,#36151,#36152,#36153));
#16348=EDGE_LOOP('',(#36154,#36155,#36156,#36157));
#16349=EDGE_LOOP('',(#36158,#36159,#36160,#36161));
#16350=EDGE_LOOP('',(#36162,#36163,#36164,#36165));
#16351=EDGE_LOOP('',(#36166,#36167,#36168,#36169));
#16352=EDGE_LOOP('',(#36170,#36171,#36172,#36173));
#16353=EDGE_LOOP('',(#36174,#36175,#36176,#36177));
#16354=EDGE_LOOP('',(#36178,#36179,#36180,#36181));
#16355=EDGE_LOOP('',(#36182,#36183,#36184,#36185));
#16356=EDGE_LOOP('',(#36186,#36187,#36188,#36189,#36190,#36191,#36192));
#16357=EDGE_LOOP('',(#36193,#36194,#36195,#36196));
#16358=EDGE_LOOP('',(#36197,#36198,#36199,#36200));
#16359=EDGE_LOOP('',(#36201,#36202,#36203,#36204));
#16360=EDGE_LOOP('',(#36205,#36206,#36207,#36208));
#16361=EDGE_LOOP('',(#36209,#36210,#36211,#36212));
#16362=EDGE_LOOP('',(#36213,#36214,#36215,#36216));
#16363=EDGE_LOOP('',(#36217,#36218,#36219,#36220));
#16364=EDGE_LOOP('',(#36221,#36222,#36223,#36224));
#16365=EDGE_LOOP('',(#36225,#36226,#36227,#36228));
#16366=EDGE_LOOP('',(#36229,#36230,#36231,#36232));
#16367=EDGE_LOOP('',(#36233,#36234,#36235,#36236));
#16368=EDGE_LOOP('',(#36237,#36238,#36239,#36240));
#16369=EDGE_LOOP('',(#36241,#36242,#36243,#36244));
#16370=EDGE_LOOP('',(#36245,#36246,#36247,#36248));
#16371=EDGE_LOOP('',(#36249,#36250,#36251,#36252,#36253,#36254,#36255,#36256,
#36257,#36258,#36259,#36260,#36261,#36262,#36263,#36264,#36265,#36266,#36267,
#36268,#36269,#36270,#36271,#36272,#36273,#36274,#36275,#36276,#36277,#36278,
#36279,#36280));
#16372=EDGE_LOOP('',(#36281,#36282,#36283,#36284));
#16373=EDGE_LOOP('',(#36285,#36286,#36287,#36288));
#16374=EDGE_LOOP('',(#36289,#36290,#36291,#36292));
#16375=EDGE_LOOP('',(#36293,#36294,#36295,#36296));
#16376=EDGE_LOOP('',(#36297,#36298,#36299,#36300));
#16377=EDGE_LOOP('',(#36301,#36302,#36303,#36304));
#16378=EDGE_LOOP('',(#36305,#36306,#36307,#36308));
#16379=EDGE_LOOP('',(#36309,#36310,#36311,#36312));
#16380=EDGE_LOOP('',(#36313,#36314,#36315,#36316));
#16381=EDGE_LOOP('',(#36317,#36318,#36319,#36320));
#16382=EDGE_LOOP('',(#36321,#36322,#36323,#36324));
#16383=EDGE_LOOP('',(#36325,#36326,#36327,#36328));
#16384=EDGE_LOOP('',(#36329,#36330,#36331,#36332));
#16385=EDGE_LOOP('',(#36333,#36334,#36335,#36336,#36337,#36338,#36339));
#16386=EDGE_LOOP('',(#36340,#36341,#36342,#36343));
#16387=EDGE_LOOP('',(#36344,#36345,#36346,#36347));
#16388=EDGE_LOOP('',(#36348,#36349,#36350,#36351));
#16389=EDGE_LOOP('',(#36352,#36353,#36354,#36355));
#16390=EDGE_LOOP('',(#36356,#36357,#36358,#36359));
#16391=EDGE_LOOP('',(#36360,#36361,#36362,#36363));
#16392=EDGE_LOOP('',(#36364,#36365,#36366,#36367));
#16393=EDGE_LOOP('',(#36368,#36369,#36370,#36371));
#16394=EDGE_LOOP('',(#36372,#36373,#36374,#36375));
#16395=EDGE_LOOP('',(#36376,#36377,#36378,#36379));
#16396=EDGE_LOOP('',(#36380,#36381,#36382,#36383));
#16397=EDGE_LOOP('',(#36384,#36385,#36386,#36387));
#16398=EDGE_LOOP('',(#36388,#36389,#36390,#36391));
#16399=EDGE_LOOP('',(#36392,#36393,#36394,#36395));
#16400=EDGE_LOOP('',(#36396,#36397,#36398,#36399,#36400,#36401,#36402,#36403,
#36404,#36405,#36406,#36407,#36408,#36409,#36410,#36411,#36412,#36413,#36414,
#36415,#36416,#36417,#36418,#36419,#36420,#36421,#36422,#36423,#36424,#36425,
#36426,#36427));
#16401=EDGE_LOOP('',(#36428,#36429,#36430,#36431));
#16402=EDGE_LOOP('',(#36432,#36433,#36434,#36435));
#16403=EDGE_LOOP('',(#36436,#36437,#36438,#36439));
#16404=EDGE_LOOP('',(#36440,#36441,#36442,#36443));
#16405=EDGE_LOOP('',(#36444,#36445,#36446,#36447));
#16406=EDGE_LOOP('',(#36448,#36449,#36450,#36451));
#16407=EDGE_LOOP('',(#36452,#36453,#36454,#36455));
#16408=EDGE_LOOP('',(#36456,#36457,#36458,#36459));
#16409=EDGE_LOOP('',(#36460,#36461,#36462,#36463));
#16410=EDGE_LOOP('',(#36464,#36465,#36466,#36467));
#16411=EDGE_LOOP('',(#36468,#36469,#36470,#36471));
#16412=EDGE_LOOP('',(#36472,#36473,#36474,#36475));
#16413=EDGE_LOOP('',(#36476,#36477,#36478,#36479));
#16414=EDGE_LOOP('',(#36480,#36481,#36482,#36483,#36484,#36485,#36486));
#16415=EDGE_LOOP('',(#36487,#36488,#36489,#36490));
#16416=EDGE_LOOP('',(#36491,#36492,#36493,#36494));
#16417=EDGE_LOOP('',(#36495,#36496,#36497,#36498));
#16418=EDGE_LOOP('',(#36499,#36500,#36501,#36502));
#16419=EDGE_LOOP('',(#36503,#36504,#36505,#36506));
#16420=EDGE_LOOP('',(#36507,#36508,#36509,#36510));
#16421=EDGE_LOOP('',(#36511,#36512,#36513,#36514));
#16422=EDGE_LOOP('',(#36515,#36516,#36517,#36518));
#16423=EDGE_LOOP('',(#36519,#36520,#36521,#36522));
#16424=EDGE_LOOP('',(#36523,#36524,#36525,#36526));
#16425=EDGE_LOOP('',(#36527,#36528,#36529,#36530));
#16426=EDGE_LOOP('',(#36531,#36532,#36533,#36534));
#16427=EDGE_LOOP('',(#36535,#36536,#36537,#36538));
#16428=EDGE_LOOP('',(#36539,#36540,#36541,#36542));
#16429=EDGE_LOOP('',(#36543,#36544,#36545,#36546,#36547,#36548,#36549,#36550,
#36551,#36552,#36553,#36554,#36555,#36556,#36557,#36558,#36559,#36560,#36561,
#36562,#36563,#36564,#36565,#36566,#36567,#36568,#36569,#36570,#36571,#36572,
#36573,#36574));
#16430=EDGE_LOOP('',(#36575,#36576,#36577,#36578));
#16431=EDGE_LOOP('',(#36579,#36580,#36581,#36582));
#16432=EDGE_LOOP('',(#36583,#36584,#36585,#36586));
#16433=EDGE_LOOP('',(#36587,#36588,#36589,#36590));
#16434=EDGE_LOOP('',(#36591,#36592,#36593,#36594));
#16435=EDGE_LOOP('',(#36595,#36596,#36597,#36598));
#16436=EDGE_LOOP('',(#36599,#36600,#36601,#36602));
#16437=EDGE_LOOP('',(#36603,#36604,#36605,#36606));
#16438=EDGE_LOOP('',(#36607,#36608,#36609,#36610));
#16439=EDGE_LOOP('',(#36611,#36612,#36613,#36614));
#16440=EDGE_LOOP('',(#36615,#36616,#36617,#36618));
#16441=EDGE_LOOP('',(#36619,#36620,#36621,#36622));
#16442=EDGE_LOOP('',(#36623,#36624,#36625,#36626));
#16443=EDGE_LOOP('',(#36627,#36628,#36629,#36630,#36631,#36632,#36633));
#16444=EDGE_LOOP('',(#36634,#36635,#36636,#36637));
#16445=EDGE_LOOP('',(#36638,#36639,#36640,#36641));
#16446=EDGE_LOOP('',(#36642,#36643,#36644,#36645));
#16447=EDGE_LOOP('',(#36646,#36647,#36648,#36649));
#16448=EDGE_LOOP('',(#36650,#36651,#36652,#36653));
#16449=EDGE_LOOP('',(#36654,#36655,#36656,#36657));
#16450=EDGE_LOOP('',(#36658,#36659,#36660,#36661));
#16451=EDGE_LOOP('',(#36662,#36663,#36664,#36665));
#16452=EDGE_LOOP('',(#36666,#36667,#36668,#36669));
#16453=EDGE_LOOP('',(#36670,#36671,#36672,#36673));
#16454=EDGE_LOOP('',(#36674,#36675,#36676,#36677));
#16455=EDGE_LOOP('',(#36678,#36679,#36680,#36681));
#16456=EDGE_LOOP('',(#36682,#36683,#36684,#36685));
#16457=EDGE_LOOP('',(#36686,#36687,#36688,#36689));
#16458=EDGE_LOOP('',(#36690,#36691,#36692,#36693,#36694,#36695,#36696,#36697,
#36698,#36699,#36700,#36701,#36702,#36703,#36704,#36705,#36706,#36707,#36708,
#36709,#36710,#36711,#36712,#36713,#36714,#36715,#36716,#36717,#36718,#36719,
#36720,#36721));
#16459=EDGE_LOOP('',(#36722,#36723,#36724,#36725));
#16460=EDGE_LOOP('',(#36726,#36727,#36728,#36729));
#16461=EDGE_LOOP('',(#36730,#36731,#36732,#36733));
#16462=EDGE_LOOP('',(#36734,#36735,#36736,#36737));
#16463=EDGE_LOOP('',(#36738,#36739,#36740,#36741));
#16464=EDGE_LOOP('',(#36742,#36743,#36744,#36745));
#16465=EDGE_LOOP('',(#36746,#36747,#36748,#36749));
#16466=EDGE_LOOP('',(#36750,#36751,#36752,#36753));
#16467=EDGE_LOOP('',(#36754,#36755,#36756,#36757));
#16468=EDGE_LOOP('',(#36758,#36759,#36760,#36761));
#16469=EDGE_LOOP('',(#36762,#36763,#36764,#36765));
#16470=EDGE_LOOP('',(#36766,#36767,#36768,#36769));
#16471=EDGE_LOOP('',(#36770,#36771,#36772,#36773));
#16472=EDGE_LOOP('',(#36774,#36775,#36776,#36777,#36778,#36779,#36780));
#16473=EDGE_LOOP('',(#36781,#36782,#36783,#36784));
#16474=EDGE_LOOP('',(#36785,#36786,#36787,#36788));
#16475=EDGE_LOOP('',(#36789,#36790,#36791,#36792));
#16476=EDGE_LOOP('',(#36793,#36794,#36795,#36796));
#16477=EDGE_LOOP('',(#36797,#36798,#36799,#36800));
#16478=EDGE_LOOP('',(#36801,#36802,#36803,#36804));
#16479=EDGE_LOOP('',(#36805,#36806,#36807,#36808));
#16480=EDGE_LOOP('',(#36809,#36810,#36811,#36812));
#16481=EDGE_LOOP('',(#36813,#36814,#36815,#36816));
#16482=EDGE_LOOP('',(#36817,#36818,#36819,#36820));
#16483=EDGE_LOOP('',(#36821,#36822,#36823,#36824));
#16484=EDGE_LOOP('',(#36825,#36826,#36827,#36828));
#16485=EDGE_LOOP('',(#36829,#36830,#36831,#36832));
#16486=EDGE_LOOP('',(#36833,#36834,#36835,#36836));
#16487=EDGE_LOOP('',(#36837,#36838,#36839,#36840,#36841,#36842,#36843,#36844,
#36845,#36846,#36847,#36848,#36849,#36850,#36851,#36852,#36853,#36854,#36855,
#36856,#36857,#36858,#36859,#36860,#36861,#36862,#36863,#36864,#36865,#36866,
#36867,#36868));
#16488=EDGE_LOOP('',(#36869,#36870,#36871,#36872));
#16489=EDGE_LOOP('',(#36873,#36874,#36875,#36876));
#16490=EDGE_LOOP('',(#36877,#36878,#36879,#36880));
#16491=EDGE_LOOP('',(#36881,#36882,#36883,#36884));
#16492=EDGE_LOOP('',(#36885,#36886,#36887,#36888));
#16493=EDGE_LOOP('',(#36889,#36890,#36891,#36892));
#16494=EDGE_LOOP('',(#36893,#36894,#36895,#36896));
#16495=EDGE_LOOP('',(#36897,#36898,#36899,#36900));
#16496=EDGE_LOOP('',(#36901,#36902,#36903,#36904));
#16497=EDGE_LOOP('',(#36905,#36906,#36907,#36908));
#16498=EDGE_LOOP('',(#36909,#36910,#36911,#36912));
#16499=EDGE_LOOP('',(#36913,#36914,#36915,#36916));
#16500=EDGE_LOOP('',(#36917,#36918,#36919,#36920));
#16501=EDGE_LOOP('',(#36921,#36922,#36923,#36924,#36925,#36926,#36927));
#16502=EDGE_LOOP('',(#36928,#36929,#36930,#36931));
#16503=EDGE_LOOP('',(#36932,#36933,#36934,#36935));
#16504=EDGE_LOOP('',(#36936,#36937,#36938,#36939));
#16505=EDGE_LOOP('',(#36940,#36941,#36942,#36943));
#16506=EDGE_LOOP('',(#36944,#36945,#36946,#36947));
#16507=EDGE_LOOP('',(#36948,#36949,#36950,#36951));
#16508=EDGE_LOOP('',(#36952,#36953,#36954,#36955));
#16509=EDGE_LOOP('',(#36956,#36957,#36958,#36959));
#16510=EDGE_LOOP('',(#36960,#36961,#36962,#36963));
#16511=EDGE_LOOP('',(#36964,#36965,#36966,#36967));
#16512=EDGE_LOOP('',(#36968,#36969,#36970,#36971));
#16513=EDGE_LOOP('',(#36972,#36973,#36974,#36975));
#16514=EDGE_LOOP('',(#36976,#36977,#36978,#36979));
#16515=EDGE_LOOP('',(#36980,#36981,#36982,#36983));
#16516=EDGE_LOOP('',(#36984,#36985,#36986,#36987,#36988,#36989,#36990,#36991,
#36992,#36993,#36994,#36995,#36996,#36997,#36998,#36999,#37000,#37001,#37002,
#37003,#37004,#37005,#37006,#37007,#37008,#37009,#37010,#37011,#37012,#37013,
#37014,#37015));
#16517=EDGE_LOOP('',(#37016,#37017,#37018,#37019));
#16518=EDGE_LOOP('',(#37020,#37021,#37022,#37023));
#16519=EDGE_LOOP('',(#37024,#37025,#37026,#37027));
#16520=EDGE_LOOP('',(#37028,#37029,#37030,#37031));
#16521=EDGE_LOOP('',(#37032,#37033,#37034,#37035));
#16522=EDGE_LOOP('',(#37036,#37037,#37038,#37039));
#16523=EDGE_LOOP('',(#37040,#37041,#37042,#37043));
#16524=EDGE_LOOP('',(#37044,#37045,#37046,#37047));
#16525=EDGE_LOOP('',(#37048,#37049,#37050,#37051));
#16526=EDGE_LOOP('',(#37052,#37053,#37054,#37055));
#16527=EDGE_LOOP('',(#37056,#37057,#37058,#37059));
#16528=EDGE_LOOP('',(#37060,#37061,#37062,#37063));
#16529=EDGE_LOOP('',(#37064,#37065,#37066,#37067));
#16530=EDGE_LOOP('',(#37068,#37069,#37070,#37071,#37072,#37073,#37074));
#16531=EDGE_LOOP('',(#37075,#37076,#37077,#37078));
#16532=EDGE_LOOP('',(#37079,#37080,#37081,#37082));
#16533=EDGE_LOOP('',(#37083,#37084,#37085,#37086));
#16534=EDGE_LOOP('',(#37087,#37088,#37089,#37090));
#16535=EDGE_LOOP('',(#37091,#37092,#37093,#37094));
#16536=EDGE_LOOP('',(#37095,#37096,#37097,#37098));
#16537=EDGE_LOOP('',(#37099,#37100,#37101,#37102));
#16538=EDGE_LOOP('',(#37103,#37104,#37105,#37106));
#16539=EDGE_LOOP('',(#37107,#37108,#37109,#37110));
#16540=EDGE_LOOP('',(#37111,#37112,#37113,#37114));
#16541=EDGE_LOOP('',(#37115,#37116,#37117,#37118));
#16542=EDGE_LOOP('',(#37119,#37120,#37121,#37122));
#16543=EDGE_LOOP('',(#37123,#37124,#37125,#37126));
#16544=EDGE_LOOP('',(#37127,#37128,#37129,#37130));
#16545=EDGE_LOOP('',(#37131,#37132,#37133,#37134,#37135,#37136,#37137,#37138,
#37139,#37140,#37141,#37142,#37143,#37144,#37145,#37146,#37147,#37148,#37149,
#37150,#37151,#37152,#37153,#37154,#37155,#37156,#37157,#37158,#37159,#37160,
#37161,#37162));
#16546=EDGE_LOOP('',(#37163,#37164,#37165,#37166));
#16547=EDGE_LOOP('',(#37167,#37168,#37169,#37170));
#16548=EDGE_LOOP('',(#37171,#37172,#37173,#37174));
#16549=EDGE_LOOP('',(#37175,#37176,#37177,#37178));
#16550=EDGE_LOOP('',(#37179,#37180,#37181,#37182));
#16551=EDGE_LOOP('',(#37183,#37184,#37185,#37186));
#16552=EDGE_LOOP('',(#37187,#37188,#37189,#37190));
#16553=EDGE_LOOP('',(#37191,#37192,#37193,#37194));
#16554=EDGE_LOOP('',(#37195,#37196,#37197,#37198));
#16555=EDGE_LOOP('',(#37199,#37200,#37201,#37202));
#16556=EDGE_LOOP('',(#37203,#37204,#37205,#37206));
#16557=EDGE_LOOP('',(#37207,#37208,#37209,#37210));
#16558=EDGE_LOOP('',(#37211,#37212,#37213,#37214));
#16559=EDGE_LOOP('',(#37215,#37216,#37217,#37218,#37219,#37220,#37221));
#16560=EDGE_LOOP('',(#37222,#37223,#37224,#37225));
#16561=EDGE_LOOP('',(#37226,#37227,#37228,#37229));
#16562=EDGE_LOOP('',(#37230,#37231,#37232,#37233));
#16563=EDGE_LOOP('',(#37234,#37235,#37236,#37237));
#16564=EDGE_LOOP('',(#37238,#37239,#37240,#37241));
#16565=EDGE_LOOP('',(#37242,#37243,#37244,#37245));
#16566=EDGE_LOOP('',(#37246,#37247,#37248,#37249));
#16567=EDGE_LOOP('',(#37250,#37251,#37252,#37253));
#16568=EDGE_LOOP('',(#37254,#37255,#37256,#37257));
#16569=EDGE_LOOP('',(#37258,#37259,#37260,#37261));
#16570=EDGE_LOOP('',(#37262,#37263,#37264,#37265));
#16571=EDGE_LOOP('',(#37266,#37267,#37268,#37269));
#16572=EDGE_LOOP('',(#37270,#37271,#37272,#37273));
#16573=EDGE_LOOP('',(#37274,#37275,#37276,#37277));
#16574=EDGE_LOOP('',(#37278,#37279,#37280,#37281,#37282,#37283,#37284,#37285,
#37286,#37287,#37288,#37289,#37290,#37291,#37292,#37293,#37294,#37295,#37296,
#37297,#37298,#37299,#37300,#37301,#37302,#37303,#37304,#37305,#37306,#37307,
#37308,#37309));
#16575=EDGE_LOOP('',(#37310,#37311,#37312,#37313));
#16576=EDGE_LOOP('',(#37314,#37315,#37316,#37317));
#16577=EDGE_LOOP('',(#37318,#37319,#37320,#37321));
#16578=EDGE_LOOP('',(#37322,#37323,#37324,#37325));
#16579=EDGE_LOOP('',(#37326,#37327,#37328,#37329));
#16580=EDGE_LOOP('',(#37330,#37331,#37332,#37333));
#16581=EDGE_LOOP('',(#37334,#37335,#37336,#37337));
#16582=EDGE_LOOP('',(#37338,#37339,#37340,#37341));
#16583=EDGE_LOOP('',(#37342,#37343,#37344,#37345));
#16584=EDGE_LOOP('',(#37346,#37347,#37348,#37349));
#16585=EDGE_LOOP('',(#37350,#37351,#37352,#37353));
#16586=EDGE_LOOP('',(#37354,#37355,#37356,#37357));
#16587=EDGE_LOOP('',(#37358,#37359,#37360,#37361));
#16588=EDGE_LOOP('',(#37362,#37363,#37364,#37365,#37366,#37367,#37368));
#16589=EDGE_LOOP('',(#37369,#37370,#37371,#37372));
#16590=EDGE_LOOP('',(#37373,#37374,#37375,#37376));
#16591=EDGE_LOOP('',(#37377,#37378,#37379,#37380));
#16592=EDGE_LOOP('',(#37381,#37382,#37383,#37384));
#16593=EDGE_LOOP('',(#37385,#37386,#37387,#37388));
#16594=EDGE_LOOP('',(#37389,#37390,#37391,#37392));
#16595=EDGE_LOOP('',(#37393,#37394,#37395,#37396));
#16596=EDGE_LOOP('',(#37397,#37398,#37399,#37400));
#16597=EDGE_LOOP('',(#37401,#37402,#37403,#37404));
#16598=EDGE_LOOP('',(#37405,#37406,#37407,#37408));
#16599=EDGE_LOOP('',(#37409,#37410,#37411,#37412));
#16600=EDGE_LOOP('',(#37413,#37414,#37415,#37416));
#16601=EDGE_LOOP('',(#37417,#37418,#37419,#37420));
#16602=EDGE_LOOP('',(#37421,#37422,#37423,#37424));
#16603=EDGE_LOOP('',(#37425,#37426,#37427,#37428,#37429,#37430,#37431,#37432,
#37433,#37434,#37435,#37436,#37437,#37438,#37439,#37440,#37441,#37442,#37443,
#37444,#37445,#37446,#37447,#37448,#37449,#37450,#37451,#37452,#37453,#37454,
#37455,#37456));
#16604=EDGE_LOOP('',(#37457,#37458,#37459,#37460));
#16605=EDGE_LOOP('',(#37461,#37462,#37463,#37464));
#16606=EDGE_LOOP('',(#37465,#37466,#37467,#37468));
#16607=EDGE_LOOP('',(#37469,#37470,#37471,#37472));
#16608=EDGE_LOOP('',(#37473,#37474,#37475,#37476));
#16609=EDGE_LOOP('',(#37477,#37478,#37479,#37480));
#16610=EDGE_LOOP('',(#37481,#37482,#37483,#37484));
#16611=EDGE_LOOP('',(#37485,#37486,#37487,#37488));
#16612=EDGE_LOOP('',(#37489,#37490,#37491,#37492));
#16613=EDGE_LOOP('',(#37493,#37494,#37495,#37496));
#16614=EDGE_LOOP('',(#37497,#37498,#37499,#37500));
#16615=EDGE_LOOP('',(#37501,#37502,#37503,#37504));
#16616=EDGE_LOOP('',(#37505,#37506,#37507,#37508));
#16617=EDGE_LOOP('',(#37509,#37510,#37511,#37512,#37513,#37514,#37515));
#16618=EDGE_LOOP('',(#37516,#37517,#37518,#37519));
#16619=EDGE_LOOP('',(#37520,#37521,#37522,#37523));
#16620=EDGE_LOOP('',(#37524,#37525,#37526,#37527));
#16621=EDGE_LOOP('',(#37528,#37529,#37530,#37531));
#16622=EDGE_LOOP('',(#37532,#37533,#37534,#37535));
#16623=EDGE_LOOP('',(#37536,#37537,#37538,#37539));
#16624=EDGE_LOOP('',(#37540,#37541,#37542,#37543));
#16625=EDGE_LOOP('',(#37544,#37545,#37546,#37547));
#16626=EDGE_LOOP('',(#37548,#37549,#37550,#37551));
#16627=EDGE_LOOP('',(#37552,#37553,#37554,#37555));
#16628=EDGE_LOOP('',(#37556,#37557,#37558,#37559));
#16629=EDGE_LOOP('',(#37560,#37561,#37562,#37563));
#16630=EDGE_LOOP('',(#37564,#37565,#37566,#37567));
#16631=EDGE_LOOP('',(#37568,#37569,#37570,#37571));
#16632=EDGE_LOOP('',(#37572,#37573,#37574,#37575,#37576,#37577,#37578,#37579,
#37580,#37581,#37582,#37583,#37584,#37585,#37586,#37587,#37588,#37589,#37590,
#37591,#37592,#37593,#37594,#37595,#37596,#37597,#37598,#37599,#37600,#37601,
#37602,#37603));
#16633=EDGE_LOOP('',(#37604,#37605,#37606,#37607));
#16634=EDGE_LOOP('',(#37608,#37609,#37610,#37611));
#16635=EDGE_LOOP('',(#37612,#37613,#37614,#37615));
#16636=EDGE_LOOP('',(#37616,#37617,#37618,#37619));
#16637=EDGE_LOOP('',(#37620,#37621,#37622,#37623));
#16638=EDGE_LOOP('',(#37624,#37625,#37626,#37627));
#16639=EDGE_LOOP('',(#37628,#37629,#37630,#37631));
#16640=EDGE_LOOP('',(#37632,#37633,#37634,#37635));
#16641=EDGE_LOOP('',(#37636,#37637,#37638,#37639));
#16642=EDGE_LOOP('',(#37640,#37641,#37642,#37643));
#16643=EDGE_LOOP('',(#37644,#37645,#37646,#37647));
#16644=EDGE_LOOP('',(#37648,#37649,#37650,#37651));
#16645=EDGE_LOOP('',(#37652,#37653,#37654,#37655));
#16646=EDGE_LOOP('',(#37656,#37657,#37658,#37659,#37660,#37661,#37662));
#16647=EDGE_LOOP('',(#37663,#37664,#37665,#37666));
#16648=EDGE_LOOP('',(#37667,#37668,#37669,#37670));
#16649=EDGE_LOOP('',(#37671,#37672,#37673,#37674));
#16650=EDGE_LOOP('',(#37675,#37676,#37677,#37678));
#16651=EDGE_LOOP('',(#37679,#37680,#37681,#37682));
#16652=EDGE_LOOP('',(#37683,#37684,#37685,#37686));
#16653=EDGE_LOOP('',(#37687,#37688,#37689,#37690));
#16654=EDGE_LOOP('',(#37691,#37692,#37693,#37694));
#16655=EDGE_LOOP('',(#37695,#37696,#37697,#37698));
#16656=EDGE_LOOP('',(#37699,#37700,#37701,#37702));
#16657=EDGE_LOOP('',(#37703,#37704,#37705,#37706));
#16658=EDGE_LOOP('',(#37707,#37708,#37709,#37710));
#16659=EDGE_LOOP('',(#37711,#37712,#37713,#37714));
#16660=EDGE_LOOP('',(#37715,#37716,#37717,#37718));
#16661=EDGE_LOOP('',(#37719,#37720,#37721,#37722,#37723,#37724,#37725,#37726,
#37727,#37728,#37729,#37730,#37731,#37732,#37733,#37734,#37735,#37736,#37737,
#37738,#37739,#37740,#37741,#37742,#37743,#37744,#37745,#37746,#37747,#37748,
#37749,#37750));
#16662=EDGE_LOOP('',(#37751,#37752,#37753,#37754));
#16663=EDGE_LOOP('',(#37755,#37756,#37757,#37758));
#16664=EDGE_LOOP('',(#37759,#37760,#37761,#37762));
#16665=EDGE_LOOP('',(#37763,#37764,#37765,#37766));
#16666=EDGE_LOOP('',(#37767,#37768,#37769,#37770));
#16667=EDGE_LOOP('',(#37771,#37772,#37773,#37774));
#16668=EDGE_LOOP('',(#37775,#37776,#37777,#37778));
#16669=EDGE_LOOP('',(#37779,#37780,#37781,#37782));
#16670=EDGE_LOOP('',(#37783,#37784,#37785,#37786));
#16671=EDGE_LOOP('',(#37787,#37788,#37789,#37790));
#16672=EDGE_LOOP('',(#37791,#37792,#37793,#37794));
#16673=EDGE_LOOP('',(#37795,#37796,#37797,#37798));
#16674=EDGE_LOOP('',(#37799,#37800,#37801,#37802));
#16675=EDGE_LOOP('',(#37803,#37804,#37805,#37806,#37807,#37808,#37809));
#16676=EDGE_LOOP('',(#37810,#37811,#37812,#37813));
#16677=EDGE_LOOP('',(#37814,#37815,#37816,#37817));
#16678=EDGE_LOOP('',(#37818,#37819,#37820,#37821));
#16679=EDGE_LOOP('',(#37822,#37823,#37824,#37825));
#16680=EDGE_LOOP('',(#37826,#37827,#37828,#37829));
#16681=EDGE_LOOP('',(#37830,#37831,#37832,#37833));
#16682=EDGE_LOOP('',(#37834,#37835,#37836,#37837));
#16683=EDGE_LOOP('',(#37838,#37839,#37840,#37841));
#16684=EDGE_LOOP('',(#37842,#37843,#37844,#37845));
#16685=EDGE_LOOP('',(#37846,#37847,#37848,#37849));
#16686=EDGE_LOOP('',(#37850,#37851,#37852,#37853));
#16687=EDGE_LOOP('',(#37854,#37855,#37856,#37857));
#16688=EDGE_LOOP('',(#37858,#37859,#37860,#37861));
#16689=EDGE_LOOP('',(#37862,#37863,#37864,#37865));
#16690=EDGE_LOOP('',(#37866,#37867,#37868,#37869,#37870,#37871,#37872,#37873,
#37874,#37875,#37876,#37877,#37878,#37879,#37880,#37881,#37882,#37883,#37884,
#37885,#37886,#37887,#37888,#37889,#37890,#37891,#37892,#37893,#37894,#37895,
#37896,#37897));
#16691=EDGE_LOOP('',(#37898,#37899,#37900,#37901));
#16692=EDGE_LOOP('',(#37902,#37903,#37904,#37905));
#16693=EDGE_LOOP('',(#37906,#37907,#37908,#37909));
#16694=EDGE_LOOP('',(#37910,#37911,#37912,#37913));
#16695=EDGE_LOOP('',(#37914,#37915,#37916,#37917));
#16696=EDGE_LOOP('',(#37918,#37919,#37920,#37921));
#16697=EDGE_LOOP('',(#37922,#37923,#37924,#37925));
#16698=EDGE_LOOP('',(#37926,#37927,#37928,#37929));
#16699=EDGE_LOOP('',(#37930,#37931,#37932,#37933));
#16700=EDGE_LOOP('',(#37934,#37935,#37936,#37937));
#16701=EDGE_LOOP('',(#37938,#37939,#37940,#37941));
#16702=EDGE_LOOP('',(#37942,#37943,#37944,#37945));
#16703=EDGE_LOOP('',(#37946,#37947,#37948,#37949));
#16704=EDGE_LOOP('',(#37950,#37951,#37952,#37953,#37954,#37955,#37956));
#16705=EDGE_LOOP('',(#37957,#37958,#37959,#37960));
#16706=EDGE_LOOP('',(#37961,#37962,#37963,#37964));
#16707=EDGE_LOOP('',(#37965,#37966,#37967,#37968));
#16708=EDGE_LOOP('',(#37969,#37970,#37971,#37972));
#16709=EDGE_LOOP('',(#37973,#37974,#37975,#37976));
#16710=EDGE_LOOP('',(#37977,#37978,#37979,#37980));
#16711=EDGE_LOOP('',(#37981,#37982,#37983,#37984));
#16712=EDGE_LOOP('',(#37985,#37986,#37987,#37988));
#16713=EDGE_LOOP('',(#37989,#37990,#37991,#37992));
#16714=EDGE_LOOP('',(#37993,#37994,#37995,#37996));
#16715=EDGE_LOOP('',(#37997,#37998,#37999,#38000));
#16716=EDGE_LOOP('',(#38001,#38002,#38003,#38004));
#16717=EDGE_LOOP('',(#38005,#38006,#38007,#38008));
#16718=EDGE_LOOP('',(#38009,#38010,#38011,#38012));
#16719=EDGE_LOOP('',(#38013,#38014,#38015,#38016,#38017,#38018,#38019,#38020,
#38021,#38022,#38023,#38024,#38025,#38026,#38027,#38028,#38029,#38030,#38031,
#38032,#38033,#38034,#38035,#38036,#38037,#38038,#38039,#38040,#38041,#38042,
#38043,#38044));
#16720=EDGE_LOOP('',(#38045,#38046,#38047,#38048));
#16721=EDGE_LOOP('',(#38049,#38050,#38051,#38052));
#16722=EDGE_LOOP('',(#38053,#38054,#38055,#38056));
#16723=EDGE_LOOP('',(#38057,#38058,#38059,#38060));
#16724=EDGE_LOOP('',(#38061,#38062,#38063,#38064));
#16725=EDGE_LOOP('',(#38065,#38066,#38067,#38068));
#16726=EDGE_LOOP('',(#38069,#38070,#38071,#38072));
#16727=EDGE_LOOP('',(#38073,#38074,#38075,#38076));
#16728=EDGE_LOOP('',(#38077,#38078,#38079,#38080));
#16729=EDGE_LOOP('',(#38081,#38082,#38083,#38084));
#16730=EDGE_LOOP('',(#38085,#38086,#38087,#38088));
#16731=EDGE_LOOP('',(#38089,#38090,#38091,#38092));
#16732=EDGE_LOOP('',(#38093,#38094,#38095,#38096));
#16733=EDGE_LOOP('',(#38097,#38098,#38099,#38100,#38101,#38102,#38103));
#16734=EDGE_LOOP('',(#38104,#38105,#38106,#38107));
#16735=EDGE_LOOP('',(#38108,#38109,#38110,#38111));
#16736=EDGE_LOOP('',(#38112,#38113,#38114,#38115));
#16737=EDGE_LOOP('',(#38116,#38117,#38118,#38119));
#16738=EDGE_LOOP('',(#38120,#38121,#38122,#38123));
#16739=EDGE_LOOP('',(#38124,#38125,#38126,#38127));
#16740=EDGE_LOOP('',(#38128,#38129,#38130,#38131));
#16741=EDGE_LOOP('',(#38132,#38133,#38134,#38135));
#16742=EDGE_LOOP('',(#38136,#38137,#38138,#38139));
#16743=EDGE_LOOP('',(#38140,#38141,#38142,#38143));
#16744=EDGE_LOOP('',(#38144,#38145,#38146,#38147));
#16745=EDGE_LOOP('',(#38148,#38149,#38150,#38151));
#16746=EDGE_LOOP('',(#38152,#38153,#38154,#38155));
#16747=EDGE_LOOP('',(#38156,#38157,#38158,#38159));
#16748=EDGE_LOOP('',(#38160,#38161,#38162,#38163,#38164,#38165,#38166,#38167,
#38168,#38169,#38170,#38171,#38172,#38173,#38174,#38175,#38176,#38177,#38178,
#38179,#38180,#38181,#38182,#38183,#38184,#38185,#38186,#38187,#38188,#38189,
#38190,#38191));
#16749=EDGE_LOOP('',(#38192,#38193,#38194,#38195));
#16750=EDGE_LOOP('',(#38196,#38197,#38198,#38199));
#16751=EDGE_LOOP('',(#38200,#38201,#38202,#38203));
#16752=EDGE_LOOP('',(#38204,#38205,#38206,#38207));
#16753=EDGE_LOOP('',(#38208,#38209,#38210,#38211));
#16754=EDGE_LOOP('',(#38212,#38213,#38214,#38215));
#16755=EDGE_LOOP('',(#38216,#38217,#38218,#38219));
#16756=EDGE_LOOP('',(#38220,#38221,#38222,#38223));
#16757=EDGE_LOOP('',(#38224,#38225,#38226,#38227));
#16758=EDGE_LOOP('',(#38228,#38229,#38230,#38231));
#16759=EDGE_LOOP('',(#38232,#38233,#38234,#38235));
#16760=EDGE_LOOP('',(#38236,#38237,#38238,#38239));
#16761=EDGE_LOOP('',(#38240,#38241,#38242,#38243));
#16762=EDGE_LOOP('',(#38244,#38245,#38246,#38247,#38248,#38249,#38250));
#16763=EDGE_LOOP('',(#38251,#38252,#38253,#38254));
#16764=EDGE_LOOP('',(#38255,#38256,#38257,#38258));
#16765=EDGE_LOOP('',(#38259,#38260,#38261,#38262));
#16766=EDGE_LOOP('',(#38263,#38264,#38265,#38266));
#16767=EDGE_LOOP('',(#38267,#38268,#38269,#38270));
#16768=EDGE_LOOP('',(#38271,#38272,#38273,#38274));
#16769=EDGE_LOOP('',(#38275,#38276,#38277,#38278));
#16770=EDGE_LOOP('',(#38279,#38280,#38281,#38282));
#16771=EDGE_LOOP('',(#38283,#38284,#38285,#38286));
#16772=EDGE_LOOP('',(#38287,#38288,#38289,#38290));
#16773=EDGE_LOOP('',(#38291,#38292,#38293,#38294));
#16774=EDGE_LOOP('',(#38295,#38296,#38297,#38298));
#16775=EDGE_LOOP('',(#38299,#38300,#38301,#38302));
#16776=EDGE_LOOP('',(#38303,#38304,#38305,#38306,#38307));
#16777=EDGE_LOOP('',(#38308,#38309,#38310,#38311,#38312,#38313,#38314,#38315,
#38316,#38317,#38318,#38319,#38320,#38321,#38322,#38323,#38324,#38325,#38326,
#38327,#38328,#38329,#38330,#38331,#38332,#38333,#38334,#38335,#38336,#38337,
#38338,#38339));
#16778=EDGE_LOOP('',(#38340,#38341,#38342,#38343));
#16779=EDGE_LOOP('',(#38344,#38345,#38346,#38347));
#16780=EDGE_LOOP('',(#38348,#38349,#38350,#38351));
#16781=EDGE_LOOP('',(#38352,#38353,#38354,#38355));
#16782=EDGE_LOOP('',(#38356,#38357,#38358,#38359));
#16783=EDGE_LOOP('',(#38360,#38361,#38362,#38363));
#16784=EDGE_LOOP('',(#38364,#38365,#38366,#38367));
#16785=EDGE_LOOP('',(#38368,#38369,#38370,#38371));
#16786=EDGE_LOOP('',(#38372,#38373,#38374,#38375));
#16787=EDGE_LOOP('',(#38376,#38377,#38378,#38379));
#16788=EDGE_LOOP('',(#38380,#38381,#38382,#38383));
#16789=EDGE_LOOP('',(#38384,#38385,#38386,#38387));
#16790=EDGE_LOOP('',(#38388,#38389,#38390,#38391));
#16791=EDGE_LOOP('',(#38392,#38393,#38394,#38395,#38396,#38397,#38398));
#16792=EDGE_LOOP('',(#38399,#38400,#38401,#38402));
#16793=EDGE_LOOP('',(#38403,#38404,#38405,#38406));
#16794=EDGE_LOOP('',(#38407,#38408,#38409,#38410));
#16795=EDGE_LOOP('',(#38411,#38412,#38413,#38414));
#16796=EDGE_LOOP('',(#38415,#38416,#38417,#38418));
#16797=EDGE_LOOP('',(#38419,#38420,#38421,#38422));
#16798=EDGE_LOOP('',(#38423,#38424,#38425,#38426));
#16799=EDGE_LOOP('',(#38427,#38428,#38429,#38430));
#16800=EDGE_LOOP('',(#38431,#38432,#38433,#38434));
#16801=EDGE_LOOP('',(#38435,#38436,#38437,#38438));
#16802=EDGE_LOOP('',(#38439,#38440,#38441,#38442));
#16803=EDGE_LOOP('',(#38443,#38444,#38445,#38446));
#16804=EDGE_LOOP('',(#38447,#38448,#38449,#38450));
#16805=EDGE_LOOP('',(#38451,#38452,#38453,#38454));
#16806=EDGE_LOOP('',(#38455,#38456,#38457,#38458,#38459,#38460,#38461,#38462,
#38463,#38464,#38465,#38466,#38467,#38468,#38469,#38470,#38471,#38472,#38473,
#38474,#38475,#38476,#38477,#38478,#38479,#38480,#38481,#38482,#38483,#38484,
#38485,#38486));
#16807=EDGE_LOOP('',(#38487,#38488,#38489,#38490));
#16808=EDGE_LOOP('',(#38491,#38492,#38493,#38494));
#16809=EDGE_LOOP('',(#38495,#38496,#38497,#38498));
#16810=EDGE_LOOP('',(#38499,#38500,#38501,#38502));
#16811=EDGE_LOOP('',(#38503,#38504,#38505,#38506));
#16812=EDGE_LOOP('',(#38507,#38508,#38509,#38510));
#16813=EDGE_LOOP('',(#38511,#38512,#38513,#38514));
#16814=EDGE_LOOP('',(#38515,#38516,#38517,#38518));
#16815=EDGE_LOOP('',(#38519,#38520,#38521,#38522));
#16816=EDGE_LOOP('',(#38523,#38524,#38525,#38526));
#16817=EDGE_LOOP('',(#38527,#38528,#38529,#38530));
#16818=EDGE_LOOP('',(#38531,#38532,#38533,#38534));
#16819=EDGE_LOOP('',(#38535,#38536,#38537,#38538));
#16820=EDGE_LOOP('',(#38539,#38540,#38541,#38542,#38543,#38544,#38545));
#16821=EDGE_LOOP('',(#38546,#38547,#38548,#38549));
#16822=EDGE_LOOP('',(#38550,#38551,#38552,#38553));
#16823=EDGE_LOOP('',(#38554,#38555,#38556,#38557));
#16824=EDGE_LOOP('',(#38558,#38559,#38560,#38561));
#16825=EDGE_LOOP('',(#38562,#38563,#38564,#38565));
#16826=EDGE_LOOP('',(#38566,#38567,#38568,#38569));
#16827=EDGE_LOOP('',(#38570,#38571,#38572,#38573));
#16828=EDGE_LOOP('',(#38574,#38575,#38576,#38577));
#16829=EDGE_LOOP('',(#38578,#38579,#38580,#38581));
#16830=EDGE_LOOP('',(#38582,#38583,#38584,#38585));
#16831=EDGE_LOOP('',(#38586,#38587,#38588,#38589));
#16832=EDGE_LOOP('',(#38590,#38591,#38592,#38593));
#16833=EDGE_LOOP('',(#38594,#38595,#38596,#38597));
#16834=EDGE_LOOP('',(#38598,#38599,#38600,#38601));
#16835=EDGE_LOOP('',(#38602,#38603,#38604,#38605,#38606,#38607,#38608,#38609,
#38610,#38611,#38612,#38613,#38614,#38615,#38616,#38617,#38618,#38619,#38620,
#38621,#38622,#38623,#38624,#38625,#38626,#38627,#38628,#38629,#38630,#38631,
#38632,#38633));
#16836=EDGE_LOOP('',(#38634,#38635,#38636,#38637));
#16837=EDGE_LOOP('',(#38638,#38639,#38640,#38641));
#16838=EDGE_LOOP('',(#38642,#38643,#38644,#38645));
#16839=EDGE_LOOP('',(#38646,#38647,#38648,#38649));
#16840=EDGE_LOOP('',(#38650,#38651,#38652,#38653));
#16841=EDGE_LOOP('',(#38654,#38655,#38656,#38657));
#16842=EDGE_LOOP('',(#38658,#38659,#38660,#38661));
#16843=EDGE_LOOP('',(#38662,#38663,#38664,#38665));
#16844=EDGE_LOOP('',(#38666,#38667,#38668,#38669));
#16845=EDGE_LOOP('',(#38670,#38671,#38672,#38673));
#16846=EDGE_LOOP('',(#38674,#38675,#38676,#38677));
#16847=EDGE_LOOP('',(#38678,#38679,#38680,#38681));
#16848=EDGE_LOOP('',(#38682,#38683,#38684,#38685));
#16849=EDGE_LOOP('',(#38686,#38687,#38688,#38689,#38690,#38691,#38692));
#16850=EDGE_LOOP('',(#38693,#38694,#38695,#38696));
#16851=EDGE_LOOP('',(#38697,#38698,#38699,#38700));
#16852=EDGE_LOOP('',(#38701,#38702,#38703,#38704));
#16853=EDGE_LOOP('',(#38705,#38706,#38707,#38708));
#16854=EDGE_LOOP('',(#38709,#38710,#38711,#38712));
#16855=EDGE_LOOP('',(#38713,#38714,#38715,#38716));
#16856=EDGE_LOOP('',(#38717,#38718,#38719,#38720));
#16857=EDGE_LOOP('',(#38721,#38722,#38723,#38724));
#16858=EDGE_LOOP('',(#38725,#38726,#38727,#38728));
#16859=EDGE_LOOP('',(#38729,#38730,#38731,#38732));
#16860=EDGE_LOOP('',(#38733,#38734,#38735,#38736));
#16861=EDGE_LOOP('',(#38737,#38738,#38739,#38740));
#16862=EDGE_LOOP('',(#38741,#38742,#38743,#38744));
#16863=EDGE_LOOP('',(#38745,#38746,#38747,#38748));
#16864=EDGE_LOOP('',(#38749,#38750,#38751,#38752,#38753,#38754,#38755,#38756,
#38757,#38758,#38759,#38760,#38761,#38762,#38763,#38764,#38765,#38766,#38767,
#38768,#38769,#38770,#38771,#38772,#38773,#38774,#38775,#38776,#38777,#38778,
#38779,#38780));
#16865=EDGE_LOOP('',(#38781,#38782,#38783,#38784));
#16866=EDGE_LOOP('',(#38785,#38786,#38787,#38788));
#16867=EDGE_LOOP('',(#38789,#38790,#38791,#38792));
#16868=EDGE_LOOP('',(#38793,#38794,#38795,#38796));
#16869=EDGE_LOOP('',(#38797,#38798,#38799,#38800));
#16870=EDGE_LOOP('',(#38801,#38802,#38803,#38804));
#16871=EDGE_LOOP('',(#38805,#38806,#38807,#38808));
#16872=EDGE_LOOP('',(#38809,#38810,#38811,#38812));
#16873=EDGE_LOOP('',(#38813,#38814,#38815,#38816));
#16874=EDGE_LOOP('',(#38817,#38818,#38819,#38820));
#16875=EDGE_LOOP('',(#38821,#38822,#38823,#38824));
#16876=EDGE_LOOP('',(#38825,#38826,#38827,#38828));
#16877=EDGE_LOOP('',(#38829,#38830,#38831,#38832));
#16878=EDGE_LOOP('',(#38833,#38834,#38835,#38836,#38837,#38838,#38839));
#16879=EDGE_LOOP('',(#38840,#38841,#38842,#38843));
#16880=EDGE_LOOP('',(#38844,#38845,#38846,#38847));
#16881=EDGE_LOOP('',(#38848,#38849,#38850,#38851));
#16882=EDGE_LOOP('',(#38852,#38853,#38854,#38855));
#16883=EDGE_LOOP('',(#38856,#38857,#38858,#38859));
#16884=EDGE_LOOP('',(#38860,#38861,#38862,#38863));
#16885=EDGE_LOOP('',(#38864,#38865,#38866,#38867));
#16886=EDGE_LOOP('',(#38868,#38869,#38870,#38871));
#16887=EDGE_LOOP('',(#38872,#38873,#38874,#38875));
#16888=EDGE_LOOP('',(#38876,#38877,#38878,#38879));
#16889=EDGE_LOOP('',(#38880,#38881,#38882,#38883));
#16890=EDGE_LOOP('',(#38884,#38885,#38886,#38887));
#16891=EDGE_LOOP('',(#38888,#38889,#38890,#38891));
#16892=EDGE_LOOP('',(#38892,#38893,#38894,#38895));
#16893=EDGE_LOOP('',(#38896,#38897,#38898,#38899,#38900,#38901,#38902,#38903,
#38904,#38905,#38906,#38907,#38908,#38909,#38910,#38911,#38912,#38913,#38914,
#38915,#38916,#38917,#38918,#38919,#38920,#38921,#38922,#38923,#38924,#38925,
#38926,#38927));
#16894=EDGE_LOOP('',(#38928,#38929,#38930,#38931));
#16895=EDGE_LOOP('',(#38932,#38933,#38934,#38935));
#16896=EDGE_LOOP('',(#38936,#38937,#38938,#38939));
#16897=EDGE_LOOP('',(#38940,#38941,#38942,#38943));
#16898=EDGE_LOOP('',(#38944,#38945,#38946,#38947));
#16899=EDGE_LOOP('',(#38948,#38949,#38950,#38951));
#16900=EDGE_LOOP('',(#38952,#38953,#38954,#38955));
#16901=EDGE_LOOP('',(#38956,#38957,#38958,#38959));
#16902=EDGE_LOOP('',(#38960,#38961,#38962,#38963));
#16903=EDGE_LOOP('',(#38964,#38965,#38966,#38967));
#16904=EDGE_LOOP('',(#38968,#38969,#38970,#38971));
#16905=EDGE_LOOP('',(#38972,#38973,#38974,#38975));
#16906=EDGE_LOOP('',(#38976,#38977,#38978,#38979));
#16907=EDGE_LOOP('',(#38980,#38981,#38982,#38983,#38984,#38985,#38986));
#16908=EDGE_LOOP('',(#38987,#38988,#38989,#38990));
#16909=EDGE_LOOP('',(#38991,#38992,#38993,#38994));
#16910=EDGE_LOOP('',(#38995,#38996,#38997,#38998));
#16911=EDGE_LOOP('',(#38999,#39000,#39001,#39002));
#16912=EDGE_LOOP('',(#39003,#39004,#39005,#39006));
#16913=EDGE_LOOP('',(#39007,#39008,#39009,#39010));
#16914=EDGE_LOOP('',(#39011,#39012,#39013,#39014));
#16915=EDGE_LOOP('',(#39015,#39016,#39017,#39018));
#16916=EDGE_LOOP('',(#39019,#39020,#39021,#39022));
#16917=EDGE_LOOP('',(#39023,#39024,#39025,#39026));
#16918=EDGE_LOOP('',(#39027,#39028,#39029,#39030));
#16919=EDGE_LOOP('',(#39031,#39032,#39033,#39034));
#16920=EDGE_LOOP('',(#39035,#39036,#39037,#39038));
#16921=EDGE_LOOP('',(#39039,#39040,#39041,#39042));
#16922=EDGE_LOOP('',(#39043,#39044,#39045,#39046,#39047,#39048,#39049,#39050,
#39051,#39052,#39053,#39054,#39055,#39056,#39057,#39058,#39059,#39060,#39061,
#39062,#39063,#39064,#39065,#39066,#39067,#39068,#39069,#39070,#39071,#39072,
#39073,#39074));
#16923=EDGE_LOOP('',(#39075,#39076,#39077,#39078));
#16924=EDGE_LOOP('',(#39079,#39080,#39081,#39082));
#16925=EDGE_LOOP('',(#39083,#39084,#39085,#39086));
#16926=EDGE_LOOP('',(#39087,#39088,#39089,#39090));
#16927=EDGE_LOOP('',(#39091,#39092,#39093,#39094));
#16928=EDGE_LOOP('',(#39095,#39096,#39097,#39098));
#16929=EDGE_LOOP('',(#39099,#39100,#39101,#39102));
#16930=EDGE_LOOP('',(#39103,#39104,#39105,#39106));
#16931=EDGE_LOOP('',(#39107,#39108,#39109,#39110));
#16932=EDGE_LOOP('',(#39111,#39112,#39113,#39114));
#16933=EDGE_LOOP('',(#39115,#39116,#39117,#39118));
#16934=EDGE_LOOP('',(#39119,#39120,#39121,#39122));
#16935=EDGE_LOOP('',(#39123,#39124,#39125,#39126));
#16936=EDGE_LOOP('',(#39127,#39128,#39129,#39130,#39131,#39132,#39133));
#16937=EDGE_LOOP('',(#39134,#39135,#39136,#39137));
#16938=EDGE_LOOP('',(#39138,#39139,#39140,#39141));
#16939=EDGE_LOOP('',(#39142,#39143,#39144,#39145));
#16940=EDGE_LOOP('',(#39146,#39147,#39148,#39149));
#16941=EDGE_LOOP('',(#39150,#39151,#39152,#39153));
#16942=EDGE_LOOP('',(#39154,#39155,#39156,#39157));
#16943=EDGE_LOOP('',(#39158,#39159,#39160,#39161));
#16944=EDGE_LOOP('',(#39162,#39163,#39164,#39165));
#16945=EDGE_LOOP('',(#39166,#39167,#39168,#39169));
#16946=EDGE_LOOP('',(#39170,#39171,#39172,#39173));
#16947=EDGE_LOOP('',(#39174,#39175,#39176,#39177));
#16948=EDGE_LOOP('',(#39178,#39179,#39180,#39181));
#16949=EDGE_LOOP('',(#39182,#39183,#39184,#39185));
#16950=EDGE_LOOP('',(#39186,#39187,#39188,#39189));
#16951=EDGE_LOOP('',(#39190,#39191,#39192,#39193,#39194,#39195,#39196,#39197,
#39198,#39199,#39200,#39201,#39202,#39203,#39204,#39205,#39206,#39207,#39208,
#39209,#39210,#39211,#39212,#39213,#39214,#39215,#39216,#39217,#39218,#39219,
#39220,#39221));
#16952=EDGE_LOOP('',(#39222,#39223,#39224,#39225));
#16953=EDGE_LOOP('',(#39226,#39227,#39228,#39229));
#16954=EDGE_LOOP('',(#39230,#39231,#39232,#39233));
#16955=EDGE_LOOP('',(#39234,#39235,#39236,#39237));
#16956=EDGE_LOOP('',(#39238,#39239,#39240,#39241));
#16957=EDGE_LOOP('',(#39242,#39243,#39244,#39245));
#16958=EDGE_LOOP('',(#39246,#39247,#39248,#39249));
#16959=EDGE_LOOP('',(#39250,#39251,#39252,#39253));
#16960=EDGE_LOOP('',(#39254,#39255,#39256,#39257));
#16961=EDGE_LOOP('',(#39258,#39259,#39260,#39261));
#16962=EDGE_LOOP('',(#39262,#39263,#39264,#39265));
#16963=EDGE_LOOP('',(#39266,#39267,#39268,#39269));
#16964=EDGE_LOOP('',(#39270,#39271,#39272,#39273));
#16965=EDGE_LOOP('',(#39274,#39275,#39276,#39277,#39278,#39279,#39280));
#16966=EDGE_LOOP('',(#39281,#39282,#39283,#39284));
#16967=EDGE_LOOP('',(#39285,#39286,#39287,#39288));
#16968=EDGE_LOOP('',(#39289,#39290,#39291,#39292));
#16969=EDGE_LOOP('',(#39293,#39294,#39295,#39296));
#16970=EDGE_LOOP('',(#39297,#39298,#39299,#39300));
#16971=EDGE_LOOP('',(#39301,#39302,#39303,#39304));
#16972=EDGE_LOOP('',(#39305,#39306,#39307,#39308));
#16973=EDGE_LOOP('',(#39309,#39310,#39311,#39312));
#16974=EDGE_LOOP('',(#39313,#39314,#39315,#39316));
#16975=EDGE_LOOP('',(#39317,#39318,#39319,#39320));
#16976=EDGE_LOOP('',(#39321,#39322,#39323,#39324));
#16977=EDGE_LOOP('',(#39325,#39326,#39327,#39328));
#16978=EDGE_LOOP('',(#39329,#39330,#39331,#39332));
#16979=EDGE_LOOP('',(#39333,#39334,#39335,#39336));
#16980=EDGE_LOOP('',(#39337,#39338,#39339,#39340,#39341,#39342,#39343,#39344,
#39345,#39346,#39347,#39348,#39349,#39350,#39351,#39352,#39353,#39354,#39355,
#39356,#39357,#39358,#39359,#39360,#39361,#39362,#39363,#39364,#39365,#39366,
#39367,#39368));
#16981=EDGE_LOOP('',(#39369,#39370,#39371,#39372));
#16982=EDGE_LOOP('',(#39373,#39374,#39375,#39376));
#16983=EDGE_LOOP('',(#39377,#39378,#39379,#39380));
#16984=EDGE_LOOP('',(#39381,#39382,#39383,#39384));
#16985=EDGE_LOOP('',(#39385,#39386,#39387,#39388));
#16986=EDGE_LOOP('',(#39389,#39390,#39391,#39392));
#16987=EDGE_LOOP('',(#39393,#39394,#39395,#39396));
#16988=EDGE_LOOP('',(#39397,#39398,#39399,#39400));
#16989=EDGE_LOOP('',(#39401,#39402,#39403,#39404));
#16990=EDGE_LOOP('',(#39405,#39406,#39407,#39408));
#16991=EDGE_LOOP('',(#39409,#39410,#39411,#39412));
#16992=EDGE_LOOP('',(#39413,#39414,#39415,#39416));
#16993=EDGE_LOOP('',(#39417,#39418,#39419,#39420));
#16994=EDGE_LOOP('',(#39421,#39422,#39423,#39424,#39425,#39426,#39427));
#16995=EDGE_LOOP('',(#39428,#39429,#39430,#39431));
#16996=EDGE_LOOP('',(#39432,#39433,#39434,#39435));
#16997=EDGE_LOOP('',(#39436,#39437,#39438,#39439));
#16998=EDGE_LOOP('',(#39440,#39441,#39442,#39443));
#16999=EDGE_LOOP('',(#39444,#39445,#39446,#39447));
#17000=EDGE_LOOP('',(#39448,#39449,#39450,#39451));
#17001=EDGE_LOOP('',(#39452,#39453,#39454,#39455));
#17002=EDGE_LOOP('',(#39456,#39457,#39458,#39459));
#17003=EDGE_LOOP('',(#39460,#39461,#39462,#39463));
#17004=EDGE_LOOP('',(#39464,#39465,#39466,#39467));
#17005=EDGE_LOOP('',(#39468,#39469,#39470,#39471));
#17006=EDGE_LOOP('',(#39472,#39473,#39474,#39475));
#17007=EDGE_LOOP('',(#39476,#39477,#39478,#39479));
#17008=EDGE_LOOP('',(#39480,#39481,#39482,#39483));
#17009=EDGE_LOOP('',(#39484,#39485,#39486,#39487,#39488,#39489,#39490,#39491,
#39492,#39493,#39494,#39495,#39496,#39497,#39498,#39499,#39500,#39501,#39502,
#39503,#39504,#39505,#39506,#39507,#39508,#39509,#39510,#39511,#39512,#39513,
#39514,#39515));
#17010=EDGE_LOOP('',(#39516,#39517,#39518,#39519));
#17011=EDGE_LOOP('',(#39520,#39521,#39522,#39523));
#17012=EDGE_LOOP('',(#39524,#39525,#39526,#39527));
#17013=EDGE_LOOP('',(#39528,#39529,#39530,#39531));
#17014=EDGE_LOOP('',(#39532,#39533,#39534,#39535));
#17015=EDGE_LOOP('',(#39536,#39537,#39538,#39539));
#17016=EDGE_LOOP('',(#39540,#39541,#39542,#39543));
#17017=EDGE_LOOP('',(#39544,#39545,#39546,#39547));
#17018=EDGE_LOOP('',(#39548,#39549,#39550,#39551));
#17019=EDGE_LOOP('',(#39552,#39553,#39554,#39555));
#17020=EDGE_LOOP('',(#39556,#39557,#39558,#39559));
#17021=EDGE_LOOP('',(#39560,#39561,#39562,#39563));
#17022=EDGE_LOOP('',(#39564,#39565,#39566,#39567));
#17023=EDGE_LOOP('',(#39568,#39569,#39570,#39571,#39572,#39573,#39574));
#17024=EDGE_LOOP('',(#39575,#39576,#39577,#39578));
#17025=EDGE_LOOP('',(#39579,#39580,#39581,#39582));
#17026=EDGE_LOOP('',(#39583,#39584,#39585,#39586));
#17027=EDGE_LOOP('',(#39587,#39588,#39589,#39590));
#17028=EDGE_LOOP('',(#39591,#39592,#39593,#39594));
#17029=EDGE_LOOP('',(#39595,#39596,#39597,#39598));
#17030=EDGE_LOOP('',(#39599,#39600,#39601,#39602));
#17031=EDGE_LOOP('',(#39603,#39604,#39605,#39606));
#17032=EDGE_LOOP('',(#39607,#39608,#39609,#39610));
#17033=EDGE_LOOP('',(#39611,#39612,#39613,#39614));
#17034=EDGE_LOOP('',(#39615,#39616,#39617,#39618));
#17035=EDGE_LOOP('',(#39619,#39620,#39621,#39622));
#17036=EDGE_LOOP('',(#39623,#39624,#39625,#39626));
#17037=EDGE_LOOP('',(#39627,#39628,#39629,#39630));
#17038=EDGE_LOOP('',(#39631,#39632,#39633,#39634,#39635,#39636,#39637,#39638,
#39639,#39640,#39641,#39642,#39643,#39644,#39645,#39646,#39647,#39648,#39649,
#39650,#39651,#39652,#39653,#39654,#39655,#39656,#39657,#39658,#39659,#39660,
#39661,#39662));
#17039=EDGE_LOOP('',(#39663,#39664,#39665,#39666));
#17040=EDGE_LOOP('',(#39667,#39668,#39669,#39670));
#17041=EDGE_LOOP('',(#39671,#39672,#39673,#39674));
#17042=EDGE_LOOP('',(#39675,#39676,#39677,#39678));
#17043=EDGE_LOOP('',(#39679,#39680,#39681,#39682));
#17044=EDGE_LOOP('',(#39683,#39684,#39685,#39686));
#17045=EDGE_LOOP('',(#39687,#39688,#39689,#39690));
#17046=EDGE_LOOP('',(#39691,#39692,#39693,#39694));
#17047=EDGE_LOOP('',(#39695,#39696,#39697,#39698));
#17048=EDGE_LOOP('',(#39699,#39700,#39701,#39702));
#17049=EDGE_LOOP('',(#39703,#39704,#39705,#39706));
#17050=EDGE_LOOP('',(#39707,#39708,#39709,#39710));
#17051=EDGE_LOOP('',(#39711,#39712,#39713,#39714));
#17052=EDGE_LOOP('',(#39715,#39716,#39717,#39718,#39719,#39720,#39721));
#17053=EDGE_LOOP('',(#39722,#39723,#39724,#39725));
#17054=EDGE_LOOP('',(#39726,#39727,#39728,#39729));
#17055=EDGE_LOOP('',(#39730,#39731,#39732,#39733));
#17056=EDGE_LOOP('',(#39734,#39735,#39736,#39737));
#17057=EDGE_LOOP('',(#39738,#39739,#39740,#39741));
#17058=EDGE_LOOP('',(#39742,#39743,#39744,#39745));
#17059=EDGE_LOOP('',(#39746,#39747,#39748,#39749));
#17060=EDGE_LOOP('',(#39750,#39751,#39752,#39753));
#17061=EDGE_LOOP('',(#39754,#39755,#39756,#39757));
#17062=EDGE_LOOP('',(#39758,#39759,#39760,#39761));
#17063=EDGE_LOOP('',(#39762,#39763,#39764,#39765));
#17064=EDGE_LOOP('',(#39766,#39767,#39768,#39769));
#17065=EDGE_LOOP('',(#39770,#39771,#39772,#39773));
#17066=EDGE_LOOP('',(#39774,#39775,#39776,#39777));
#17067=EDGE_LOOP('',(#39778,#39779,#39780,#39781,#39782,#39783,#39784,#39785,
#39786,#39787,#39788,#39789,#39790,#39791,#39792,#39793,#39794,#39795,#39796,
#39797,#39798,#39799,#39800,#39801,#39802,#39803,#39804,#39805,#39806,#39807,
#39808,#39809));
#17068=EDGE_LOOP('',(#39810,#39811,#39812,#39813));
#17069=EDGE_LOOP('',(#39814,#39815,#39816,#39817));
#17070=EDGE_LOOP('',(#39818,#39819,#39820,#39821));
#17071=EDGE_LOOP('',(#39822,#39823,#39824,#39825));
#17072=EDGE_LOOP('',(#39826,#39827,#39828,#39829));
#17073=EDGE_LOOP('',(#39830,#39831,#39832,#39833));
#17074=EDGE_LOOP('',(#39834,#39835,#39836,#39837));
#17075=EDGE_LOOP('',(#39838,#39839,#39840,#39841));
#17076=EDGE_LOOP('',(#39842,#39843,#39844,#39845));
#17077=EDGE_LOOP('',(#39846,#39847,#39848,#39849));
#17078=EDGE_LOOP('',(#39850,#39851,#39852,#39853));
#17079=EDGE_LOOP('',(#39854,#39855,#39856,#39857));
#17080=EDGE_LOOP('',(#39858,#39859,#39860,#39861));
#17081=EDGE_LOOP('',(#39862,#39863,#39864,#39865,#39866,#39867,#39868));
#17082=EDGE_LOOP('',(#39869,#39870,#39871,#39872));
#17083=EDGE_LOOP('',(#39873,#39874,#39875,#39876));
#17084=EDGE_LOOP('',(#39877,#39878,#39879,#39880));
#17085=EDGE_LOOP('',(#39881,#39882,#39883,#39884));
#17086=EDGE_LOOP('',(#39885,#39886,#39887,#39888));
#17087=EDGE_LOOP('',(#39889,#39890,#39891,#39892));
#17088=EDGE_LOOP('',(#39893,#39894,#39895,#39896));
#17089=EDGE_LOOP('',(#39897,#39898,#39899,#39900));
#17090=EDGE_LOOP('',(#39901,#39902,#39903,#39904));
#17091=EDGE_LOOP('',(#39905,#39906,#39907,#39908));
#17092=EDGE_LOOP('',(#39909,#39910,#39911,#39912));
#17093=EDGE_LOOP('',(#39913,#39914,#39915,#39916));
#17094=EDGE_LOOP('',(#39917,#39918,#39919,#39920));
#17095=EDGE_LOOP('',(#39921,#39922,#39923,#39924));
#17096=EDGE_LOOP('',(#39925,#39926,#39927,#39928,#39929,#39930,#39931,#39932,
#39933,#39934,#39935,#39936,#39937,#39938,#39939,#39940,#39941,#39942,#39943,
#39944,#39945,#39946,#39947,#39948,#39949,#39950,#39951,#39952,#39953,#39954,
#39955,#39956));
#17097=EDGE_LOOP('',(#39957,#39958,#39959,#39960));
#17098=EDGE_LOOP('',(#39961,#39962,#39963,#39964));
#17099=EDGE_LOOP('',(#39965,#39966,#39967,#39968));
#17100=EDGE_LOOP('',(#39969,#39970,#39971,#39972));
#17101=EDGE_LOOP('',(#39973,#39974,#39975,#39976));
#17102=EDGE_LOOP('',(#39977,#39978,#39979,#39980));
#17103=EDGE_LOOP('',(#39981,#39982,#39983,#39984));
#17104=EDGE_LOOP('',(#39985,#39986,#39987,#39988));
#17105=EDGE_LOOP('',(#39989,#39990,#39991,#39992));
#17106=EDGE_LOOP('',(#39993,#39994,#39995,#39996));
#17107=EDGE_LOOP('',(#39997,#39998,#39999,#40000));
#17108=EDGE_LOOP('',(#40001,#40002,#40003,#40004));
#17109=EDGE_LOOP('',(#40005,#40006,#40007,#40008));
#17110=EDGE_LOOP('',(#40009,#40010,#40011,#40012,#40013,#40014,#40015));
#17111=EDGE_LOOP('',(#40016,#40017,#40018,#40019));
#17112=EDGE_LOOP('',(#40020,#40021,#40022,#40023));
#17113=EDGE_LOOP('',(#40024,#40025,#40026,#40027));
#17114=EDGE_LOOP('',(#40028,#40029,#40030,#40031));
#17115=EDGE_LOOP('',(#40032,#40033,#40034,#40035));
#17116=EDGE_LOOP('',(#40036,#40037,#40038,#40039));
#17117=EDGE_LOOP('',(#40040,#40041,#40042,#40043));
#17118=EDGE_LOOP('',(#40044,#40045,#40046,#40047));
#17119=EDGE_LOOP('',(#40048,#40049,#40050,#40051));
#17120=EDGE_LOOP('',(#40052,#40053,#40054,#40055));
#17121=EDGE_LOOP('',(#40056,#40057,#40058,#40059));
#17122=EDGE_LOOP('',(#40060,#40061,#40062,#40063));
#17123=EDGE_LOOP('',(#40064,#40065,#40066,#40067));
#17124=EDGE_LOOP('',(#40068,#40069,#40070,#40071));
#17125=EDGE_LOOP('',(#40072,#40073,#40074,#40075,#40076,#40077,#40078,#40079,
#40080,#40081,#40082,#40083,#40084,#40085,#40086,#40087,#40088,#40089,#40090,
#40091,#40092,#40093,#40094,#40095,#40096,#40097,#40098,#40099,#40100,#40101,
#40102,#40103));
#17126=EDGE_LOOP('',(#40104,#40105,#40106,#40107));
#17127=EDGE_LOOP('',(#40108,#40109,#40110,#40111));
#17128=EDGE_LOOP('',(#40112,#40113,#40114,#40115));
#17129=EDGE_LOOP('',(#40116,#40117,#40118,#40119));
#17130=EDGE_LOOP('',(#40120,#40121,#40122,#40123));
#17131=EDGE_LOOP('',(#40124,#40125,#40126,#40127));
#17132=EDGE_LOOP('',(#40128,#40129,#40130,#40131));
#17133=EDGE_LOOP('',(#40132,#40133,#40134,#40135));
#17134=EDGE_LOOP('',(#40136,#40137,#40138,#40139));
#17135=EDGE_LOOP('',(#40140,#40141,#40142,#40143));
#17136=EDGE_LOOP('',(#40144,#40145,#40146,#40147));
#17137=EDGE_LOOP('',(#40148,#40149,#40150,#40151));
#17138=EDGE_LOOP('',(#40152,#40153,#40154,#40155));
#17139=EDGE_LOOP('',(#40156,#40157,#40158,#40159,#40160,#40161,#40162));
#17140=EDGE_LOOP('',(#40163,#40164,#40165,#40166));
#17141=EDGE_LOOP('',(#40167,#40168,#40169,#40170));
#17142=EDGE_LOOP('',(#40171,#40172,#40173,#40174));
#17143=EDGE_LOOP('',(#40175,#40176,#40177,#40178));
#17144=EDGE_LOOP('',(#40179,#40180,#40181,#40182));
#17145=EDGE_LOOP('',(#40183,#40184,#40185,#40186));
#17146=EDGE_LOOP('',(#40187,#40188,#40189,#40190));
#17147=EDGE_LOOP('',(#40191,#40192,#40193,#40194));
#17148=EDGE_LOOP('',(#40195,#40196,#40197,#40198));
#17149=EDGE_LOOP('',(#40199,#40200,#40201,#40202));
#17150=EDGE_LOOP('',(#40203,#40204,#40205,#40206));
#17151=EDGE_LOOP('',(#40207,#40208,#40209,#40210));
#17152=EDGE_LOOP('',(#40211,#40212,#40213,#40214));
#17153=EDGE_LOOP('',(#40215,#40216,#40217,#40218));
#17154=EDGE_LOOP('',(#40219,#40220,#40221,#40222,#40223,#40224,#40225,#40226,
#40227,#40228,#40229,#40230,#40231,#40232,#40233,#40234,#40235,#40236,#40237,
#40238,#40239,#40240,#40241,#40242,#40243,#40244,#40245,#40246,#40247,#40248,
#40249,#40250));
#17155=EDGE_LOOP('',(#40251,#40252,#40253,#40254));
#17156=EDGE_LOOP('',(#40255,#40256,#40257,#40258));
#17157=EDGE_LOOP('',(#40259,#40260,#40261,#40262));
#17158=EDGE_LOOP('',(#40263,#40264,#40265,#40266));
#17159=EDGE_LOOP('',(#40267,#40268,#40269,#40270));
#17160=EDGE_LOOP('',(#40271,#40272,#40273,#40274));
#17161=EDGE_LOOP('',(#40275,#40276,#40277,#40278));
#17162=EDGE_LOOP('',(#40279,#40280,#40281,#40282));
#17163=EDGE_LOOP('',(#40283,#40284,#40285,#40286));
#17164=EDGE_LOOP('',(#40287,#40288,#40289,#40290));
#17165=EDGE_LOOP('',(#40291,#40292,#40293,#40294));
#17166=EDGE_LOOP('',(#40295,#40296,#40297,#40298));
#17167=EDGE_LOOP('',(#40299,#40300,#40301,#40302));
#17168=EDGE_LOOP('',(#40303,#40304,#40305,#40306,#40307,#40308,#40309));
#17169=EDGE_LOOP('',(#40310,#40311,#40312,#40313));
#17170=EDGE_LOOP('',(#40314,#40315,#40316,#40317));
#17171=EDGE_LOOP('',(#40318,#40319,#40320,#40321));
#17172=EDGE_LOOP('',(#40322,#40323,#40324,#40325));
#17173=EDGE_LOOP('',(#40326,#40327,#40328,#40329));
#17174=EDGE_LOOP('',(#40330,#40331,#40332,#40333));
#17175=EDGE_LOOP('',(#40334,#40335,#40336,#40337));
#17176=EDGE_LOOP('',(#40338,#40339,#40340,#40341));
#17177=EDGE_LOOP('',(#40342,#40343,#40344,#40345));
#17178=EDGE_LOOP('',(#40346,#40347,#40348,#40349));
#17179=EDGE_LOOP('',(#40350,#40351,#40352,#40353));
#17180=EDGE_LOOP('',(#40354,#40355,#40356,#40357));
#17181=EDGE_LOOP('',(#40358,#40359,#40360,#40361));
#17182=EDGE_LOOP('',(#40362,#40363,#40364,#40365));
#17183=EDGE_LOOP('',(#40366,#40367,#40368,#40369,#40370,#40371,#40372,#40373,
#40374,#40375,#40376,#40377,#40378,#40379,#40380,#40381,#40382,#40383,#40384,
#40385,#40386,#40387,#40388,#40389,#40390,#40391,#40392,#40393,#40394,#40395,
#40396,#40397));
#17184=EDGE_LOOP('',(#40398,#40399,#40400,#40401));
#17185=EDGE_LOOP('',(#40402,#40403,#40404,#40405));
#17186=EDGE_LOOP('',(#40406,#40407,#40408,#40409));
#17187=EDGE_LOOP('',(#40410,#40411,#40412,#40413));
#17188=EDGE_LOOP('',(#40414,#40415,#40416,#40417));
#17189=EDGE_LOOP('',(#40418,#40419,#40420,#40421));
#17190=EDGE_LOOP('',(#40422,#40423,#40424,#40425));
#17191=EDGE_LOOP('',(#40426,#40427,#40428,#40429));
#17192=EDGE_LOOP('',(#40430,#40431,#40432,#40433));
#17193=EDGE_LOOP('',(#40434,#40435,#40436,#40437));
#17194=EDGE_LOOP('',(#40438,#40439,#40440,#40441));
#17195=EDGE_LOOP('',(#40442,#40443,#40444,#40445));
#17196=EDGE_LOOP('',(#40446,#40447,#40448,#40449));
#17197=EDGE_LOOP('',(#40450,#40451,#40452,#40453,#40454,#40455,#40456));
#17198=EDGE_LOOP('',(#40457,#40458,#40459,#40460));
#17199=EDGE_LOOP('',(#40461,#40462,#40463,#40464));
#17200=EDGE_LOOP('',(#40465,#40466,#40467,#40468));
#17201=EDGE_LOOP('',(#40469,#40470,#40471,#40472));
#17202=EDGE_LOOP('',(#40473,#40474,#40475,#40476));
#17203=EDGE_LOOP('',(#40477,#40478,#40479,#40480));
#17204=EDGE_LOOP('',(#40481,#40482,#40483,#40484));
#17205=EDGE_LOOP('',(#40485,#40486,#40487,#40488));
#17206=EDGE_LOOP('',(#40489,#40490,#40491,#40492));
#17207=EDGE_LOOP('',(#40493,#40494,#40495,#40496));
#17208=EDGE_LOOP('',(#40497,#40498,#40499,#40500));
#17209=EDGE_LOOP('',(#40501,#40502,#40503,#40504));
#17210=EDGE_LOOP('',(#40505,#40506,#40507,#40508));
#17211=EDGE_LOOP('',(#40509,#40510,#40511,#40512));
#17212=EDGE_LOOP('',(#40513,#40514,#40515,#40516,#40517,#40518,#40519,#40520,
#40521,#40522,#40523,#40524,#40525,#40526,#40527,#40528,#40529,#40530,#40531,
#40532,#40533,#40534,#40535,#40536,#40537,#40538,#40539,#40540,#40541,#40542,
#40543,#40544));
#17213=EDGE_LOOP('',(#40545,#40546,#40547,#40548));
#17214=EDGE_LOOP('',(#40549,#40550,#40551,#40552));
#17215=EDGE_LOOP('',(#40553,#40554,#40555,#40556));
#17216=EDGE_LOOP('',(#40557,#40558,#40559,#40560));
#17217=EDGE_LOOP('',(#40561,#40562,#40563,#40564));
#17218=EDGE_LOOP('',(#40565,#40566,#40567,#40568));
#17219=EDGE_LOOP('',(#40569,#40570,#40571,#40572));
#17220=EDGE_LOOP('',(#40573,#40574,#40575,#40576));
#17221=EDGE_LOOP('',(#40577,#40578,#40579,#40580));
#17222=EDGE_LOOP('',(#40581,#40582,#40583,#40584));
#17223=EDGE_LOOP('',(#40585,#40586,#40587,#40588));
#17224=EDGE_LOOP('',(#40589,#40590,#40591,#40592));
#17225=EDGE_LOOP('',(#40593,#40594,#40595,#40596));
#17226=EDGE_LOOP('',(#40597,#40598,#40599,#40600,#40601,#40602,#40603));
#17227=EDGE_LOOP('',(#40604,#40605,#40606,#40607));
#17228=EDGE_LOOP('',(#40608,#40609,#40610,#40611));
#17229=EDGE_LOOP('',(#40612,#40613,#40614,#40615));
#17230=EDGE_LOOP('',(#40616,#40617,#40618,#40619));
#17231=EDGE_LOOP('',(#40620,#40621,#40622,#40623));
#17232=EDGE_LOOP('',(#40624,#40625,#40626,#40627));
#17233=EDGE_LOOP('',(#40628,#40629,#40630,#40631));
#17234=EDGE_LOOP('',(#40632,#40633,#40634,#40635));
#17235=EDGE_LOOP('',(#40636,#40637,#40638,#40639));
#17236=EDGE_LOOP('',(#40640,#40641,#40642,#40643));
#17237=EDGE_LOOP('',(#40644,#40645,#40646,#40647));
#17238=EDGE_LOOP('',(#40648,#40649,#40650,#40651));
#17239=EDGE_LOOP('',(#40652,#40653,#40654,#40655));
#17240=EDGE_LOOP('',(#40656,#40657,#40658,#40659));
#17241=EDGE_LOOP('',(#40660,#40661,#40662,#40663,#40664,#40665,#40666,#40667,
#40668,#40669,#40670,#40671,#40672,#40673,#40674,#40675,#40676,#40677,#40678,
#40679,#40680,#40681,#40682,#40683,#40684,#40685,#40686,#40687,#40688,#40689,
#40690,#40691));
#17242=EDGE_LOOP('',(#40692,#40693,#40694,#40695));
#17243=EDGE_LOOP('',(#40696,#40697,#40698,#40699));
#17244=EDGE_LOOP('',(#40700,#40701,#40702,#40703));
#17245=EDGE_LOOP('',(#40704,#40705,#40706,#40707));
#17246=EDGE_LOOP('',(#40708,#40709,#40710,#40711));
#17247=EDGE_LOOP('',(#40712,#40713,#40714,#40715));
#17248=EDGE_LOOP('',(#40716,#40717,#40718,#40719));
#17249=EDGE_LOOP('',(#40720,#40721,#40722,#40723));
#17250=EDGE_LOOP('',(#40724,#40725,#40726,#40727));
#17251=EDGE_LOOP('',(#40728,#40729,#40730,#40731));
#17252=EDGE_LOOP('',(#40732,#40733,#40734,#40735));
#17253=EDGE_LOOP('',(#40736,#40737,#40738,#40739));
#17254=EDGE_LOOP('',(#40740,#40741,#40742,#40743));
#17255=EDGE_LOOP('',(#40744,#40745,#40746,#40747,#40748,#40749,#40750));
#17256=EDGE_LOOP('',(#40751,#40752,#40753,#40754));
#17257=EDGE_LOOP('',(#40755,#40756,#40757,#40758));
#17258=EDGE_LOOP('',(#40759,#40760,#40761,#40762));
#17259=EDGE_LOOP('',(#40763,#40764,#40765,#40766));
#17260=EDGE_LOOP('',(#40767,#40768,#40769,#40770));
#17261=EDGE_LOOP('',(#40771,#40772,#40773,#40774));
#17262=EDGE_LOOP('',(#40775,#40776,#40777,#40778));
#17263=EDGE_LOOP('',(#40779,#40780,#40781,#40782));
#17264=EDGE_LOOP('',(#40783,#40784,#40785,#40786));
#17265=EDGE_LOOP('',(#40787,#40788,#40789,#40790));
#17266=EDGE_LOOP('',(#40791,#40792,#40793,#40794));
#17267=EDGE_LOOP('',(#40795,#40796,#40797,#40798));
#17268=EDGE_LOOP('',(#40799,#40800,#40801,#40802));
#17269=EDGE_LOOP('',(#40803,#40804,#40805,#40806));
#17270=EDGE_LOOP('',(#40807,#40808,#40809,#40810,#40811,#40812,#40813,#40814,
#40815,#40816,#40817,#40818,#40819,#40820,#40821,#40822,#40823,#40824,#40825,
#40826,#40827,#40828,#40829,#40830,#40831,#40832,#40833,#40834,#40835,#40836,
#40837,#40838));
#17271=EDGE_LOOP('',(#40839,#40840,#40841,#40842));
#17272=EDGE_LOOP('',(#40843,#40844,#40845,#40846));
#17273=EDGE_LOOP('',(#40847,#40848,#40849,#40850));
#17274=EDGE_LOOP('',(#40851,#40852,#40853,#40854));
#17275=EDGE_LOOP('',(#40855,#40856,#40857,#40858));
#17276=EDGE_LOOP('',(#40859,#40860,#40861,#40862));
#17277=EDGE_LOOP('',(#40863,#40864,#40865,#40866));
#17278=EDGE_LOOP('',(#40867,#40868,#40869,#40870));
#17279=EDGE_LOOP('',(#40871,#40872,#40873,#40874));
#17280=EDGE_LOOP('',(#40875,#40876,#40877,#40878));
#17281=EDGE_LOOP('',(#40879,#40880,#40881,#40882));
#17282=EDGE_LOOP('',(#40883,#40884,#40885,#40886));
#17283=EDGE_LOOP('',(#40887,#40888,#40889,#40890));
#17284=EDGE_LOOP('',(#40891,#40892,#40893,#40894,#40895,#40896,#40897));
#17285=EDGE_LOOP('',(#40898,#40899,#40900,#40901));
#17286=EDGE_LOOP('',(#40902,#40903,#40904,#40905));
#17287=EDGE_LOOP('',(#40906,#40907,#40908,#40909));
#17288=EDGE_LOOP('',(#40910,#40911,#40912,#40913));
#17289=EDGE_LOOP('',(#40914,#40915,#40916,#40917));
#17290=EDGE_LOOP('',(#40918,#40919,#40920,#40921));
#17291=EDGE_LOOP('',(#40922,#40923,#40924,#40925));
#17292=EDGE_LOOP('',(#40926,#40927,#40928,#40929));
#17293=EDGE_LOOP('',(#40930,#40931,#40932,#40933));
#17294=EDGE_LOOP('',(#40934,#40935,#40936,#40937));
#17295=EDGE_LOOP('',(#40938,#40939,#40940,#40941));
#17296=EDGE_LOOP('',(#40942,#40943,#40944,#40945));
#17297=EDGE_LOOP('',(#40946,#40947,#40948,#40949));
#17298=EDGE_LOOP('',(#40950,#40951,#40952,#40953,#40954,#40955,#40956));
#17299=EDGE_LOOP('',(#40957,#40958,#40959,#40960,#40961,#40962,#40963,#40964,
#40965,#40966,#40967,#40968,#40969,#40970,#40971,#40972,#40973,#40974,#40975,
#40976,#40977,#40978,#40979,#40980,#40981,#40982,#40983,#40984,#40985,#40986,
#40987,#40988,#40989,#40990,#40991,#40992,#40993,#40994,#40995,#40996,#40997,
#40998,#40999,#41000,#41001,#41002,#41003,#41004,#41005,#41006,#41007,#41008,
#41009,#41010,#41011,#41012,#41013,#41014,#41015,#41016,#41017,#41018,#41019,
#41020,#41021,#41022,#41023,#41024,#41025,#41026,#41027,#41028,#41029,#41030,
#41031,#41032,#41033,#41034,#41035,#41036,#41037,#41038,#41039,#41040,#41041,
#41042,#41043,#41044,#41045,#41046,#41047,#41048,#41049,#41050,#41051,#41052,
#41053,#41054,#41055,#41056,#41057,#41058,#41059,#41060,#41061,#41062,#41063,
#41064,#41065,#41066,#41067,#41068,#41069,#41070,#41071,#41072,#41073,#41074,
#41075,#41076,#41077,#41078,#41079,#41080,#41081,#41082,#41083,#41084,#41085,
#41086,#41087,#41088,#41089,#41090,#41091,#41092,#41093,#41094,#41095,#41096,
#41097,#41098,#41099,#41100,#41101,#41102,#41103,#41104));
#17300=EDGE_LOOP('',(#41105,#41106,#41107,#41108,#41109));
#17301=EDGE_LOOP('',(#41110,#41111,#41112,#41113,#41114,#41115));
#17302=EDGE_LOOP('',(#41116));
#17303=EDGE_LOOP('',(#41117));
#17304=EDGE_LOOP('',(#41118,#41119,#41120,#41121,#41122,#41123));
#17305=EDGE_LOOP('',(#41124,#41125,#41126,#41127,#41128));
#17306=EDGE_LOOP('',(#41129,#41130,#41131,#41132,#41133));
#17307=EDGE_LOOP('',(#41134,#41135,#41136,#41137,#41138,#41139));
#17308=EDGE_LOOP('',(#41140));
#17309=EDGE_LOOP('',(#41141));
#17310=EDGE_LOOP('',(#41142,#41143,#41144,#41145,#41146));
#17311=EDGE_LOOP('',(#41147));
#17312=EDGE_LOOP('',(#41148));
#17313=EDGE_LOOP('',(#41149,#41150,#41151,#41152,#41153,#41154,#41155,#41156,
#41157,#41158,#41159,#41160,#41161,#41162,#41163,#41164,#41165,#41166,#41167,
#41168,#41169,#41170,#41171,#41172,#41173,#41174,#41175,#41176,#41177,#41178,
#41179,#41180));
#17314=EDGE_LOOP('',(#41181));
#17315=EDGE_LOOP('',(#41182));
#17316=EDGE_LOOP('',(#41183,#41184,#41185,#41186));
#17317=EDGE_LOOP('',(#41187,#41188,#41189,#41190));
#17318=EDGE_LOOP('',(#41191,#41192,#41193,#41194));
#17319=EDGE_LOOP('',(#41195,#41196,#41197,#41198));
#17320=EDGE_LOOP('',(#41199,#41200,#41201,#41202));
#17321=EDGE_LOOP('',(#41203,#41204,#41205,#41206,#41207,#41208));
#17322=EDGE_LOOP('',(#41209,#41210,#41211,#41212,#41213,#41214));
#17323=EDGE_LOOP('',(#41215,#41216,#41217,#41218));
#17324=EDGE_LOOP('',(#41219,#41220,#41221,#41222));
#17325=EDGE_LOOP('',(#41223,#41224,#41225,#41226,#41227,#41228,#41229,#41230,
#41231,#41232,#41233,#41234,#41235,#41236,#41237,#41238,#41239,#41240,#41241,
#41242,#41243,#41244,#41245,#41246,#41247,#41248,#41249,#41250,#41251,#41252,
#41253,#41254,#41255,#41256,#41257,#41258,#41259,#41260,#41261,#41262,#41263,
#41264,#41265,#41266,#41267,#41268,#41269,#41270));
#17326=EDGE_LOOP('',(#41271,#41272,#41273,#41274,#41275,#41276,#41277,#41278,
#41279,#41280,#41281,#41282));
#17327=EDGE_LOOP('',(#41283));
#17328=EDGE_LOOP('',(#41284,#41285,#41286,#41287,#41288,#41289,#41290,#41291,
#41292,#41293,#41294,#41295,#41296,#41297,#41298,#41299,#41300,#41301,#41302,
#41303,#41304,#41305,#41306,#41307,#41308,#41309,#41310,#41311,#41312,#41313,
#41314,#41315,#41316,#41317,#41318,#41319,#41320,#41321,#41322,#41323,#41324,
#41325,#41326,#41327,#41328,#41329,#41330,#41331));
#17329=EDGE_LOOP('',(#41332,#41333,#41334,#41335,#41336,#41337,#41338,#41339,
#41340,#41341,#41342,#41343,#41344,#41345,#41346,#41347,#41348,#41349,#41350,
#41351,#41352,#41353,#41354,#41355,#41356,#41357,#41358,#41359,#41360,#41361,
#41362,#41363,#41364,#41365,#41366,#41367,#41368,#41369,#41370,#41371,#41372,
#41373,#41374,#41375,#41376,#41377,#41378,#41379));
#17330=EDGE_LOOP('',(#41380,#41381,#41382,#41383,#41384,#41385));
#17331=EDGE_LOOP('',(#41386,#41387,#41388,#41389,#41390,#41391));
#17332=EDGE_LOOP('',(#41392,#41393,#41394,#41395));
#17333=EDGE_LOOP('',(#41396,#41397,#41398,#41399,#41400,#41401,#41402,#41403,
#41404,#41405,#41406,#41407,#41408,#41409,#41410,#41411,#41412,#41413,#41414,
#41415,#41416,#41417,#41418,#41419,#41420,#41421,#41422,#41423,#41424,#41425,
#41426,#41427,#41428,#41429,#41430,#41431,#41432,#41433,#41434,#41435,#41436,
#41437,#41438,#41439,#41440,#41441,#41442,#41443));
#17334=EDGE_LOOP('',(#41444,#41445,#41446,#41447,#41448,#41449,#41450,#41451,
#41452,#41453,#41454,#41455,#41456,#41457,#41458,#41459,#41460,#41461,#41462,
#41463,#41464,#41465,#41466,#41467,#41468,#41469,#41470,#41471,#41472,#41473,
#41474,#41475,#41476,#41477,#41478,#41479,#41480,#41481,#41482,#41483,#41484,
#41485,#41486,#41487,#41488,#41489,#41490,#41491));
#17335=EDGE_LOOP('',(#41492,#41493,#41494,#41495));
#17336=EDGE_LOOP('',(#41496,#41497,#41498,#41499,#41500,#41501,#41502,#41503,
#41504,#41505,#41506,#41507,#41508,#41509,#41510,#41511,#41512,#41513,#41514,
#41515,#41516,#41517,#41518,#41519,#41520,#41521,#41522,#41523,#41524,#41525,
#41526,#41527,#41528,#41529,#41530,#41531,#41532,#41533,#41534,#41535,#41536,
#41537,#41538,#41539,#41540,#41541,#41542,#41543));
#17337=EDGE_LOOP('',(#41544,#41545,#41546,#41547,#41548,#41549));
#17338=EDGE_LOOP('',(#41550,#41551,#41552,#41553,#41554,#41555));
#17339=EDGE_LOOP('',(#41556,#41557,#41558,#41559));
#17340=EDGE_LOOP('',(#41560,#41561,#41562,#41563));
#17341=EDGE_LOOP('',(#41564,#41565,#41566,#41567));
#17342=EDGE_LOOP('',(#41568,#41569,#41570,#41571));
#17343=EDGE_LOOP('',(#41572,#41573,#41574,#41575));
#17344=EDGE_LOOP('',(#41576,#41577,#41578,#41579));
#17345=EDGE_LOOP('',(#41580,#41581,#41582,#41583));
#17346=EDGE_LOOP('',(#41584,#41585,#41586,#41587));
#17347=EDGE_LOOP('',(#41588,#41589,#41590,#41591));
#17348=EDGE_LOOP('',(#41592,#41593,#41594,#41595));
#17349=EDGE_LOOP('',(#41596,#41597,#41598,#41599));
#17350=EDGE_LOOP('',(#41600,#41601,#41602,#41603));
#17351=EDGE_LOOP('',(#41604,#41605,#41606,#41607));
#17352=EDGE_LOOP('',(#41608,#41609,#41610,#41611));
#17353=EDGE_LOOP('',(#41612,#41613,#41614,#41615));
#17354=EDGE_LOOP('',(#41616,#41617,#41618,#41619));
#17355=EDGE_LOOP('',(#41620,#41621,#41622,#41623));
#17356=EDGE_LOOP('',(#41624,#41625,#41626,#41627));
#17357=EDGE_LOOP('',(#41628,#41629,#41630,#41631));
#17358=EDGE_LOOP('',(#41632,#41633,#41634,#41635));
#17359=EDGE_LOOP('',(#41636,#41637,#41638,#41639));
#17360=EDGE_LOOP('',(#41640,#41641,#41642,#41643));
#17361=EDGE_LOOP('',(#41644,#41645,#41646,#41647));
#17362=EDGE_LOOP('',(#41648,#41649,#41650,#41651));
#17363=EDGE_LOOP('',(#41652,#41653,#41654,#41655));
#17364=EDGE_LOOP('',(#41656,#41657,#41658,#41659));
#17365=EDGE_LOOP('',(#41660,#41661,#41662,#41663));
#17366=EDGE_LOOP('',(#41664,#41665,#41666,#41667));
#17367=EDGE_LOOP('',(#41668,#41669,#41670,#41671));
#17368=EDGE_LOOP('',(#41672,#41673,#41674,#41675));
#17369=EDGE_LOOP('',(#41676,#41677,#41678,#41679));
#17370=EDGE_LOOP('',(#41680,#41681,#41682,#41683));
#17371=EDGE_LOOP('',(#41684,#41685,#41686,#41687));
#17372=EDGE_LOOP('',(#41688,#41689,#41690,#41691));
#17373=EDGE_LOOP('',(#41692,#41693,#41694,#41695));
#17374=EDGE_LOOP('',(#41696,#41697,#41698,#41699,#41700,#41701,#41702,#41703,
#41704,#41705));
#17375=EDGE_LOOP('',(#41706,#41707,#41708,#41709));
#17376=EDGE_LOOP('',(#41710,#41711,#41712,#41713,#41714,#41715,#41716,#41717,
#41718,#41719));
#17377=EDGE_LOOP('',(#41720,#41721,#41722,#41723));
#17378=EDGE_LOOP('',(#41724,#41725,#41726,#41727,#41728,#41729,#41730,#41731,
#41732,#41733));
#17379=EDGE_LOOP('',(#41734,#41735,#41736,#41737));
#17380=EDGE_LOOP('',(#41738,#41739,#41740,#41741,#41742,#41743,#41744,#41745,
#41746,#41747));
#17381=EDGE_LOOP('',(#41748,#41749,#41750,#41751));
#17382=EDGE_LOOP('',(#41752,#41753,#41754,#41755,#41756,#41757,#41758,#41759,
#41760,#41761));
#17383=EDGE_LOOP('',(#41762,#41763,#41764,#41765));
#17384=EDGE_LOOP('',(#41766,#41767,#41768,#41769,#41770,#41771,#41772,#41773,
#41774,#41775));
#17385=EDGE_LOOP('',(#41776,#41777,#41778,#41779));
#17386=EDGE_LOOP('',(#41780,#41781,#41782,#41783,#41784,#41785,#41786,#41787,
#41788,#41789));
#17387=EDGE_LOOP('',(#41790,#41791,#41792,#41793));
#17388=EDGE_LOOP('',(#41794,#41795,#41796,#41797,#41798,#41799,#41800,#41801,
#41802,#41803));
#17389=EDGE_LOOP('',(#41804,#41805,#41806,#41807));
#17390=EDGE_LOOP('',(#41808,#41809,#41810,#41811,#41812,#41813,#41814,#41815,
#41816,#41817));
#17391=EDGE_LOOP('',(#41818,#41819,#41820,#41821));
#17392=EDGE_LOOP('',(#41822,#41823,#41824,#41825,#41826,#41827,#41828,#41829,
#41830,#41831));
#17393=EDGE_LOOP('',(#41832,#41833,#41834,#41835));
#17394=EDGE_LOOP('',(#41836,#41837,#41838,#41839,#41840,#41841,#41842,#41843,
#41844,#41845));
#17395=EDGE_LOOP('',(#41846,#41847,#41848,#41849));
#17396=EDGE_LOOP('',(#41850,#41851,#41852,#41853,#41854,#41855,#41856,#41857,
#41858,#41859));
#17397=EDGE_LOOP('',(#41860,#41861,#41862,#41863));
#17398=EDGE_LOOP('',(#41864,#41865,#41866,#41867,#41868,#41869,#41870,#41871,
#41872,#41873));
#17399=EDGE_LOOP('',(#41874,#41875,#41876,#41877));
#17400=EDGE_LOOP('',(#41878,#41879,#41880,#41881,#41882,#41883,#41884,#41885,
#41886,#41887));
#17401=EDGE_LOOP('',(#41888,#41889,#41890,#41891));
#17402=EDGE_LOOP('',(#41892,#41893,#41894,#41895,#41896,#41897,#41898,#41899,
#41900,#41901));
#17403=EDGE_LOOP('',(#41902,#41903,#41904,#41905));
#17404=EDGE_LOOP('',(#41906,#41907,#41908,#41909,#41910,#41911,#41912,#41913,
#41914,#41915));
#17405=EDGE_LOOP('',(#41916,#41917,#41918,#41919));
#17406=EDGE_LOOP('',(#41920,#41921,#41922,#41923,#41924,#41925,#41926,#41927,
#41928,#41929));
#17407=EDGE_LOOP('',(#41930,#41931,#41932,#41933));
#17408=EDGE_LOOP('',(#41934,#41935,#41936,#41937,#41938,#41939,#41940,#41941,
#41942,#41943));
#17409=EDGE_LOOP('',(#41944,#41945,#41946,#41947));
#17410=EDGE_LOOP('',(#41948,#41949,#41950,#41951,#41952,#41953,#41954,#41955,
#41956,#41957));
#17411=EDGE_LOOP('',(#41958,#41959,#41960,#41961));
#17412=EDGE_LOOP('',(#41962,#41963,#41964,#41965,#41966,#41967,#41968,#41969,
#41970,#41971));
#17413=EDGE_LOOP('',(#41972,#41973,#41974,#41975));
#17414=EDGE_LOOP('',(#41976,#41977,#41978,#41979,#41980,#41981,#41982,#41983,
#41984,#41985));
#17415=EDGE_LOOP('',(#41986,#41987,#41988,#41989));
#17416=EDGE_LOOP('',(#41990,#41991,#41992,#41993,#41994,#41995,#41996,#41997,
#41998,#41999));
#17417=EDGE_LOOP('',(#42000,#42001,#42002,#42003));
#17418=EDGE_LOOP('',(#42004,#42005,#42006,#42007,#42008,#42009,#42010,#42011,
#42012,#42013));
#17419=EDGE_LOOP('',(#42014,#42015,#42016,#42017));
#17420=EDGE_LOOP('',(#42018,#42019,#42020,#42021,#42022,#42023,#42024,#42025,
#42026,#42027));
#17421=EDGE_LOOP('',(#42028,#42029,#42030,#42031));
#17422=EDGE_LOOP('',(#42032,#42033,#42034,#42035,#42036,#42037,#42038,#42039,
#42040,#42041));
#17423=EDGE_LOOP('',(#42042,#42043,#42044,#42045));
#17424=EDGE_LOOP('',(#42046,#42047,#42048,#42049,#42050,#42051,#42052,#42053,
#42054,#42055));
#17425=EDGE_LOOP('',(#42056,#42057,#42058,#42059));
#17426=EDGE_LOOP('',(#42060,#42061,#42062,#42063,#42064,#42065,#42066,#42067,
#42068,#42069));
#17427=EDGE_LOOP('',(#42070,#42071,#42072,#42073));
#17428=EDGE_LOOP('',(#42074,#42075,#42076,#42077,#42078,#42079,#42080,#42081,
#42082,#42083));
#17429=EDGE_LOOP('',(#42084,#42085,#42086,#42087));
#17430=EDGE_LOOP('',(#42088,#42089,#42090,#42091,#42092,#42093,#42094,#42095,
#42096,#42097));
#17431=EDGE_LOOP('',(#42098,#42099,#42100,#42101));
#17432=EDGE_LOOP('',(#42102,#42103,#42104,#42105,#42106,#42107,#42108,#42109,
#42110,#42111));
#17433=EDGE_LOOP('',(#42112,#42113,#42114,#42115));
#17434=EDGE_LOOP('',(#42116,#42117,#42118,#42119,#42120,#42121,#42122,#42123,
#42124,#42125));
#17435=EDGE_LOOP('',(#42126,#42127,#42128,#42129));
#17436=EDGE_LOOP('',(#42130,#42131,#42132,#42133,#42134,#42135,#42136,#42137,
#42138,#42139));
#17437=EDGE_LOOP('',(#42140,#42141,#42142,#42143));
#17438=EDGE_LOOP('',(#42144,#42145,#42146,#42147,#42148,#42149,#42150,#42151,
#42152,#42153));
#17439=EDGE_LOOP('',(#42154,#42155,#42156,#42157));
#17440=EDGE_LOOP('',(#42158,#42159,#42160,#42161));
#17441=EDGE_LOOP('',(#42162,#42163,#42164,#42165));
#17442=EDGE_LOOP('',(#42166,#42167,#42168,#42169));
#17443=EDGE_LOOP('',(#42170,#42171,#42172,#42173));
#17444=EDGE_LOOP('',(#42174,#42175,#42176,#42177));
#17445=EDGE_LOOP('',(#42178,#42179,#42180,#42181));
#17446=EDGE_LOOP('',(#42182,#42183,#42184,#42185));
#17447=EDGE_LOOP('',(#42186,#42187,#42188,#42189));
#17448=EDGE_LOOP('',(#42190,#42191,#42192,#42193));
#17449=EDGE_LOOP('',(#42194,#42195,#42196,#42197));
#17450=EDGE_LOOP('',(#42198,#42199,#42200,#42201));
#17451=EDGE_LOOP('',(#42202,#42203,#42204,#42205));
#17452=EDGE_LOOP('',(#42206,#42207,#42208,#42209));
#17453=EDGE_LOOP('',(#42210,#42211,#42212,#42213));
#17454=EDGE_LOOP('',(#42214,#42215,#42216,#42217));
#17455=EDGE_LOOP('',(#42218,#42219,#42220,#42221));
#17456=EDGE_LOOP('',(#42222,#42223,#42224,#42225));
#17457=EDGE_LOOP('',(#42226,#42227,#42228,#42229));
#17458=EDGE_LOOP('',(#42230,#42231,#42232,#42233));
#17459=EDGE_LOOP('',(#42234,#42235,#42236,#42237));
#17460=EDGE_LOOP('',(#42238,#42239,#42240,#42241));
#17461=EDGE_LOOP('',(#42242,#42243,#42244,#42245));
#17462=EDGE_LOOP('',(#42246,#42247,#42248,#42249));
#17463=EDGE_LOOP('',(#42250,#42251,#42252,#42253));
#17464=EDGE_LOOP('',(#42254,#42255,#42256,#42257));
#17465=EDGE_LOOP('',(#42258,#42259,#42260,#42261));
#17466=EDGE_LOOP('',(#42262,#42263,#42264,#42265));
#17467=EDGE_LOOP('',(#42266,#42267,#42268,#42269));
#17468=EDGE_LOOP('',(#42270,#42271,#42272,#42273));
#17469=EDGE_LOOP('',(#42274,#42275,#42276,#42277));
#17470=EDGE_LOOP('',(#42278,#42279,#42280,#42281));
#17471=EDGE_LOOP('',(#42282,#42283,#42284,#42285));
#17472=EDGE_LOOP('',(#42286,#42287,#42288,#42289));
#17473=EDGE_LOOP('',(#42290,#42291,#42292,#42293,#42294,#42295,#42296,#42297,
#42298,#42299));
#17474=EDGE_LOOP('',(#42300,#42301,#42302,#42303,#42304,#42305,#42306,#42307,
#42308,#42309));
#17475=EDGE_LOOP('',(#42310,#42311,#42312,#42313,#42314,#42315,#42316,#42317,
#42318,#42319));
#17476=EDGE_LOOP('',(#42320,#42321,#42322,#42323,#42324,#42325,#42326,#42327,
#42328,#42329));
#17477=EDGE_LOOP('',(#42330,#42331,#42332,#42333,#42334,#42335,#42336,#42337,
#42338,#42339));
#17478=EDGE_LOOP('',(#42340,#42341,#42342,#42343,#42344,#42345,#42346,#42347,
#42348,#42349));
#17479=EDGE_LOOP('',(#42350,#42351,#42352,#42353,#42354,#42355,#42356,#42357,
#42358,#42359));
#17480=EDGE_LOOP('',(#42360,#42361,#42362,#42363,#42364,#42365,#42366,#42367,
#42368,#42369));
#17481=EDGE_LOOP('',(#42370,#42371,#42372,#42373,#42374,#42375,#42376,#42377,
#42378,#42379));
#17482=EDGE_LOOP('',(#42380,#42381,#42382,#42383,#42384,#42385,#42386,#42387,
#42388,#42389));
#17483=EDGE_LOOP('',(#42390,#42391,#42392,#42393,#42394,#42395,#42396,#42397,
#42398,#42399));
#17484=EDGE_LOOP('',(#42400,#42401,#42402,#42403,#42404,#42405,#42406,#42407,
#42408,#42409));
#17485=EDGE_LOOP('',(#42410,#42411,#42412,#42413,#42414,#42415,#42416,#42417,
#42418,#42419));
#17486=EDGE_LOOP('',(#42420,#42421,#42422,#42423,#42424,#42425,#42426,#42427,
#42428,#42429));
#17487=EDGE_LOOP('',(#42430,#42431,#42432,#42433,#42434,#42435,#42436,#42437,
#42438,#42439));
#17488=EDGE_LOOP('',(#42440,#42441,#42442,#42443,#42444,#42445,#42446,#42447,
#42448,#42449));
#17489=EDGE_LOOP('',(#42450,#42451,#42452,#42453,#42454,#42455,#42456,#42457,
#42458,#42459));
#17490=EDGE_LOOP('',(#42460,#42461,#42462,#42463,#42464,#42465,#42466,#42467,
#42468,#42469));
#17491=EDGE_LOOP('',(#42470,#42471,#42472,#42473,#42474,#42475,#42476,#42477,
#42478,#42479));
#17492=EDGE_LOOP('',(#42480,#42481,#42482,#42483,#42484,#42485,#42486,#42487,
#42488,#42489));
#17493=EDGE_LOOP('',(#42490,#42491,#42492,#42493,#42494,#42495,#42496,#42497,
#42498,#42499));
#17494=EDGE_LOOP('',(#42500,#42501,#42502,#42503,#42504,#42505,#42506,#42507,
#42508,#42509));
#17495=EDGE_LOOP('',(#42510,#42511,#42512,#42513,#42514,#42515,#42516,#42517,
#42518,#42519));
#17496=EDGE_LOOP('',(#42520,#42521,#42522,#42523,#42524,#42525,#42526,#42527,
#42528,#42529));
#17497=EDGE_LOOP('',(#42530,#42531,#42532,#42533,#42534,#42535,#42536,#42537,
#42538,#42539));
#17498=EDGE_LOOP('',(#42540,#42541,#42542,#42543,#42544,#42545,#42546,#42547,
#42548,#42549));
#17499=EDGE_LOOP('',(#42550,#42551,#42552,#42553,#42554,#42555,#42556,#42557,
#42558,#42559));
#17500=EDGE_LOOP('',(#42560,#42561,#42562,#42563,#42564,#42565,#42566,#42567,
#42568,#42569));
#17501=EDGE_LOOP('',(#42570,#42571,#42572,#42573,#42574,#42575,#42576,#42577,
#42578,#42579));
#17502=EDGE_LOOP('',(#42580,#42581,#42582,#42583,#42584,#42585,#42586,#42587,
#42588,#42589));
#17503=EDGE_LOOP('',(#42590,#42591,#42592,#42593,#42594,#42595,#42596,#42597,
#42598,#42599));
#17504=EDGE_LOOP('',(#42600,#42601,#42602,#42603,#42604,#42605,#42606,#42607,
#42608,#42609));
#17505=EDGE_LOOP('',(#42610,#42611,#42612,#42613,#42614,#42615,#42616,#42617,
#42618,#42619));
#17506=EDGE_LOOP('',(#42620,#42621,#42622,#42623));
#17507=EDGE_LOOP('',(#42624,#42625,#42626,#42627));
#17508=EDGE_LOOP('',(#42628,#42629,#42630,#42631));
#17509=EDGE_LOOP('',(#42632,#42633,#42634,#42635));
#17510=EDGE_LOOP('',(#42636,#42637,#42638,#42639));
#17511=EDGE_LOOP('',(#42640,#42641,#42642,#42643));
#17512=EDGE_LOOP('',(#42644,#42645,#42646,#42647));
#17513=EDGE_LOOP('',(#42648,#42649,#42650,#42651));
#17514=EDGE_LOOP('',(#42652,#42653,#42654,#42655));
#17515=EDGE_LOOP('',(#42656,#42657,#42658,#42659));
#17516=EDGE_LOOP('',(#42660,#42661,#42662,#42663));
#17517=EDGE_LOOP('',(#42664,#42665,#42666,#42667));
#17518=EDGE_LOOP('',(#42668,#42669,#42670,#42671));
#17519=EDGE_LOOP('',(#42672,#42673,#42674,#42675));
#17520=EDGE_LOOP('',(#42676,#42677,#42678,#42679));
#17521=EDGE_LOOP('',(#42680,#42681,#42682,#42683));
#17522=EDGE_LOOP('',(#42684,#42685,#42686,#42687));
#17523=EDGE_LOOP('',(#42688,#42689,#42690,#42691));
#17524=EDGE_LOOP('',(#42692,#42693,#42694,#42695));
#17525=EDGE_LOOP('',(#42696,#42697,#42698,#42699));
#17526=EDGE_LOOP('',(#42700,#42701,#42702,#42703));
#17527=EDGE_LOOP('',(#42704,#42705,#42706,#42707));
#17528=EDGE_LOOP('',(#42708,#42709,#42710,#42711));
#17529=EDGE_LOOP('',(#42712,#42713,#42714,#42715));
#17530=EDGE_LOOP('',(#42716,#42717,#42718,#42719));
#17531=EDGE_LOOP('',(#42720,#42721,#42722,#42723));
#17532=EDGE_LOOP('',(#42724,#42725,#42726,#42727));
#17533=EDGE_LOOP('',(#42728,#42729,#42730,#42731));
#17534=EDGE_LOOP('',(#42732,#42733,#42734,#42735));
#17535=EDGE_LOOP('',(#42736,#42737,#42738,#42739));
#17536=EDGE_LOOP('',(#42740,#42741,#42742,#42743));
#17537=EDGE_LOOP('',(#42744,#42745,#42746,#42747));
#17538=EDGE_LOOP('',(#42748,#42749,#42750,#42751));
#17539=EDGE_LOOP('',(#42752,#42753,#42754,#42755));
#17540=EDGE_LOOP('',(#42756,#42757,#42758,#42759));
#17541=EDGE_LOOP('',(#42760,#42761,#42762,#42763));
#17542=EDGE_LOOP('',(#42764,#42765,#42766,#42767));
#17543=EDGE_LOOP('',(#42768,#42769,#42770,#42771));
#17544=EDGE_LOOP('',(#42772,#42773,#42774,#42775));
#17545=EDGE_LOOP('',(#42776,#42777,#42778,#42779));
#17546=EDGE_LOOP('',(#42780,#42781,#42782,#42783));
#17547=EDGE_LOOP('',(#42784,#42785,#42786,#42787));
#17548=EDGE_LOOP('',(#42788,#42789,#42790,#42791));
#17549=EDGE_LOOP('',(#42792,#42793,#42794,#42795));
#17550=EDGE_LOOP('',(#42796,#42797,#42798,#42799));
#17551=EDGE_LOOP('',(#42800,#42801,#42802,#42803));
#17552=EDGE_LOOP('',(#42804,#42805,#42806,#42807));
#17553=EDGE_LOOP('',(#42808,#42809,#42810,#42811));
#17554=EDGE_LOOP('',(#42812,#42813,#42814,#42815));
#17555=EDGE_LOOP('',(#42816,#42817,#42818,#42819));
#17556=EDGE_LOOP('',(#42820,#42821,#42822,#42823));
#17557=EDGE_LOOP('',(#42824,#42825,#42826,#42827));
#17558=EDGE_LOOP('',(#42828,#42829,#42830,#42831));
#17559=EDGE_LOOP('',(#42832,#42833,#42834,#42835));
#17560=EDGE_LOOP('',(#42836,#42837,#42838,#42839));
#17561=EDGE_LOOP('',(#42840,#42841,#42842,#42843));
#17562=EDGE_LOOP('',(#42844,#42845,#42846,#42847));
#17563=EDGE_LOOP('',(#42848,#42849,#42850,#42851));
#17564=EDGE_LOOP('',(#42852,#42853,#42854,#42855));
#17565=EDGE_LOOP('',(#42856,#42857,#42858,#42859));
#17566=EDGE_LOOP('',(#42860,#42861,#42862,#42863));
#17567=EDGE_LOOP('',(#42864,#42865,#42866,#42867));
#17568=EDGE_LOOP('',(#42868,#42869,#42870,#42871));
#17569=EDGE_LOOP('',(#42872,#42873,#42874,#42875));
#17570=EDGE_LOOP('',(#42876,#42877,#42878,#42879));
#17571=EDGE_LOOP('',(#42880,#42881,#42882,#42883));
#17572=EDGE_LOOP('',(#42884,#42885,#42886,#42887));
#17573=EDGE_LOOP('',(#42888,#42889,#42890,#42891));
#17574=EDGE_LOOP('',(#42892,#42893,#42894,#42895));
#17575=EDGE_LOOP('',(#42896,#42897,#42898,#42899));
#17576=EDGE_LOOP('',(#42900,#42901,#42902,#42903));
#17577=EDGE_LOOP('',(#42904,#42905,#42906,#42907));
#17578=EDGE_LOOP('',(#42908,#42909,#42910,#42911));
#17579=EDGE_LOOP('',(#42912,#42913,#42914,#42915));
#17580=EDGE_LOOP('',(#42916,#42917,#42918,#42919));
#17581=EDGE_LOOP('',(#42920,#42921,#42922,#42923));
#17582=EDGE_LOOP('',(#42924,#42925,#42926,#42927));
#17583=EDGE_LOOP('',(#42928,#42929,#42930,#42931));
#17584=EDGE_LOOP('',(#42932,#42933,#42934,#42935));
#17585=EDGE_LOOP('',(#42936,#42937,#42938,#42939));
#17586=EDGE_LOOP('',(#42940,#42941,#42942,#42943));
#17587=EDGE_LOOP('',(#42944,#42945,#42946,#42947));
#17588=EDGE_LOOP('',(#42948,#42949,#42950,#42951));
#17589=EDGE_LOOP('',(#42952,#42953,#42954,#42955));
#17590=EDGE_LOOP('',(#42956,#42957,#42958,#42959));
#17591=EDGE_LOOP('',(#42960,#42961,#42962,#42963));
#17592=EDGE_LOOP('',(#42964,#42965,#42966,#42967));
#17593=EDGE_LOOP('',(#42968,#42969,#42970,#42971));
#17594=EDGE_LOOP('',(#42972,#42973,#42974,#42975));
#17595=EDGE_LOOP('',(#42976,#42977,#42978,#42979));
#17596=EDGE_LOOP('',(#42980,#42981,#42982,#42983));
#17597=EDGE_LOOP('',(#42984,#42985,#42986,#42987));
#17598=EDGE_LOOP('',(#42988,#42989,#42990,#42991));
#17599=EDGE_LOOP('',(#42992,#42993,#42994,#42995));
#17600=EDGE_LOOP('',(#42996,#42997,#42998,#42999));
#17601=EDGE_LOOP('',(#43000,#43001,#43002,#43003));
#17602=EDGE_LOOP('',(#43004,#43005,#43006,#43007));
#17603=EDGE_LOOP('',(#43008,#43009,#43010,#43011));
#17604=EDGE_LOOP('',(#43012,#43013,#43014,#43015));
#17605=EDGE_LOOP('',(#43016,#43017,#43018,#43019));
#17606=EDGE_LOOP('',(#43020,#43021,#43022,#43023));
#17607=EDGE_LOOP('',(#43024,#43025,#43026,#43027));
#17608=EDGE_LOOP('',(#43028,#43029,#43030,#43031));
#17609=EDGE_LOOP('',(#43032,#43033,#43034,#43035));
#17610=EDGE_LOOP('',(#43036,#43037,#43038,#43039));
#17611=EDGE_LOOP('',(#43040,#43041,#43042,#43043));
#17612=EDGE_LOOP('',(#43044,#43045,#43046,#43047));
#17613=EDGE_LOOP('',(#43048,#43049,#43050,#43051));
#17614=EDGE_LOOP('',(#43052,#43053,#43054,#43055));
#17615=EDGE_LOOP('',(#43056,#43057,#43058,#43059));
#17616=EDGE_LOOP('',(#43060,#43061,#43062,#43063));
#17617=EDGE_LOOP('',(#43064,#43065,#43066,#43067));
#17618=EDGE_LOOP('',(#43068,#43069,#43070,#43071));
#17619=EDGE_LOOP('',(#43072,#43073,#43074,#43075));
#17620=EDGE_LOOP('',(#43076,#43077,#43078,#43079));
#17621=EDGE_LOOP('',(#43080,#43081,#43082,#43083));
#17622=EDGE_LOOP('',(#43084,#43085,#43086,#43087));
#17623=EDGE_LOOP('',(#43088,#43089,#43090,#43091));
#17624=EDGE_LOOP('',(#43092,#43093,#43094,#43095));
#17625=EDGE_LOOP('',(#43096,#43097,#43098,#43099));
#17626=EDGE_LOOP('',(#43100,#43101,#43102,#43103));
#17627=EDGE_LOOP('',(#43104,#43105,#43106,#43107));
#17628=EDGE_LOOP('',(#43108,#43109,#43110,#43111));
#17629=EDGE_LOOP('',(#43112,#43113,#43114,#43115));
#17630=EDGE_LOOP('',(#43116,#43117,#43118,#43119));
#17631=EDGE_LOOP('',(#43120,#43121,#43122,#43123));
#17632=EDGE_LOOP('',(#43124,#43125,#43126,#43127));
#17633=EDGE_LOOP('',(#43128,#43129,#43130,#43131));
#17634=EDGE_LOOP('',(#43132,#43133,#43134,#43135));
#17635=EDGE_LOOP('',(#43136,#43137,#43138,#43139));
#17636=EDGE_LOOP('',(#43140,#43141,#43142,#43143));
#17637=EDGE_LOOP('',(#43144,#43145,#43146,#43147));
#17638=EDGE_LOOP('',(#43148,#43149,#43150,#43151));
#17639=EDGE_LOOP('',(#43152,#43153,#43154,#43155));
#17640=EDGE_LOOP('',(#43156,#43157,#43158,#43159));
#17641=EDGE_LOOP('',(#43160,#43161,#43162,#43163));
#17642=EDGE_LOOP('',(#43164,#43165,#43166,#43167));
#17643=EDGE_LOOP('',(#43168,#43169,#43170,#43171));
#17644=EDGE_LOOP('',(#43172,#43173,#43174,#43175));
#17645=EDGE_LOOP('',(#43176,#43177,#43178,#43179));
#17646=EDGE_LOOP('',(#43180,#43181,#43182,#43183));
#17647=EDGE_LOOP('',(#43184,#43185,#43186,#43187));
#17648=EDGE_LOOP('',(#43188,#43189,#43190,#43191));
#17649=EDGE_LOOP('',(#43192,#43193,#43194,#43195));
#17650=EDGE_LOOP('',(#43196,#43197,#43198,#43199));
#17651=EDGE_LOOP('',(#43200,#43201,#43202,#43203));
#17652=EDGE_LOOP('',(#43204,#43205,#43206,#43207));
#17653=EDGE_LOOP('',(#43208,#43209,#43210,#43211));
#17654=EDGE_LOOP('',(#43212,#43213,#43214,#43215));
#17655=EDGE_LOOP('',(#43216,#43217,#43218,#43219));
#17656=EDGE_LOOP('',(#43220,#43221,#43222,#43223));
#17657=EDGE_LOOP('',(#43224,#43225,#43226,#43227));
#17658=EDGE_LOOP('',(#43228,#43229,#43230,#43231));
#17659=EDGE_LOOP('',(#43232,#43233,#43234,#43235));
#17660=EDGE_LOOP('',(#43236,#43237,#43238,#43239));
#17661=EDGE_LOOP('',(#43240,#43241,#43242,#43243));
#17662=EDGE_LOOP('',(#43244,#43245,#43246,#43247));
#17663=EDGE_LOOP('',(#43248,#43249,#43250,#43251));
#17664=EDGE_LOOP('',(#43252,#43253,#43254,#43255));
#17665=EDGE_LOOP('',(#43256,#43257,#43258,#43259));
#17666=EDGE_LOOP('',(#43260,#43261,#43262,#43263));
#17667=EDGE_LOOP('',(#43264,#43265,#43266,#43267));
#17668=EDGE_LOOP('',(#43268,#43269,#43270,#43271));
#17669=EDGE_LOOP('',(#43272,#43273,#43274,#43275));
#17670=EDGE_LOOP('',(#43276,#43277,#43278,#43279));
#17671=EDGE_LOOP('',(#43280,#43281,#43282,#43283,#43284));
#17672=EDGE_LOOP('',(#43285));
#17673=EDGE_LOOP('',(#43286));
#17674=EDGE_LOOP('',(#43287,#43288,#43289,#43290,#43291));
#17675=EDGE_LOOP('',(#43292,#43293,#43294,#43295,#43296));
#17676=EDGE_LOOP('',(#43297));
#17677=EDGE_LOOP('',(#43298));
#17678=EDGE_LOOP('',(#43299,#43300,#43301,#43302,#43303));
#17679=EDGE_LOOP('',(#43304,#43305,#43306,#43307,#43308));
#17680=EDGE_LOOP('',(#43309,#43310,#43311,#43312,#43313));
#17681=EDGE_LOOP('',(#43314,#43315,#43316,#43317,#43318));
#17682=EDGE_LOOP('',(#43319,#43320,#43321,#43322,#43323));
#17683=EDGE_LOOP('',(#43324,#43325,#43326,#43327));
#17684=EDGE_LOOP('',(#43328,#43329,#43330,#43331));
#17685=EDGE_LOOP('',(#43332));
#17686=EDGE_LOOP('',(#43333));
#17687=EDGE_LOOP('',(#43334,#43335,#43336,#43337,#43338,#43339,#43340,#43341,
#43342,#43343,#43344,#43345));
#17688=EDGE_LOOP('',(#43346));
#17689=EDGE_LOOP('',(#43347));
#17690=EDGE_LOOP('',(#43348));
#17691=EDGE_LOOP('',(#43349,#43350,#43351,#43352));
#17692=EDGE_LOOP('',(#43353,#43354,#43355,#43356));
#17693=EDGE_LOOP('',(#43357));
#17694=EDGE_LOOP('',(#43358));
#17695=EDGE_LOOP('',(#43359));
#17696=EDGE_LOOP('',(#43360));
#17697=EDGE_LOOP('',(#43361));
#17698=EDGE_LOOP('',(#43362));
#17699=EDGE_LOOP('',(#43363));
#17700=EDGE_LOOP('',(#43364));
#17701=EDGE_LOOP('',(#43365,#43366,#43367,#43368));
#17702=EDGE_LOOP('',(#43369,#43370,#43371,#43372));
#17703=EDGE_LOOP('',(#43373,#43374,#43375,#43376));
#17704=EDGE_LOOP('',(#43377,#43378,#43379,#43380));
#17705=EDGE_LOOP('',(#43381,#43382,#43383,#43384));
#17706=EDGE_LOOP('',(#43385,#43386,#43387,#43388));
#17707=EDGE_LOOP('',(#43389,#43390,#43391,#43392));
#17708=EDGE_LOOP('',(#43393,#43394,#43395,#43396));
#17709=EDGE_LOOP('',(#43397));
#17710=EDGE_LOOP('',(#43398));
#17711=EDGE_LOOP('',(#43399,#43400,#43401,#43402));
#17712=EDGE_LOOP('',(#43403));
#17713=EDGE_LOOP('',(#43404));
#17714=EDGE_LOOP('',(#43405,#43406,#43407,#43408));
#17715=EDGE_LOOP('',(#43409));
#17716=EDGE_LOOP('',(#43410));
#17717=EDGE_LOOP('',(#43411,#43412,#43413,#43414));
#17718=EDGE_LOOP('',(#43415));
#17719=EDGE_LOOP('',(#43416));
#17720=EDGE_LOOP('',(#43417,#43418,#43419));
#17721=EDGE_LOOP('',(#43420,#43421,#43422,#43423));
#17722=EDGE_LOOP('',(#43424,#43425,#43426,#43427));
#17723=EDGE_LOOP('',(#43428,#43429,#43430,#43431,#43432));
#17724=EDGE_LOOP('',(#43433,#43434,#43435,#43436,#43437));
#17725=EDGE_LOOP('',(#43438));
#17726=EDGE_LOOP('',(#43439,#43440,#43441,#43442));
#17727=EDGE_LOOP('',(#43443,#43444,#43445,#43446));
#17728=EDGE_LOOP('',(#43447));
#17729=EDGE_LOOP('',(#43448));
#17730=EDGE_LOOP('',(#43449));
#17731=EDGE_LOOP('',(#43450));
#17732=EDGE_LOOP('',(#43451));
#17733=EDGE_LOOP('',(#43452));
#17734=EDGE_LOOP('',(#43453));
#17735=EDGE_LOOP('',(#43454));
#17736=EDGE_LOOP('',(#43455,#43456,#43457,#43458));
#17737=EDGE_LOOP('',(#43459,#43460,#43461,#43462));
#17738=EDGE_LOOP('',(#43463,#43464,#43465,#43466));
#17739=EDGE_LOOP('',(#43467));
#17740=EDGE_LOOP('',(#43468));
#17741=EDGE_LOOP('',(#43469,#43470,#43471,#43472));
#17742=EDGE_LOOP('',(#43473,#43474,#43475,#43476));
#17743=EDGE_LOOP('',(#43477));
#17744=EDGE_LOOP('',(#43478));
#17745=EDGE_LOOP('',(#43479,#43480,#43481,#43482));
#17746=EDGE_LOOP('',(#43483,#43484,#43485,#43486));
#17747=EDGE_LOOP('',(#43487,#43488,#43489,#43490));
#17748=EDGE_LOOP('',(#43491,#43492,#43493,#43494));
#17749=EDGE_LOOP('',(#43495,#43496,#43497,#43498));
#17750=EDGE_LOOP('',(#43499,#43500,#43501,#43502));
#17751=EDGE_LOOP('',(#43503,#43504,#43505,#43506));
#17752=EDGE_LOOP('',(#43507,#43508,#43509,#43510));
#17753=EDGE_LOOP('',(#43511,#43512,#43513,#43514));
#17754=EDGE_LOOP('',(#43515,#43516,#43517,#43518));
#17755=EDGE_LOOP('',(#43519,#43520,#43521,#43522));
#17756=EDGE_LOOP('',(#43523,#43524,#43525,#43526));
#17757=EDGE_LOOP('',(#43527,#43528,#43529,#43530,#43531,#43532,#43533,#43534,
#43535,#43536,#43537,#43538));
#17758=EDGE_LOOP('',(#43539,#43540,#43541,#43542));
#17759=EDGE_LOOP('',(#43543,#43544,#43545,#43546));
#17760=EDGE_LOOP('',(#43547,#43548,#43549,#43550));
#17761=EDGE_LOOP('',(#43551,#43552,#43553,#43554));
#17762=EDGE_LOOP('',(#43555,#43556,#43557,#43558));
#17763=EDGE_LOOP('',(#43559,#43560,#43561,#43562));
#17764=EDGE_LOOP('',(#43563,#43564,#43565,#43566));
#17765=EDGE_LOOP('',(#43567,#43568,#43569,#43570));
#17766=EDGE_LOOP('',(#43571,#43572,#43573,#43574));
#17767=EDGE_LOOP('',(#43575,#43576,#43577,#43578));
#17768=EDGE_LOOP('',(#43579,#43580,#43581,#43582));
#17769=EDGE_LOOP('',(#43583,#43584,#43585,#43586));
#17770=EDGE_LOOP('',(#43587,#43588,#43589,#43590));
#17771=EDGE_LOOP('',(#43591,#43592,#43593,#43594));
#17772=EDGE_LOOP('',(#43595,#43596,#43597,#43598));
#17773=EDGE_LOOP('',(#43599,#43600,#43601,#43602));
#17774=EDGE_LOOP('',(#43603,#43604,#43605,#43606));
#17775=EDGE_LOOP('',(#43607,#43608,#43609,#43610));
#17776=EDGE_LOOP('',(#43611,#43612,#43613,#43614));
#17777=EDGE_LOOP('',(#43615,#43616,#43617,#43618));
#17778=EDGE_LOOP('',(#43619,#43620,#43621,#43622));
#17779=EDGE_LOOP('',(#43623,#43624,#43625,#43626));
#17780=EDGE_LOOP('',(#43627,#43628,#43629,#43630));
#17781=EDGE_LOOP('',(#43631,#43632,#43633,#43634));
#17782=EDGE_LOOP('',(#43635,#43636,#43637,#43638));
#17783=EDGE_LOOP('',(#43639,#43640,#43641,#43642));
#17784=EDGE_LOOP('',(#43643,#43644,#43645,#43646));
#17785=EDGE_LOOP('',(#43647,#43648,#43649,#43650));
#17786=EDGE_LOOP('',(#43651,#43652,#43653,#43654));
#17787=EDGE_LOOP('',(#43655,#43656,#43657,#43658));
#17788=EDGE_LOOP('',(#43659,#43660,#43661,#43662));
#17789=EDGE_LOOP('',(#43663,#43664,#43665,#43666));
#17790=EDGE_LOOP('',(#43667,#43668,#43669,#43670));
#17791=EDGE_LOOP('',(#43671,#43672,#43673,#43674));
#17792=EDGE_LOOP('',(#43675,#43676,#43677,#43678));
#17793=EDGE_LOOP('',(#43679,#43680,#43681,#43682));
#17794=EDGE_LOOP('',(#43683,#43684,#43685,#43686));
#17795=EDGE_LOOP('',(#43687,#43688,#43689,#43690));
#17796=EDGE_LOOP('',(#43691,#43692,#43693,#43694));
#17797=EDGE_LOOP('',(#43695,#43696,#43697,#43698));
#17798=EDGE_LOOP('',(#43699,#43700,#43701,#43702,#43703,#43704,#43705,#43706,
#43707,#43708,#43709,#43710,#43711,#43712,#43713,#43714,#43715,#43716,#43717,
#43718,#43719,#43720,#43721,#43722,#43723,#43724,#43725,#43726,#43727,#43728,
#43729,#43730,#43731,#43732,#43733));
#17799=EDGE_LOOP('',(#43734,#43735,#43736,#43737));
#17800=EDGE_LOOP('',(#43738,#43739,#43740,#43741));
#17801=EDGE_LOOP('',(#43742,#43743,#43744,#43745));
#17802=EDGE_LOOP('',(#43746,#43747,#43748,#43749));
#17803=EDGE_LOOP('',(#43750,#43751,#43752,#43753));
#17804=EDGE_LOOP('',(#43754,#43755,#43756,#43757));
#17805=EDGE_LOOP('',(#43758,#43759,#43760,#43761));
#17806=EDGE_LOOP('',(#43762,#43763,#43764,#43765));
#17807=EDGE_LOOP('',(#43766,#43767,#43768,#43769));
#17808=EDGE_LOOP('',(#43770,#43771,#43772,#43773));
#17809=EDGE_LOOP('',(#43774,#43775,#43776,#43777));
#17810=EDGE_LOOP('',(#43778,#43779,#43780,#43781));
#17811=EDGE_LOOP('',(#43782,#43783,#43784,#43785));
#17812=EDGE_LOOP('',(#43786,#43787,#43788,#43789));
#17813=EDGE_LOOP('',(#43790,#43791,#43792,#43793));
#17814=EDGE_LOOP('',(#43794,#43795,#43796,#43797));
#17815=EDGE_LOOP('',(#43798,#43799,#43800,#43801));
#17816=EDGE_LOOP('',(#43802,#43803,#43804,#43805));
#17817=EDGE_LOOP('',(#43806,#43807,#43808,#43809));
#17818=EDGE_LOOP('',(#43810,#43811,#43812,#43813));
#17819=EDGE_LOOP('',(#43814,#43815,#43816,#43817));
#17820=EDGE_LOOP('',(#43818,#43819,#43820,#43821));
#17821=EDGE_LOOP('',(#43822,#43823,#43824,#43825,#43826,#43827,#43828,#43829,
#43830,#43831,#43832,#43833,#43834,#43835,#43836,#43837,#43838,#43839,#43840,
#43841,#43842,#43843));
#17822=EDGE_LOOP('',(#43844,#43845,#43846,#43847));
#17823=EDGE_LOOP('',(#43848,#43849,#43850,#43851));
#17824=EDGE_LOOP('',(#43852,#43853,#43854,#43855));
#17825=EDGE_LOOP('',(#43856,#43857,#43858,#43859));
#17826=EDGE_LOOP('',(#43860,#43861,#43862,#43863));
#17827=EDGE_LOOP('',(#43864,#43865,#43866,#43867));
#17828=EDGE_LOOP('',(#43868,#43869,#43870,#43871,#43872,#43873));
#17829=EDGE_LOOP('',(#43874,#43875,#43876,#43877));
#17830=EDGE_LOOP('',(#43878,#43879,#43880,#43881));
#17831=EDGE_LOOP('',(#43882,#43883,#43884,#43885));
#17832=EDGE_LOOP('',(#43886,#43887,#43888,#43889));
#17833=EDGE_LOOP('',(#43890,#43891,#43892,#43893));
#17834=EDGE_LOOP('',(#43894,#43895,#43896,#43897));
#17835=EDGE_LOOP('',(#43898,#43899,#43900,#43901));
#17836=EDGE_LOOP('',(#43902,#43903,#43904,#43905));
#17837=EDGE_LOOP('',(#43906,#43907,#43908,#43909,#43910,#43911,#43912,#43913));
#17838=EDGE_LOOP('',(#43914,#43915,#43916,#43917));
#17839=EDGE_LOOP('',(#43918,#43919,#43920,#43921));
#17840=EDGE_LOOP('',(#43922,#43923,#43924,#43925));
#17841=EDGE_LOOP('',(#43926,#43927,#43928,#43929));
#17842=EDGE_LOOP('',(#43930,#43931,#43932,#43933));
#17843=EDGE_LOOP('',(#43934,#43935,#43936,#43937));
#17844=EDGE_LOOP('',(#43938,#43939,#43940,#43941));
#17845=EDGE_LOOP('',(#43942,#43943,#43944,#43945));
#17846=EDGE_LOOP('',(#43946,#43947,#43948,#43949));
#17847=EDGE_LOOP('',(#43950,#43951,#43952,#43953));
#17848=EDGE_LOOP('',(#43954,#43955,#43956,#43957));
#17849=EDGE_LOOP('',(#43958,#43959,#43960,#43961));
#17850=EDGE_LOOP('',(#43962,#43963,#43964,#43965));
#17851=EDGE_LOOP('',(#43966,#43967,#43968,#43969));
#17852=EDGE_LOOP('',(#43970,#43971,#43972,#43973));
#17853=EDGE_LOOP('',(#43974,#43975,#43976,#43977));
#17854=EDGE_LOOP('',(#43978,#43979,#43980,#43981));
#17855=EDGE_LOOP('',(#43982,#43983,#43984,#43985,#43986,#43987,#43988,#43989,
#43990,#43991,#43992,#43993,#43994,#43995,#43996,#43997,#43998));
#17856=EDGE_LOOP('',(#43999,#44000,#44001,#44002));
#17857=EDGE_LOOP('',(#44003,#44004,#44005,#44006));
#17858=EDGE_LOOP('',(#44007,#44008,#44009,#44010));
#17859=EDGE_LOOP('',(#44011,#44012,#44013,#44014));
#17860=EDGE_LOOP('',(#44015,#44016,#44017,#44018));
#17861=EDGE_LOOP('',(#44019,#44020,#44021,#44022));
#17862=EDGE_LOOP('',(#44023,#44024,#44025,#44026));
#17863=EDGE_LOOP('',(#44027,#44028,#44029,#44030));
#17864=EDGE_LOOP('',(#44031,#44032,#44033,#44034));
#17865=EDGE_LOOP('',(#44035,#44036,#44037,#44038));
#17866=EDGE_LOOP('',(#44039,#44040,#44041,#44042));
#17867=EDGE_LOOP('',(#44043,#44044,#44045,#44046));
#17868=EDGE_LOOP('',(#44047,#44048,#44049,#44050));
#17869=EDGE_LOOP('',(#44051,#44052,#44053,#44054));
#17870=EDGE_LOOP('',(#44055,#44056,#44057,#44058));
#17871=EDGE_LOOP('',(#44059,#44060,#44061,#44062));
#17872=EDGE_LOOP('',(#44063,#44064,#44065,#44066));
#17873=EDGE_LOOP('',(#44067,#44068,#44069,#44070));
#17874=EDGE_LOOP('',(#44071,#44072,#44073,#44074));
#17875=EDGE_LOOP('',(#44075,#44076,#44077,#44078,#44079,#44080,#44081,#44082,
#44083,#44084,#44085,#44086,#44087,#44088,#44089,#44090,#44091,#44092,#44093));
#17876=EDGE_LOOP('',(#44094,#44095,#44096,#44097));
#17877=EDGE_LOOP('',(#44098,#44099,#44100,#44101));
#17878=EDGE_LOOP('',(#44102,#44103,#44104,#44105));
#17879=EDGE_LOOP('',(#44106,#44107,#44108,#44109));
#17880=EDGE_LOOP('',(#44110,#44111,#44112,#44113));
#17881=EDGE_LOOP('',(#44114,#44115,#44116,#44117));
#17882=EDGE_LOOP('',(#44118,#44119,#44120,#44121));
#17883=EDGE_LOOP('',(#44122,#44123,#44124,#44125));
#17884=EDGE_LOOP('',(#44126,#44127,#44128,#44129,#44130,#44131,#44132,#44133));
#17885=EDGE_LOOP('',(#44134,#44135,#44136,#44137));
#17886=EDGE_LOOP('',(#44138,#44139,#44140,#44141));
#17887=EDGE_LOOP('',(#44142,#44143,#44144,#44145));
#17888=EDGE_LOOP('',(#44146,#44147,#44148,#44149));
#17889=EDGE_LOOP('',(#44150,#44151,#44152,#44153));
#17890=EDGE_LOOP('',(#44154,#44155,#44156,#44157));
#17891=EDGE_LOOP('',(#44158,#44159,#44160,#44161));
#17892=EDGE_LOOP('',(#44162,#44163,#44164,#44165));
#17893=EDGE_LOOP('',(#44166,#44167,#44168,#44169));
#17894=EDGE_LOOP('',(#44170,#44171,#44172,#44173,#44174,#44175,#44176,#44177,
#44178));
#17895=EDGE_LOOP('',(#44179,#44180,#44181,#44182));
#17896=EDGE_LOOP('',(#44183,#44184,#44185,#44186));
#17897=EDGE_LOOP('',(#44187,#44188,#44189,#44190));
#17898=EDGE_LOOP('',(#44191,#44192,#44193,#44194));
#17899=EDGE_LOOP('',(#44195,#44196,#44197,#44198));
#17900=EDGE_LOOP('',(#44199,#44200,#44201,#44202));
#17901=EDGE_LOOP('',(#44203,#44204,#44205,#44206));
#17902=EDGE_LOOP('',(#44207,#44208,#44209,#44210));
#17903=EDGE_LOOP('',(#44211,#44212,#44213,#44214));
#17904=EDGE_LOOP('',(#44215,#44216,#44217,#44218));
#17905=EDGE_LOOP('',(#44219,#44220,#44221,#44222));
#17906=EDGE_LOOP('',(#44223,#44224,#44225,#44226));
#17907=EDGE_LOOP('',(#44227,#44228,#44229,#44230,#44231,#44232,#44233,#44234,
#44235,#44236,#44237,#44238));
#17908=EDGE_LOOP('',(#44239,#44240,#44241,#44242));
#17909=EDGE_LOOP('',(#44243,#44244,#44245,#44246));
#17910=EDGE_LOOP('',(#44247,#44248,#44249,#44250));
#17911=EDGE_LOOP('',(#44251,#44252,#44253,#44254));
#17912=EDGE_LOOP('',(#44255,#44256,#44257,#44258));
#17913=EDGE_LOOP('',(#44259,#44260,#44261,#44262));
#17914=EDGE_LOOP('',(#44263,#44264,#44265,#44266));
#17915=EDGE_LOOP('',(#44267,#44268,#44269,#44270));
#17916=EDGE_LOOP('',(#44271,#44272,#44273,#44274));
#17917=EDGE_LOOP('',(#44275,#44276,#44277,#44278,#44279,#44280,#44281,#44282,
#44283));
#17918=EDGE_LOOP('',(#44284,#44285,#44286,#44287));
#17919=EDGE_LOOP('',(#44288,#44289,#44290,#44291));
#17920=EDGE_LOOP('',(#44292,#44293,#44294,#44295));
#17921=EDGE_LOOP('',(#44296,#44297,#44298,#44299));
#17922=EDGE_LOOP('',(#44300,#44301,#44302,#44303));
#17923=EDGE_LOOP('',(#44304,#44305,#44306,#44307));
#17924=EDGE_LOOP('',(#44308,#44309,#44310,#44311));
#17925=EDGE_LOOP('',(#44312,#44313,#44314,#44315));
#17926=EDGE_LOOP('',(#44316,#44317,#44318,#44319));
#17927=EDGE_LOOP('',(#44320,#44321,#44322,#44323));
#17928=EDGE_LOOP('',(#44324,#44325,#44326,#44327));
#17929=EDGE_LOOP('',(#44328,#44329,#44330,#44331));
#17930=EDGE_LOOP('',(#44332,#44333,#44334,#44335));
#17931=EDGE_LOOP('',(#44336,#44337,#44338,#44339));
#17932=EDGE_LOOP('',(#44340,#44341,#44342,#44343));
#17933=EDGE_LOOP('',(#44344,#44345,#44346,#44347));
#17934=EDGE_LOOP('',(#44348,#44349,#44350,#44351));
#17935=EDGE_LOOP('',(#44352,#44353,#44354,#44355));
#17936=EDGE_LOOP('',(#44356,#44357,#44358,#44359));
#17937=EDGE_LOOP('',(#44360,#44361,#44362,#44363));
#17938=EDGE_LOOP('',(#44364,#44365,#44366,#44367));
#17939=EDGE_LOOP('',(#44368,#44369,#44370,#44371));
#17940=EDGE_LOOP('',(#44372,#44373,#44374,#44375));
#17941=EDGE_LOOP('',(#44376,#44377,#44378,#44379));
#17942=EDGE_LOOP('',(#44380,#44381,#44382,#44383));
#17943=EDGE_LOOP('',(#44384,#44385,#44386,#44387));
#17944=EDGE_LOOP('',(#44388,#44389,#44390,#44391));
#17945=EDGE_LOOP('',(#44392,#44393,#44394,#44395,#44396,#44397,#44398,#44399,
#44400,#44401,#44402,#44403,#44404,#44405,#44406,#44407,#44408,#44409,#44410,
#44411,#44412,#44413));
#17946=EDGE_LOOP('',(#44414,#44415,#44416,#44417));
#17947=EDGE_LOOP('',(#44418,#44419,#44420,#44421));
#17948=EDGE_LOOP('',(#44422,#44423,#44424,#44425));
#17949=EDGE_LOOP('',(#44426,#44427,#44428,#44429));
#17950=EDGE_LOOP('',(#44430,#44431,#44432,#44433));
#17951=EDGE_LOOP('',(#44434,#44435,#44436,#44437));
#17952=EDGE_LOOP('',(#44438,#44439,#44440,#44441));
#17953=EDGE_LOOP('',(#44442,#44443,#44444,#44445));
#17954=EDGE_LOOP('',(#44446,#44447,#44448,#44449));
#17955=EDGE_LOOP('',(#44450,#44451,#44452,#44453));
#17956=EDGE_LOOP('',(#44454,#44455,#44456,#44457));
#17957=EDGE_LOOP('',(#44458,#44459,#44460,#44461,#44462,#44463,#44464,#44465,
#44466,#44467,#44468));
#17958=EDGE_LOOP('',(#44469,#44470,#44471,#44472));
#17959=EDGE_LOOP('',(#44473,#44474,#44475,#44476));
#17960=EDGE_LOOP('',(#44477,#44478,#44479,#44480));
#17961=EDGE_LOOP('',(#44481,#44482,#44483,#44484));
#17962=EDGE_LOOP('',(#44485,#44486,#44487,#44488));
#17963=EDGE_LOOP('',(#44489,#44490,#44491,#44492));
#17964=EDGE_LOOP('',(#44493,#44494,#44495,#44496));
#17965=EDGE_LOOP('',(#44497,#44498,#44499,#44500));
#17966=EDGE_LOOP('',(#44501,#44502,#44503,#44504));
#17967=EDGE_LOOP('',(#44505,#44506,#44507,#44508));
#17968=EDGE_LOOP('',(#44509,#44510,#44511,#44512));
#17969=EDGE_LOOP('',(#44513,#44514,#44515,#44516));
#17970=EDGE_LOOP('',(#44517,#44518,#44519,#44520));
#17971=EDGE_LOOP('',(#44521,#44522,#44523,#44524));
#17972=EDGE_LOOP('',(#44525,#44526,#44527,#44528));
#17973=EDGE_LOOP('',(#44529,#44530,#44531,#44532,#44533,#44534,#44535,#44536,
#44537,#44538,#44539,#44540,#44541,#44542,#44543));
#17974=EDGE_LOOP('',(#44544,#44545,#44546,#44547));
#17975=EDGE_LOOP('',(#44548,#44549,#44550,#44551));
#17976=EDGE_LOOP('',(#44552,#44553,#44554,#44555));
#17977=EDGE_LOOP('',(#44556,#44557,#44558,#44559));
#17978=EDGE_LOOP('',(#44560,#44561,#44562,#44563));
#17979=EDGE_LOOP('',(#44564,#44565,#44566,#44567));
#17980=EDGE_LOOP('',(#44568,#44569,#44570,#44571));
#17981=EDGE_LOOP('',(#44572,#44573,#44574,#44575));
#17982=EDGE_LOOP('',(#44576,#44577,#44578,#44579));
#17983=EDGE_LOOP('',(#44580,#44581,#44582,#44583));
#17984=EDGE_LOOP('',(#44584,#44585,#44586,#44587));
#17985=EDGE_LOOP('',(#44588,#44589,#44590,#44591));
#17986=EDGE_LOOP('',(#44592,#44593,#44594,#44595,#44596,#44597,#44598,#44599,
#44600,#44601,#44602,#44603));
#17987=EDGE_LOOP('',(#44604,#44605,#44606,#44607));
#17988=EDGE_LOOP('',(#44608,#44609,#44610,#44611));
#17989=EDGE_LOOP('',(#44612,#44613,#44614,#44615));
#17990=EDGE_LOOP('',(#44616,#44617,#44618,#44619));
#17991=EDGE_LOOP('',(#44620,#44621,#44622,#44623));
#17992=EDGE_LOOP('',(#44624,#44625,#44626,#44627));
#17993=EDGE_LOOP('',(#44628,#44629,#44630,#44631));
#17994=EDGE_LOOP('',(#44632,#44633,#44634,#44635));
#17995=EDGE_LOOP('',(#44636,#44637,#44638,#44639));
#17996=EDGE_LOOP('',(#44640,#44641,#44642,#44643));
#17997=EDGE_LOOP('',(#44644,#44645,#44646,#44647));
#17998=EDGE_LOOP('',(#44648,#44649,#44650,#44651));
#17999=EDGE_LOOP('',(#44652,#44653,#44654,#44655));
#18000=EDGE_LOOP('',(#44656,#44657,#44658,#44659));
#18001=EDGE_LOOP('',(#44660,#44661,#44662,#44663));
#18002=EDGE_LOOP('',(#44664,#44665,#44666,#44667));
#18003=EDGE_LOOP('',(#44668,#44669,#44670,#44671,#44672,#44673,#44674,#44675,
#44676,#44677,#44678));
#18004=EDGE_LOOP('',(#44679,#44680,#44681,#44682));
#18005=EDGE_LOOP('',(#44683,#44684,#44685,#44686));
#18006=EDGE_LOOP('',(#44687,#44688,#44689,#44690));
#18007=EDGE_LOOP('',(#44691,#44692,#44693,#44694));
#18008=EDGE_LOOP('',(#44695,#44696,#44697,#44698));
#18009=EDGE_LOOP('',(#44699,#44700,#44701,#44702));
#18010=EDGE_LOOP('',(#44703,#44704,#44705,#44706));
#18011=EDGE_LOOP('',(#44707,#44708,#44709,#44710));
#18012=EDGE_LOOP('',(#44711,#44712,#44713,#44714));
#18013=EDGE_LOOP('',(#44715,#44716,#44717,#44718));
#18014=EDGE_LOOP('',(#44719,#44720,#44721,#44722));
#18015=EDGE_LOOP('',(#44723,#44724,#44725,#44726));
#18016=EDGE_LOOP('',(#44727,#44728,#44729,#44730,#44731,#44732,#44733,#44734,
#44735,#44736,#44737,#44738));
#18017=EDGE_LOOP('',(#44739,#44740,#44741,#44742));
#18018=EDGE_LOOP('',(#44743,#44744,#44745,#44746));
#18019=EDGE_LOOP('',(#44747,#44748,#44749,#44750));
#18020=EDGE_LOOP('',(#44751,#44752,#44753,#44754));
#18021=EDGE_LOOP('',(#44755,#44756,#44757,#44758));
#18022=EDGE_LOOP('',(#44759,#44760,#44761,#44762));
#18023=EDGE_LOOP('',(#44763,#44764,#44765,#44766,#44767,#44768));
#18024=EDGE_LOOP('',(#44769,#44770,#44771,#44772));
#18025=EDGE_LOOP('',(#44773,#44774,#44775,#44776));
#18026=EDGE_LOOP('',(#44777,#44778,#44779,#44780));
#18027=EDGE_LOOP('',(#44781,#44782,#44783,#44784));
#18028=EDGE_LOOP('',(#44785,#44786,#44787,#44788));
#18029=EDGE_LOOP('',(#44789,#44790,#44791,#44792));
#18030=EDGE_LOOP('',(#44793,#44794,#44795,#44796));
#18031=EDGE_LOOP('',(#44797,#44798,#44799,#44800));
#18032=EDGE_LOOP('',(#44801,#44802,#44803,#44804));
#18033=EDGE_LOOP('',(#44805,#44806,#44807,#44808));
#18034=EDGE_LOOP('',(#44809,#44810,#44811,#44812));
#18035=EDGE_LOOP('',(#44813,#44814,#44815,#44816));
#18036=EDGE_LOOP('',(#44817,#44818,#44819,#44820,#44821,#44822,#44823,#44824,
#44825,#44826,#44827,#44828));
#18037=EDGE_LOOP('',(#44829,#44830,#44831,#44832));
#18038=EDGE_LOOP('',(#44833,#44834,#44835,#44836));
#18039=EDGE_LOOP('',(#44837,#44838,#44839,#44840));
#18040=EDGE_LOOP('',(#44841,#44842,#44843,#44844));
#18041=EDGE_LOOP('',(#44845,#44846,#44847,#44848));
#18042=EDGE_LOOP('',(#44849,#44850,#44851,#44852));
#18043=EDGE_LOOP('',(#44853,#44854,#44855,#44856));
#18044=EDGE_LOOP('',(#44857,#44858,#44859,#44860));
#18045=EDGE_LOOP('',(#44861,#44862,#44863,#44864));
#18046=EDGE_LOOP('',(#44865,#44866,#44867,#44868));
#18047=EDGE_LOOP('',(#44869,#44870,#44871,#44872));
#18048=EDGE_LOOP('',(#44873,#44874,#44875,#44876));
#18049=EDGE_LOOP('',(#44877,#44878,#44879,#44880));
#18050=EDGE_LOOP('',(#44881,#44882,#44883,#44884));
#18051=EDGE_LOOP('',(#44885,#44886,#44887,#44888));
#18052=EDGE_LOOP('',(#44889,#44890,#44891,#44892));
#18053=EDGE_LOOP('',(#44893,#44894,#44895,#44896));
#18054=EDGE_LOOP('',(#44897,#44898,#44899,#44900));
#18055=EDGE_LOOP('',(#44901,#44902,#44903,#44904));
#18056=EDGE_LOOP('',(#44905,#44906,#44907,#44908,#44909,#44910,#44911,#44912,
#44913,#44914,#44915,#44916,#44917,#44918,#44919,#44920,#44921,#44922,#44923));
#18057=EDGE_LOOP('',(#44924,#44925,#44926,#44927));
#18058=EDGE_LOOP('',(#44928,#44929,#44930,#44931));
#18059=EDGE_LOOP('',(#44932,#44933,#44934,#44935));
#18060=EDGE_LOOP('',(#44936,#44937,#44938,#44939));
#18061=EDGE_LOOP('',(#44940,#44941,#44942,#44943));
#18062=EDGE_LOOP('',(#44944,#44945,#44946,#44947,#44948,#44949,#44950,#44951,
#44952,#44953,#44954,#44955,#44956,#44957,#44958,#44959,#44960,#44961,#44962));
#18063=EDGE_LOOP('',(#44963,#44964,#44965,#44966,#44967,#44968,#44969,#44970,
#44971,#44972,#44973,#44974));
#18064=EDGE_LOOP('',(#44975,#44976,#44977,#44978,#44979,#44980));
#18065=EDGE_LOOP('',(#44981,#44982,#44983,#44984,#44985,#44986,#44987,#44988,
#44989,#44990,#44991,#44992));
#18066=EDGE_LOOP('',(#44993,#44994,#44995,#44996,#44997,#44998,#44999,#45000,
#45001,#45002,#45003));
#18067=EDGE_LOOP('',(#45004,#45005,#45006,#45007));
#18068=EDGE_LOOP('',(#45008,#45009,#45010,#45011,#45012,#45013,#45014,#45015,
#45016,#45017,#45018,#45019));
#18069=EDGE_LOOP('',(#45020,#45021,#45022,#45023,#45024,#45025,#45026,#45027,
#45028,#45029,#45030,#45031,#45032,#45033,#45034));
#18070=EDGE_LOOP('',(#45035,#45036,#45037,#45038,#45039,#45040,#45041,#45042,
#45043,#45044,#45045));
#18071=EDGE_LOOP('',(#45046,#45047,#45048,#45049,#45050,#45051,#45052,#45053,
#45054,#45055,#45056,#45057,#45058,#45059,#45060,#45061,#45062,#45063,#45064,
#45065,#45066,#45067));
#18072=EDGE_LOOP('',(#45068,#45069,#45070,#45071));
#18073=EDGE_LOOP('',(#45072,#45073,#45074,#45075,#45076,#45077,#45078,#45079,
#45080));
#18074=EDGE_LOOP('',(#45081,#45082,#45083,#45084,#45085,#45086,#45087,#45088,
#45089,#45090,#45091,#45092));
#18075=EDGE_LOOP('',(#45093,#45094,#45095,#45096,#45097,#45098,#45099,#45100,
#45101));
#18076=EDGE_LOOP('',(#45102,#45103,#45104,#45105,#45106,#45107,#45108,#45109));
#18077=EDGE_LOOP('',(#45110,#45111,#45112,#45113,#45114,#45115,#45116,#45117,
#45118,#45119,#45120,#45121,#45122,#45123,#45124,#45125,#45126,#45127,#45128));
#18078=EDGE_LOOP('',(#45129,#45130,#45131,#45132,#45133,#45134,#45135,#45136,
#45137,#45138,#45139,#45140,#45141,#45142,#45143,#45144,#45145));
#18079=EDGE_LOOP('',(#45146,#45147,#45148,#45149,#45150,#45151,#45152,#45153));
#18080=EDGE_LOOP('',(#45154,#45155,#45156,#45157,#45158,#45159));
#18081=EDGE_LOOP('',(#45160,#45161,#45162,#45163,#45164,#45165,#45166,#45167,
#45168,#45169,#45170,#45171,#45172,#45173,#45174,#45175,#45176,#45177,#45178,
#45179,#45180,#45181));
#18082=EDGE_LOOP('',(#45182,#45183,#45184,#45185,#45186,#45187,#45188,#45189,
#45190,#45191,#45192,#45193,#45194,#45195,#45196,#45197,#45198,#45199,#45200,
#45201,#45202,#45203,#45204,#45205,#45206,#45207,#45208,#45209,#45210,#45211,
#45212,#45213,#45214,#45215,#45216));
#18083=EDGE_LOOP('',(#45217,#45218,#45219,#45220));
#18084=EDGE_LOOP('',(#45221,#45222,#45223,#45224,#45225,#45226,#45227,#45228,
#45229,#45230,#45231,#45232));
#18085=EDGE_LOOP('',(#45233,#45234,#45235,#45236));
#18086=EDGE_LOOP('',(#45237,#45238,#45239,#45240));
#18087=EDGE_LOOP('',(#45241,#45242,#45243,#45244,#45245,#45246,#45247,#45248));
#18088=EDGE_LOOP('',(#45249));
#18089=EDGE_LOOP('',(#45250));
#18090=EDGE_LOOP('',(#45251));
#18091=EDGE_LOOP('',(#45252));
#18092=EDGE_LOOP('',(#45253));
#18093=EDGE_LOOP('',(#45254));
#18094=EDGE_LOOP('',(#45255));
#18095=EDGE_LOOP('',(#45256));
#18096=EDGE_LOOP('',(#45257));
#18097=EDGE_LOOP('',(#45258));
#18098=EDGE_LOOP('',(#45259));
#18099=EDGE_LOOP('',(#45260,#45261,#45262,#45263));
#18100=EDGE_LOOP('',(#45264,#45265,#45266,#45267));
#18101=EDGE_LOOP('',(#45268,#45269,#45270,#45271,#45272,#45273,#45274,#45275));
#18102=EDGE_LOOP('',(#45276));
#18103=EDGE_LOOP('',(#45277));
#18104=EDGE_LOOP('',(#45278));
#18105=EDGE_LOOP('',(#45279));
#18106=EDGE_LOOP('',(#45280,#45281,#45282,#45283));
#18107=EDGE_LOOP('',(#45284,#45285,#45286,#45287));
#18108=EDGE_LOOP('',(#45288,#45289,#45290,#45291));
#18109=EDGE_LOOP('',(#45292,#45293,#45294,#45295));
#18110=EDGE_LOOP('',(#45296,#45297,#45298,#45299));
#18111=EDGE_LOOP('',(#45300,#45301,#45302,#45303));
#18112=EDGE_LOOP('',(#45304,#45305,#45306,#45307));
#18113=EDGE_LOOP('',(#45308,#45309,#45310,#45311));
#18114=EDGE_LOOP('',(#45312,#45313,#45314,#45315));
#18115=EDGE_LOOP('',(#45316,#45317,#45318));
#18116=EDGE_LOOP('',(#45319,#45320,#45321,#45322));
#18117=EDGE_LOOP('',(#45323,#45324,#45325));
#18118=EDGE_LOOP('',(#45326,#45327,#45328,#45329));
#18119=EDGE_LOOP('',(#45330,#45331,#45332));
#18120=EDGE_LOOP('',(#45333,#45334,#45335,#45336));
#18121=EDGE_LOOP('',(#45337,#45338,#45339,#45340));
#18122=EDGE_LOOP('',(#45341,#45342,#45343));
#18123=EDGE_LOOP('',(#45344,#45345,#45346,#45347));
#18124=EDGE_LOOP('',(#45348,#45349,#45350,#45351));
#18125=EDGE_LOOP('',(#45352,#45353,#45354));
#18126=EDGE_LOOP('',(#45355,#45356,#45357,#45358));
#18127=EDGE_LOOP('',(#45359,#45360,#45361,#45362));
#18128=EDGE_LOOP('',(#45363,#45364,#45365));
#18129=EDGE_LOOP('',(#45366,#45367,#45368,#45369));
#18130=EDGE_LOOP('',(#45370,#45371,#45372,#45373));
#18131=EDGE_LOOP('',(#45374,#45375,#45376,#45377));
#18132=EDGE_LOOP('',(#45378));
#18133=EDGE_LOOP('',(#45379,#45380,#45381,#45382));
#18134=EDGE_LOOP('',(#45383,#45384,#45385,#45386));
#18135=EDGE_LOOP('',(#45387,#45388,#45389,#45390));
#18136=EDGE_LOOP('',(#45391,#45392,#45393,#45394));
#18137=EDGE_LOOP('',(#45395,#45396,#45397,#45398));
#18138=EDGE_LOOP('',(#45399,#45400,#45401,#45402));
#18139=EDGE_LOOP('',(#45403,#45404,#45405,#45406));
#18140=EDGE_LOOP('',(#45407,#45408,#45409,#45410));
#18141=EDGE_LOOP('',(#45411,#45412,#45413,#45414));
#18142=EDGE_LOOP('',(#45415,#45416,#45417,#45418));
#18143=EDGE_LOOP('',(#45419,#45420,#45421,#45422));
#18144=EDGE_LOOP('',(#45423,#45424,#45425,#45426));
#18145=EDGE_LOOP('',(#45427,#45428,#45429,#45430));
#18146=EDGE_LOOP('',(#45431,#45432,#45433,#45434));
#18147=EDGE_LOOP('',(#45435,#45436,#45437,#45438));
#18148=EDGE_LOOP('',(#45439,#45440,#45441,#45442));
#18149=EDGE_LOOP('',(#45443,#45444,#45445,#45446));
#18150=EDGE_LOOP('',(#45447,#45448,#45449,#45450));
#18151=EDGE_LOOP('',(#45451,#45452,#45453,#45454));
#18152=EDGE_LOOP('',(#45455,#45456,#45457,#45458));
#18153=EDGE_LOOP('',(#45459,#45460,#45461,#45462));
#18154=EDGE_LOOP('',(#45463,#45464,#45465,#45466));
#18155=EDGE_LOOP('',(#45467,#45468,#45469,#45470));
#18156=EDGE_LOOP('',(#45471,#45472,#45473,#45474));
#18157=EDGE_LOOP('',(#45475,#45476,#45477,#45478));
#18158=EDGE_LOOP('',(#45479,#45480,#45481,#45482));
#18159=EDGE_LOOP('',(#45483));
#18160=EDGE_LOOP('',(#45484));
#18161=EDGE_LOOP('',(#45485,#45486,#45487,#45488));
#18162=EDGE_LOOP('',(#45489,#45490,#45491,#45492));
#18163=EDGE_LOOP('',(#45493,#45494,#45495,#45496));
#18164=EDGE_LOOP('',(#45497));
#18165=EDGE_LOOP('',(#45498));
#18166=EDGE_LOOP('',(#45499,#45500,#45501,#45502));
#18167=EDGE_LOOP('',(#45503,#45504,#45505,#45506));
#18168=EDGE_LOOP('',(#45507,#45508,#45509,#45510));
#18169=EDGE_LOOP('',(#45511,#45512,#45513,#45514));
#18170=EDGE_LOOP('',(#45515,#45516,#45517,#45518));
#18171=EDGE_LOOP('',(#45519,#45520,#45521,#45522));
#18172=EDGE_LOOP('',(#45523,#45524,#45525,#45526));
#18173=EDGE_LOOP('',(#45527,#45528,#45529,#45530));
#18174=EDGE_LOOP('',(#45531,#45532,#45533,#45534));
#18175=EDGE_LOOP('',(#45535,#45536,#45537,#45538));
#18176=EDGE_LOOP('',(#45539,#45540,#45541,#45542));
#18177=EDGE_LOOP('',(#45543,#45544,#45545,#45546));
#18178=EDGE_LOOP('',(#45547,#45548,#45549,#45550));
#18179=EDGE_LOOP('',(#45551,#45552,#45553,#45554));
#18180=EDGE_LOOP('',(#45555,#45556,#45557,#45558));
#18181=EDGE_LOOP('',(#45559,#45560,#45561,#45562));
#18182=EDGE_LOOP('',(#45563,#45564,#45565,#45566));
#18183=EDGE_LOOP('',(#45567,#45568,#45569));
#18184=EDGE_LOOP('',(#45570,#45571,#45572,#45573,#45574));
#18185=EDGE_LOOP('',(#45575,#45576,#45577,#45578));
#18186=EDGE_LOOP('',(#45579,#45580,#45581,#45582));
#18187=EDGE_LOOP('',(#45583,#45584,#45585,#45586));
#18188=EDGE_LOOP('',(#45587,#45588,#45589,#45590));
#18189=EDGE_LOOP('',(#45591,#45592,#45593,#45594));
#18190=EDGE_LOOP('',(#45595,#45596,#45597,#45598));
#18191=EDGE_LOOP('',(#45599,#45600,#45601,#45602));
#18192=EDGE_LOOP('',(#45603,#45604,#45605,#45606));
#18193=EDGE_LOOP('',(#45607,#45608,#45609,#45610));
#18194=EDGE_LOOP('',(#45611,#45612,#45613,#45614));
#18195=EDGE_LOOP('',(#45615,#45616,#45617,#45618));
#18196=EDGE_LOOP('',(#45619,#45620,#45621,#45622));
#18197=EDGE_LOOP('',(#45623,#45624,#45625,#45626));
#18198=EDGE_LOOP('',(#45627,#45628,#45629,#45630));
#18199=EDGE_LOOP('',(#45631,#45632,#45633,#45634,#45635,#45636));
#18200=EDGE_LOOP('',(#45637,#45638,#45639,#45640,#45641,#45642,#45643,#45644,
#45645,#45646,#45647,#45648,#45649,#45650,#45651,#45652,#45653,#45654,#45655,
#45656,#45657,#45658,#45659,#45660,#45661,#45662,#45663,#45664,#45665,#45666,
#45667,#45668,#45669,#45670,#45671));
#18201=EDGE_LOOP('',(#45672,#45673,#45674,#45675,#45676));
#18202=EDGE_LOOP('',(#45677,#45678,#45679,#45680));
#18203=EDGE_LOOP('',(#45681,#45682,#45683,#45684,#45685,#45686,#45687,#45688,
#45689,#45690,#45691,#45692,#45693,#45694,#45695,#45696,#45697,#45698,#45699,
#45700,#45701,#45702,#45703,#45704,#45705,#45706,#45707,#45708,#45709,#45710,
#45711,#45712,#45713,#45714,#45715,#45716));
#18204=EDGE_LOOP('',(#45717,#45718,#45719,#45720,#45721,#45722));
#18205=EDGE_LOOP('',(#45723,#45724,#45725,#45726));
#18206=EDGE_LOOP('',(#45727));
#18207=EDGE_LOOP('',(#45728));
#18208=EDGE_LOOP('',(#45729,#45730,#45731,#45732));
#18209=EDGE_LOOP('',(#45733,#45734,#45735));
#18210=EDGE_LOOP('',(#45736,#45737,#45738,#45739));
#18211=EDGE_LOOP('',(#45740,#45741,#45742));
#18212=EDGE_LOOP('',(#45743,#45744,#45745,#45746));
#18213=EDGE_LOOP('',(#45747,#45748,#45749));
#18214=EDGE_LOOP('',(#45750,#45751,#45752,#45753));
#18215=EDGE_LOOP('',(#45754,#45755,#45756));
#18216=EDGE_LOOP('',(#45757,#45758,#45759,#45760));
#18217=EDGE_LOOP('',(#45761,#45762,#45763));
#18218=EDGE_LOOP('',(#45764,#45765,#45766,#45767));
#18219=EDGE_LOOP('',(#45768,#45769,#45770));
#18220=EDGE_LOOP('',(#45771,#45772,#45773,#45774));
#18221=EDGE_LOOP('',(#45775,#45776,#45777));
#18222=EDGE_LOOP('',(#45778,#45779,#45780,#45781));
#18223=EDGE_LOOP('',(#45782,#45783,#45784));
#18224=EDGE_LOOP('',(#45785,#45786,#45787,#45788));
#18225=EDGE_LOOP('',(#45789,#45790,#45791));
#18226=EDGE_LOOP('',(#45792,#45793,#45794,#45795));
#18227=EDGE_LOOP('',(#45796,#45797,#45798));
#18228=EDGE_LOOP('',(#45799,#45800,#45801,#45802));
#18229=EDGE_LOOP('',(#45803,#45804,#45805));
#18230=EDGE_LOOP('',(#45806,#45807,#45808,#45809));
#18231=EDGE_LOOP('',(#45810,#45811,#45812));
#18232=EDGE_LOOP('',(#45813,#45814,#45815,#45816));
#18233=EDGE_LOOP('',(#45817,#45818,#45819));
#18234=EDGE_LOOP('',(#45820,#45821,#45822,#45823));
#18235=EDGE_LOOP('',(#45824,#45825,#45826));
#18236=EDGE_LOOP('',(#45827,#45828,#45829,#45830));
#18237=EDGE_LOOP('',(#45831,#45832,#45833));
#18238=EDGE_LOOP('',(#45834,#45835,#45836,#45837));
#18239=EDGE_LOOP('',(#45838,#45839,#45840));
#18240=EDGE_LOOP('',(#45841,#45842,#45843,#45844));
#18241=EDGE_LOOP('',(#45845,#45846,#45847));
#18242=EDGE_LOOP('',(#45848,#45849,#45850,#45851));
#18243=EDGE_LOOP('',(#45852,#45853,#45854));
#18244=EDGE_LOOP('',(#45855,#45856,#45857,#45858));
#18245=EDGE_LOOP('',(#45859,#45860,#45861));
#18246=EDGE_LOOP('',(#45862,#45863,#45864,#45865));
#18247=EDGE_LOOP('',(#45866,#45867,#45868));
#18248=EDGE_LOOP('',(#45869,#45870,#45871,#45872));
#18249=EDGE_LOOP('',(#45873,#45874,#45875));
#18250=EDGE_LOOP('',(#45876,#45877,#45878,#45879));
#18251=EDGE_LOOP('',(#45880,#45881,#45882));
#18252=EDGE_LOOP('',(#45883,#45884,#45885,#45886));
#18253=EDGE_LOOP('',(#45887,#45888,#45889));
#18254=EDGE_LOOP('',(#45890,#45891,#45892,#45893));
#18255=EDGE_LOOP('',(#45894,#45895,#45896));
#18256=EDGE_LOOP('',(#45897,#45898,#45899,#45900));
#18257=EDGE_LOOP('',(#45901,#45902,#45903));
#18258=EDGE_LOOP('',(#45904,#45905,#45906,#45907));
#18259=EDGE_LOOP('',(#45908,#45909,#45910));
#18260=EDGE_LOOP('',(#45911,#45912,#45913,#45914));
#18261=EDGE_LOOP('',(#45915,#45916,#45917));
#18262=EDGE_LOOP('',(#45918,#45919,#45920,#45921));
#18263=EDGE_LOOP('',(#45922,#45923,#45924));
#18264=EDGE_LOOP('',(#45925,#45926,#45927,#45928));
#18265=EDGE_LOOP('',(#45929,#45930,#45931));
#18266=EDGE_LOOP('',(#45932,#45933,#45934,#45935));
#18267=EDGE_LOOP('',(#45936,#45937,#45938));
#18268=EDGE_LOOP('',(#45939,#45940,#45941,#45942));
#18269=EDGE_LOOP('',(#45943,#45944,#45945));
#18270=EDGE_LOOP('',(#45946,#45947,#45948,#45949));
#18271=EDGE_LOOP('',(#45950,#45951,#45952));
#18272=EDGE_LOOP('',(#45953,#45954,#45955,#45956));
#18273=EDGE_LOOP('',(#45957,#45958,#45959));
#18274=EDGE_LOOP('',(#45960,#45961,#45962,#45963));
#18275=EDGE_LOOP('',(#45964,#45965,#45966));
#18276=EDGE_LOOP('',(#45967,#45968,#45969,#45970));
#18277=EDGE_LOOP('',(#45971,#45972,#45973,#45974));
#18278=EDGE_LOOP('',(#45975,#45976,#45977,#45978));
#18279=EDGE_LOOP('',(#45979,#45980,#45981,#45982));
#18280=EDGE_LOOP('',(#45983,#45984,#45985,#45986));
#18281=EDGE_LOOP('',(#45987,#45988,#45989));
#18282=EDGE_LOOP('',(#45990,#45991,#45992,#45993));
#18283=EDGE_LOOP('',(#45994,#45995,#45996));
#18284=EDGE_LOOP('',(#45997,#45998,#45999,#46000));
#18285=EDGE_LOOP('',(#46001,#46002,#46003));
#18286=EDGE_LOOP('',(#46004,#46005,#46006,#46007));
#18287=EDGE_LOOP('',(#46008,#46009,#46010));
#18288=EDGE_LOOP('',(#46011,#46012,#46013,#46014));
#18289=EDGE_LOOP('',(#46015,#46016,#46017));
#18290=EDGE_LOOP('',(#46018,#46019,#46020,#46021));
#18291=EDGE_LOOP('',(#46022,#46023,#46024));
#18292=EDGE_LOOP('',(#46025,#46026,#46027,#46028));
#18293=EDGE_LOOP('',(#46029,#46030,#46031));
#18294=EDGE_LOOP('',(#46032,#46033,#46034,#46035));
#18295=EDGE_LOOP('',(#46036,#46037,#46038));
#18296=EDGE_LOOP('',(#46039,#46040,#46041,#46042));
#18297=EDGE_LOOP('',(#46043,#46044,#46045));
#18298=EDGE_LOOP('',(#46046,#46047,#46048,#46049));
#18299=EDGE_LOOP('',(#46050,#46051,#46052));
#18300=EDGE_LOOP('',(#46053,#46054,#46055,#46056));
#18301=EDGE_LOOP('',(#46057,#46058,#46059));
#18302=EDGE_LOOP('',(#46060,#46061,#46062,#46063));
#18303=EDGE_LOOP('',(#46064,#46065,#46066));
#18304=EDGE_LOOP('',(#46067,#46068,#46069,#46070));
#18305=EDGE_LOOP('',(#46071,#46072,#46073));
#18306=EDGE_LOOP('',(#46074,#46075,#46076,#46077));
#18307=EDGE_LOOP('',(#46078,#46079,#46080));
#18308=EDGE_LOOP('',(#46081,#46082,#46083,#46084));
#18309=EDGE_LOOP('',(#46085,#46086,#46087));
#18310=EDGE_LOOP('',(#46088,#46089,#46090,#46091));
#18311=EDGE_LOOP('',(#46092,#46093,#46094));
#18312=EDGE_LOOP('',(#46095,#46096,#46097,#46098));
#18313=EDGE_LOOP('',(#46099,#46100,#46101));
#18314=EDGE_LOOP('',(#46102,#46103,#46104,#46105));
#18315=EDGE_LOOP('',(#46106,#46107,#46108));
#18316=EDGE_LOOP('',(#46109,#46110,#46111,#46112));
#18317=EDGE_LOOP('',(#46113,#46114,#46115));
#18318=EDGE_LOOP('',(#46116,#46117,#46118,#46119));
#18319=EDGE_LOOP('',(#46120,#46121,#46122));
#18320=EDGE_LOOP('',(#46123,#46124,#46125,#46126));
#18321=EDGE_LOOP('',(#46127,#46128,#46129));
#18322=EDGE_LOOP('',(#46130,#46131,#46132,#46133));
#18323=EDGE_LOOP('',(#46134,#46135,#46136));
#18324=EDGE_LOOP('',(#46137,#46138,#46139,#46140));
#18325=EDGE_LOOP('',(#46141,#46142,#46143));
#18326=EDGE_LOOP('',(#46144,#46145,#46146,#46147));
#18327=EDGE_LOOP('',(#46148,#46149,#46150));
#18328=EDGE_LOOP('',(#46151,#46152,#46153,#46154));
#18329=EDGE_LOOP('',(#46155,#46156,#46157));
#18330=EDGE_LOOP('',(#46158,#46159,#46160,#46161));
#18331=EDGE_LOOP('',(#46162,#46163,#46164));
#18332=EDGE_LOOP('',(#46165,#46166,#46167,#46168));
#18333=EDGE_LOOP('',(#46169,#46170,#46171));
#18334=EDGE_LOOP('',(#46172,#46173,#46174,#46175));
#18335=EDGE_LOOP('',(#46176,#46177,#46178));
#18336=EDGE_LOOP('',(#46179,#46180,#46181,#46182));
#18337=EDGE_LOOP('',(#46183,#46184,#46185));
#18338=EDGE_LOOP('',(#46186,#46187,#46188,#46189));
#18339=EDGE_LOOP('',(#46190,#46191,#46192));
#18340=EDGE_LOOP('',(#46193,#46194,#46195,#46196));
#18341=EDGE_LOOP('',(#46197,#46198,#46199));
#18342=EDGE_LOOP('',(#46200,#46201,#46202,#46203));
#18343=EDGE_LOOP('',(#46204,#46205,#46206));
#18344=EDGE_LOOP('',(#46207,#46208,#46209,#46210));
#18345=EDGE_LOOP('',(#46211,#46212,#46213));
#18346=EDGE_LOOP('',(#46214,#46215,#46216,#46217));
#18347=EDGE_LOOP('',(#46218,#46219,#46220));
#18348=EDGE_LOOP('',(#46221,#46222,#46223));
#18349=EDGE_LOOP('',(#46224,#46225,#46226,#46227));
#18350=EDGE_LOOP('',(#46228,#46229,#46230,#46231));
#18351=EDGE_LOOP('',(#46232,#46233,#46234));
#18352=EDGE_LOOP('',(#46235,#46236,#46237));
#18353=EDGE_LOOP('',(#46238,#46239,#46240,#46241));
#18354=EDGE_LOOP('',(#46242,#46243,#46244,#46245));
#18355=EDGE_LOOP('',(#46246,#46247,#46248,#46249));
#18356=EDGE_LOOP('',(#46250,#46251,#46252,#46253));
#18357=EDGE_LOOP('',(#46254,#46255,#46256,#46257));
#18358=EDGE_LOOP('',(#46258,#46259,#46260,#46261));
#18359=EDGE_LOOP('',(#46262,#46263,#46264,#46265,#46266,#46267));
#18360=EDGE_LOOP('',(#46268));
#18361=EDGE_LOOP('',(#46269));
#18362=EDGE_LOOP('',(#46270,#46271,#46272,#46273,#46274,#46275));
#18363=EDGE_LOOP('',(#46276,#46277,#46278,#46279,#46280,#46281,#46282,#46283,
#46284,#46285,#46286,#46287,#46288,#46289,#46290,#46291,#46292,#46293,#46294,
#46295,#46296,#46297,#46298,#46299,#46300,#46301,#46302,#46303,#46304,#46305,
#46306,#46307,#46308,#46309,#46310,#46311,#46312,#46313,#46314,#46315,#46316,
#46317,#46318,#46319,#46320,#46321,#46322,#46323,#46324,#46325,#46326,#46327,
#46328,#46329,#46330,#46331,#46332,#46333,#46334,#46335,#46336,#46337,#46338,
#46339,#46340,#46341,#46342,#46343,#46344,#46345,#46346,#46347,#46348,#46349,
#46350,#46351,#46352,#46353,#46354,#46355,#46356,#46357,#46358,#46359,#46360,
#46361,#46362,#46363,#46364,#46365,#46366,#46367,#46368,#46369,#46370,#46371,
#46372,#46373,#46374,#46375,#46376,#46377,#46378,#46379,#46380,#46381,#46382,
#46383,#46384,#46385,#46386,#46387,#46388,#46389,#46390,#46391,#46392,#46393,
#46394,#46395,#46396,#46397,#46398,#46399,#46400,#46401,#46402,#46403,#46404,
#46405,#46406,#46407,#46408,#46409,#46410,#46411,#46412,#46413,#46414,#46415,
#46416,#46417,#46418,#46419,#46420,#46421,#46422,#46423));
#18364=EDGE_LOOP('',(#46424,#46425,#46426,#46427,#46428,#46429,#46430,#46431,
#46432,#46433,#46434,#46435,#46436,#46437,#46438,#46439,#46440,#46441,#46442,
#46443,#46444,#46445,#46446,#46447,#46448,#46449,#46450,#46451,#46452,#46453,
#46454,#46455,#46456,#46457,#46458,#46459,#46460,#46461,#46462,#46463,#46464,
#46465,#46466,#46467,#46468,#46469,#46470,#46471,#46472,#46473,#46474,#46475,
#46476,#46477,#46478,#46479,#46480,#46481,#46482,#46483,#46484,#46485,#46486,
#46487,#46488,#46489,#46490,#46491,#46492,#46493,#46494,#46495,#46496,#46497,
#46498,#46499));
#18365=EDGE_LOOP('',(#46500));
#18366=EDGE_LOOP('',(#46501,#46502,#46503,#46504,#46505,#46506));
#18367=EDGE_LOOP('',(#46507,#46508,#46509,#46510));
#18368=EDGE_LOOP('',(#46511,#46512,#46513,#46514));
#18369=EDGE_LOOP('',(#46515,#46516,#46517,#46518));
#18370=EDGE_LOOP('',(#46519));
#18371=EDGE_LOOP('',(#46520));
#18372=EDGE_LOOP('',(#46521,#46522,#46523,#46524));
#18373=EDGE_LOOP('',(#46525,#46526,#46527,#46528));
#18374=EDGE_LOOP('',(#46529,#46530,#46531,#46532));
#18375=EDGE_LOOP('',(#46533));
#18376=EDGE_LOOP('',(#46534));
#18377=EDGE_LOOP('',(#46535,#46536,#46537,#46538));
#18378=EDGE_LOOP('',(#46539,#46540,#46541,#46542));
#18379=EDGE_LOOP('',(#46543,#46544,#46545,#46546,#46547,#46548,#46549,#46550));
#18380=EDGE_LOOP('',(#46551,#46552,#46553,#46554,#46555,#46556,#46557,#46558));
#18381=EDGE_LOOP('',(#46559,#46560,#46561,#46562,#46563));
#18382=EDGE_LOOP('',(#46564,#46565,#46566,#46567));
#18383=EDGE_LOOP('',(#46568,#46569,#46570,#46571,#46572));
#18384=EDGE_LOOP('',(#46573,#46574,#46575,#46576));
#18385=EDGE_LOOP('',(#46577,#46578,#46579,#46580,#46581));
#18386=EDGE_LOOP('',(#46582,#46583,#46584,#46585));
#18387=EDGE_LOOP('',(#46586,#46587,#46588,#46589,#46590));
#18388=EDGE_LOOP('',(#46591,#46592,#46593,#46594));
#18389=EDGE_LOOP('',(#46595,#46596,#46597,#46598));
#18390=EDGE_LOOP('',(#46599,#46600,#46601,#46602));
#18391=EDGE_LOOP('',(#46603,#46604,#46605,#46606));
#18392=EDGE_LOOP('',(#46607,#46608,#46609,#46610));
#18393=EDGE_LOOP('',(#46611,#46612,#46613,#46614));
#18394=EDGE_LOOP('',(#46615,#46616,#46617,#46618));
#18395=EDGE_LOOP('',(#46619,#46620,#46621,#46622));
#18396=EDGE_LOOP('',(#46623,#46624,#46625,#46626));
#18397=EDGE_LOOP('',(#46627,#46628,#46629,#46630));
#18398=EDGE_LOOP('',(#46631,#46632,#46633,#46634));
#18399=EDGE_LOOP('',(#46635,#46636,#46637,#46638));
#18400=EDGE_LOOP('',(#46639,#46640,#46641,#46642));
#18401=EDGE_LOOP('',(#46643,#46644,#46645,#46646));
#18402=EDGE_LOOP('',(#46647,#46648,#46649,#46650));
#18403=EDGE_LOOP('',(#46651,#46652,#46653,#46654));
#18404=EDGE_LOOP('',(#46655,#46656,#46657,#46658,#46659));
#18405=EDGE_LOOP('',(#46660,#46661,#46662,#46663));
#18406=EDGE_LOOP('',(#46664,#46665,#46666,#46667));
#18407=EDGE_LOOP('',(#46668,#46669,#46670,#46671));
#18408=EDGE_LOOP('',(#46672,#46673,#46674,#46675));
#18409=EDGE_LOOP('',(#46676,#46677,#46678,#46679));
#18410=EDGE_LOOP('',(#46680,#46681,#46682,#46683));
#18411=EDGE_LOOP('',(#46684,#46685,#46686,#46687));
#18412=EDGE_LOOP('',(#46688,#46689,#46690,#46691));
#18413=EDGE_LOOP('',(#46692,#46693,#46694,#46695));
#18414=EDGE_LOOP('',(#46696,#46697,#46698,#46699));
#18415=EDGE_LOOP('',(#46700,#46701,#46702,#46703));
#18416=EDGE_LOOP('',(#46704,#46705,#46706,#46707));
#18417=EDGE_LOOP('',(#46708,#46709,#46710,#46711));
#18418=EDGE_LOOP('',(#46712,#46713,#46714,#46715));
#18419=EDGE_LOOP('',(#46716,#46717,#46718,#46719));
#18420=EDGE_LOOP('',(#46720,#46721,#46722,#46723,#46724));
#18421=EDGE_LOOP('',(#46725,#46726,#46727,#46728,#46729,#46730,#46731,#46732,
#46733,#46734,#46735,#46736,#46737,#46738,#46739,#46740,#46741,#46742,#46743,
#46744,#46745,#46746,#46747,#46748,#46749,#46750,#46751,#46752,#46753,#46754,
#46755,#46756,#46757,#46758,#46759));
#18422=EDGE_LOOP('',(#46760,#46761,#46762,#46763,#46764));
#18423=EDGE_LOOP('',(#46765,#46766,#46767,#46768));
#18424=EDGE_LOOP('',(#46769,#46770,#46771,#46772,#46773,#46774,#46775,#46776,
#46777,#46778,#46779,#46780,#46781,#46782,#46783,#46784,#46785,#46786,#46787,
#46788,#46789,#46790,#46791,#46792,#46793,#46794,#46795,#46796,#46797,#46798,
#46799,#46800,#46801,#46802));
#18425=EDGE_LOOP('',(#46803,#46804,#46805,#46806,#46807,#46808,#46809));
#18426=EDGE_LOOP('',(#46810,#46811,#46812));
#18427=EDGE_LOOP('',(#46813));
#18428=EDGE_LOOP('',(#46814));
#18429=EDGE_LOOP('',(#46815,#46816,#46817,#46818));
#18430=EDGE_LOOP('',(#46819,#46820,#46821));
#18431=EDGE_LOOP('',(#46822,#46823,#46824,#46825));
#18432=EDGE_LOOP('',(#46826,#46827,#46828));
#18433=EDGE_LOOP('',(#46829,#46830,#46831,#46832));
#18434=EDGE_LOOP('',(#46833,#46834,#46835));
#18435=EDGE_LOOP('',(#46836,#46837,#46838,#46839));
#18436=EDGE_LOOP('',(#46840,#46841,#46842));
#18437=EDGE_LOOP('',(#46843,#46844,#46845,#46846));
#18438=EDGE_LOOP('',(#46847,#46848,#46849));
#18439=EDGE_LOOP('',(#46850,#46851,#46852,#46853));
#18440=EDGE_LOOP('',(#46854,#46855,#46856));
#18441=EDGE_LOOP('',(#46857,#46858,#46859,#46860));
#18442=EDGE_LOOP('',(#46861,#46862,#46863));
#18443=EDGE_LOOP('',(#46864,#46865,#46866,#46867));
#18444=EDGE_LOOP('',(#46868,#46869,#46870));
#18445=EDGE_LOOP('',(#46871,#46872,#46873,#46874));
#18446=EDGE_LOOP('',(#46875,#46876,#46877));
#18447=EDGE_LOOP('',(#46878,#46879,#46880,#46881));
#18448=EDGE_LOOP('',(#46882,#46883,#46884));
#18449=EDGE_LOOP('',(#46885,#46886,#46887,#46888));
#18450=EDGE_LOOP('',(#46889,#46890,#46891));
#18451=EDGE_LOOP('',(#46892,#46893,#46894,#46895));
#18452=EDGE_LOOP('',(#46896,#46897,#46898));
#18453=EDGE_LOOP('',(#46899,#46900,#46901,#46902));
#18454=EDGE_LOOP('',(#46903,#46904,#46905));
#18455=EDGE_LOOP('',(#46906,#46907,#46908,#46909));
#18456=EDGE_LOOP('',(#46910,#46911,#46912));
#18457=EDGE_LOOP('',(#46913,#46914,#46915,#46916));
#18458=EDGE_LOOP('',(#46917,#46918,#46919));
#18459=EDGE_LOOP('',(#46920,#46921,#46922,#46923));
#18460=EDGE_LOOP('',(#46924,#46925,#46926));
#18461=EDGE_LOOP('',(#46927,#46928,#46929,#46930));
#18462=EDGE_LOOP('',(#46931,#46932,#46933));
#18463=EDGE_LOOP('',(#46934,#46935,#46936,#46937));
#18464=EDGE_LOOP('',(#46938,#46939,#46940));
#18465=EDGE_LOOP('',(#46941,#46942,#46943,#46944));
#18466=EDGE_LOOP('',(#46945,#46946,#46947));
#18467=EDGE_LOOP('',(#46948,#46949,#46950,#46951));
#18468=EDGE_LOOP('',(#46952,#46953,#46954));
#18469=EDGE_LOOP('',(#46955,#46956,#46957,#46958));
#18470=EDGE_LOOP('',(#46959,#46960,#46961));
#18471=EDGE_LOOP('',(#46962,#46963,#46964,#46965));
#18472=EDGE_LOOP('',(#46966,#46967,#46968));
#18473=EDGE_LOOP('',(#46969,#46970,#46971,#46972));
#18474=EDGE_LOOP('',(#46973,#46974,#46975));
#18475=EDGE_LOOP('',(#46976,#46977,#46978,#46979));
#18476=EDGE_LOOP('',(#46980,#46981,#46982));
#18477=EDGE_LOOP('',(#46983,#46984,#46985,#46986));
#18478=EDGE_LOOP('',(#46987,#46988,#46989));
#18479=EDGE_LOOP('',(#46990,#46991,#46992,#46993));
#18480=EDGE_LOOP('',(#46994,#46995,#46996));
#18481=EDGE_LOOP('',(#46997,#46998,#46999,#47000));
#18482=EDGE_LOOP('',(#47001,#47002,#47003));
#18483=EDGE_LOOP('',(#47004,#47005,#47006,#47007));
#18484=EDGE_LOOP('',(#47008,#47009,#47010));
#18485=EDGE_LOOP('',(#47011,#47012,#47013,#47014));
#18486=EDGE_LOOP('',(#47015,#47016,#47017));
#18487=EDGE_LOOP('',(#47018,#47019,#47020,#47021));
#18488=EDGE_LOOP('',(#47022,#47023,#47024));
#18489=EDGE_LOOP('',(#47025,#47026,#47027,#47028));
#18490=EDGE_LOOP('',(#47029,#47030,#47031));
#18491=EDGE_LOOP('',(#47032,#47033,#47034,#47035));
#18492=EDGE_LOOP('',(#47036,#47037,#47038));
#18493=EDGE_LOOP('',(#47039,#47040,#47041,#47042));
#18494=EDGE_LOOP('',(#47043,#47044,#47045));
#18495=EDGE_LOOP('',(#47046,#47047,#47048,#47049));
#18496=EDGE_LOOP('',(#47050,#47051,#47052));
#18497=EDGE_LOOP('',(#47053,#47054,#47055,#47056));
#18498=EDGE_LOOP('',(#47057,#47058,#47059,#47060));
#18499=EDGE_LOOP('',(#47061,#47062,#47063,#47064));
#18500=EDGE_LOOP('',(#47065,#47066,#47067,#47068));
#18501=EDGE_LOOP('',(#47069,#47070,#47071,#47072));
#18502=EDGE_LOOP('',(#47073,#47074,#47075));
#18503=EDGE_LOOP('',(#47076,#47077,#47078,#47079));
#18504=EDGE_LOOP('',(#47080,#47081,#47082));
#18505=EDGE_LOOP('',(#47083,#47084,#47085,#47086));
#18506=EDGE_LOOP('',(#47087,#47088,#47089));
#18507=EDGE_LOOP('',(#47090,#47091,#47092,#47093));
#18508=EDGE_LOOP('',(#47094,#47095,#47096));
#18509=EDGE_LOOP('',(#47097,#47098,#47099,#47100));
#18510=EDGE_LOOP('',(#47101,#47102,#47103));
#18511=EDGE_LOOP('',(#47104,#47105,#47106,#47107));
#18512=EDGE_LOOP('',(#47108,#47109,#47110));
#18513=EDGE_LOOP('',(#47111,#47112,#47113,#47114));
#18514=EDGE_LOOP('',(#47115,#47116,#47117));
#18515=EDGE_LOOP('',(#47118,#47119,#47120,#47121));
#18516=EDGE_LOOP('',(#47122,#47123,#47124));
#18517=EDGE_LOOP('',(#47125,#47126,#47127,#47128));
#18518=EDGE_LOOP('',(#47129,#47130,#47131));
#18519=EDGE_LOOP('',(#47132,#47133,#47134,#47135));
#18520=EDGE_LOOP('',(#47136,#47137,#47138));
#18521=EDGE_LOOP('',(#47139,#47140,#47141,#47142));
#18522=EDGE_LOOP('',(#47143,#47144,#47145));
#18523=EDGE_LOOP('',(#47146,#47147,#47148,#47149));
#18524=EDGE_LOOP('',(#47150,#47151,#47152));
#18525=EDGE_LOOP('',(#47153,#47154,#47155,#47156));
#18526=EDGE_LOOP('',(#47157,#47158,#47159));
#18527=EDGE_LOOP('',(#47160,#47161,#47162,#47163));
#18528=EDGE_LOOP('',(#47164,#47165,#47166));
#18529=EDGE_LOOP('',(#47167,#47168,#47169,#47170));
#18530=EDGE_LOOP('',(#47171,#47172,#47173));
#18531=EDGE_LOOP('',(#47174,#47175,#47176,#47177));
#18532=EDGE_LOOP('',(#47178,#47179,#47180));
#18533=EDGE_LOOP('',(#47181,#47182,#47183,#47184));
#18534=EDGE_LOOP('',(#47185,#47186,#47187));
#18535=EDGE_LOOP('',(#47188,#47189,#47190,#47191));
#18536=EDGE_LOOP('',(#47192,#47193,#47194));
#18537=EDGE_LOOP('',(#47195,#47196,#47197,#47198));
#18538=EDGE_LOOP('',(#47199,#47200,#47201));
#18539=EDGE_LOOP('',(#47202,#47203,#47204,#47205));
#18540=EDGE_LOOP('',(#47206,#47207,#47208));
#18541=EDGE_LOOP('',(#47209,#47210,#47211,#47212));
#18542=EDGE_LOOP('',(#47213,#47214,#47215));
#18543=EDGE_LOOP('',(#47216,#47217,#47218,#47219));
#18544=EDGE_LOOP('',(#47220,#47221,#47222));
#18545=EDGE_LOOP('',(#47223,#47224,#47225,#47226));
#18546=EDGE_LOOP('',(#47227,#47228,#47229));
#18547=EDGE_LOOP('',(#47230,#47231,#47232,#47233));
#18548=EDGE_LOOP('',(#47234,#47235,#47236));
#18549=EDGE_LOOP('',(#47237,#47238,#47239,#47240));
#18550=EDGE_LOOP('',(#47241,#47242,#47243));
#18551=EDGE_LOOP('',(#47244,#47245,#47246,#47247));
#18552=EDGE_LOOP('',(#47248,#47249,#47250));
#18553=EDGE_LOOP('',(#47251,#47252,#47253,#47254));
#18554=EDGE_LOOP('',(#47255,#47256,#47257));
#18555=EDGE_LOOP('',(#47258,#47259,#47260,#47261));
#18556=EDGE_LOOP('',(#47262,#47263,#47264));
#18557=EDGE_LOOP('',(#47265,#47266,#47267,#47268));
#18558=EDGE_LOOP('',(#47269,#47270,#47271));
#18559=EDGE_LOOP('',(#47272,#47273,#47274,#47275));
#18560=EDGE_LOOP('',(#47276,#47277,#47278));
#18561=EDGE_LOOP('',(#47279,#47280,#47281,#47282));
#18562=EDGE_LOOP('',(#47283,#47284,#47285));
#18563=EDGE_LOOP('',(#47286,#47287,#47288,#47289));
#18564=EDGE_LOOP('',(#47290,#47291,#47292));
#18565=EDGE_LOOP('',(#47293,#47294,#47295,#47296));
#18566=EDGE_LOOP('',(#47297,#47298,#47299));
#18567=EDGE_LOOP('',(#47300,#47301,#47302,#47303));
#18568=EDGE_LOOP('',(#47304,#47305,#47306));
#18569=EDGE_LOOP('',(#47307,#47308,#47309));
#18570=EDGE_LOOP('',(#47310,#47311,#47312,#47313));
#18571=EDGE_LOOP('',(#47314,#47315,#47316,#47317));
#18572=EDGE_LOOP('',(#47318,#47319,#47320));
#18573=EDGE_LOOP('',(#47321,#47322,#47323));
#18574=EDGE_LOOP('',(#47324,#47325,#47326,#47327));
#18575=EDGE_LOOP('',(#47328,#47329,#47330,#47331));
#18576=EDGE_LOOP('',(#47332,#47333,#47334,#47335));
#18577=EDGE_LOOP('',(#47336,#47337,#47338,#47339));
#18578=EDGE_LOOP('',(#47340,#47341,#47342,#47343));
#18579=EDGE_LOOP('',(#47344,#47345,#47346,#47347));
#18580=EDGE_LOOP('',(#47348,#47349,#47350,#47351,#47352,#47353));
#18581=EDGE_LOOP('',(#47354));
#18582=EDGE_LOOP('',(#47355));
#18583=EDGE_LOOP('',(#47356,#47357,#47358,#47359,#47360,#47361));
#18584=EDGE_LOOP('',(#47362,#47363,#47364,#47365,#47366,#47367,#47368,#47369,
#47370,#47371,#47372,#47373,#47374,#47375,#47376,#47377,#47378,#47379,#47380,
#47381,#47382,#47383,#47384,#47385,#47386,#47387,#47388,#47389,#47390,#47391,
#47392,#47393,#47394,#47395,#47396,#47397,#47398,#47399,#47400,#47401,#47402,
#47403,#47404,#47405,#47406,#47407,#47408,#47409,#47410,#47411,#47412,#47413,
#47414,#47415,#47416,#47417,#47418,#47419,#47420,#47421,#47422,#47423,#47424,
#47425,#47426,#47427,#47428,#47429,#47430,#47431,#47432,#47433,#47434,#47435,
#47436,#47437,#47438,#47439,#47440,#47441,#47442,#47443,#47444,#47445,#47446,
#47447,#47448,#47449,#47450,#47451,#47452,#47453,#47454,#47455,#47456,#47457,
#47458,#47459,#47460,#47461,#47462,#47463,#47464,#47465,#47466,#47467,#47468,
#47469,#47470,#47471,#47472,#47473,#47474,#47475,#47476,#47477,#47478,#47479,
#47480,#47481,#47482,#47483,#47484,#47485,#47486,#47487,#47488,#47489,#47490,
#47491,#47492,#47493,#47494,#47495,#47496,#47497,#47498,#47499,#47500,#47501,
#47502,#47503,#47504,#47505,#47506,#47507,#47508,#47509));
#18585=EDGE_LOOP('',(#47510,#47511,#47512,#47513,#47514,#47515,#47516,#47517,
#47518,#47519,#47520,#47521,#47522,#47523,#47524,#47525,#47526,#47527,#47528,
#47529,#47530,#47531,#47532,#47533,#47534,#47535,#47536,#47537,#47538,#47539,
#47540,#47541,#47542,#47543,#47544,#47545,#47546,#47547,#47548,#47549,#47550,
#47551,#47552,#47553,#47554,#47555,#47556,#47557,#47558,#47559,#47560,#47561,
#47562,#47563,#47564,#47565,#47566,#47567,#47568,#47569,#47570,#47571,#47572,
#47573,#47574,#47575,#47576,#47577,#47578,#47579,#47580,#47581,#47582,#47583,
#47584,#47585));
#18586=EDGE_LOOP('',(#47586));
#18587=EDGE_LOOP('',(#47587,#47588,#47589,#47590,#47591,#47592));
#18588=EDGE_LOOP('',(#47593,#47594,#47595,#47596,#47597));
#18589=EDGE_LOOP('',(#47598,#47599,#47600,#47601,#47602));
#18590=EDGE_LOOP('',(#47603));
#18591=EDGE_LOOP('',(#47604));
#18592=EDGE_LOOP('',(#47605,#47606,#47607,#47608));
#18593=EDGE_LOOP('',(#47609,#47610,#47611,#47612));
#18594=EDGE_LOOP('',(#47613,#47614,#47615,#47616));
#18595=EDGE_LOOP('',(#47617,#47618,#47619,#47620));
#18596=EDGE_LOOP('',(#47621,#47622,#47623,#47624));
#18597=EDGE_LOOP('',(#47625,#47626,#47627,#47628));
#18598=EDGE_LOOP('',(#47629,#47630,#47631,#47632));
#18599=EDGE_LOOP('',(#47633,#47634,#47635,#47636));
#18600=EDGE_LOOP('',(#47637,#47638,#47639,#47640));
#18601=EDGE_LOOP('',(#47641,#47642,#47643,#47644));
#18602=EDGE_LOOP('',(#47645,#47646,#47647,#47648));
#18603=EDGE_LOOP('',(#47649,#47650,#47651,#47652));
#18604=EDGE_LOOP('',(#47653,#47654,#47655,#47656));
#18605=EDGE_LOOP('',(#47657,#47658,#47659,#47660));
#18606=EDGE_LOOP('',(#47661,#47662,#47663,#47664));
#18607=EDGE_LOOP('',(#47665,#47666,#47667,#47668));
#18608=EDGE_LOOP('',(#47669,#47670,#47671,#47672));
#18609=EDGE_LOOP('',(#47673,#47674,#47675,#47676));
#18610=EDGE_LOOP('',(#47677,#47678,#47679,#47680));
#18611=EDGE_LOOP('',(#47681,#47682,#47683,#47684));
#18612=EDGE_LOOP('',(#47685,#47686,#47687,#47688));
#18613=EDGE_LOOP('',(#47689,#47690,#47691,#47692));
#18614=EDGE_LOOP('',(#47693,#47694,#47695,#47696));
#18615=EDGE_LOOP('',(#47697,#47698,#47699,#47700));
#18616=EDGE_LOOP('',(#47701,#47702,#47703,#47704));
#18617=EDGE_LOOP('',(#47705,#47706,#47707,#47708));
#18618=EDGE_LOOP('',(#47709,#47710,#47711,#47712));
#18619=EDGE_LOOP('',(#47713,#47714,#47715,#47716));
#18620=EDGE_LOOP('',(#47717,#47718,#47719,#47720));
#18621=EDGE_LOOP('',(#47721,#47722,#47723,#47724));
#18622=EDGE_LOOP('',(#47725,#47726,#47727,#47728));
#18623=EDGE_LOOP('',(#47729,#47730,#47731,#47732));
#18624=EDGE_LOOP('',(#47733,#47734,#47735,#47736));
#18625=EDGE_LOOP('',(#47737,#47738,#47739,#47740));
#18626=EDGE_LOOP('',(#47741,#47742,#47743,#47744));
#18627=EDGE_LOOP('',(#47745,#47746,#47747,#47748));
#18628=EDGE_LOOP('',(#47749,#47750,#47751,#47752));
#18629=EDGE_LOOP('',(#47753,#47754,#47755,#47756));
#18630=EDGE_LOOP('',(#47757,#47758,#47759,#47760));
#18631=EDGE_LOOP('',(#47761,#47762,#47763,#47764));
#18632=EDGE_LOOP('',(#47765,#47766,#47767,#47768));
#18633=EDGE_LOOP('',(#47769,#47770,#47771,#47772));
#18634=EDGE_LOOP('',(#47773,#47774,#47775,#47776));
#18635=EDGE_LOOP('',(#47777,#47778,#47779,#47780));
#18636=EDGE_LOOP('',(#47781,#47782,#47783,#47784));
#18637=EDGE_LOOP('',(#47785,#47786,#47787,#47788));
#18638=EDGE_LOOP('',(#47789,#47790,#47791,#47792));
#18639=EDGE_LOOP('',(#47793,#47794,#47795,#47796));
#18640=EDGE_LOOP('',(#47797,#47798,#47799,#47800,#47801));
#18641=EDGE_LOOP('',(#47802,#47803,#47804,#47805,#47806,#47807,#47808,#47809,
#47810,#47811,#47812,#47813,#47814,#47815,#47816,#47817,#47818,#47819,#47820,
#47821,#47822,#47823,#47824,#47825,#47826,#47827,#47828,#47829,#47830,#47831,
#47832,#47833,#47834,#47835,#47836,#47837,#47838,#47839,#47840,#47841,#47842,
#47843,#47844,#47845,#47846,#47847,#47848,#47849,#47850,#47851));
#18642=EDGE_LOOP('',(#47852,#47853,#47854,#47855,#47856));
#18643=EDGE_LOOP('',(#47857,#47858,#47859,#47860));
#18644=EDGE_LOOP('',(#47861,#47862,#47863,#47864,#47865,#47866,#47867,#47868,
#47869,#47870,#47871,#47872,#47873,#47874,#47875,#47876,#47877,#47878,#47879,
#47880,#47881,#47882,#47883,#47884,#47885,#47886,#47887,#47888,#47889,#47890,
#47891,#47892,#47893,#47894,#47895,#47896,#47897,#47898,#47899,#47900,#47901,
#47902,#47903,#47904,#47905,#47906,#47907,#47908,#47909,#47910));
#18645=EDGE_LOOP('',(#47911,#47912,#47913,#47914,#47915,#47916));
#18646=EDGE_LOOP('',(#47917,#47918,#47919,#47920));
#18647=EDGE_LOOP('',(#47921));
#18648=EDGE_LOOP('',(#47922));
#18649=EDGE_LOOP('',(#47923,#47924,#47925,#47926,#47927,#47928,#47929,#47930,
#47931));
#18650=EDGE_LOOP('',(#47932,#47933,#47934,#47935));
#18651=EDGE_LOOP('',(#47936,#47937,#47938,#47939));
#18652=EDGE_LOOP('',(#47940,#47941,#47942,#47943));
#18653=EDGE_LOOP('',(#47944,#47945,#47946,#47947));
#18654=EDGE_LOOP('',(#47948));
#18655=EDGE_LOOP('',(#47949,#47950,#47951,#47952,#47953,#47954));
#18656=EDGE_LOOP('',(#47955,#47956,#47957,#47958));
#18657=EDGE_LOOP('',(#47959,#47960,#47961,#47962));
#18658=EDGE_LOOP('',(#47963,#47964,#47965,#47966));
#18659=EDGE_LOOP('',(#47967));
#18660=EDGE_LOOP('',(#47968,#47969,#47970,#47971,#47972,#47973));
#18661=EDGE_LOOP('',(#47974));
#18662=EDGE_LOOP('',(#47975,#47976,#47977,#47978));
#18663=EDGE_LOOP('',(#47979,#47980,#47981,#47982));
#18664=EDGE_LOOP('',(#47983,#47984,#47985,#47986));
#18665=EDGE_LOOP('',(#47987));
#18666=EDGE_LOOP('',(#47988));
#18667=EDGE_LOOP('',(#47989,#47990,#47991,#47992));
#18668=EDGE_LOOP('',(#47993,#47994,#47995,#47996));
#18669=EDGE_LOOP('',(#47997,#47998,#47999,#48000));
#18670=EDGE_LOOP('',(#48001));
#18671=EDGE_LOOP('',(#48002));
#18672=EDGE_LOOP('',(#48003,#48004,#48005,#48006));
#18673=EDGE_LOOP('',(#48007,#48008,#48009,#48010,#48011,#48012,#48013,#48014));
#18674=EDGE_LOOP('',(#48015,#48016,#48017,#48018,#48019,#48020,#48021,#48022));
#18675=EDGE_LOOP('',(#48023,#48024,#48025,#48026,#48027));
#18676=EDGE_LOOP('',(#48028,#48029,#48030,#48031));
#18677=EDGE_LOOP('',(#48032,#48033,#48034,#48035,#48036));
#18678=EDGE_LOOP('',(#48037,#48038,#48039,#48040));
#18679=EDGE_LOOP('',(#48041,#48042,#48043,#48044));
#18680=EDGE_LOOP('',(#48045,#48046,#48047,#48048));
#18681=EDGE_LOOP('',(#48049,#48050,#48051,#48052));
#18682=EDGE_LOOP('',(#48053,#48054,#48055,#48056));
#18683=EDGE_LOOP('',(#48057,#48058,#48059,#48060));
#18684=EDGE_LOOP('',(#48061,#48062,#48063,#48064));
#18685=EDGE_LOOP('',(#48065,#48066,#48067,#48068));
#18686=EDGE_LOOP('',(#48069,#48070,#48071,#48072,#48073,#48074,#48075,#48076,
#48077));
#18687=EDGE_LOOP('',(#48078,#48079,#48080,#48081));
#18688=EDGE_LOOP('',(#48082,#48083,#48084,#48085));
#18689=EDGE_LOOP('',(#48086,#48087,#48088,#48089));
#18690=EDGE_LOOP('',(#48090,#48091,#48092,#48093,#48094,#48095,#48096,#48097,
#48098));
#18691=EDGE_LOOP('',(#48099,#48100,#48101,#48102));
#18692=EDGE_LOOP('',(#48103,#48104,#48105,#48106));
#18693=EDGE_LOOP('',(#48107,#48108,#48109,#48110));
#18694=EDGE_LOOP('',(#48111));
#18695=EDGE_LOOP('',(#48112));
#18696=EDGE_LOOP('',(#48113));
#18697=EDGE_LOOP('',(#48114));
#18698=(
BOUNDED_CURVE()
B_SPLINE_CURVE(2,(#68265,#68266,#68267),.UNSPECIFIED.,.F.,.F.)
B_SPLINE_CURVE_WITH_KNOTS((3,3),(0.0522192481407972,0.300149053231598),
 .UNSPECIFIED.)
CURVE()
GEOMETRIC_REPRESENTATION_ITEM()
RATIONAL_B_SPLINE_CURVE((1.00002415803342,1.00006942852605,1.))
REPRESENTATION_ITEM('')
);
#18699=(
BOUNDED_CURVE()
B_SPLINE_CURVE(2,(#68269,#68270,#68271),.UNSPECIFIED.,.F.,.F.)
B_SPLINE_CURVE_WITH_KNOTS((3,3),(0.98462316632217,1.26677639839307),
 .UNSPECIFIED.)
CURVE()
GEOMETRIC_REPRESENTATION_ITEM()
RATIONAL_B_SPLINE_CURVE((1.02072197947249,1.0213832836854,1.02072197947249))
REPRESENTATION_ITEM('')
);
#18700=(
BOUNDED_CURVE()
B_SPLINE_CURVE(2,(#68272,#68273,#68274),.UNSPECIFIED.,.F.,.F.)
B_SPLINE_CURVE_WITH_KNOTS((3,3),(0.,0.247929805090986),.UNSPECIFIED.)
CURVE()
GEOMETRIC_REPRESENTATION_ITEM()
RATIONAL_B_SPLINE_CURVE((1.,1.0000694285291,1.00002415803448))
REPRESENTATION_ITEM('')
);
#18701=(
BOUNDED_CURVE()
B_SPLINE_CURVE(2,(#68280,#68281,#68282),.UNSPECIFIED.,.F.,.F.)
B_SPLINE_CURVE_WITH_KNOTS((3,3),(0.0522192481407795,0.300149053231598),
 .UNSPECIFIED.)
CURVE()
GEOMETRIC_REPRESENTATION_ITEM()
RATIONAL_B_SPLINE_CURVE((1.00002415803391,1.00006942852745,1.))
REPRESENTATION_ITEM('')
);
#18702=(
BOUNDED_CURVE()
B_SPLINE_CURVE(2,(#68284,#68285,#68286),.UNSPECIFIED.,.F.,.F.)
B_SPLINE_CURVE_WITH_KNOTS((3,3),(0.984623166322172,1.26677639839308),
 .UNSPECIFIED.)
CURVE()
GEOMETRIC_REPRESENTATION_ITEM()
RATIONAL_B_SPLINE_CURVE((1.02072197947249,1.02138328368541,1.02072197947249))
REPRESENTATION_ITEM('')
);
#18703=(
BOUNDED_CURVE()
B_SPLINE_CURVE(2,(#68287,#68288,#68289),.UNSPECIFIED.,.F.,.F.)
B_SPLINE_CURVE_WITH_KNOTS((3,3),(0.,0.247929805090959),.UNSPECIFIED.)
CURVE()
GEOMETRIC_REPRESENTATION_ITEM()
RATIONAL_B_SPLINE_CURVE((1.,1.00006942853144,1.0000241580353))
REPRESENTATION_ITEM('')
);
#18704=(
BOUNDED_CURVE()
B_SPLINE_CURVE(2,(#68295,#68296,#68297),.UNSPECIFIED.,.F.,.F.)
B_SPLINE_CURVE_WITH_KNOTS((3,3),(0.0522192481406614,0.300149053231599),
 .UNSPECIFIED.)
CURVE()
GEOMETRIC_REPRESENTATION_ITEM()
RATIONAL_B_SPLINE_CURVE((1.00002415803474,1.00006942852983,1.))
REPRESENTATION_ITEM('')
);
#18705=(
BOUNDED_CURVE()
B_SPLINE_CURVE(2,(#68299,#68300,#68301),.UNSPECIFIED.,.F.,.F.)
B_SPLINE_CURVE_WITH_KNOTS((3,3),(0.984623166322172,1.26677639839307),
 .UNSPECIFIED.)
CURVE()
GEOMETRIC_REPRESENTATION_ITEM()
RATIONAL_B_SPLINE_CURVE((1.02072197947249,1.02138328368541,1.02072197947249))
REPRESENTATION_ITEM('')
);
#18706=(
BOUNDED_CURVE()
B_SPLINE_CURVE(2,(#68302,#68303,#68304),.UNSPECIFIED.,.F.,.F.)
B_SPLINE_CURVE_WITH_KNOTS((3,3),(0.,0.247929805090876),.UNSPECIFIED.)
CURVE()
GEOMETRIC_REPRESENTATION_ITEM()
RATIONAL_B_SPLINE_CURVE((1.,1.00006942852873,1.00002415803435))
REPRESENTATION_ITEM('')
);
#18707=(
BOUNDED_CURVE()
B_SPLINE_CURVE(2,(#68310,#68311,#68312),.UNSPECIFIED.,.F.,.F.)
B_SPLINE_CURVE_WITH_KNOTS((3,3),(0.0522192481406224,0.300149053231599),
 .UNSPECIFIED.)
CURVE()
GEOMETRIC_REPRESENTATION_ITEM()
RATIONAL_B_SPLINE_CURVE((1.00002415803453,1.00006942852923,1.))
REPRESENTATION_ITEM('')
);
#18708=(
BOUNDED_CURVE()
B_SPLINE_CURVE(2,(#68314,#68315,#68316),.UNSPECIFIED.,.F.,.F.)
B_SPLINE_CURVE_WITH_KNOTS((3,3),(0.984623166322173,1.26677639839308),
 .UNSPECIFIED.)
CURVE()
GEOMETRIC_REPRESENTATION_ITEM()
RATIONAL_B_SPLINE_CURVE((1.02072197947249,1.02138328368541,1.02072197947249))
REPRESENTATION_ITEM('')
);
#18709=(
BOUNDED_CURVE()
B_SPLINE_CURVE(2,(#68317,#68318,#68319),.UNSPECIFIED.,.F.,.F.)
B_SPLINE_CURVE_WITH_KNOTS((3,3),(0.,0.247929805090936),.UNSPECIFIED.)
CURVE()
GEOMETRIC_REPRESENTATION_ITEM()
RATIONAL_B_SPLINE_CURVE((1.,1.00006942853044,1.00002415803495))
REPRESENTATION_ITEM('')
);
#18710=(
BOUNDED_CURVE()
B_SPLINE_CURVE(2,(#68325,#68326,#68327),.UNSPECIFIED.,.F.,.F.)
B_SPLINE_CURVE_WITH_KNOTS((3,3),(0.0522192481406471,0.300149053231599),
 .UNSPECIFIED.)
CURVE()
GEOMETRIC_REPRESENTATION_ITEM()
RATIONAL_B_SPLINE_CURVE((1.00002415803429,1.00006942852855,1.))
REPRESENTATION_ITEM('')
);
#18711=(
BOUNDED_CURVE()
B_SPLINE_CURVE(2,(#68329,#68330,#68331),.UNSPECIFIED.,.F.,.F.)
B_SPLINE_CURVE_WITH_KNOTS((3,3),(0.98462316632217,1.26677639839307),
 .UNSPECIFIED.)
CURVE()
GEOMETRIC_REPRESENTATION_ITEM()
RATIONAL_B_SPLINE_CURVE((1.02072197947249,1.02138328368541,1.02072197947249))
REPRESENTATION_ITEM('')
);
#18712=(
BOUNDED_CURVE()
B_SPLINE_CURVE(2,(#68332,#68333,#68334),.UNSPECIFIED.,.F.,.F.)
B_SPLINE_CURVE_WITH_KNOTS((3,3),(0.,0.247929805090895),.UNSPECIFIED.)
CURVE()
GEOMETRIC_REPRESENTATION_ITEM()
RATIONAL_B_SPLINE_CURVE((1.,1.000069428528,1.0000241580341))
REPRESENTATION_ITEM('')
);
#18713=(
BOUNDED_CURVE()
B_SPLINE_CURVE(2,(#68340,#68341,#68342),.UNSPECIFIED.,.F.,.F.)
B_SPLINE_CURVE_WITH_KNOTS((3,3),(0.0522192481406872,0.300149053231598),
 .UNSPECIFIED.)
CURVE()
GEOMETRIC_REPRESENTATION_ITEM()
RATIONAL_B_SPLINE_CURVE((1.00002415803456,1.00006942852931,1.))
REPRESENTATION_ITEM('')
);
#18714=(
BOUNDED_CURVE()
B_SPLINE_CURVE(2,(#68344,#68345,#68346),.UNSPECIFIED.,.F.,.F.)
B_SPLINE_CURVE_WITH_KNOTS((3,3),(0.984623166322171,1.26677639839307),
 .UNSPECIFIED.)
CURVE()
GEOMETRIC_REPRESENTATION_ITEM()
RATIONAL_B_SPLINE_CURVE((1.02072197947249,1.02138328368541,1.02072197947249))
REPRESENTATION_ITEM('')
);
#18715=(
BOUNDED_CURVE()
B_SPLINE_CURVE(2,(#68347,#68348,#68349),.UNSPECIFIED.,.F.,.F.)
B_SPLINE_CURVE_WITH_KNOTS((3,3),(0.,0.247929805090952),.UNSPECIFIED.)
CURVE()
GEOMETRIC_REPRESENTATION_ITEM()
RATIONAL_B_SPLINE_CURVE((1.,1.00006942852864,1.00002415803432))
REPRESENTATION_ITEM('')
);
#18716=(
BOUNDED_CURVE()
B_SPLINE_CURVE(2,(#68355,#68356,#68357),.UNSPECIFIED.,.F.,.F.)
B_SPLINE_CURVE_WITH_KNOTS((3,3),(0.0522192481406724,0.300149053231598),
 .UNSPECIFIED.)
CURVE()
GEOMETRIC_REPRESENTATION_ITEM()
RATIONAL_B_SPLINE_CURVE((1.00002415803439,1.00006942852885,1.))
REPRESENTATION_ITEM('')
);
#18717=(
BOUNDED_CURVE()
B_SPLINE_CURVE(2,(#68359,#68360,#68361),.UNSPECIFIED.,.F.,.F.)
B_SPLINE_CURVE_WITH_KNOTS((3,3),(0.984623166322169,1.26677639839307),
 .UNSPECIFIED.)
CURVE()
GEOMETRIC_REPRESENTATION_ITEM()
RATIONAL_B_SPLINE_CURVE((1.02072197947249,1.02138328368541,1.02072197947249))
REPRESENTATION_ITEM('')
);
#18718=(
BOUNDED_CURVE()
B_SPLINE_CURVE(2,(#68362,#68363,#68364),.UNSPECIFIED.,.F.,.F.)
B_SPLINE_CURVE_WITH_KNOTS((3,3),(0.,0.24792980509092),.UNSPECIFIED.)
CURVE()
GEOMETRIC_REPRESENTATION_ITEM()
RATIONAL_B_SPLINE_CURVE((1.,1.0000694285281,1.00002415803414))
REPRESENTATION_ITEM('')
);
#18719=(
BOUNDED_CURVE()
B_SPLINE_CURVE(2,(#68370,#68371,#68372),.UNSPECIFIED.,.F.,.F.)
B_SPLINE_CURVE_WITH_KNOTS((3,3),(0.0522192481407194,0.300149053231599),
 .UNSPECIFIED.)
CURVE()
GEOMETRIC_REPRESENTATION_ITEM()
RATIONAL_B_SPLINE_CURVE((1.00002415803445,1.00006942852901,1.))
REPRESENTATION_ITEM('')
);
#18720=(
BOUNDED_CURVE()
B_SPLINE_CURVE(2,(#68374,#68375,#68376),.UNSPECIFIED.,.F.,.F.)
B_SPLINE_CURVE_WITH_KNOTS((3,3),(0.984623166322171,1.26677639839307),
 .UNSPECIFIED.)
CURVE()
GEOMETRIC_REPRESENTATION_ITEM()
RATIONAL_B_SPLINE_CURVE((1.02072197947249,1.02138328368541,1.02072197947249))
REPRESENTATION_ITEM('')
);
#18721=(
BOUNDED_CURVE()
B_SPLINE_CURVE(2,(#68377,#68378,#68379),.UNSPECIFIED.,.F.,.F.)
B_SPLINE_CURVE_WITH_KNOTS((3,3),(0.,0.247929805090845),.UNSPECIFIED.)
CURVE()
GEOMETRIC_REPRESENTATION_ITEM()
RATIONAL_B_SPLINE_CURVE((1.,1.00006942852734,1.00002415803387))
REPRESENTATION_ITEM('')
);
#18722=(
BOUNDED_CURVE()
B_SPLINE_CURVE(2,(#68385,#68386,#68387),.UNSPECIFIED.,.F.,.F.)
B_SPLINE_CURVE_WITH_KNOTS((3,3),(0.0522192481406634,0.300149053231598),
 .UNSPECIFIED.)
CURVE()
GEOMETRIC_REPRESENTATION_ITEM()
RATIONAL_B_SPLINE_CURVE((1.00002415803422,1.00006942852834,1.))
REPRESENTATION_ITEM('')
);
#18723=(
BOUNDED_CURVE()
B_SPLINE_CURVE(2,(#68389,#68390,#68391),.UNSPECIFIED.,.F.,.F.)
B_SPLINE_CURVE_WITH_KNOTS((3,3),(0.984623166322172,1.26677639839307),
 .UNSPECIFIED.)
CURVE()
GEOMETRIC_REPRESENTATION_ITEM()
RATIONAL_B_SPLINE_CURVE((1.02072197947249,1.02138328368541,1.02072197947249))
REPRESENTATION_ITEM('')
);
#18724=(
BOUNDED_CURVE()
B_SPLINE_CURVE(2,(#68392,#68393,#68394),.UNSPECIFIED.,.F.,.F.)
B_SPLINE_CURVE_WITH_KNOTS((3,3),(0.,0.247929805090971),.UNSPECIFIED.)
CURVE()
GEOMETRIC_REPRESENTATION_ITEM()
RATIONAL_B_SPLINE_CURVE((1.,1.0000694285305,1.00002415803497))
REPRESENTATION_ITEM('')
);
#18725=(
BOUNDED_CURVE()
B_SPLINE_CURVE(2,(#68400,#68401,#68402),.UNSPECIFIED.,.F.,.F.)
B_SPLINE_CURVE_WITH_KNOTS((3,3),(0.052219248140715,0.300149053231599),
 .UNSPECIFIED.)
CURVE()
GEOMETRIC_REPRESENTATION_ITEM()
RATIONAL_B_SPLINE_CURVE((1.00002415803427,1.00006942852848,1.))
REPRESENTATION_ITEM('')
);
#18726=(
BOUNDED_CURVE()
B_SPLINE_CURVE(2,(#68404,#68405,#68406),.UNSPECIFIED.,.F.,.F.)
B_SPLINE_CURVE_WITH_KNOTS((3,3),(0.98462316632217,1.26677639839307),
 .UNSPECIFIED.)
CURVE()
GEOMETRIC_REPRESENTATION_ITEM()
RATIONAL_B_SPLINE_CURVE((1.02072197947249,1.0213832836854,1.02072197947249))
REPRESENTATION_ITEM('')
);
#18727=(
BOUNDED_CURVE()
B_SPLINE_CURVE(2,(#68407,#68408,#68409),.UNSPECIFIED.,.F.,.F.)
B_SPLINE_CURVE_WITH_KNOTS((3,3),(0.,0.247929805090914),.UNSPECIFIED.)
CURVE()
GEOMETRIC_REPRESENTATION_ITEM()
RATIONAL_B_SPLINE_CURVE((1.,1.00006942852705,1.00002415803377))
REPRESENTATION_ITEM('')
);
#18728=(
BOUNDED_CURVE()
B_SPLINE_CURVE(2,(#68415,#68416,#68417),.UNSPECIFIED.,.F.,.F.)
B_SPLINE_CURVE_WITH_KNOTS((3,3),(0.0522192481406779,0.300149053231598),
 .UNSPECIFIED.)
CURVE()
GEOMETRIC_REPRESENTATION_ITEM()
RATIONAL_B_SPLINE_CURVE((1.00002415803406,1.0000694285279,1.))
REPRESENTATION_ITEM('')
);
#18729=(
BOUNDED_CURVE()
B_SPLINE_CURVE(2,(#68419,#68420,#68421),.UNSPECIFIED.,.F.,.F.)
B_SPLINE_CURVE_WITH_KNOTS((3,3),(0.984623166322172,1.26677639839307),
 .UNSPECIFIED.)
CURVE()
GEOMETRIC_REPRESENTATION_ITEM()
RATIONAL_B_SPLINE_CURVE((1.02072197947249,1.02138328368541,1.02072197947249))
REPRESENTATION_ITEM('')
);
#18730=(
BOUNDED_CURVE()
B_SPLINE_CURVE(2,(#68422,#68423,#68424),.UNSPECIFIED.,.F.,.F.)
B_SPLINE_CURVE_WITH_KNOTS((3,3),(0.,0.247929805090857),.UNSPECIFIED.)
CURVE()
GEOMETRIC_REPRESENTATION_ITEM()
RATIONAL_B_SPLINE_CURVE((1.,1.00006942852857,1.0000241580343))
REPRESENTATION_ITEM('')
);
#18731=(
BOUNDED_CURVE()
B_SPLINE_CURVE(2,(#68430,#68431,#68432),.UNSPECIFIED.,.F.,.F.)
B_SPLINE_CURVE_WITH_KNOTS((3,3),(0.0522192481406934,0.300149053231599),
 .UNSPECIFIED.)
CURVE()
GEOMETRIC_REPRESENTATION_ITEM()
RATIONAL_B_SPLINE_CURVE((1.00002415803403,1.00006942852779,1.))
REPRESENTATION_ITEM('')
);
#18732=(
BOUNDED_CURVE()
B_SPLINE_CURVE(2,(#68434,#68435,#68436),.UNSPECIFIED.,.F.,.F.)
B_SPLINE_CURVE_WITH_KNOTS((3,3),(0.984623166322171,1.26677639839307),
 .UNSPECIFIED.)
CURVE()
GEOMETRIC_REPRESENTATION_ITEM()
RATIONAL_B_SPLINE_CURVE((1.02072197947249,1.02138328368541,1.02072197947249))
REPRESENTATION_ITEM('')
);
#18733=(
BOUNDED_CURVE()
B_SPLINE_CURVE(2,(#68437,#68438,#68439),.UNSPECIFIED.,.F.,.F.)
B_SPLINE_CURVE_WITH_KNOTS((3,3),(0.,0.247929805090923),.UNSPECIFIED.)
CURVE()
GEOMETRIC_REPRESENTATION_ITEM()
RATIONAL_B_SPLINE_CURVE((1.,1.00006942853014,1.00002415803484))
REPRESENTATION_ITEM('')
);
#18734=(
BOUNDED_CURVE()
B_SPLINE_CURVE(2,(#68445,#68446,#68447),.UNSPECIFIED.,.F.,.F.)
B_SPLINE_CURVE_WITH_KNOTS((3,3),(0.0522192481406993,0.300149053231599),
 .UNSPECIFIED.)
CURVE()
GEOMETRIC_REPRESENTATION_ITEM()
RATIONAL_B_SPLINE_CURVE((1.0000241580339,1.00006942852741,1.))
REPRESENTATION_ITEM('')
);
#18735=(
BOUNDED_CURVE()
B_SPLINE_CURVE(2,(#68449,#68450,#68451),.UNSPECIFIED.,.F.,.F.)
B_SPLINE_CURVE_WITH_KNOTS((3,3),(0.984623166322172,1.26677639839308),
 .UNSPECIFIED.)
CURVE()
GEOMETRIC_REPRESENTATION_ITEM()
RATIONAL_B_SPLINE_CURVE((1.02072197947249,1.02138328368541,1.02072197947249))
REPRESENTATION_ITEM('')
);
#18736=(
BOUNDED_CURVE()
B_SPLINE_CURVE(2,(#68452,#68453,#68454),.UNSPECIFIED.,.F.,.F.)
B_SPLINE_CURVE_WITH_KNOTS((3,3),(0.,0.247929805090912),.UNSPECIFIED.)
CURVE()
GEOMETRIC_REPRESENTATION_ITEM()
RATIONAL_B_SPLINE_CURVE((1.,1.00006942852758,1.00002415803395))
REPRESENTATION_ITEM('')
);
#18737=(
BOUNDED_CURVE()
B_SPLINE_CURVE(2,(#68460,#68461,#68462),.UNSPECIFIED.,.F.,.F.)
B_SPLINE_CURVE_WITH_KNOTS((3,3),(0.0522192481406619,0.300149053231598),
 .UNSPECIFIED.)
CURVE()
GEOMETRIC_REPRESENTATION_ITEM()
RATIONAL_B_SPLINE_CURVE((1.00002415803529,1.00006942853141,1.))
REPRESENTATION_ITEM('')
);
#18738=(
BOUNDED_CURVE()
B_SPLINE_CURVE(2,(#68464,#68465,#68466),.UNSPECIFIED.,.F.,.F.)
B_SPLINE_CURVE_WITH_KNOTS((3,3),(0.984623166322169,1.26677639839307),
 .UNSPECIFIED.)
CURVE()
GEOMETRIC_REPRESENTATION_ITEM()
RATIONAL_B_SPLINE_CURVE((1.02072197947249,1.02138328368541,1.02072197947249))
REPRESENTATION_ITEM('')
);
#18739=(
BOUNDED_CURVE()
B_SPLINE_CURVE(2,(#68467,#68468,#68469),.UNSPECIFIED.,.F.,.F.)
B_SPLINE_CURVE_WITH_KNOTS((3,3),(0.,0.247929805090904),.UNSPECIFIED.)
CURVE()
GEOMETRIC_REPRESENTATION_ITEM()
RATIONAL_B_SPLINE_CURVE((1.,1.00006942852951,1.00002415803463))
REPRESENTATION_ITEM('')
);
#18740=(
BOUNDED_CURVE()
B_SPLINE_CURVE(2,(#68475,#68476,#68477),.UNSPECIFIED.,.F.,.F.)
B_SPLINE_CURVE_WITH_KNOTS((3,3),(0.0522192481406167,0.300149053231598),
 .UNSPECIFIED.)
CURVE()
GEOMETRIC_REPRESENTATION_ITEM()
RATIONAL_B_SPLINE_CURVE((1.0000241580343,1.00006942852858,1.))
REPRESENTATION_ITEM('')
);
#18741=(
BOUNDED_CURVE()
B_SPLINE_CURVE(2,(#68479,#68480,#68481),.UNSPECIFIED.,.F.,.F.)
B_SPLINE_CURVE_WITH_KNOTS((3,3),(0.984623166322174,1.26677639839308),
 .UNSPECIFIED.)
CURVE()
GEOMETRIC_REPRESENTATION_ITEM()
RATIONAL_B_SPLINE_CURVE((1.02072197947249,1.02138328368541,1.02072197947249))
REPRESENTATION_ITEM('')
);
#18742=(
BOUNDED_CURVE()
B_SPLINE_CURVE(2,(#68482,#68483,#68484),.UNSPECIFIED.,.F.,.F.)
B_SPLINE_CURVE_WITH_KNOTS((3,3),(0.,0.247929805090943),.UNSPECIFIED.)
CURVE()
GEOMETRIC_REPRESENTATION_ITEM()
RATIONAL_B_SPLINE_CURVE((1.,1.0000694285289,1.00002415803441))
REPRESENTATION_ITEM('')
);
#18743=(
BOUNDED_CURVE()
B_SPLINE_CURVE(2,(#68490,#68491,#68492),.UNSPECIFIED.,.F.,.F.)
B_SPLINE_CURVE_WITH_KNOTS((3,3),(0.0522192481406359,0.300149053231599),
 .UNSPECIFIED.)
CURVE()
GEOMETRIC_REPRESENTATION_ITEM()
RATIONAL_B_SPLINE_CURVE((1.00002415803477,1.00006942852992,1.))
REPRESENTATION_ITEM('')
);
#18744=(
BOUNDED_CURVE()
B_SPLINE_CURVE(2,(#68494,#68495,#68496),.UNSPECIFIED.,.F.,.F.)
B_SPLINE_CURVE_WITH_KNOTS((3,3),(0.984623166322174,1.26677639839308),
 .UNSPECIFIED.)
CURVE()
GEOMETRIC_REPRESENTATION_ITEM()
RATIONAL_B_SPLINE_CURVE((1.02072197947249,1.0213832836854,1.02072197947249))
REPRESENTATION_ITEM('')
);
#18745=(
BOUNDED_CURVE()
B_SPLINE_CURVE(2,(#68497,#68498,#68499),.UNSPECIFIED.,.F.,.F.)
B_SPLINE_CURVE_WITH_KNOTS((3,3),(0.,0.247929805090921),.UNSPECIFIED.)
CURVE()
GEOMETRIC_REPRESENTATION_ITEM()
RATIONAL_B_SPLINE_CURVE((1.,1.00006942852933,1.00002415803456))
REPRESENTATION_ITEM('')
);
#18746=(
BOUNDED_CURVE()
B_SPLINE_CURVE(2,(#68505,#68506,#68507),.UNSPECIFIED.,.F.,.F.)
B_SPLINE_CURVE_WITH_KNOTS((3,3),(0.052219248140584,0.300149053231599),
 .UNSPECIFIED.)
CURVE()
GEOMETRIC_REPRESENTATION_ITEM()
RATIONAL_B_SPLINE_CURVE((1.00002415803526,1.00006942853134,1.))
REPRESENTATION_ITEM('')
);
#18747=(
BOUNDED_CURVE()
B_SPLINE_CURVE(2,(#68509,#68510,#68511),.UNSPECIFIED.,.F.,.F.)
B_SPLINE_CURVE_WITH_KNOTS((3,3),(0.984623166322171,1.26677639839308),
 .UNSPECIFIED.)
CURVE()
GEOMETRIC_REPRESENTATION_ITEM()
RATIONAL_B_SPLINE_CURVE((1.02072197947249,1.02138328368541,1.02072197947249))
REPRESENTATION_ITEM('')
);
#18748=(
BOUNDED_CURVE()
B_SPLINE_CURVE(2,(#68512,#68513,#68514),.UNSPECIFIED.,.F.,.F.)
B_SPLINE_CURVE_WITH_KNOTS((3,3),(0.,0.247929805090749),.UNSPECIFIED.)
CURVE()
GEOMETRIC_REPRESENTATION_ITEM()
RATIONAL_B_SPLINE_CURVE((1.,1.0000694285275,1.00002415803393))
REPRESENTATION_ITEM('')
);
#18749=(
BOUNDED_CURVE()
B_SPLINE_CURVE(2,(#68520,#68521,#68522),.UNSPECIFIED.,.F.,.F.)
B_SPLINE_CURVE_WITH_KNOTS((3,3),(0.0522192481406365,0.300149053231598),
 .UNSPECIFIED.)
CURVE()
GEOMETRIC_REPRESENTATION_ITEM()
RATIONAL_B_SPLINE_CURVE((1.00002415803451,1.00006942852916,1.))
REPRESENTATION_ITEM('')
);
#18750=(
BOUNDED_CURVE()
B_SPLINE_CURVE(2,(#68524,#68525,#68526),.UNSPECIFIED.,.F.,.F.)
B_SPLINE_CURVE_WITH_KNOTS((3,3),(0.984623166322172,1.26677639839307),
 .UNSPECIFIED.)
CURVE()
GEOMETRIC_REPRESENTATION_ITEM()
RATIONAL_B_SPLINE_CURVE((1.02072197947249,1.02138328368541,1.02072197947249))
REPRESENTATION_ITEM('')
);
#18751=(
BOUNDED_CURVE()
B_SPLINE_CURVE(2,(#68527,#68528,#68529),.UNSPECIFIED.,.F.,.F.)
B_SPLINE_CURVE_WITH_KNOTS((3,3),(0.,0.247929805090921),.UNSPECIFIED.)
CURVE()
GEOMETRIC_REPRESENTATION_ITEM()
RATIONAL_B_SPLINE_CURVE((1.,1.00006942852834,1.00002415803422))
REPRESENTATION_ITEM('')
);
#18752=(
BOUNDED_CURVE()
B_SPLINE_CURVE(2,(#68535,#68536,#68537),.UNSPECIFIED.,.F.,.F.)
B_SPLINE_CURVE_WITH_KNOTS((3,3),(0.0522192481407573,0.300149053231598),
 .UNSPECIFIED.)
CURVE()
GEOMETRIC_REPRESENTATION_ITEM()
RATIONAL_B_SPLINE_CURVE((1.00002415803426,1.00006942852846,1.))
REPRESENTATION_ITEM('')
);
#18753=(
BOUNDED_CURVE()
B_SPLINE_CURVE(2,(#68539,#68540,#68541),.UNSPECIFIED.,.F.,.F.)
B_SPLINE_CURVE_WITH_KNOTS((3,3),(0.984623166322171,1.26677639839307),
 .UNSPECIFIED.)
CURVE()
GEOMETRIC_REPRESENTATION_ITEM()
RATIONAL_B_SPLINE_CURVE((1.02072197947249,1.0213832836854,1.02072197947249))
REPRESENTATION_ITEM('')
);
#18754=(
BOUNDED_CURVE()
B_SPLINE_CURVE(2,(#68542,#68543,#68544),.UNSPECIFIED.,.F.,.F.)
B_SPLINE_CURVE_WITH_KNOTS((3,3),(0.,0.247929805091041),.UNSPECIFIED.)
CURVE()
GEOMETRIC_REPRESENTATION_ITEM()
RATIONAL_B_SPLINE_CURVE((1.,1.0000694285297,1.00002415803469))
REPRESENTATION_ITEM('')
);
#18755=(
BOUNDED_CURVE()
B_SPLINE_CURVE(2,(#68550,#68551,#68552),.UNSPECIFIED.,.F.,.F.)
B_SPLINE_CURVE_WITH_KNOTS((3,3),(0.0522192481406059,0.300149053231598),
 .UNSPECIFIED.)
CURVE()
GEOMETRIC_REPRESENTATION_ITEM()
RATIONAL_B_SPLINE_CURVE((1.00002415803507,1.00006942853079,1.))
REPRESENTATION_ITEM('')
);
#18756=(
BOUNDED_CURVE()
B_SPLINE_CURVE(2,(#68554,#68555,#68556),.UNSPECIFIED.,.F.,.F.)
B_SPLINE_CURVE_WITH_KNOTS((3,3),(0.984623166322169,1.26677639839307),
 .UNSPECIFIED.)
CURVE()
GEOMETRIC_REPRESENTATION_ITEM()
RATIONAL_B_SPLINE_CURVE((1.02072197947249,1.02138328368541,1.02072197947249))
REPRESENTATION_ITEM('')
);
#18757=(
BOUNDED_CURVE()
B_SPLINE_CURVE(2,(#68557,#68558,#68559),.UNSPECIFIED.,.F.,.F.)
B_SPLINE_CURVE_WITH_KNOTS((3,3),(0.,0.247929805090961),.UNSPECIFIED.)
CURVE()
GEOMETRIC_REPRESENTATION_ITEM()
RATIONAL_B_SPLINE_CURVE((1.,1.00006942852846,1.00002415803426))
REPRESENTATION_ITEM('')
);
#18758=(
BOUNDED_CURVE()
B_SPLINE_CURVE(2,(#68565,#68566,#68567),.UNSPECIFIED.,.F.,.F.)
B_SPLINE_CURVE_WITH_KNOTS((3,3),(0.0522192481407161,0.300149053231599),
 .UNSPECIFIED.)
CURVE()
GEOMETRIC_REPRESENTATION_ITEM()
RATIONAL_B_SPLINE_CURVE((1.00002415803387,1.00006942852735,1.))
REPRESENTATION_ITEM('')
);
#18759=(
BOUNDED_CURVE()
B_SPLINE_CURVE(2,(#68569,#68570,#68571),.UNSPECIFIED.,.F.,.F.)
B_SPLINE_CURVE_WITH_KNOTS((3,3),(0.984623166322171,1.26677639839307),
 .UNSPECIFIED.)
CURVE()
GEOMETRIC_REPRESENTATION_ITEM()
RATIONAL_B_SPLINE_CURVE((1.02072197947249,1.02138328368541,1.02072197947249))
REPRESENTATION_ITEM('')
);
#18760=(
BOUNDED_CURVE()
B_SPLINE_CURVE(2,(#68572,#68573,#68574),.UNSPECIFIED.,.F.,.F.)
B_SPLINE_CURVE_WITH_KNOTS((3,3),(0.,0.247929805090882),.UNSPECIFIED.)
CURVE()
GEOMETRIC_REPRESENTATION_ITEM()
RATIONAL_B_SPLINE_CURVE((1.,1.00006942852857,1.0000241580343))
REPRESENTATION_ITEM('')
);
#18761=(
BOUNDED_CURVE()
B_SPLINE_CURVE(2,(#68580,#68581,#68582),.UNSPECIFIED.,.F.,.F.)
B_SPLINE_CURVE_WITH_KNOTS((3,3),(0.0522192481406709,0.300149053231599),
 .UNSPECIFIED.)
CURVE()
GEOMETRIC_REPRESENTATION_ITEM()
RATIONAL_B_SPLINE_CURVE((1.00002415803448,1.0000694285291,1.))
REPRESENTATION_ITEM('')
);
#18762=(
BOUNDED_CURVE()
B_SPLINE_CURVE(2,(#68584,#68585,#68586),.UNSPECIFIED.,.F.,.F.)
B_SPLINE_CURVE_WITH_KNOTS((3,3),(0.984623166322173,1.26677639839308),
 .UNSPECIFIED.)
CURVE()
GEOMETRIC_REPRESENTATION_ITEM()
RATIONAL_B_SPLINE_CURVE((1.02072197947249,1.02138328368541,1.02072197947249))
REPRESENTATION_ITEM('')
);
#18763=(
BOUNDED_CURVE()
B_SPLINE_CURVE(2,(#68587,#68588,#68589),.UNSPECIFIED.,.F.,.F.)
B_SPLINE_CURVE_WITH_KNOTS((3,3),(0.,0.247929805090867),.UNSPECIFIED.)
CURVE()
GEOMETRIC_REPRESENTATION_ITEM()
RATIONAL_B_SPLINE_CURVE((1.,1.00006942852627,1.0000241580335))
REPRESENTATION_ITEM('')
);
#18764=(
BOUNDED_CURVE()
B_SPLINE_CURVE(2,(#68595,#68596,#68597),.UNSPECIFIED.,.F.,.F.)
B_SPLINE_CURVE_WITH_KNOTS((3,3),(0.0522192481406783,0.300149053231598),
 .UNSPECIFIED.)
CURVE()
GEOMETRIC_REPRESENTATION_ITEM()
RATIONAL_B_SPLINE_CURVE((1.00002415803455,1.00006942852929,1.))
REPRESENTATION_ITEM('')
);
#18765=(
BOUNDED_CURVE()
B_SPLINE_CURVE(2,(#68599,#68600,#68601),.UNSPECIFIED.,.F.,.F.)
B_SPLINE_CURVE_WITH_KNOTS((3,3),(0.984623166322171,1.26677639839307),
 .UNSPECIFIED.)
CURVE()
GEOMETRIC_REPRESENTATION_ITEM()
RATIONAL_B_SPLINE_CURVE((1.02072197947249,1.02138328368541,1.02072197947249))
REPRESENTATION_ITEM('')
);
#18766=(
BOUNDED_CURVE()
B_SPLINE_CURVE(2,(#68602,#68603,#68604),.UNSPECIFIED.,.F.,.F.)
B_SPLINE_CURVE_WITH_KNOTS((3,3),(0.,0.247929805090952),.UNSPECIFIED.)
CURVE()
GEOMETRIC_REPRESENTATION_ITEM()
RATIONAL_B_SPLINE_CURVE((1.,1.00006942852834,1.00002415803422))
REPRESENTATION_ITEM('')
);
#18767=(
BOUNDED_CURVE()
B_SPLINE_CURVE(2,(#68610,#68611,#68612),.UNSPECIFIED.,.F.,.F.)
B_SPLINE_CURVE_WITH_KNOTS((3,3),(0.052219248140653,0.300149053231598),
 .UNSPECIFIED.)
CURVE()
GEOMETRIC_REPRESENTATION_ITEM()
RATIONAL_B_SPLINE_CURVE((1.00002415803398,1.00006942852765,1.))
REPRESENTATION_ITEM('')
);
#18768=(
BOUNDED_CURVE()
B_SPLINE_CURVE(2,(#68614,#68615,#68616),.UNSPECIFIED.,.F.,.F.)
B_SPLINE_CURVE_WITH_KNOTS((3,3),(0.984623166322171,1.26677639839307),
 .UNSPECIFIED.)
CURVE()
GEOMETRIC_REPRESENTATION_ITEM()
RATIONAL_B_SPLINE_CURVE((1.02072197947248,1.0213832836854,1.02072197947248))
REPRESENTATION_ITEM('')
);
#18769=(
BOUNDED_CURVE()
B_SPLINE_CURVE(2,(#68617,#68618,#68619),.UNSPECIFIED.,.F.,.F.)
B_SPLINE_CURVE_WITH_KNOTS((3,3),(0.,0.24792980509099),.UNSPECIFIED.)
CURVE()
GEOMETRIC_REPRESENTATION_ITEM()
RATIONAL_B_SPLINE_CURVE((1.,1.00006942852938,1.00002415803458))
REPRESENTATION_ITEM('')
);
#18770=(
BOUNDED_CURVE()
B_SPLINE_CURVE(2,(#68625,#68626,#68627),.UNSPECIFIED.,.F.,.F.)
B_SPLINE_CURVE_WITH_KNOTS((3,3),(0.0522192481406856,0.300149053231599),
 .UNSPECIFIED.)
CURVE()
GEOMETRIC_REPRESENTATION_ITEM()
RATIONAL_B_SPLINE_CURVE((1.00002415803379,1.00006942852711,1.))
REPRESENTATION_ITEM('')
);
#18771=(
BOUNDED_CURVE()
B_SPLINE_CURVE(2,(#68629,#68630,#68631),.UNSPECIFIED.,.F.,.F.)
B_SPLINE_CURVE_WITH_KNOTS((3,3),(0.984623166322173,1.26677639839307),
 .UNSPECIFIED.)
CURVE()
GEOMETRIC_REPRESENTATION_ITEM()
RATIONAL_B_SPLINE_CURVE((1.02072197947249,1.02138328368541,1.02072197947249))
REPRESENTATION_ITEM('')
);
#18772=(
BOUNDED_CURVE()
B_SPLINE_CURVE(2,(#68632,#68633,#68634),.UNSPECIFIED.,.F.,.F.)
B_SPLINE_CURVE_WITH_KNOTS((3,3),(0.,0.247929805090904),.UNSPECIFIED.)
CURVE()
GEOMETRIC_REPRESENTATION_ITEM()
RATIONAL_B_SPLINE_CURVE((1.,1.00006942852969,1.00002415803469))
REPRESENTATION_ITEM('')
);
#18773=(
BOUNDED_CURVE()
B_SPLINE_CURVE(2,(#68640,#68641,#68642),.UNSPECIFIED.,.F.,.F.)
B_SPLINE_CURVE_WITH_KNOTS((3,3),(0.0522192481406978,0.300149053231598),
 .UNSPECIFIED.)
CURVE()
GEOMETRIC_REPRESENTATION_ITEM()
RATIONAL_B_SPLINE_CURVE((1.00002415803478,1.00006942852994,1.))
REPRESENTATION_ITEM('')
);
#18774=(
BOUNDED_CURVE()
B_SPLINE_CURVE(2,(#68644,#68645,#68646),.UNSPECIFIED.,.F.,.F.)
B_SPLINE_CURVE_WITH_KNOTS((3,3),(0.984623166322171,1.26677639839307),
 .UNSPECIFIED.)
CURVE()
GEOMETRIC_REPRESENTATION_ITEM()
RATIONAL_B_SPLINE_CURVE((1.02072197947249,1.02138328368541,1.02072197947249))
REPRESENTATION_ITEM('')
);
#18775=(
BOUNDED_CURVE()
B_SPLINE_CURVE(2,(#68647,#68648,#68649),.UNSPECIFIED.,.F.,.F.)
B_SPLINE_CURVE_WITH_KNOTS((3,3),(0.,0.247929805090887),.UNSPECIFIED.)
CURVE()
GEOMETRIC_REPRESENTATION_ITEM()
RATIONAL_B_SPLINE_CURVE((1.,1.00006942852981,1.00002415803473))
REPRESENTATION_ITEM('')
);
#18776=(
BOUNDED_CURVE()
B_SPLINE_CURVE(2,(#68655,#68656,#68657),.UNSPECIFIED.,.F.,.F.)
B_SPLINE_CURVE_WITH_KNOTS((3,3),(0.0522192481406133,0.300149053231598),
 .UNSPECIFIED.)
CURVE()
GEOMETRIC_REPRESENTATION_ITEM()
RATIONAL_B_SPLINE_CURVE((1.00002415803473,1.00006942852981,1.))
REPRESENTATION_ITEM('')
);
#18777=(
BOUNDED_CURVE()
B_SPLINE_CURVE(2,(#68659,#68660,#68661),.UNSPECIFIED.,.F.,.F.)
B_SPLINE_CURVE_WITH_KNOTS((3,3),(0.984623166322172,1.26677639839307),
 .UNSPECIFIED.)
CURVE()
GEOMETRIC_REPRESENTATION_ITEM()
RATIONAL_B_SPLINE_CURVE((1.02072197947249,1.02138328368541,1.02072197947249))
REPRESENTATION_ITEM('')
);
#18778=(
BOUNDED_CURVE()
B_SPLINE_CURVE(2,(#68662,#68663,#68664),.UNSPECIFIED.,.F.,.F.)
B_SPLINE_CURVE_WITH_KNOTS((3,3),(0.,0.247929805090893),.UNSPECIFIED.)
CURVE()
GEOMETRIC_REPRESENTATION_ITEM()
RATIONAL_B_SPLINE_CURVE((1.,1.00006942852818,1.00002415803416))
REPRESENTATION_ITEM('')
);
#18779=(
BOUNDED_CURVE()
B_SPLINE_CURVE(2,(#68670,#68671,#68672),.UNSPECIFIED.,.F.,.F.)
B_SPLINE_CURVE_WITH_KNOTS((3,3),(0.0522192481407881,0.300149053231599),
 .UNSPECIFIED.)
CURVE()
GEOMETRIC_REPRESENTATION_ITEM()
RATIONAL_B_SPLINE_CURVE((1.0000241580339,1.00006942852742,1.))
REPRESENTATION_ITEM('')
);
#18780=(
BOUNDED_CURVE()
B_SPLINE_CURVE(2,(#68674,#68675,#68676),.UNSPECIFIED.,.F.,.F.)
B_SPLINE_CURVE_WITH_KNOTS((3,3),(0.984623166322172,1.26677639839307),
 .UNSPECIFIED.)
CURVE()
GEOMETRIC_REPRESENTATION_ITEM()
RATIONAL_B_SPLINE_CURVE((1.02072197947249,1.02138328368541,1.02072197947249))
REPRESENTATION_ITEM('')
);
#18781=(
BOUNDED_CURVE()
B_SPLINE_CURVE(2,(#68677,#68678,#68679),.UNSPECIFIED.,.F.,.F.)
B_SPLINE_CURVE_WITH_KNOTS((3,3),(0.,0.24792980509091),.UNSPECIFIED.)
CURVE()
GEOMETRIC_REPRESENTATION_ITEM()
RATIONAL_B_SPLINE_CURVE((1.,1.00006942852692,1.00002415803372))
REPRESENTATION_ITEM('')
);
#18782=(
BOUNDED_CURVE()
B_SPLINE_CURVE(2,(#68685,#68686,#68687),.UNSPECIFIED.,.F.,.F.)
B_SPLINE_CURVE_WITH_KNOTS((3,3),(0.0522192481406546,0.300149053231598),
 .UNSPECIFIED.)
CURVE()
GEOMETRIC_REPRESENTATION_ITEM()
RATIONAL_B_SPLINE_CURVE((1.00002415803456,1.00006942852932,1.))
REPRESENTATION_ITEM('')
);
#18783=(
BOUNDED_CURVE()
B_SPLINE_CURVE(2,(#68689,#68690,#68691),.UNSPECIFIED.,.F.,.F.)
B_SPLINE_CURVE_WITH_KNOTS((3,3),(0.984623166322169,1.26677639839307),
 .UNSPECIFIED.)
CURVE()
GEOMETRIC_REPRESENTATION_ITEM()
RATIONAL_B_SPLINE_CURVE((1.02072197947249,1.02138328368541,1.02072197947249))
REPRESENTATION_ITEM('')
);
#18784=(
BOUNDED_CURVE()
B_SPLINE_CURVE(2,(#68692,#68693,#68694),.UNSPECIFIED.,.F.,.F.)
B_SPLINE_CURVE_WITH_KNOTS((3,3),(0.,0.247929805090884),.UNSPECIFIED.)
CURVE()
GEOMETRIC_REPRESENTATION_ITEM()
RATIONAL_B_SPLINE_CURVE((1.,1.00006942852775,1.00002415803401))
REPRESENTATION_ITEM('')
);
#18785=(
BOUNDED_CURVE()
B_SPLINE_CURVE(2,(#68700,#68701,#68702),.UNSPECIFIED.,.F.,.F.)
B_SPLINE_CURVE_WITH_KNOTS((3,3),(0.0522192481406402,0.300149053231599),
 .UNSPECIFIED.)
CURVE()
GEOMETRIC_REPRESENTATION_ITEM()
RATIONAL_B_SPLINE_CURVE((1.00002415803407,1.0000694285279,1.))
REPRESENTATION_ITEM('')
);
#18786=(
BOUNDED_CURVE()
B_SPLINE_CURVE(2,(#68704,#68705,#68706),.UNSPECIFIED.,.F.,.F.)
B_SPLINE_CURVE_WITH_KNOTS((3,3),(0.984623166322172,1.26677639839307),
 .UNSPECIFIED.)
CURVE()
GEOMETRIC_REPRESENTATION_ITEM()
RATIONAL_B_SPLINE_CURVE((1.02072197947249,1.02138328368541,1.02072197947249))
REPRESENTATION_ITEM('')
);
#18787=(
BOUNDED_CURVE()
B_SPLINE_CURVE(2,(#68707,#68708,#68709),.UNSPECIFIED.,.F.,.F.)
B_SPLINE_CURVE_WITH_KNOTS((3,3),(0.,0.247929805090997),.UNSPECIFIED.)
CURVE()
GEOMETRIC_REPRESENTATION_ITEM()
RATIONAL_B_SPLINE_CURVE((1.,1.00006942852925,1.00002415803454))
REPRESENTATION_ITEM('')
);
#18788=(
BOUNDED_CURVE()
B_SPLINE_CURVE(2,(#68715,#68716,#68717),.UNSPECIFIED.,.F.,.F.)
B_SPLINE_CURVE_WITH_KNOTS((3,3),(0.0522192481407274,0.300149053231599),
 .UNSPECIFIED.)
CURVE()
GEOMETRIC_REPRESENTATION_ITEM()
RATIONAL_B_SPLINE_CURVE((1.00002415803356,1.00006942852645,1.))
REPRESENTATION_ITEM('')
);
#18789=(
BOUNDED_CURVE()
B_SPLINE_CURVE(2,(#68719,#68720,#68721),.UNSPECIFIED.,.F.,.F.)
B_SPLINE_CURVE_WITH_KNOTS((3,3),(0.984623166322171,1.26677639839307),
 .UNSPECIFIED.)
CURVE()
GEOMETRIC_REPRESENTATION_ITEM()
RATIONAL_B_SPLINE_CURVE((1.02072197947249,1.02138328368541,1.02072197947249))
REPRESENTATION_ITEM('')
);
#18790=(
BOUNDED_CURVE()
B_SPLINE_CURVE(2,(#68722,#68723,#68724),.UNSPECIFIED.,.F.,.F.)
B_SPLINE_CURVE_WITH_KNOTS((3,3),(0.,0.247929805090888),.UNSPECIFIED.)
CURVE()
GEOMETRIC_REPRESENTATION_ITEM()
RATIONAL_B_SPLINE_CURVE((1.,1.00006942852913,1.00002415803449))
REPRESENTATION_ITEM('')
);
#18791=(
BOUNDED_CURVE()
B_SPLINE_CURVE(2,(#68730,#68731,#68732),.UNSPECIFIED.,.F.,.F.)
B_SPLINE_CURVE_WITH_KNOTS((3,3),(0.0522192481406619,0.300149053231598),
 .UNSPECIFIED.)
CURVE()
GEOMETRIC_REPRESENTATION_ITEM()
RATIONAL_B_SPLINE_CURVE((1.00002415803529,1.00006942853141,1.))
REPRESENTATION_ITEM('')
);
#18792=(
BOUNDED_CURVE()
B_SPLINE_CURVE(2,(#68734,#68735,#68736),.UNSPECIFIED.,.F.,.F.)
B_SPLINE_CURVE_WITH_KNOTS((3,3),(0.984623166322169,1.26677639839307),
 .UNSPECIFIED.)
CURVE()
GEOMETRIC_REPRESENTATION_ITEM()
RATIONAL_B_SPLINE_CURVE((1.02072197947249,1.02138328368541,1.02072197947249))
REPRESENTATION_ITEM('')
);
#18793=(
BOUNDED_CURVE()
B_SPLINE_CURVE(2,(#68737,#68738,#68739),.UNSPECIFIED.,.F.,.F.)
B_SPLINE_CURVE_WITH_KNOTS((3,3),(0.,0.247929805090904),.UNSPECIFIED.)
CURVE()
GEOMETRIC_REPRESENTATION_ITEM()
RATIONAL_B_SPLINE_CURVE((1.,1.00006942852951,1.00002415803463))
REPRESENTATION_ITEM('')
);
#18794=(
BOUNDED_CURVE()
B_SPLINE_CURVE(2,(#68745,#68746,#68747),.UNSPECIFIED.,.F.,.F.)
B_SPLINE_CURVE_WITH_KNOTS((3,3),(0.0522192481407164,0.300149053231598),
 .UNSPECIFIED.)
CURVE()
GEOMETRIC_REPRESENTATION_ITEM()
RATIONAL_B_SPLINE_CURVE((1.00002415803377,1.00006942852705,1.))
REPRESENTATION_ITEM('')
);
#18795=(
BOUNDED_CURVE()
B_SPLINE_CURVE(2,(#68749,#68750,#68751),.UNSPECIFIED.,.F.,.F.)
B_SPLINE_CURVE_WITH_KNOTS((3,3),(0.984623166322171,1.26677639839307),
 .UNSPECIFIED.)
CURVE()
GEOMETRIC_REPRESENTATION_ITEM()
RATIONAL_B_SPLINE_CURVE((1.02072197947249,1.02138328368541,1.02072197947249))
REPRESENTATION_ITEM('')
);
#18796=(
BOUNDED_CURVE()
B_SPLINE_CURVE(2,(#68752,#68753,#68754),.UNSPECIFIED.,.F.,.F.)
B_SPLINE_CURVE_WITH_KNOTS((3,3),(0.,0.247929805090835),.UNSPECIFIED.)
CURVE()
GEOMETRIC_REPRESENTATION_ITEM()
RATIONAL_B_SPLINE_CURVE((1.,1.00006942852771,1.000024158034))
REPRESENTATION_ITEM('')
);
#18797=(
BOUNDED_CURVE()
B_SPLINE_CURVE(2,(#68760,#68761,#68762),.UNSPECIFIED.,.F.,.F.)
B_SPLINE_CURVE_WITH_KNOTS((3,3),(0.0522192481406349,0.300149053231599),
 .UNSPECIFIED.)
CURVE()
GEOMETRIC_REPRESENTATION_ITEM()
RATIONAL_B_SPLINE_CURVE((1.00002415803477,1.00006942852992,1.))
REPRESENTATION_ITEM('')
);
#18798=(
BOUNDED_CURVE()
B_SPLINE_CURVE(2,(#68764,#68765,#68766),.UNSPECIFIED.,.F.,.F.)
B_SPLINE_CURVE_WITH_KNOTS((3,3),(0.984623166322174,1.26677639839308),
 .UNSPECIFIED.)
CURVE()
GEOMETRIC_REPRESENTATION_ITEM()
RATIONAL_B_SPLINE_CURVE((1.02072197947248,1.0213832836854,1.02072197947248))
REPRESENTATION_ITEM('')
);
#18799=(
BOUNDED_CURVE()
B_SPLINE_CURVE(2,(#68767,#68768,#68769),.UNSPECIFIED.,.F.,.F.)
B_SPLINE_CURVE_WITH_KNOTS((3,3),(0.,0.247929805090929),.UNSPECIFIED.)
CURVE()
GEOMETRIC_REPRESENTATION_ITEM()
RATIONAL_B_SPLINE_CURVE((1.,1.00006942852897,1.00002415803444))
REPRESENTATION_ITEM('')
);
#18800=(
BOUNDED_CURVE()
B_SPLINE_CURVE(2,(#68775,#68776,#68777),.UNSPECIFIED.,.F.,.F.)
B_SPLINE_CURVE_WITH_KNOTS((3,3),(0.0522192481406456,0.300149053231598),
 .UNSPECIFIED.)
CURVE()
GEOMETRIC_REPRESENTATION_ITEM()
RATIONAL_B_SPLINE_CURVE((1.0000241580344,1.00006942852887,1.))
REPRESENTATION_ITEM('')
);
#18801=(
BOUNDED_CURVE()
B_SPLINE_CURVE(2,(#68779,#68780,#68781),.UNSPECIFIED.,.F.,.F.)
B_SPLINE_CURVE_WITH_KNOTS((3,3),(0.984623166322169,1.26677639839307),
 .UNSPECIFIED.)
CURVE()
GEOMETRIC_REPRESENTATION_ITEM()
RATIONAL_B_SPLINE_CURVE((1.02072197947249,1.0213832836854,1.02072197947249))
REPRESENTATION_ITEM('')
);
#18802=(
BOUNDED_CURVE()
B_SPLINE_CURVE(2,(#68782,#68783,#68784),.UNSPECIFIED.,.F.,.F.)
B_SPLINE_CURVE_WITH_KNOTS((3,3),(0.,0.247929805090801),.UNSPECIFIED.)
CURVE()
GEOMETRIC_REPRESENTATION_ITEM()
RATIONAL_B_SPLINE_CURVE((1.,1.00006942852834,1.00002415803422))
REPRESENTATION_ITEM('')
);
#18803=(
BOUNDED_CURVE()
B_SPLINE_CURVE(2,(#68790,#68791,#68792),.UNSPECIFIED.,.F.,.F.)
B_SPLINE_CURVE_WITH_KNOTS((3,3),(0.0522192481407089,0.300149053231598),
 .UNSPECIFIED.)
CURVE()
GEOMETRIC_REPRESENTATION_ITEM()
RATIONAL_B_SPLINE_CURVE((1.00002415803465,1.00006942852957,1.))
REPRESENTATION_ITEM('')
);
#18804=(
BOUNDED_CURVE()
B_SPLINE_CURVE(2,(#68794,#68795,#68796),.UNSPECIFIED.,.F.,.F.)
B_SPLINE_CURVE_WITH_KNOTS((3,3),(0.984623166322172,1.26677639839307),
 .UNSPECIFIED.)
CURVE()
GEOMETRIC_REPRESENTATION_ITEM()
RATIONAL_B_SPLINE_CURVE((1.02072197947249,1.02138328368541,1.02072197947249))
REPRESENTATION_ITEM('')
);
#18805=(
BOUNDED_CURVE()
B_SPLINE_CURVE(2,(#68797,#68798,#68799),.UNSPECIFIED.,.F.,.F.)
B_SPLINE_CURVE_WITH_KNOTS((3,3),(0.,0.247929805090902),.UNSPECIFIED.)
CURVE()
GEOMETRIC_REPRESENTATION_ITEM()
RATIONAL_B_SPLINE_CURVE((1.,1.0000694285288,1.00002415803438))
REPRESENTATION_ITEM('')
);
#18806=(
BOUNDED_CURVE()
B_SPLINE_CURVE(2,(#68832,#68833,#68834),.UNSPECIFIED.,.F.,.F.)
B_SPLINE_CURVE_WITH_KNOTS((3,3),(0.984623166322171,1.26677639839307),
 .UNSPECIFIED.)
CURVE()
GEOMETRIC_REPRESENTATION_ITEM()
RATIONAL_B_SPLINE_CURVE((1.02072197947249,1.02138328368541,1.02072197947249))
REPRESENTATION_ITEM('')
);
#18807=(
BOUNDED_CURVE()
B_SPLINE_CURVE(2,(#68870,#68871,#68872),.UNSPECIFIED.,.F.,.F.)
B_SPLINE_CURVE_WITH_KNOTS((3,3),(0.,0.0730837266078461),.UNSPECIFIED.)
CURVE()
GEOMETRIC_REPRESENTATION_ITEM()
RATIONAL_B_SPLINE_CURVE((1.,1.00000531281866,1.0000024358309))
REPRESENTATION_ITEM('')
);
#18808=(
BOUNDED_CURVE()
B_SPLINE_CURVE(2,(#68908,#68909,#68910),.UNSPECIFIED.,.F.,.F.)
B_SPLINE_CURVE_WITH_KNOTS((3,3),(0.98462316632217,1.26677639839307),
 .UNSPECIFIED.)
CURVE()
GEOMETRIC_REPRESENTATION_ITEM()
RATIONAL_B_SPLINE_CURVE((1.02072197947249,1.02138328368541,1.02072197947249))
REPRESENTATION_ITEM('')
);
#18809=(
BOUNDED_CURVE()
B_SPLINE_CURVE(2,(#68946,#68947,#68948),.UNSPECIFIED.,.F.,.F.)
B_SPLINE_CURVE_WITH_KNOTS((3,3),(0.,0.0730837266087433),.UNSPECIFIED.)
CURVE()
GEOMETRIC_REPRESENTATION_ITEM()
RATIONAL_B_SPLINE_CURVE((1.,1.00000531285818,1.00000243584903))
REPRESENTATION_ITEM('')
);
#18810=(
BOUNDED_CURVE()
B_SPLINE_CURVE(2,(#68984,#68985,#68986),.UNSPECIFIED.,.F.,.F.)
B_SPLINE_CURVE_WITH_KNOTS((3,3),(0.984623166322173,1.26677639839308),
 .UNSPECIFIED.)
CURVE()
GEOMETRIC_REPRESENTATION_ITEM()
RATIONAL_B_SPLINE_CURVE((1.02072197947249,1.02138328368541,1.02072197947249))
REPRESENTATION_ITEM('')
);
#18811=(
BOUNDED_CURVE()
B_SPLINE_CURVE(2,(#69022,#69023,#69024),.UNSPECIFIED.,.F.,.F.)
B_SPLINE_CURVE_WITH_KNOTS((3,3),(0.,0.0730837266085301),.UNSPECIFIED.)
CURVE()
GEOMETRIC_REPRESENTATION_ITEM()
RATIONAL_B_SPLINE_CURVE((1.,1.0000053128329,1.00000243583743))
REPRESENTATION_ITEM('')
);
#18812=(
BOUNDED_CURVE()
B_SPLINE_CURVE(2,(#69060,#69061,#69062),.UNSPECIFIED.,.F.,.F.)
B_SPLINE_CURVE_WITH_KNOTS((3,3),(0.984623166322171,1.26677639839307),
 .UNSPECIFIED.)
CURVE()
GEOMETRIC_REPRESENTATION_ITEM()
RATIONAL_B_SPLINE_CURVE((1.02072197947249,1.02138328368541,1.02072197947249))
REPRESENTATION_ITEM('')
);
#18813=(
BOUNDED_CURVE()
B_SPLINE_CURVE(2,(#69098,#69099,#69100),.UNSPECIFIED.,.F.,.F.)
B_SPLINE_CURVE_WITH_KNOTS((3,3),(0.,0.073083726608233),.UNSPECIFIED.)
CURVE()
GEOMETRIC_REPRESENTATION_ITEM()
RATIONAL_B_SPLINE_CURVE((1.,1.00000531282325,1.00000243583301))
REPRESENTATION_ITEM('')
);
#18814=(
BOUNDED_CURVE()
B_SPLINE_CURVE(2,(#69136,#69137,#69138),.UNSPECIFIED.,.F.,.F.)
B_SPLINE_CURVE_WITH_KNOTS((3,3),(0.98462316632217,1.26677639839307),
 .UNSPECIFIED.)
CURVE()
GEOMETRIC_REPRESENTATION_ITEM()
RATIONAL_B_SPLINE_CURVE((1.02072197947249,1.02138328368541,1.02072197947249))
REPRESENTATION_ITEM('')
);
#18815=(
BOUNDED_CURVE()
B_SPLINE_CURVE(2,(#69174,#69175,#69176),.UNSPECIFIED.,.F.,.F.)
B_SPLINE_CURVE_WITH_KNOTS((3,3),(0.,0.0730837266086981),.UNSPECIFIED.)
CURVE()
GEOMETRIC_REPRESENTATION_ITEM()
RATIONAL_B_SPLINE_CURVE((1.,1.000005312841,1.00000243584115))
REPRESENTATION_ITEM('')
);
#18816=(
BOUNDED_CURVE()
B_SPLINE_CURVE(2,(#69212,#69213,#69214),.UNSPECIFIED.,.F.,.F.)
B_SPLINE_CURVE_WITH_KNOTS((3,3),(0.984623166322174,1.26677639839308),
 .UNSPECIFIED.)
CURVE()
GEOMETRIC_REPRESENTATION_ITEM()
RATIONAL_B_SPLINE_CURVE((1.02072197947249,1.02138328368541,1.02072197947249))
REPRESENTATION_ITEM('')
);
#18817=(
BOUNDED_CURVE()
B_SPLINE_CURVE(2,(#69250,#69251,#69252),.UNSPECIFIED.,.F.,.F.)
B_SPLINE_CURVE_WITH_KNOTS((3,3),(0.,0.0730837266083448),.UNSPECIFIED.)
CURVE()
GEOMETRIC_REPRESENTATION_ITEM()
RATIONAL_B_SPLINE_CURVE((1.,1.00000531283336,1.00000243583764))
REPRESENTATION_ITEM('')
);
#18818=(
BOUNDED_CURVE()
B_SPLINE_CURVE(2,(#69288,#69289,#69290),.UNSPECIFIED.,.F.,.F.)
B_SPLINE_CURVE_WITH_KNOTS((3,3),(0.984623166322172,1.26677639839307),
 .UNSPECIFIED.)
CURVE()
GEOMETRIC_REPRESENTATION_ITEM()
RATIONAL_B_SPLINE_CURVE((1.02072197947249,1.02138328368541,1.02072197947249))
REPRESENTATION_ITEM('')
);
#18819=(
BOUNDED_CURVE()
B_SPLINE_CURVE(2,(#69326,#69327,#69328),.UNSPECIFIED.,.F.,.F.)
B_SPLINE_CURVE_WITH_KNOTS((3,3),(0.,0.0730837266085423),.UNSPECIFIED.)
CURVE()
GEOMETRIC_REPRESENTATION_ITEM()
RATIONAL_B_SPLINE_CURVE((1.,1.00000531284476,1.00000243584287))
REPRESENTATION_ITEM('')
);
#18820=(
BOUNDED_CURVE()
B_SPLINE_CURVE(2,(#69364,#69365,#69366),.UNSPECIFIED.,.F.,.F.)
B_SPLINE_CURVE_WITH_KNOTS((3,3),(0.98462316632217,1.26677639839307),
 .UNSPECIFIED.)
CURVE()
GEOMETRIC_REPRESENTATION_ITEM()
RATIONAL_B_SPLINE_CURVE((1.02072197947249,1.02138328368541,1.02072197947249))
REPRESENTATION_ITEM('')
);
#18821=(
BOUNDED_CURVE()
B_SPLINE_CURVE(2,(#69402,#69403,#69404),.UNSPECIFIED.,.F.,.F.)
B_SPLINE_CURVE_WITH_KNOTS((3,3),(0.,0.0730837266082547),.UNSPECIFIED.)
CURVE()
GEOMETRIC_REPRESENTATION_ITEM()
RATIONAL_B_SPLINE_CURVE((1.,1.0000053128325,1.00000243583725))
REPRESENTATION_ITEM('')
);
#18822=(
BOUNDED_CURVE()
B_SPLINE_CURVE(2,(#69440,#69441,#69442),.UNSPECIFIED.,.F.,.F.)
B_SPLINE_CURVE_WITH_KNOTS((3,3),(0.984623166322172,1.26677639839307),
 .UNSPECIFIED.)
CURVE()
GEOMETRIC_REPRESENTATION_ITEM()
RATIONAL_B_SPLINE_CURVE((1.02072197947249,1.02138328368541,1.02072197947249))
REPRESENTATION_ITEM('')
);
#18823=(
BOUNDED_CURVE()
B_SPLINE_CURVE(2,(#69478,#69479,#69480),.UNSPECIFIED.,.F.,.F.)
B_SPLINE_CURVE_WITH_KNOTS((3,3),(0.,0.0730837266088366),.UNSPECIFIED.)
CURVE()
GEOMETRIC_REPRESENTATION_ITEM()
RATIONAL_B_SPLINE_CURVE((1.,1.00000531284141,1.00000243584134))
REPRESENTATION_ITEM('')
);
#18824=(
BOUNDED_CURVE()
B_SPLINE_CURVE(2,(#69516,#69517,#69518),.UNSPECIFIED.,.F.,.F.)
B_SPLINE_CURVE_WITH_KNOTS((3,3),(0.984623166322171,1.26677639839307),
 .UNSPECIFIED.)
CURVE()
GEOMETRIC_REPRESENTATION_ITEM()
RATIONAL_B_SPLINE_CURVE((1.02072197947249,1.02138328368541,1.02072197947249))
REPRESENTATION_ITEM('')
);
#18825=(
BOUNDED_CURVE()
B_SPLINE_CURVE(2,(#69554,#69555,#69556),.UNSPECIFIED.,.F.,.F.)
B_SPLINE_CURVE_WITH_KNOTS((3,3),(0.,0.0730837266084984),.UNSPECIFIED.)
CURVE()
GEOMETRIC_REPRESENTATION_ITEM()
RATIONAL_B_SPLINE_CURVE((1.,1.00000531283258,1.00000243583729))
REPRESENTATION_ITEM('')
);
#18826=(
BOUNDED_CURVE()
B_SPLINE_CURVE(2,(#69592,#69593,#69594),.UNSPECIFIED.,.F.,.F.)
B_SPLINE_CURVE_WITH_KNOTS((3,3),(0.984623166322171,1.26677639839307),
 .UNSPECIFIED.)
CURVE()
GEOMETRIC_REPRESENTATION_ITEM()
RATIONAL_B_SPLINE_CURVE((1.02072197947249,1.02138328368541,1.02072197947249))
REPRESENTATION_ITEM('')
);
#18827=(
BOUNDED_CURVE()
B_SPLINE_CURVE(2,(#69630,#69631,#69632),.UNSPECIFIED.,.F.,.F.)
B_SPLINE_CURVE_WITH_KNOTS((3,3),(0.,0.07308372660832),.UNSPECIFIED.)
CURVE()
GEOMETRIC_REPRESENTATION_ITEM()
RATIONAL_B_SPLINE_CURVE((1.,1.00000531285587,1.00000243584797))
REPRESENTATION_ITEM('')
);
#18828=(
BOUNDED_CURVE()
B_SPLINE_CURVE(2,(#69668,#69669,#69670),.UNSPECIFIED.,.F.,.F.)
B_SPLINE_CURVE_WITH_KNOTS((3,3),(0.984623166322173,1.26677639839308),
 .UNSPECIFIED.)
CURVE()
GEOMETRIC_REPRESENTATION_ITEM()
RATIONAL_B_SPLINE_CURVE((1.02072197947249,1.02138328368541,1.02072197947249))
REPRESENTATION_ITEM('')
);
#18829=(
BOUNDED_CURVE()
B_SPLINE_CURVE(2,(#69706,#69707,#69708),.UNSPECIFIED.,.F.,.F.)
B_SPLINE_CURVE_WITH_KNOTS((3,3),(0.,0.0730837266084226),.UNSPECIFIED.)
CURVE()
GEOMETRIC_REPRESENTATION_ITEM()
RATIONAL_B_SPLINE_CURVE((1.,1.00000531284265,1.0000024358419))
REPRESENTATION_ITEM('')
);
#18830=(
BOUNDED_CURVE()
B_SPLINE_CURVE(2,(#69744,#69745,#69746),.UNSPECIFIED.,.F.,.F.)
B_SPLINE_CURVE_WITH_KNOTS((3,3),(0.984623166322167,1.26677639839307),
 .UNSPECIFIED.)
CURVE()
GEOMETRIC_REPRESENTATION_ITEM()
RATIONAL_B_SPLINE_CURVE((1.02072197947249,1.02138328368541,1.02072197947249))
REPRESENTATION_ITEM('')
);
#18831=(
BOUNDED_CURVE()
B_SPLINE_CURVE(2,(#69782,#69783,#69784),.UNSPECIFIED.,.F.,.F.)
B_SPLINE_CURVE_WITH_KNOTS((3,3),(0.,0.0730837266083765),.UNSPECIFIED.)
CURVE()
GEOMETRIC_REPRESENTATION_ITEM()
RATIONAL_B_SPLINE_CURVE((1.,1.00000531283331,1.00000243583762))
REPRESENTATION_ITEM('')
);
#18832=(
BOUNDED_CURVE()
B_SPLINE_CURVE(2,(#69820,#69821,#69822),.UNSPECIFIED.,.F.,.F.)
B_SPLINE_CURVE_WITH_KNOTS((3,3),(0.984623166322173,1.26677639839307),
 .UNSPECIFIED.)
CURVE()
GEOMETRIC_REPRESENTATION_ITEM()
RATIONAL_B_SPLINE_CURVE((1.02072197947249,1.02138328368541,1.02072197947249))
REPRESENTATION_ITEM('')
);
#18833=(
BOUNDED_CURVE()
B_SPLINE_CURVE(2,(#69858,#69859,#69860),.UNSPECIFIED.,.F.,.F.)
B_SPLINE_CURVE_WITH_KNOTS((3,3),(0.,0.0730837266082079),.UNSPECIFIED.)
CURVE()
GEOMETRIC_REPRESENTATION_ITEM()
RATIONAL_B_SPLINE_CURVE((1.,1.00000531281752,1.00000243583038))
REPRESENTATION_ITEM('')
);
#18834=(
BOUNDED_CURVE()
B_SPLINE_CURVE(2,(#69896,#69897,#69898),.UNSPECIFIED.,.F.,.F.)
B_SPLINE_CURVE_WITH_KNOTS((3,3),(0.984623166322173,1.26677639839308),
 .UNSPECIFIED.)
CURVE()
GEOMETRIC_REPRESENTATION_ITEM()
RATIONAL_B_SPLINE_CURVE((1.02072197947249,1.02138328368541,1.02072197947249))
REPRESENTATION_ITEM('')
);
#18835=(
BOUNDED_CURVE()
B_SPLINE_CURVE(2,(#69934,#69935,#69936),.UNSPECIFIED.,.F.,.F.)
B_SPLINE_CURVE_WITH_KNOTS((3,3),(0.,0.0730837266086429),.UNSPECIFIED.)
CURVE()
GEOMETRIC_REPRESENTATION_ITEM()
RATIONAL_B_SPLINE_CURVE((1.,1.00000531285462,1.00000243584739))
REPRESENTATION_ITEM('')
);
#18836=(
BOUNDED_CURVE()
B_SPLINE_CURVE(2,(#69972,#69973,#69974),.UNSPECIFIED.,.F.,.F.)
B_SPLINE_CURVE_WITH_KNOTS((3,3),(0.98462316632217,1.26677639839307),
 .UNSPECIFIED.)
CURVE()
GEOMETRIC_REPRESENTATION_ITEM()
RATIONAL_B_SPLINE_CURVE((1.02072197947249,1.02138328368541,1.02072197947249))
REPRESENTATION_ITEM('')
);
#18837=(
BOUNDED_CURVE()
B_SPLINE_CURVE(2,(#70010,#70011,#70012),.UNSPECIFIED.,.F.,.F.)
B_SPLINE_CURVE_WITH_KNOTS((3,3),(0.,0.0730837266083056),.UNSPECIFIED.)
CURVE()
GEOMETRIC_REPRESENTATION_ITEM()
RATIONAL_B_SPLINE_CURVE((1.,1.00000531283932,1.00000243584038))
REPRESENTATION_ITEM('')
);
#18838=(
BOUNDED_CURVE()
B_SPLINE_CURVE(2,(#70048,#70049,#70050),.UNSPECIFIED.,.F.,.F.)
B_SPLINE_CURVE_WITH_KNOTS((3,3),(0.98462316632217,1.26677639839307),
 .UNSPECIFIED.)
CURVE()
GEOMETRIC_REPRESENTATION_ITEM()
RATIONAL_B_SPLINE_CURVE((1.02072197947249,1.02138328368541,1.02072197947249))
REPRESENTATION_ITEM('')
);
#18839=(
BOUNDED_CURVE()
B_SPLINE_CURVE(2,(#70086,#70087,#70088),.UNSPECIFIED.,.F.,.F.)
B_SPLINE_CURVE_WITH_KNOTS((3,3),(0.,0.0730837266081987),.UNSPECIFIED.)
CURVE()
GEOMETRIC_REPRESENTATION_ITEM()
RATIONAL_B_SPLINE_CURVE((1.,1.00000531282782,1.00000243583511))
REPRESENTATION_ITEM('')
);
#18840=(
BOUNDED_CURVE()
B_SPLINE_CURVE(2,(#70124,#70125,#70126),.UNSPECIFIED.,.F.,.F.)
B_SPLINE_CURVE_WITH_KNOTS((3,3),(0.984623166322174,1.26677639839308),
 .UNSPECIFIED.)
CURVE()
GEOMETRIC_REPRESENTATION_ITEM()
RATIONAL_B_SPLINE_CURVE((1.02072197947248,1.0213832836854,1.02072197947248))
REPRESENTATION_ITEM('')
);
#18841=(
BOUNDED_CURVE()
B_SPLINE_CURVE(2,(#70162,#70163,#70164),.UNSPECIFIED.,.F.,.F.)
B_SPLINE_CURVE_WITH_KNOTS((3,3),(0.,0.0730837266084284),.UNSPECIFIED.)
CURVE()
GEOMETRIC_REPRESENTATION_ITEM()
RATIONAL_B_SPLINE_CURVE((1.,1.00000531283343,1.00000243583768))
REPRESENTATION_ITEM('')
);
#18842=(
BOUNDED_CURVE()
B_SPLINE_CURVE(2,(#70200,#70201,#70202),.UNSPECIFIED.,.F.,.F.)
B_SPLINE_CURVE_WITH_KNOTS((3,3),(0.984623166322172,1.26677639839307),
 .UNSPECIFIED.)
CURVE()
GEOMETRIC_REPRESENTATION_ITEM()
RATIONAL_B_SPLINE_CURVE((1.02072197947249,1.02138328368541,1.02072197947249))
REPRESENTATION_ITEM('')
);
#18843=(
BOUNDED_CURVE()
B_SPLINE_CURVE(2,(#70238,#70239,#70240),.UNSPECIFIED.,.F.,.F.)
B_SPLINE_CURVE_WITH_KNOTS((3,3),(0.,0.0730837266080622),.UNSPECIFIED.)
CURVE()
GEOMETRIC_REPRESENTATION_ITEM()
RATIONAL_B_SPLINE_CURVE((1.,1.00000531280049,1.00000243582258))
REPRESENTATION_ITEM('')
);
#18844=(
BOUNDED_CURVE()
B_SPLINE_CURVE(2,(#70276,#70277,#70278),.UNSPECIFIED.,.F.,.F.)
B_SPLINE_CURVE_WITH_KNOTS((3,3),(0.984623166322171,1.26677639839307),
 .UNSPECIFIED.)
CURVE()
GEOMETRIC_REPRESENTATION_ITEM()
RATIONAL_B_SPLINE_CURVE((1.02072197947249,1.02138328368541,1.02072197947249))
REPRESENTATION_ITEM('')
);
#18845=(
BOUNDED_CURVE()
B_SPLINE_CURVE(2,(#70314,#70315,#70316),.UNSPECIFIED.,.F.,.F.)
B_SPLINE_CURVE_WITH_KNOTS((3,3),(0.,0.0730837266082324),.UNSPECIFIED.)
CURVE()
GEOMETRIC_REPRESENTATION_ITEM()
RATIONAL_B_SPLINE_CURVE((1.,1.00000531281127,1.00000243582752))
REPRESENTATION_ITEM('')
);
#18846=(
BOUNDED_CURVE()
B_SPLINE_CURVE(2,(#70352,#70353,#70354),.UNSPECIFIED.,.F.,.F.)
B_SPLINE_CURVE_WITH_KNOTS((3,3),(0.984623166322172,1.26677639839308),
 .UNSPECIFIED.)
CURVE()
GEOMETRIC_REPRESENTATION_ITEM()
RATIONAL_B_SPLINE_CURVE((1.02072197947249,1.02138328368541,1.02072197947249))
REPRESENTATION_ITEM('')
);
#18847=(
BOUNDED_CURVE()
B_SPLINE_CURVE(2,(#70390,#70391,#70392),.UNSPECIFIED.,.F.,.F.)
B_SPLINE_CURVE_WITH_KNOTS((3,3),(0.,0.0730837266089022),.UNSPECIFIED.)
CURVE()
GEOMETRIC_REPRESENTATION_ITEM()
RATIONAL_B_SPLINE_CURVE((1.,1.00000531286309,1.00000243585128))
REPRESENTATION_ITEM('')
);
#18848=(
BOUNDED_CURVE()
B_SPLINE_CURVE(2,(#70428,#70429,#70430),.UNSPECIFIED.,.F.,.F.)
B_SPLINE_CURVE_WITH_KNOTS((3,3),(0.984623166322172,1.26677639839308),
 .UNSPECIFIED.)
CURVE()
GEOMETRIC_REPRESENTATION_ITEM()
RATIONAL_B_SPLINE_CURVE((1.02072197947249,1.02138328368541,1.02072197947249))
REPRESENTATION_ITEM('')
);
#18849=(
BOUNDED_CURVE()
B_SPLINE_CURVE(2,(#70466,#70467,#70468),.UNSPECIFIED.,.F.,.F.)
B_SPLINE_CURVE_WITH_KNOTS((3,3),(0.,0.0730837266085706),.UNSPECIFIED.)
CURVE()
GEOMETRIC_REPRESENTATION_ITEM()
RATIONAL_B_SPLINE_CURVE((1.,1.00000531283577,1.00000243583875))
REPRESENTATION_ITEM('')
);
#18850=(
BOUNDED_CURVE()
B_SPLINE_CURVE(2,(#70504,#70505,#70506),.UNSPECIFIED.,.F.,.F.)
B_SPLINE_CURVE_WITH_KNOTS((3,3),(0.98462316632217,1.26677639839307),
 .UNSPECIFIED.)
CURVE()
GEOMETRIC_REPRESENTATION_ITEM()
RATIONAL_B_SPLINE_CURVE((1.02072197947249,1.02138328368541,1.02072197947249))
REPRESENTATION_ITEM('')
);
#18851=(
BOUNDED_CURVE()
B_SPLINE_CURVE(2,(#70542,#70543,#70544),.UNSPECIFIED.,.F.,.F.)
B_SPLINE_CURVE_WITH_KNOTS((3,3),(0.,0.0730837266086981),.UNSPECIFIED.)
CURVE()
GEOMETRIC_REPRESENTATION_ITEM()
RATIONAL_B_SPLINE_CURVE((1.,1.000005312841,1.00000243584115))
REPRESENTATION_ITEM('')
);
#18852=(
BOUNDED_CURVE()
B_SPLINE_CURVE(2,(#70580,#70581,#70582),.UNSPECIFIED.,.F.,.F.)
B_SPLINE_CURVE_WITH_KNOTS((3,3),(0.984623166322173,1.26677639839308),
 .UNSPECIFIED.)
CURVE()
GEOMETRIC_REPRESENTATION_ITEM()
RATIONAL_B_SPLINE_CURVE((1.02072197947249,1.02138328368541,1.02072197947249))
REPRESENTATION_ITEM('')
);
#18853=(
BOUNDED_CURVE()
B_SPLINE_CURVE(2,(#70618,#70619,#70620),.UNSPECIFIED.,.F.,.F.)
B_SPLINE_CURVE_WITH_KNOTS((3,3),(0.,0.0730837266081137),.UNSPECIFIED.)
CURVE()
GEOMETRIC_REPRESENTATION_ITEM()
RATIONAL_B_SPLINE_CURVE((1.,1.0000053128201,1.00000243583157))
REPRESENTATION_ITEM('')
);
#18854=(
BOUNDED_CURVE()
B_SPLINE_CURVE(2,(#70656,#70657,#70658),.UNSPECIFIED.,.F.,.F.)
B_SPLINE_CURVE_WITH_KNOTS((3,3),(0.98462316632217,1.26677639839307),
 .UNSPECIFIED.)
CURVE()
GEOMETRIC_REPRESENTATION_ITEM()
RATIONAL_B_SPLINE_CURVE((1.02072197947249,1.02138328368541,1.02072197947249))
REPRESENTATION_ITEM('')
);
#18855=(
BOUNDED_CURVE()
B_SPLINE_CURVE(2,(#70694,#70695,#70696),.UNSPECIFIED.,.F.,.F.)
B_SPLINE_CURVE_WITH_KNOTS((3,3),(0.,0.0730837266081729),.UNSPECIFIED.)
CURVE()
GEOMETRIC_REPRESENTATION_ITEM()
RATIONAL_B_SPLINE_CURVE((1.,1.00000531281639,1.00000243582987))
REPRESENTATION_ITEM('')
);
#18856=(
BOUNDED_CURVE()
B_SPLINE_CURVE(2,(#70732,#70733,#70734),.UNSPECIFIED.,.F.,.F.)
B_SPLINE_CURVE_WITH_KNOTS((3,3),(0.984623166322172,1.26677639839307),
 .UNSPECIFIED.)
CURVE()
GEOMETRIC_REPRESENTATION_ITEM()
RATIONAL_B_SPLINE_CURVE((1.02072197947249,1.0213832836854,1.02072197947249))
REPRESENTATION_ITEM('')
);
#18857=(
BOUNDED_CURVE()
B_SPLINE_CURVE(2,(#70770,#70771,#70772),.UNSPECIFIED.,.F.,.F.)
B_SPLINE_CURVE_WITH_KNOTS((3,3),(0.,0.0730837266080691),.UNSPECIFIED.)
CURVE()
GEOMETRIC_REPRESENTATION_ITEM()
RATIONAL_B_SPLINE_CURVE((1.,1.00000531281001,1.00000243582694))
REPRESENTATION_ITEM('')
);
#18858=(
BOUNDED_CURVE()
B_SPLINE_CURVE(2,(#70808,#70809,#70810),.UNSPECIFIED.,.F.,.F.)
B_SPLINE_CURVE_WITH_KNOTS((3,3),(0.984623166322169,1.26677639839307),
 .UNSPECIFIED.)
CURVE()
GEOMETRIC_REPRESENTATION_ITEM()
RATIONAL_B_SPLINE_CURVE((1.02072197947249,1.02138328368541,1.02072197947249))
REPRESENTATION_ITEM('')
);
#18859=(
BOUNDED_CURVE()
B_SPLINE_CURVE(2,(#70846,#70847,#70848),.UNSPECIFIED.,.F.,.F.)
B_SPLINE_CURVE_WITH_KNOTS((3,3),(0.,0.0730837266082608),.UNSPECIFIED.)
CURVE()
GEOMETRIC_REPRESENTATION_ITEM()
RATIONAL_B_SPLINE_CURVE((1.,1.00000531281977,1.00000243583142))
REPRESENTATION_ITEM('')
);
#18860=(
BOUNDED_CURVE()
B_SPLINE_CURVE(2,(#70884,#70885,#70886),.UNSPECIFIED.,.F.,.F.)
B_SPLINE_CURVE_WITH_KNOTS((3,3),(0.984623166322172,1.26677639839307),
 .UNSPECIFIED.)
CURVE()
GEOMETRIC_REPRESENTATION_ITEM()
RATIONAL_B_SPLINE_CURVE((1.02072197947249,1.02138328368541,1.02072197947249))
REPRESENTATION_ITEM('')
);
#18861=(
BOUNDED_CURVE()
B_SPLINE_CURVE(2,(#70922,#70923,#70924),.UNSPECIFIED.,.F.,.F.)
B_SPLINE_CURVE_WITH_KNOTS((3,3),(0.,0.0730837266082887),.UNSPECIFIED.)
CURVE()
GEOMETRIC_REPRESENTATION_ITEM()
RATIONAL_B_SPLINE_CURVE((1.,1.00000531281023,1.00000243582704))
REPRESENTATION_ITEM('')
);
#18862=(
BOUNDED_CURVE()
B_SPLINE_CURVE(2,(#70960,#70961,#70962),.UNSPECIFIED.,.F.,.F.)
B_SPLINE_CURVE_WITH_KNOTS((3,3),(0.984623166322172,1.26677639839307),
 .UNSPECIFIED.)
CURVE()
GEOMETRIC_REPRESENTATION_ITEM()
RATIONAL_B_SPLINE_CURVE((1.02072197947249,1.02138328368541,1.02072197947249))
REPRESENTATION_ITEM('')
);
#18863=(
BOUNDED_CURVE()
B_SPLINE_CURVE(2,(#70998,#70999,#71000),.UNSPECIFIED.,.F.,.F.)
B_SPLINE_CURVE_WITH_KNOTS((3,3),(0.,0.0730837266079997),.UNSPECIFIED.)
CURVE()
GEOMETRIC_REPRESENTATION_ITEM()
RATIONAL_B_SPLINE_CURVE((1.,1.00000531280928,1.0000024358266))
REPRESENTATION_ITEM('')
);
#18864=(
BOUNDED_CURVE()
B_SPLINE_CURVE(2,(#71036,#71037,#71038),.UNSPECIFIED.,.F.,.F.)
B_SPLINE_CURVE_WITH_KNOTS((3,3),(0.984623166322169,1.26677639839307),
 .UNSPECIFIED.)
CURVE()
GEOMETRIC_REPRESENTATION_ITEM()
RATIONAL_B_SPLINE_CURVE((1.02072197947249,1.02138328368541,1.02072197947249))
REPRESENTATION_ITEM('')
);
#18865=(
BOUNDED_CURVE()
B_SPLINE_CURVE(2,(#71074,#71075,#71076),.UNSPECIFIED.,.F.,.F.)
B_SPLINE_CURVE_WITH_KNOTS((3,3),(0.,0.0730837266086672),.UNSPECIFIED.)
CURVE()
GEOMETRIC_REPRESENTATION_ITEM()
RATIONAL_B_SPLINE_CURVE((1.,1.00000531284996,1.00000243584525))
REPRESENTATION_ITEM('')
);
#18866=(
BOUNDED_CURVE()
B_SPLINE_CURVE(2,(#71112,#71113,#71114),.UNSPECIFIED.,.F.,.F.)
B_SPLINE_CURVE_WITH_KNOTS((3,3),(0.984623166322172,1.26677639839307),
 .UNSPECIFIED.)
CURVE()
GEOMETRIC_REPRESENTATION_ITEM()
RATIONAL_B_SPLINE_CURVE((1.02072197947249,1.02138328368541,1.02072197947249))
REPRESENTATION_ITEM('')
);
#18867=(
BOUNDED_CURVE()
B_SPLINE_CURVE(2,(#71150,#71151,#71152),.UNSPECIFIED.,.F.,.F.)
B_SPLINE_CURVE_WITH_KNOTS((3,3),(0.,0.0730837266084481),.UNSPECIFIED.)
CURVE()
GEOMETRIC_REPRESENTATION_ITEM()
RATIONAL_B_SPLINE_CURVE((1.,1.00000531284005,1.00000243584071))
REPRESENTATION_ITEM('')
);
#18868=(
BOUNDED_CURVE()
B_SPLINE_CURVE(2,(#71188,#71189,#71190),.UNSPECIFIED.,.F.,.F.)
B_SPLINE_CURVE_WITH_KNOTS((3,3),(0.984623166322169,1.26677639839307),
 .UNSPECIFIED.)
CURVE()
GEOMETRIC_REPRESENTATION_ITEM()
RATIONAL_B_SPLINE_CURVE((1.02072197947249,1.02138328368541,1.02072197947249))
REPRESENTATION_ITEM('')
);
#18869=(
BOUNDED_CURVE()
B_SPLINE_CURVE(2,(#71226,#71227,#71228),.UNSPECIFIED.,.F.,.F.)
B_SPLINE_CURVE_WITH_KNOTS((3,3),(0.,0.073083726608594),.UNSPECIFIED.)
CURVE()
GEOMETRIC_REPRESENTATION_ITEM()
RATIONAL_B_SPLINE_CURVE((1.,1.00000531283215,1.00000243583709))
REPRESENTATION_ITEM('')
);
#18870=(
BOUNDED_CURVE()
B_SPLINE_CURVE(2,(#71264,#71265,#71266),.UNSPECIFIED.,.F.,.F.)
B_SPLINE_CURVE_WITH_KNOTS((3,3),(0.984623166322171,1.26677639839307),
 .UNSPECIFIED.)
CURVE()
GEOMETRIC_REPRESENTATION_ITEM()
RATIONAL_B_SPLINE_CURVE((1.02072197947249,1.02138328368541,1.02072197947249))
REPRESENTATION_ITEM('')
);
#18871=(
BOUNDED_CURVE()
B_SPLINE_CURVE(2,(#71302,#71303,#71304),.UNSPECIFIED.,.F.,.F.)
B_SPLINE_CURVE_WITH_KNOTS((3,3),(0.,0.0730837266086082),.UNSPECIFIED.)
CURVE()
GEOMETRIC_REPRESENTATION_ITEM()
RATIONAL_B_SPLINE_CURVE((1.,1.00000531285031,1.00000243584542))
REPRESENTATION_ITEM('')
);
#18872=(
BOUNDED_CURVE()
B_SPLINE_CURVE(2,(#71340,#71341,#71342),.UNSPECIFIED.,.F.,.F.)
B_SPLINE_CURVE_WITH_KNOTS((3,3),(0.984623166322171,1.26677639839307),
 .UNSPECIFIED.)
CURVE()
GEOMETRIC_REPRESENTATION_ITEM()
RATIONAL_B_SPLINE_CURVE((1.02072197947249,1.02138328368541,1.02072197947249))
REPRESENTATION_ITEM('')
);
#18873=(
BOUNDED_CURVE()
B_SPLINE_CURVE(2,(#71378,#71379,#71380),.UNSPECIFIED.,.F.,.F.)
B_SPLINE_CURVE_WITH_KNOTS((3,3),(0.,0.0730837266081729),.UNSPECIFIED.)
CURVE()
GEOMETRIC_REPRESENTATION_ITEM()
RATIONAL_B_SPLINE_CURVE((1.,1.00000531281639,1.00000243582987))
REPRESENTATION_ITEM('')
);
#18874=(
BOUNDED_CURVE()
B_SPLINE_CURVE(2,(#71416,#71417,#71418),.UNSPECIFIED.,.F.,.F.)
B_SPLINE_CURVE_WITH_KNOTS((3,3),(0.984623166322171,1.26677639839308),
 .UNSPECIFIED.)
CURVE()
GEOMETRIC_REPRESENTATION_ITEM()
RATIONAL_B_SPLINE_CURVE((1.02072197947249,1.02138328368541,1.02072197947249))
REPRESENTATION_ITEM('')
);
#18875=(
BOUNDED_CURVE()
B_SPLINE_CURVE(2,(#71454,#71455,#71456),.UNSPECIFIED.,.F.,.F.)
B_SPLINE_CURVE_WITH_KNOTS((3,3),(0.,0.0730837266083873),.UNSPECIFIED.)
CURVE()
GEOMETRIC_REPRESENTATION_ITEM()
RATIONAL_B_SPLINE_CURVE((1.,1.00000531281801,1.00000243583061))
REPRESENTATION_ITEM('')
);
#18876=(
BOUNDED_CURVE()
B_SPLINE_CURVE(2,(#71492,#71493,#71494),.UNSPECIFIED.,.F.,.F.)
B_SPLINE_CURVE_WITH_KNOTS((3,3),(0.984623166322171,1.26677639839307),
 .UNSPECIFIED.)
CURVE()
GEOMETRIC_REPRESENTATION_ITEM()
RATIONAL_B_SPLINE_CURVE((1.02072197947249,1.02138328368541,1.02072197947249))
REPRESENTATION_ITEM('')
);
#18877=(
BOUNDED_CURVE()
B_SPLINE_CURVE(2,(#71530,#71531,#71532),.UNSPECIFIED.,.F.,.F.)
B_SPLINE_CURVE_WITH_KNOTS((3,3),(0.,0.0730837266086276),.UNSPECIFIED.)
CURVE()
GEOMETRIC_REPRESENTATION_ITEM()
RATIONAL_B_SPLINE_CURVE((1.,1.00000531283797,1.00000243583976))
REPRESENTATION_ITEM('')
);
#18878=(
BOUNDED_CURVE()
B_SPLINE_CURVE(2,(#71540,#71541,#71542),.UNSPECIFIED.,.F.,.F.)
B_SPLINE_CURVE_WITH_KNOTS((3,3),(0.0522192481407343,0.300149053231598),
 .UNSPECIFIED.)
CURVE()
GEOMETRIC_REPRESENTATION_ITEM()
RATIONAL_B_SPLINE_CURVE((1.00002415803369,1.00006942852683,1.))
REPRESENTATION_ITEM('')
);
#18879=(
BOUNDED_CURVE()
B_SPLINE_CURVE(2,(#71543,#71544,#71545),.UNSPECIFIED.,.F.,.F.)
B_SPLINE_CURVE_WITH_KNOTS((3,3),(0.,0.247929805090937),.UNSPECIFIED.)
CURVE()
GEOMETRIC_REPRESENTATION_ITEM()
RATIONAL_B_SPLINE_CURVE((1.,1.00006942853014,1.00002415803485))
REPRESENTATION_ITEM('')
);
#18880=(
BOUNDED_CURVE()
B_SPLINE_CURVE(2,(#71550,#71551,#71552),.UNSPECIFIED.,.F.,.F.)
B_SPLINE_CURVE_WITH_KNOTS((3,3),(0.0522192481406321,0.300149053231599),
 .UNSPECIFIED.)
CURVE()
GEOMETRIC_REPRESENTATION_ITEM()
RATIONAL_B_SPLINE_CURVE((1.00002415803476,1.00006942852989,1.))
REPRESENTATION_ITEM('')
);
#18881=(
BOUNDED_CURVE()
B_SPLINE_CURVE(2,(#71553,#71554,#71555),.UNSPECIFIED.,.F.,.F.)
B_SPLINE_CURVE_WITH_KNOTS((3,3),(0.,0.247929805090946),.UNSPECIFIED.)
CURVE()
GEOMETRIC_REPRESENTATION_ITEM()
RATIONAL_B_SPLINE_CURVE((1.,1.00006942853077,1.00002415803506))
REPRESENTATION_ITEM('')
);
#18882=(
BOUNDED_CURVE()
B_SPLINE_CURVE(2,(#71560,#71561,#71562),.UNSPECIFIED.,.F.,.F.)
B_SPLINE_CURVE_WITH_KNOTS((3,3),(0.0522192481406271,0.300149053231598),
 .UNSPECIFIED.)
CURVE()
GEOMETRIC_REPRESENTATION_ITEM()
RATIONAL_B_SPLINE_CURVE((1.00002415803463,1.00006942852952,1.))
REPRESENTATION_ITEM('')
);
#18883=(
BOUNDED_CURVE()
B_SPLINE_CURVE(2,(#71563,#71564,#71565),.UNSPECIFIED.,.F.,.F.)
B_SPLINE_CURVE_WITH_KNOTS((3,3),(0.,0.247929805090861),.UNSPECIFIED.)
CURVE()
GEOMETRIC_REPRESENTATION_ITEM()
RATIONAL_B_SPLINE_CURVE((1.,1.00006942852808,1.00002415803413))
REPRESENTATION_ITEM('')
);
#18884=(
BOUNDED_CURVE()
B_SPLINE_CURVE(2,(#71570,#71571,#71572),.UNSPECIFIED.,.F.,.F.)
B_SPLINE_CURVE_WITH_KNOTS((3,3),(0.0522192481407297,0.300149053231598),
 .UNSPECIFIED.)
CURVE()
GEOMETRIC_REPRESENTATION_ITEM()
RATIONAL_B_SPLINE_CURVE((1.00002415803409,1.00006942852797,1.))
REPRESENTATION_ITEM('')
);
#18885=(
BOUNDED_CURVE()
B_SPLINE_CURVE(2,(#71573,#71574,#71575),.UNSPECIFIED.,.F.,.F.)
B_SPLINE_CURVE_WITH_KNOTS((3,3),(0.,0.247929805090852),.UNSPECIFIED.)
CURVE()
GEOMETRIC_REPRESENTATION_ITEM()
RATIONAL_B_SPLINE_CURVE((1.,1.00006942852787,1.00002415803405))
REPRESENTATION_ITEM('')
);
#18886=(
BOUNDED_CURVE()
B_SPLINE_CURVE(2,(#71580,#71581,#71582),.UNSPECIFIED.,.F.,.F.)
B_SPLINE_CURVE_WITH_KNOTS((3,3),(0.0522192481407573,0.300149053231599),
 .UNSPECIFIED.)
CURVE()
GEOMETRIC_REPRESENTATION_ITEM()
RATIONAL_B_SPLINE_CURVE((1.00002415803393,1.00006942852751,1.))
REPRESENTATION_ITEM('')
);
#18887=(
BOUNDED_CURVE()
B_SPLINE_CURVE(2,(#71583,#71584,#71585),.UNSPECIFIED.,.F.,.F.)
B_SPLINE_CURVE_WITH_KNOTS((3,3),(0.,0.247929805090877),.UNSPECIFIED.)
CURVE()
GEOMETRIC_REPRESENTATION_ITEM()
RATIONAL_B_SPLINE_CURVE((1.,1.00006942852796,1.00002415803409))
REPRESENTATION_ITEM('')
);
#18888=(
BOUNDED_CURVE()
B_SPLINE_CURVE(2,(#71590,#71591,#71592),.UNSPECIFIED.,.F.,.F.)
B_SPLINE_CURVE_WITH_KNOTS((3,3),(0.0522192481406628,0.300149053231599),
 .UNSPECIFIED.)
CURVE()
GEOMETRIC_REPRESENTATION_ITEM()
RATIONAL_B_SPLINE_CURVE((1.00002415803503,1.00006942853066,1.))
REPRESENTATION_ITEM('')
);
#18889=(
BOUNDED_CURVE()
B_SPLINE_CURVE(2,(#71593,#71594,#71595),.UNSPECIFIED.,.F.,.F.)
B_SPLINE_CURVE_WITH_KNOTS((3,3),(0.,0.247929805090816),.UNSPECIFIED.)
CURVE()
GEOMETRIC_REPRESENTATION_ITEM()
RATIONAL_B_SPLINE_CURVE((1.,1.00006942852647,1.00002415803357))
REPRESENTATION_ITEM('')
);
#18890=(
BOUNDED_CURVE()
B_SPLINE_CURVE(2,(#71600,#71601,#71602),.UNSPECIFIED.,.F.,.F.)
B_SPLINE_CURVE_WITH_KNOTS((3,3),(0.0522192481406917,0.300149053231598),
 .UNSPECIFIED.)
CURVE()
GEOMETRIC_REPRESENTATION_ITEM()
RATIONAL_B_SPLINE_CURVE((1.0000241580342,1.00006942852828,1.))
REPRESENTATION_ITEM('')
);
#18891=(
BOUNDED_CURVE()
B_SPLINE_CURVE(2,(#71603,#71604,#71605),.UNSPECIFIED.,.F.,.F.)
B_SPLINE_CURVE_WITH_KNOTS((3,3),(0.,0.247929805090809),.UNSPECIFIED.)
CURVE()
GEOMETRIC_REPRESENTATION_ITEM()
RATIONAL_B_SPLINE_CURVE((1.,1.0000694285267,1.00002415803365))
REPRESENTATION_ITEM('')
);
#18892=(
BOUNDED_CURVE()
B_SPLINE_CURVE(2,(#71610,#71611,#71612),.UNSPECIFIED.,.F.,.F.)
B_SPLINE_CURVE_WITH_KNOTS((3,3),(0.0522192481406725,0.300149053231599),
 .UNSPECIFIED.)
CURVE()
GEOMETRIC_REPRESENTATION_ITEM()
RATIONAL_B_SPLINE_CURVE((1.00002415803451,1.00006942852917,1.))
REPRESENTATION_ITEM('')
);
#18893=(
BOUNDED_CURVE()
B_SPLINE_CURVE(2,(#71613,#71614,#71615),.UNSPECIFIED.,.F.,.F.)
B_SPLINE_CURVE_WITH_KNOTS((3,3),(0.,0.247929805090887),.UNSPECIFIED.)
CURVE()
GEOMETRIC_REPRESENTATION_ITEM()
RATIONAL_B_SPLINE_CURVE((1.,1.00006942852972,1.0000241580347))
REPRESENTATION_ITEM('')
);
#18894=(
BOUNDED_CURVE()
B_SPLINE_CURVE(2,(#71620,#71621,#71622),.UNSPECIFIED.,.F.,.F.)
B_SPLINE_CURVE_WITH_KNOTS((3,3),(0.0522192481407858,0.300149053231598),
 .UNSPECIFIED.)
CURVE()
GEOMETRIC_REPRESENTATION_ITEM()
RATIONAL_B_SPLINE_CURVE((1.00002415803371,1.00006942852687,1.))
REPRESENTATION_ITEM('')
);
#18895=(
BOUNDED_CURVE()
B_SPLINE_CURVE(2,(#71623,#71624,#71625),.UNSPECIFIED.,.F.,.F.)
B_SPLINE_CURVE_WITH_KNOTS((3,3),(0.,0.247929805090891),.UNSPECIFIED.)
CURVE()
GEOMETRIC_REPRESENTATION_ITEM()
RATIONAL_B_SPLINE_CURVE((1.,1.00006942852915,1.0000241580345))
REPRESENTATION_ITEM('')
);
#18896=(
BOUNDED_CURVE()
B_SPLINE_CURVE(2,(#71630,#71631,#71632),.UNSPECIFIED.,.F.,.F.)
B_SPLINE_CURVE_WITH_KNOTS((3,3),(0.0522192481406479,0.300149053231599),
 .UNSPECIFIED.)
CURVE()
GEOMETRIC_REPRESENTATION_ITEM()
RATIONAL_B_SPLINE_CURVE((1.0000241580347,1.00006942852973,1.))
REPRESENTATION_ITEM('')
);
#18897=(
BOUNDED_CURVE()
B_SPLINE_CURVE(2,(#71633,#71634,#71635),.UNSPECIFIED.,.F.,.F.)
B_SPLINE_CURVE_WITH_KNOTS((3,3),(0.,0.24792980509089),.UNSPECIFIED.)
CURVE()
GEOMETRIC_REPRESENTATION_ITEM()
RATIONAL_B_SPLINE_CURVE((1.,1.0000694285297,1.00002415803469))
REPRESENTATION_ITEM('')
);
#18898=(
BOUNDED_CURVE()
B_SPLINE_CURVE(2,(#71640,#71641,#71642),.UNSPECIFIED.,.F.,.F.)
B_SPLINE_CURVE_WITH_KNOTS((3,3),(0.0522192481407442,0.300149053231599),
 .UNSPECIFIED.)
CURVE()
GEOMETRIC_REPRESENTATION_ITEM()
RATIONAL_B_SPLINE_CURVE((1.00002415803411,1.00006942852801,1.))
REPRESENTATION_ITEM('')
);
#18899=(
BOUNDED_CURVE()
B_SPLINE_CURVE(2,(#71643,#71644,#71645),.UNSPECIFIED.,.F.,.F.)
B_SPLINE_CURVE_WITH_KNOTS((3,3),(0.,0.247929805090961),.UNSPECIFIED.)
CURVE()
GEOMETRIC_REPRESENTATION_ITEM()
RATIONAL_B_SPLINE_CURVE((1.,1.00006942852871,1.00002415803435))
REPRESENTATION_ITEM('')
);
#18900=(
BOUNDED_CURVE()
B_SPLINE_CURVE(2,(#71650,#71651,#71652),.UNSPECIFIED.,.F.,.F.)
B_SPLINE_CURVE_WITH_KNOTS((3,3),(0.0522192481406183,0.300149053231598),
 .UNSPECIFIED.)
CURVE()
GEOMETRIC_REPRESENTATION_ITEM()
RATIONAL_B_SPLINE_CURVE((1.0000241580348,1.00006942853,1.))
REPRESENTATION_ITEM('')
);
#18901=(
BOUNDED_CURVE()
B_SPLINE_CURVE(2,(#71653,#71654,#71655),.UNSPECIFIED.,.F.,.F.)
B_SPLINE_CURVE_WITH_KNOTS((3,3),(0.,0.247929805090888),.UNSPECIFIED.)
CURVE()
GEOMETRIC_REPRESENTATION_ITEM()
RATIONAL_B_SPLINE_CURVE((1.,1.00006942852642,1.00002415803355))
REPRESENTATION_ITEM('')
);
#18902=(
BOUNDED_CURVE()
B_SPLINE_CURVE(2,(#71660,#71661,#71662),.UNSPECIFIED.,.F.,.F.)
B_SPLINE_CURVE_WITH_KNOTS((3,3),(0.0522192481406737,0.300149053231598),
 .UNSPECIFIED.)
CURVE()
GEOMETRIC_REPRESENTATION_ITEM()
RATIONAL_B_SPLINE_CURVE((1.00002415803462,1.00006942852949,1.))
REPRESENTATION_ITEM('')
);
#18903=(
BOUNDED_CURVE()
B_SPLINE_CURVE(2,(#71663,#71664,#71665),.UNSPECIFIED.,.F.,.F.)
B_SPLINE_CURVE_WITH_KNOTS((3,3),(0.,0.247929805090943),.UNSPECIFIED.)
CURVE()
GEOMETRIC_REPRESENTATION_ITEM()
RATIONAL_B_SPLINE_CURVE((1.,1.00006942852869,1.00002415803434))
REPRESENTATION_ITEM('')
);
#18904=(
BOUNDED_CURVE()
B_SPLINE_CURVE(2,(#71670,#71671,#71672),.UNSPECIFIED.,.F.,.F.)
B_SPLINE_CURVE_WITH_KNOTS((3,3),(0.0522192481407655,0.300149053231599),
 .UNSPECIFIED.)
CURVE()
GEOMETRIC_REPRESENTATION_ITEM()
RATIONAL_B_SPLINE_CURVE((1.00002415803309,1.00006942852508,1.))
REPRESENTATION_ITEM('')
);
#18905=(
BOUNDED_CURVE()
B_SPLINE_CURVE(2,(#71673,#71674,#71675),.UNSPECIFIED.,.F.,.F.)
B_SPLINE_CURVE_WITH_KNOTS((3,3),(0.,0.247929805090823),.UNSPECIFIED.)
CURVE()
GEOMETRIC_REPRESENTATION_ITEM()
RATIONAL_B_SPLINE_CURVE((1.,1.00006942852759,1.00002415803396))
REPRESENTATION_ITEM('')
);
#18906=(
BOUNDED_CURVE()
B_SPLINE_CURVE(2,(#71680,#71681,#71682),.UNSPECIFIED.,.F.,.F.)
B_SPLINE_CURVE_WITH_KNOTS((3,3),(0.0522192481406535,0.300149053231599),
 .UNSPECIFIED.)
CURVE()
GEOMETRIC_REPRESENTATION_ITEM()
RATIONAL_B_SPLINE_CURVE((1.0000241580346,1.00006942852943,1.))
REPRESENTATION_ITEM('')
);
#18907=(
BOUNDED_CURVE()
B_SPLINE_CURVE(2,(#71683,#71684,#71685),.UNSPECIFIED.,.F.,.F.)
B_SPLINE_CURVE_WITH_KNOTS((3,3),(0.,0.247929805090934),.UNSPECIFIED.)
CURVE()
GEOMETRIC_REPRESENTATION_ITEM()
RATIONAL_B_SPLINE_CURVE((1.,1.00006942852716,1.00002415803381))
REPRESENTATION_ITEM('')
);
#18908=(
BOUNDED_CURVE()
B_SPLINE_CURVE(2,(#71690,#71691,#71692),.UNSPECIFIED.,.F.,.F.)
B_SPLINE_CURVE_WITH_KNOTS((3,3),(0.0522192481407335,0.300149053231598),
 .UNSPECIFIED.)
CURVE()
GEOMETRIC_REPRESENTATION_ITEM()
RATIONAL_B_SPLINE_CURVE((1.00002415803399,1.00006942852769,1.))
REPRESENTATION_ITEM('')
);
#18909=(
BOUNDED_CURVE()
B_SPLINE_CURVE(2,(#71693,#71694,#71695),.UNSPECIFIED.,.F.,.F.)
B_SPLINE_CURVE_WITH_KNOTS((3,3),(0.,0.247929805090796),.UNSPECIFIED.)
CURVE()
GEOMETRIC_REPRESENTATION_ITEM()
RATIONAL_B_SPLINE_CURVE((1.,1.00006942852549,1.00002415803323))
REPRESENTATION_ITEM('')
);
#18910=(
BOUNDED_CURVE()
B_SPLINE_CURVE(2,(#71700,#71701,#71702),.UNSPECIFIED.,.F.,.F.)
B_SPLINE_CURVE_WITH_KNOTS((3,3),(0.0522192481408277,0.300149053231598),
 .UNSPECIFIED.)
CURVE()
GEOMETRIC_REPRESENTATION_ITEM()
RATIONAL_B_SPLINE_CURVE((1.00002415803309,1.00006942852509,1.))
REPRESENTATION_ITEM('')
);
#18911=(
BOUNDED_CURVE()
B_SPLINE_CURVE(2,(#71703,#71704,#71705),.UNSPECIFIED.,.F.,.F.)
B_SPLINE_CURVE_WITH_KNOTS((3,3),(0.,0.247929805090907),.UNSPECIFIED.)
CURVE()
GEOMETRIC_REPRESENTATION_ITEM()
RATIONAL_B_SPLINE_CURVE((1.,1.00006942852842,1.00002415803425))
REPRESENTATION_ITEM('')
);
#18912=(
BOUNDED_CURVE()
B_SPLINE_CURVE(2,(#71710,#71711,#71712),.UNSPECIFIED.,.F.,.F.)
B_SPLINE_CURVE_WITH_KNOTS((3,3),(0.0522192481406971,0.300149053231598),
 .UNSPECIFIED.)
CURVE()
GEOMETRIC_REPRESENTATION_ITEM()
RATIONAL_B_SPLINE_CURVE((1.00002415803424,1.00006942852841,1.))
REPRESENTATION_ITEM('')
);
#18913=(
BOUNDED_CURVE()
B_SPLINE_CURVE(2,(#71713,#71714,#71715),.UNSPECIFIED.,.F.,.F.)
B_SPLINE_CURVE_WITH_KNOTS((3,3),(0.,0.247929805090908),.UNSPECIFIED.)
CURVE()
GEOMETRIC_REPRESENTATION_ITEM()
RATIONAL_B_SPLINE_CURVE((1.,1.00006942852784,1.00002415803404))
REPRESENTATION_ITEM('')
);
#18914=(
BOUNDED_CURVE()
B_SPLINE_CURVE(2,(#71720,#71721,#71722),.UNSPECIFIED.,.F.,.F.)
B_SPLINE_CURVE_WITH_KNOTS((3,3),(0.0522192481407081,0.300149053231599),
 .UNSPECIFIED.)
CURVE()
GEOMETRIC_REPRESENTATION_ITEM()
RATIONAL_B_SPLINE_CURVE((1.00002415803401,1.00006942852773,1.))
REPRESENTATION_ITEM('')
);
#18915=(
BOUNDED_CURVE()
B_SPLINE_CURVE(2,(#71723,#71724,#71725),.UNSPECIFIED.,.F.,.F.)
B_SPLINE_CURVE_WITH_KNOTS((3,3),(0.,0.247929805090776),.UNSPECIFIED.)
CURVE()
GEOMETRIC_REPRESENTATION_ITEM()
RATIONAL_B_SPLINE_CURVE((1.,1.00006942852821,1.00002415803417))
REPRESENTATION_ITEM('')
);
#18916=(
BOUNDED_CURVE()
B_SPLINE_CURVE(2,(#71730,#71731,#71732),.UNSPECIFIED.,.F.,.F.)
B_SPLINE_CURVE_WITH_KNOTS((3,3),(0.0522192481407325,0.300149053231599),
 .UNSPECIFIED.)
CURVE()
GEOMETRIC_REPRESENTATION_ITEM()
RATIONAL_B_SPLINE_CURVE((1.00002415803403,1.0000694285278,1.))
REPRESENTATION_ITEM('')
);
#18917=(
BOUNDED_CURVE()
B_SPLINE_CURVE(2,(#71733,#71734,#71735),.UNSPECIFIED.,.F.,.F.)
B_SPLINE_CURVE_WITH_KNOTS((3,3),(0.,0.24792980509088),.UNSPECIFIED.)
CURVE()
GEOMETRIC_REPRESENTATION_ITEM()
RATIONAL_B_SPLINE_CURVE((1.,1.00006942852859,1.00002415803431))
REPRESENTATION_ITEM('')
);
#18918=(
BOUNDED_CURVE()
B_SPLINE_CURVE(2,(#71740,#71741,#71742),.UNSPECIFIED.,.F.,.F.)
B_SPLINE_CURVE_WITH_KNOTS((3,3),(0.0522192481407089,0.300149053231599),
 .UNSPECIFIED.)
CURVE()
GEOMETRIC_REPRESENTATION_ITEM()
RATIONAL_B_SPLINE_CURVE((1.00002415803469,1.00006942852969,1.))
REPRESENTATION_ITEM('')
);
#18919=(
BOUNDED_CURVE()
B_SPLINE_CURVE(2,(#71743,#71744,#71745),.UNSPECIFIED.,.F.,.F.)
B_SPLINE_CURVE_WITH_KNOTS((3,3),(0.,0.24792980509083),.UNSPECIFIED.)
CURVE()
GEOMETRIC_REPRESENTATION_ITEM()
RATIONAL_B_SPLINE_CURVE((1.,1.00006942852682,1.00002415803369))
REPRESENTATION_ITEM('')
);
#18920=(
BOUNDED_CURVE()
B_SPLINE_CURVE(2,(#71750,#71751,#71752),.UNSPECIFIED.,.F.,.F.)
B_SPLINE_CURVE_WITH_KNOTS((3,3),(0.0522192481406734,0.300149053231598),
 .UNSPECIFIED.)
CURVE()
GEOMETRIC_REPRESENTATION_ITEM()
RATIONAL_B_SPLINE_CURVE((1.00002415803462,1.0000694285295,1.))
REPRESENTATION_ITEM('')
);
#18921=(
BOUNDED_CURVE()
B_SPLINE_CURVE(2,(#71753,#71754,#71755),.UNSPECIFIED.,.F.,.F.)
B_SPLINE_CURVE_WITH_KNOTS((3,3),(0.,0.247929805090843),.UNSPECIFIED.)
CURVE()
GEOMETRIC_REPRESENTATION_ITEM()
RATIONAL_B_SPLINE_CURVE((1.,1.00006942852709,1.00002415803378))
REPRESENTATION_ITEM('')
);
#18922=(
BOUNDED_CURVE()
B_SPLINE_CURVE(2,(#71760,#71761,#71762),.UNSPECIFIED.,.F.,.F.)
B_SPLINE_CURVE_WITH_KNOTS((3,3),(0.0522192481406847,0.300149053231599),
 .UNSPECIFIED.)
CURVE()
GEOMETRIC_REPRESENTATION_ITEM()
RATIONAL_B_SPLINE_CURVE((1.00002415803482,1.00006942853006,1.))
REPRESENTATION_ITEM('')
);
#18923=(
BOUNDED_CURVE()
B_SPLINE_CURVE(2,(#71763,#71764,#71765),.UNSPECIFIED.,.F.,.F.)
B_SPLINE_CURVE_WITH_KNOTS((3,3),(0.,0.247929805090743),.UNSPECIFIED.)
CURVE()
GEOMETRIC_REPRESENTATION_ITEM()
RATIONAL_B_SPLINE_CURVE((1.,1.00006942852572,1.00002415803331))
REPRESENTATION_ITEM('')
);
#18924=(
BOUNDED_CURVE()
B_SPLINE_CURVE(2,(#71770,#71771,#71772),.UNSPECIFIED.,.F.,.F.)
B_SPLINE_CURVE_WITH_KNOTS((3,3),(0.0522192481406775,0.300149053231598),
 .UNSPECIFIED.)
CURVE()
GEOMETRIC_REPRESENTATION_ITEM()
RATIONAL_B_SPLINE_CURVE((1.00002415803416,1.00006942852817,1.))
REPRESENTATION_ITEM('')
);
#18925=(
BOUNDED_CURVE()
B_SPLINE_CURVE(2,(#71773,#71774,#71775),.UNSPECIFIED.,.F.,.F.)
B_SPLINE_CURVE_WITH_KNOTS((3,3),(0.,0.247929805090921),.UNSPECIFIED.)
CURVE()
GEOMETRIC_REPRESENTATION_ITEM()
RATIONAL_B_SPLINE_CURVE((1.,1.00006942852804,1.00002415803411))
REPRESENTATION_ITEM('')
);
#18926=(
BOUNDED_CURVE()
B_SPLINE_CURVE(2,(#71780,#71781,#71782),.UNSPECIFIED.,.F.,.F.)
B_SPLINE_CURVE_WITH_KNOTS((3,3),(0.0522192481406454,0.300149053231599),
 .UNSPECIFIED.)
CURVE()
GEOMETRIC_REPRESENTATION_ITEM()
RATIONAL_B_SPLINE_CURVE((1.0000241580342,1.00006942852828,1.))
REPRESENTATION_ITEM('')
);
#18927=(
BOUNDED_CURVE()
B_SPLINE_CURVE(2,(#71783,#71784,#71785),.UNSPECIFIED.,.F.,.F.)
B_SPLINE_CURVE_WITH_KNOTS((3,3),(0.,0.247929805090911),.UNSPECIFIED.)
CURVE()
GEOMETRIC_REPRESENTATION_ITEM()
RATIONAL_B_SPLINE_CURVE((1.,1.00006942852954,1.00002415803464))
REPRESENTATION_ITEM('')
);
#18928=(
BOUNDED_CURVE()
B_SPLINE_CURVE(2,(#71790,#71791,#71792),.UNSPECIFIED.,.F.,.F.)
B_SPLINE_CURVE_WITH_KNOTS((3,3),(0.0522192481406103,0.300149053231599),
 .UNSPECIFIED.)
CURVE()
GEOMETRIC_REPRESENTATION_ITEM()
RATIONAL_B_SPLINE_CURVE((1.00002415803486,1.00006942853019,1.))
REPRESENTATION_ITEM('')
);
#18929=(
BOUNDED_CURVE()
B_SPLINE_CURVE(2,(#71793,#71794,#71795),.UNSPECIFIED.,.F.,.F.)
B_SPLINE_CURVE_WITH_KNOTS((3,3),(0.,0.247929805090893),.UNSPECIFIED.)
CURVE()
GEOMETRIC_REPRESENTATION_ITEM()
RATIONAL_B_SPLINE_CURVE((1.,1.00006942853005,1.00002415803481))
REPRESENTATION_ITEM('')
);
#18930=(
BOUNDED_CURVE()
B_SPLINE_CURVE(2,(#71800,#71801,#71802),.UNSPECIFIED.,.F.,.F.)
B_SPLINE_CURVE_WITH_KNOTS((3,3),(0.0522192481407398,0.300149053231598),
 .UNSPECIFIED.)
CURVE()
GEOMETRIC_REPRESENTATION_ITEM()
RATIONAL_B_SPLINE_CURVE((1.0000241580337,1.00006942852686,1.))
REPRESENTATION_ITEM('')
);
#18931=(
BOUNDED_CURVE()
B_SPLINE_CURVE(2,(#71803,#71804,#71805),.UNSPECIFIED.,.F.,.F.)
B_SPLINE_CURVE_WITH_KNOTS((3,3),(0.,0.247929805090968),.UNSPECIFIED.)
CURVE()
GEOMETRIC_REPRESENTATION_ITEM()
RATIONAL_B_SPLINE_CURVE((1.,1.00006942852967,1.00002415803468))
REPRESENTATION_ITEM('')
);
#18932=(
BOUNDED_CURVE()
B_SPLINE_CURVE(2,(#71810,#71811,#71812),.UNSPECIFIED.,.F.,.F.)
B_SPLINE_CURVE_WITH_KNOTS((3,3),(0.0522192481406895,0.300149053231599),
 .UNSPECIFIED.)
CURVE()
GEOMETRIC_REPRESENTATION_ITEM()
RATIONAL_B_SPLINE_CURVE((1.00002415803463,1.00006942852952,1.))
REPRESENTATION_ITEM('')
);
#18933=(
BOUNDED_CURVE()
B_SPLINE_CURVE(2,(#71813,#71814,#71815),.UNSPECIFIED.,.F.,.F.)
B_SPLINE_CURVE_WITH_KNOTS((3,3),(0.,0.247929805090878),.UNSPECIFIED.)
CURVE()
GEOMETRIC_REPRESENTATION_ITEM()
RATIONAL_B_SPLINE_CURVE((1.,1.00006942852936,1.00002415803458))
REPRESENTATION_ITEM('')
);
#18934=(
BOUNDED_CURVE()
B_SPLINE_CURVE(2,(#71820,#71821,#71822),.UNSPECIFIED.,.F.,.F.)
B_SPLINE_CURVE_WITH_KNOTS((3,3),(0.0522192481406974,0.300149053231598),
 .UNSPECIFIED.)
CURVE()
GEOMETRIC_REPRESENTATION_ITEM()
RATIONAL_B_SPLINE_CURVE((1.00002415803451,1.00006942852919,1.))
REPRESENTATION_ITEM('')
);
#18935=(
BOUNDED_CURVE()
B_SPLINE_CURVE(2,(#71823,#71824,#71825),.UNSPECIFIED.,.F.,.F.)
B_SPLINE_CURVE_WITH_KNOTS((3,3),(0.,0.247929805090898),.UNSPECIFIED.)
CURVE()
GEOMETRIC_REPRESENTATION_ITEM()
RATIONAL_B_SPLINE_CURVE((1.,1.00006942852895,1.00002415803443))
REPRESENTATION_ITEM('')
);
#18936=(
BOUNDED_CURVE()
B_SPLINE_CURVE(2,(#71830,#71831,#71832),.UNSPECIFIED.,.F.,.F.)
B_SPLINE_CURVE_WITH_KNOTS((3,3),(0.0522192481407298,0.300149053231598),
 .UNSPECIFIED.)
CURVE()
GEOMETRIC_REPRESENTATION_ITEM()
RATIONAL_B_SPLINE_CURVE((1.00002415803412,1.00006942852805,1.))
REPRESENTATION_ITEM('')
);
#18937=(
BOUNDED_CURVE()
B_SPLINE_CURVE(2,(#71833,#71834,#71835),.UNSPECIFIED.,.F.,.F.)
B_SPLINE_CURVE_WITH_KNOTS((3,3),(0.,0.247929805090915),.UNSPECIFIED.)
CURVE()
GEOMETRIC_REPRESENTATION_ITEM()
RATIONAL_B_SPLINE_CURVE((1.,1.00006942852918,1.00002415803451))
REPRESENTATION_ITEM('')
);
#18938=(
BOUNDED_CURVE()
B_SPLINE_CURVE(2,(#71840,#71841,#71842),.UNSPECIFIED.,.F.,.F.)
B_SPLINE_CURVE_WITH_KNOTS((3,3),(0.0522192481407133,0.300149053231598),
 .UNSPECIFIED.)
CURVE()
GEOMETRIC_REPRESENTATION_ITEM()
RATIONAL_B_SPLINE_CURVE((1.00002415803458,1.00006942852939,1.))
REPRESENTATION_ITEM('')
);
#18939=(
BOUNDED_CURVE()
B_SPLINE_CURVE(2,(#71843,#71844,#71845),.UNSPECIFIED.,.F.,.F.)
B_SPLINE_CURVE_WITH_KNOTS((3,3),(0.,0.247929805090875),.UNSPECIFIED.)
CURVE()
GEOMETRIC_REPRESENTATION_ITEM()
RATIONAL_B_SPLINE_CURVE((1.,1.00006942852786,1.00002415803405))
REPRESENTATION_ITEM('')
);
#18940=(
BOUNDED_CURVE()
B_SPLINE_CURVE(2,(#71850,#71851,#71852),.UNSPECIFIED.,.F.,.F.)
B_SPLINE_CURVE_WITH_KNOTS((3,3),(0.0522192481407655,0.300149053231599),
 .UNSPECIFIED.)
CURVE()
GEOMETRIC_REPRESENTATION_ITEM()
RATIONAL_B_SPLINE_CURVE((1.00002415803309,1.00006942852508,1.))
REPRESENTATION_ITEM('')
);
#18941=(
BOUNDED_CURVE()
B_SPLINE_CURVE(2,(#71853,#71854,#71855),.UNSPECIFIED.,.F.,.F.)
B_SPLINE_CURVE_WITH_KNOTS((3,3),(0.,0.247929805090823),.UNSPECIFIED.)
CURVE()
GEOMETRIC_REPRESENTATION_ITEM()
RATIONAL_B_SPLINE_CURVE((1.,1.00006942852759,1.00002415803396))
REPRESENTATION_ITEM('')
);
#18942=(
BOUNDED_CURVE()
B_SPLINE_CURVE(2,(#71860,#71861,#71862),.UNSPECIFIED.,.F.,.F.)
B_SPLINE_CURVE_WITH_KNOTS((3,3),(0.0522192481406882,0.300149053231598),
 .UNSPECIFIED.)
CURVE()
GEOMETRIC_REPRESENTATION_ITEM()
RATIONAL_B_SPLINE_CURVE((1.00002415803415,1.00006942852814,1.))
REPRESENTATION_ITEM('')
);
#18943=(
BOUNDED_CURVE()
B_SPLINE_CURVE(2,(#71863,#71864,#71865),.UNSPECIFIED.,.F.,.F.)
B_SPLINE_CURVE_WITH_KNOTS((3,3),(0.,0.247929805090945),.UNSPECIFIED.)
CURVE()
GEOMETRIC_REPRESENTATION_ITEM()
RATIONAL_B_SPLINE_CURVE((1.,1.00006942852919,1.00002415803451))
REPRESENTATION_ITEM('')
);
#18944=(
BOUNDED_CURVE()
B_SPLINE_CURVE(2,(#71870,#71871,#71872),.UNSPECIFIED.,.F.,.F.)
B_SPLINE_CURVE_WITH_KNOTS((3,3),(0.0522192481406479,0.300149053231598),
 .UNSPECIFIED.)
CURVE()
GEOMETRIC_REPRESENTATION_ITEM()
RATIONAL_B_SPLINE_CURVE((1.00002415803429,1.00006942852855,1.))
REPRESENTATION_ITEM('')
);
#18945=(
BOUNDED_CURVE()
B_SPLINE_CURVE(2,(#71873,#71874,#71875),.UNSPECIFIED.,.F.,.F.)
B_SPLINE_CURVE_WITH_KNOTS((3,3),(0.,0.2479298050909),.UNSPECIFIED.)
CURVE()
GEOMETRIC_REPRESENTATION_ITEM()
RATIONAL_B_SPLINE_CURVE((1.,1.00006942852908,1.00002415803448))
REPRESENTATION_ITEM('')
);
#18946=(
BOUNDED_CURVE()
B_SPLINE_CURVE(2,(#71880,#71881,#71882),.UNSPECIFIED.,.F.,.F.)
B_SPLINE_CURVE_WITH_KNOTS((3,3),(0.052219248140666,0.300149053231598),
 .UNSPECIFIED.)
CURVE()
GEOMETRIC_REPRESENTATION_ITEM()
RATIONAL_B_SPLINE_CURVE((1.0000241580347,1.00006942852973,1.))
REPRESENTATION_ITEM('')
);
#18947=(
BOUNDED_CURVE()
B_SPLINE_CURVE(2,(#71883,#71884,#71885),.UNSPECIFIED.,.F.,.F.)
B_SPLINE_CURVE_WITH_KNOTS((3,3),(0.,0.247929805090926),.UNSPECIFIED.)
CURVE()
GEOMETRIC_REPRESENTATION_ITEM()
RATIONAL_B_SPLINE_CURVE((1.,1.00006942852844,1.00002415803425))
REPRESENTATION_ITEM('')
);
#18948=(
BOUNDED_CURVE()
B_SPLINE_CURVE(2,(#71890,#71891,#71892),.UNSPECIFIED.,.F.,.F.)
B_SPLINE_CURVE_WITH_KNOTS((3,3),(0.05221924814067,0.300149053231598),
 .UNSPECIFIED.)
CURVE()
GEOMETRIC_REPRESENTATION_ITEM()
RATIONAL_B_SPLINE_CURVE((1.0000241580343,1.00006942852856,1.))
REPRESENTATION_ITEM('')
);
#18949=(
BOUNDED_CURVE()
B_SPLINE_CURVE(2,(#71893,#71894,#71895),.UNSPECIFIED.,.F.,.F.)
B_SPLINE_CURVE_WITH_KNOTS((3,3),(0.,0.247929805090796),.UNSPECIFIED.)
CURVE()
GEOMETRIC_REPRESENTATION_ITEM()
RATIONAL_B_SPLINE_CURVE((1.,1.0000694285271,1.00002415803379))
REPRESENTATION_ITEM('')
);
#18950=(
BOUNDED_CURVE()
B_SPLINE_CURVE(2,(#71902,#71903,#71904),.UNSPECIFIED.,.F.,.F.)
B_SPLINE_CURVE_WITH_KNOTS((3,3),(0.,0.0730837266077788),.UNSPECIFIED.)
CURVE()
GEOMETRIC_REPRESENTATION_ITEM()
RATIONAL_B_SPLINE_CURVE((1.,1.00000531280199,1.00000243582326))
REPRESENTATION_ITEM('')
);
#18951=(
BOUNDED_CURVE()
B_SPLINE_CURVE(2,(#71914,#71915,#71916),.UNSPECIFIED.,.F.,.F.)
B_SPLINE_CURVE_WITH_KNOTS((3,3),(0.,0.0730837266081571),.UNSPECIFIED.)
CURVE()
GEOMETRIC_REPRESENTATION_ITEM()
RATIONAL_B_SPLINE_CURVE((1.,1.00000531282708,1.00000243583477))
REPRESENTATION_ITEM('')
);
#18952=(
BOUNDED_CURVE()
B_SPLINE_CURVE(2,(#71926,#71927,#71928),.UNSPECIFIED.,.F.,.F.)
B_SPLINE_CURVE_WITH_KNOTS((3,3),(0.,0.0730837266086552),.UNSPECIFIED.)
CURVE()
GEOMETRIC_REPRESENTATION_ITEM()
RATIONAL_B_SPLINE_CURVE((1.,1.00000531285702,1.0000024358485))
REPRESENTATION_ITEM('')
);
#18953=(
BOUNDED_CURVE()
B_SPLINE_CURVE(2,(#71938,#71939,#71940),.UNSPECIFIED.,.F.,.F.)
B_SPLINE_CURVE_WITH_KNOTS((3,3),(0.,0.0730837266083511),.UNSPECIFIED.)
CURVE()
GEOMETRIC_REPRESENTATION_ITEM()
RATIONAL_B_SPLINE_CURVE((1.,1.00000531283583,1.00000243583878))
REPRESENTATION_ITEM('')
);
#18954=(
BOUNDED_CURVE()
B_SPLINE_CURVE(2,(#71950,#71951,#71952),.UNSPECIFIED.,.F.,.F.)
B_SPLINE_CURVE_WITH_KNOTS((3,3),(0.,0.0730837266086366),.UNSPECIFIED.)
CURVE()
GEOMETRIC_REPRESENTATION_ITEM()
RATIONAL_B_SPLINE_CURVE((1.,1.00000531282378,1.00000243583325))
REPRESENTATION_ITEM('')
);
#18955=(
BOUNDED_CURVE()
B_SPLINE_CURVE(2,(#71962,#71963,#71964),.UNSPECIFIED.,.F.,.F.)
B_SPLINE_CURVE_WITH_KNOTS((3,3),(0.,0.0730837266082308),.UNSPECIFIED.)
CURVE()
GEOMETRIC_REPRESENTATION_ITEM()
RATIONAL_B_SPLINE_CURVE((1.,1.00000531281989,1.00000243583147))
REPRESENTATION_ITEM('')
);
#18956=(
BOUNDED_CURVE()
B_SPLINE_CURVE(2,(#71974,#71975,#71976),.UNSPECIFIED.,.F.,.F.)
B_SPLINE_CURVE_WITH_KNOTS((3,3),(0.,0.0730837266084392),.UNSPECIFIED.)
CURVE()
GEOMETRIC_REPRESENTATION_ITEM()
RATIONAL_B_SPLINE_CURVE((1.,1.00000531283989,1.00000243584064))
REPRESENTATION_ITEM('')
);
#18957=(
BOUNDED_CURVE()
B_SPLINE_CURVE(2,(#71986,#71987,#71988),.UNSPECIFIED.,.F.,.F.)
B_SPLINE_CURVE_WITH_KNOTS((3,3),(0.,0.0730837266081689),.UNSPECIFIED.)
CURVE()
GEOMETRIC_REPRESENTATION_ITEM()
RATIONAL_B_SPLINE_CURVE((1.,1.00000531283784,1.0000024358397))
REPRESENTATION_ITEM('')
);
#18958=(
BOUNDED_CURVE()
B_SPLINE_CURVE(2,(#71998,#71999,#72000),.UNSPECIFIED.,.F.,.F.)
B_SPLINE_CURVE_WITH_KNOTS((3,3),(0.,0.0730837266082052),.UNSPECIFIED.)
CURVE()
GEOMETRIC_REPRESENTATION_ITEM()
RATIONAL_B_SPLINE_CURVE((1.,1.00000531284527,1.00000243584311))
REPRESENTATION_ITEM('')
);
#18959=(
BOUNDED_CURVE()
B_SPLINE_CURVE(2,(#72010,#72011,#72012),.UNSPECIFIED.,.F.,.F.)
B_SPLINE_CURVE_WITH_KNOTS((3,3),(0.,0.0730837266083936),.UNSPECIFIED.)
CURVE()
GEOMETRIC_REPRESENTATION_ITEM()
RATIONAL_B_SPLINE_CURVE((1.,1.00000531284332,1.00000243584221))
REPRESENTATION_ITEM('')
);
#18960=(
BOUNDED_CURVE()
B_SPLINE_CURVE(2,(#72022,#72023,#72024),.UNSPECIFIED.,.F.,.F.)
B_SPLINE_CURVE_WITH_KNOTS((3,3),(0.,0.073083726608569),.UNSPECIFIED.)
CURVE()
GEOMETRIC_REPRESENTATION_ITEM()
RATIONAL_B_SPLINE_CURVE((1.,1.00000531285339,1.00000243584683))
REPRESENTATION_ITEM('')
);
#18961=(
BOUNDED_CURVE()
B_SPLINE_CURVE(2,(#72034,#72035,#72036),.UNSPECIFIED.,.F.,.F.)
B_SPLINE_CURVE_WITH_KNOTS((3,3),(0.,0.0730837266082845),.UNSPECIFIED.)
CURVE()
GEOMETRIC_REPRESENTATION_ITEM()
RATIONAL_B_SPLINE_CURVE((1.,1.00000531285795,1.00000243584892))
REPRESENTATION_ITEM('')
);
#18962=(
BOUNDED_CURVE()
B_SPLINE_CURVE(2,(#72046,#72047,#72048),.UNSPECIFIED.,.F.,.F.)
B_SPLINE_CURVE_WITH_KNOTS((3,3),(0.,0.0730837266087279),.UNSPECIFIED.)
CURVE()
GEOMETRIC_REPRESENTATION_ITEM()
RATIONAL_B_SPLINE_CURVE((1.,1.00000531284088,1.00000243584109))
REPRESENTATION_ITEM('')
);
#18963=(
BOUNDED_CURVE()
B_SPLINE_CURVE(2,(#72058,#72059,#72060),.UNSPECIFIED.,.F.,.F.)
B_SPLINE_CURVE_WITH_KNOTS((3,3),(0.,0.07308372660842),.UNSPECIFIED.)
CURVE()
GEOMETRIC_REPRESENTATION_ITEM()
RATIONAL_B_SPLINE_CURVE((1.,1.0000053128307,1.00000243583643))
REPRESENTATION_ITEM('')
);
#18964=(
BOUNDED_CURVE()
B_SPLINE_CURVE(2,(#72070,#72071,#72072),.UNSPECIFIED.,.F.,.F.)
B_SPLINE_CURVE_WITH_KNOTS((3,3),(0.,0.0730837266082381),.UNSPECIFIED.)
CURVE()
GEOMETRIC_REPRESENTATION_ITEM()
RATIONAL_B_SPLINE_CURVE((1.,1.00000531281961,1.00000243583134))
REPRESENTATION_ITEM('')
);
#18965=(
BOUNDED_CURVE()
B_SPLINE_CURVE(2,(#72082,#72083,#72084),.UNSPECIFIED.,.F.,.F.)
B_SPLINE_CURVE_WITH_KNOTS((3,3),(0.,0.0730837266082899),.UNSPECIFIED.)
CURVE()
GEOMETRIC_REPRESENTATION_ITEM()
RATIONAL_B_SPLINE_CURVE((1.,1.00000531282543,1.00000243583401))
REPRESENTATION_ITEM('')
);
#18966=(
BOUNDED_CURVE()
B_SPLINE_CURVE(2,(#72094,#72095,#72096),.UNSPECIFIED.,.F.,.F.)
B_SPLINE_CURVE_WITH_KNOTS((3,3),(0.,0.07308372660794),.UNSPECIFIED.)
CURVE()
GEOMETRIC_REPRESENTATION_ITEM()
RATIONAL_B_SPLINE_CURVE((1.,1.0000053128172,1.00000243583024))
REPRESENTATION_ITEM('')
);
#18967=(
BOUNDED_CURVE()
B_SPLINE_CURVE(2,(#72106,#72107,#72108),.UNSPECIFIED.,.F.,.F.)
B_SPLINE_CURVE_WITH_KNOTS((3,3),(0.,0.0730837266081521),.UNSPECIFIED.)
CURVE()
GEOMETRIC_REPRESENTATION_ITEM()
RATIONAL_B_SPLINE_CURVE((1.,1.00000531282239,1.00000243583262))
REPRESENTATION_ITEM('')
);
#18968=(
BOUNDED_CURVE()
B_SPLINE_CURVE(2,(#72118,#72119,#72120),.UNSPECIFIED.,.F.,.F.)
B_SPLINE_CURVE_WITH_KNOTS((3,3),(0.,0.0730837266086474),.UNSPECIFIED.)
CURVE()
GEOMETRIC_REPRESENTATION_ITEM()
RATIONAL_B_SPLINE_CURVE((1.,1.00000531283521,1.0000024358385))
REPRESENTATION_ITEM('')
);
#18969=(
BOUNDED_CURVE()
B_SPLINE_CURVE(2,(#72130,#72131,#72132),.UNSPECIFIED.,.F.,.F.)
B_SPLINE_CURVE_WITH_KNOTS((3,3),(0.,0.0730837266084578),.UNSPECIFIED.)
CURVE()
GEOMETRIC_REPRESENTATION_ITEM()
RATIONAL_B_SPLINE_CURVE((1.,1.00000531285618,1.00000243584811))
REPRESENTATION_ITEM('')
);
#18970=(
BOUNDED_CURVE()
B_SPLINE_CURVE(2,(#72142,#72143,#72144),.UNSPECIFIED.,.F.,.F.)
B_SPLINE_CURVE_WITH_KNOTS((3,3),(0.,0.0730837266085192),.UNSPECIFIED.)
CURVE()
GEOMETRIC_REPRESENTATION_ITEM()
RATIONAL_B_SPLINE_CURVE((1.,1.0000053128433,1.0000024358422))
REPRESENTATION_ITEM('')
);
#18971=(
BOUNDED_CURVE()
B_SPLINE_CURVE(2,(#72154,#72155,#72156),.UNSPECIFIED.,.F.,.F.)
B_SPLINE_CURVE_WITH_KNOTS((3,3),(0.,0.0730837266085013),.UNSPECIFIED.)
CURVE()
GEOMETRIC_REPRESENTATION_ITEM()
RATIONAL_B_SPLINE_CURVE((1.,1.00000531284403,1.00000243584254))
REPRESENTATION_ITEM('')
);
#18972=(
BOUNDED_CURVE()
B_SPLINE_CURVE(2,(#72166,#72167,#72168),.UNSPECIFIED.,.F.,.F.)
B_SPLINE_CURVE_WITH_KNOTS((3,3),(0.,0.0730837266088684),.UNSPECIFIED.)
CURVE()
GEOMETRIC_REPRESENTATION_ITEM()
RATIONAL_B_SPLINE_CURVE((1.,1.00000531283876,1.00000243584012))
REPRESENTATION_ITEM('')
);
#18973=(
BOUNDED_CURVE()
B_SPLINE_CURVE(2,(#72178,#72179,#72180),.UNSPECIFIED.,.F.,.F.)
B_SPLINE_CURVE_WITH_KNOTS((3,3),(0.,0.0730837266083975),.UNSPECIFIED.)
CURVE()
GEOMETRIC_REPRESENTATION_ITEM()
RATIONAL_B_SPLINE_CURVE((1.,1.00000531281974,1.0000024358314))
REPRESENTATION_ITEM('')
);
#18974=(
BOUNDED_CURVE()
B_SPLINE_CURVE(2,(#72190,#72191,#72192),.UNSPECIFIED.,.F.,.F.)
B_SPLINE_CURVE_WITH_KNOTS((3,3),(0.,0.0730837266088218),.UNSPECIFIED.)
CURVE()
GEOMETRIC_REPRESENTATION_ITEM()
RATIONAL_B_SPLINE_CURVE((1.,1.00000531283784,1.0000024358397))
REPRESENTATION_ITEM('')
);
#18975=(
BOUNDED_CURVE()
B_SPLINE_CURVE(2,(#72202,#72203,#72204),.UNSPECIFIED.,.F.,.F.)
B_SPLINE_CURVE_WITH_KNOTS((3,3),(0.,0.0730837266083783),.UNSPECIFIED.)
CURVE()
GEOMETRIC_REPRESENTATION_ITEM()
RATIONAL_B_SPLINE_CURVE((1.,1.00000531283749,1.00000243583954))
REPRESENTATION_ITEM('')
);
#18976=(
BOUNDED_CURVE()
B_SPLINE_CURVE(2,(#72214,#72215,#72216),.UNSPECIFIED.,.F.,.F.)
B_SPLINE_CURVE_WITH_KNOTS((3,3),(0.,0.0730837266082154),.UNSPECIFIED.)
CURVE()
GEOMETRIC_REPRESENTATION_ITEM()
RATIONAL_B_SPLINE_CURVE((1.,1.00000531284379,1.00000243584243))
REPRESENTATION_ITEM('')
);
#18977=(
BOUNDED_CURVE()
B_SPLINE_CURVE(2,(#72226,#72227,#72228),.UNSPECIFIED.,.F.,.F.)
B_SPLINE_CURVE_WITH_KNOTS((3,3),(0.,0.0730837266084736),.UNSPECIFIED.)
CURVE()
GEOMETRIC_REPRESENTATION_ITEM()
RATIONAL_B_SPLINE_CURVE((1.,1.00000531282395,1.00000243583333))
REPRESENTATION_ITEM('')
);
#18978=(
BOUNDED_CURVE()
B_SPLINE_CURVE(2,(#72238,#72239,#72240),.UNSPECIFIED.,.F.,.F.)
B_SPLINE_CURVE_WITH_KNOTS((3,3),(0.,0.0730837266084901),.UNSPECIFIED.)
CURVE()
GEOMETRIC_REPRESENTATION_ITEM()
RATIONAL_B_SPLINE_CURVE((1.,1.00000531285787,1.00000243584888))
REPRESENTATION_ITEM('')
);
#18979=(
BOUNDED_CURVE()
B_SPLINE_CURVE(2,(#72250,#72251,#72252),.UNSPECIFIED.,.F.,.F.)
B_SPLINE_CURVE_WITH_KNOTS((3,3),(0.,0.0730837266088617),.UNSPECIFIED.)
CURVE()
GEOMETRIC_REPRESENTATION_ITEM()
RATIONAL_B_SPLINE_CURVE((1.,1.00000531286035,1.00000243585002))
REPRESENTATION_ITEM('')
);
#18980=(
BOUNDED_CURVE()
B_SPLINE_CURVE(2,(#72262,#72263,#72264),.UNSPECIFIED.,.F.,.F.)
B_SPLINE_CURVE_WITH_KNOTS((3,3),(0.,0.0730837266085078),.UNSPECIFIED.)
CURVE()
GEOMETRIC_REPRESENTATION_ITEM()
RATIONAL_B_SPLINE_CURVE((1.,1.00000531283572,1.00000243583873))
REPRESENTATION_ITEM('')
);
#18981=(
BOUNDED_CURVE()
B_SPLINE_CURVE(2,(#72274,#72275,#72276),.UNSPECIFIED.,.F.,.F.)
B_SPLINE_CURVE_WITH_KNOTS((3,3),(0.,0.0730837266082782),.UNSPECIFIED.)
CURVE()
GEOMETRIC_REPRESENTATION_ITEM()
RATIONAL_B_SPLINE_CURVE((1.,1.00000531280434,1.00000243582434))
REPRESENTATION_ITEM('')
);
#18982=(
BOUNDED_CURVE()
B_SPLINE_CURVE(2,(#72286,#72287,#72288),.UNSPECIFIED.,.F.,.F.)
B_SPLINE_CURVE_WITH_KNOTS((3,3),(0.,0.0730837266084148),.UNSPECIFIED.)
CURVE()
GEOMETRIC_REPRESENTATION_ITEM()
RATIONAL_B_SPLINE_CURVE((1.,1.00000531285132,1.00000243584588))
REPRESENTATION_ITEM('')
);
#18983=(
BOUNDED_CURVE()
B_SPLINE_CURVE(2,(#72298,#72299,#72300),.UNSPECIFIED.,.F.,.F.)
B_SPLINE_CURVE_WITH_KNOTS((3,3),(0.,0.0730837266088265),.UNSPECIFIED.)
CURVE()
GEOMETRIC_REPRESENTATION_ITEM()
RATIONAL_B_SPLINE_CURVE((1.,1.00000531285575,1.00000243584791))
REPRESENTATION_ITEM('')
);
#18984=(
BOUNDED_CURVE()
B_SPLINE_CURVE(2,(#72310,#72311,#72312),.UNSPECIFIED.,.F.,.F.)
B_SPLINE_CURVE_WITH_KNOTS((3,3),(0.,0.0730837266080522),.UNSPECIFIED.)
CURVE()
GEOMETRIC_REPRESENTATION_ITEM()
RATIONAL_B_SPLINE_CURVE((1.,1.00000531282666,1.00000243583457))
REPRESENTATION_ITEM('')
);
#18985=(
BOUNDED_CURVE()
B_SPLINE_CURVE(2,(#72322,#72323,#72324),.UNSPECIFIED.,.F.,.F.)
B_SPLINE_CURVE_WITH_KNOTS((3,3),(0.,0.0730837266080658),.UNSPECIFIED.)
CURVE()
GEOMETRIC_REPRESENTATION_ITEM()
RATIONAL_B_SPLINE_CURVE((1.,1.00000531283637,1.00000243583903))
REPRESENTATION_ITEM('')
);
#18986=(
BOUNDED_CURVE()
B_SPLINE_CURVE(2,(#72478,#72479,#72480),.UNSPECIFIED.,.F.,.F.)
B_SPLINE_CURVE_WITH_KNOTS((3,3),(0.021736728690041,0.0948204552983262),
 .UNSPECIFIED.)
CURVE()
GEOMETRIC_REPRESENTATION_ITEM()
RATIONAL_B_SPLINE_CURVE((1.00000243583482,1.00000531282719,1.))
REPRESENTATION_ITEM('')
);
#18987=(
BOUNDED_CURVE()
B_SPLINE_CURVE(2,(#72488,#72489,#72490),.UNSPECIFIED.,.F.,.F.)
B_SPLINE_CURVE_WITH_KNOTS((3,3),(0.0217367286900403,0.0948204552983261),
 .UNSPECIFIED.)
CURVE()
GEOMETRIC_REPRESENTATION_ITEM()
RATIONAL_B_SPLINE_CURVE((1.00000243584436,1.000005312848,1.))
REPRESENTATION_ITEM('')
);
#18988=(
BOUNDED_CURVE()
B_SPLINE_CURVE(2,(#72498,#72499,#72500),.UNSPECIFIED.,.F.,.F.)
B_SPLINE_CURVE_WITH_KNOTS((3,3),(0.0217367286900503,0.0948204552983257),
 .UNSPECIFIED.)
CURVE()
GEOMETRIC_REPRESENTATION_ITEM()
RATIONAL_B_SPLINE_CURVE((1.00000243583393,1.00000531282525,1.))
REPRESENTATION_ITEM('')
);
#18989=(
BOUNDED_CURVE()
B_SPLINE_CURVE(2,(#72508,#72509,#72510),.UNSPECIFIED.,.F.,.F.)
B_SPLINE_CURVE_WITH_KNOTS((3,3),(0.0217367286899,0.0948204552983259),
 .UNSPECIFIED.)
CURVE()
GEOMETRIC_REPRESENTATION_ITEM()
RATIONAL_B_SPLINE_CURVE((1.00000243583775,1.00000531283359,1.))
REPRESENTATION_ITEM('')
);
#18990=(
BOUNDED_CURVE()
B_SPLINE_CURVE(2,(#72518,#72519,#72520),.UNSPECIFIED.,.F.,.F.)
B_SPLINE_CURVE_WITH_KNOTS((3,3),(0.0217367286894302,0.0948204552983252),
 .UNSPECIFIED.)
CURVE()
GEOMETRIC_REPRESENTATION_ITEM()
RATIONAL_B_SPLINE_CURVE((1.00000243585063,1.00000531286168,1.))
REPRESENTATION_ITEM('')
);
#18991=(
BOUNDED_CURVE()
B_SPLINE_CURVE(2,(#72528,#72529,#72530),.UNSPECIFIED.,.F.,.F.)
B_SPLINE_CURVE_WITH_KNOTS((3,3),(0.0217367286902311,0.0948204552983257),
 .UNSPECIFIED.)
CURVE()
GEOMETRIC_REPRESENTATION_ITEM()
RATIONAL_B_SPLINE_CURVE((1.00000243584031,1.00000531283916,1.))
REPRESENTATION_ITEM('')
);
#18992=(
BOUNDED_CURVE()
B_SPLINE_CURVE(2,(#72538,#72539,#72540),.UNSPECIFIED.,.F.,.F.)
B_SPLINE_CURVE_WITH_KNOTS((3,3),(0.0217367286900553,0.0948204552983258),
 .UNSPECIFIED.)
CURVE()
GEOMETRIC_REPRESENTATION_ITEM()
RATIONAL_B_SPLINE_CURVE((1.00000243583602,1.00000531282982,1.))
REPRESENTATION_ITEM('')
);
#18993=(
BOUNDED_CURVE()
B_SPLINE_CURVE(2,(#72548,#72549,#72550),.UNSPECIFIED.,.F.,.F.)
B_SPLINE_CURVE_WITH_KNOTS((3,3),(0.0217367286900607,0.0948204552983253),
 .UNSPECIFIED.)
CURVE()
GEOMETRIC_REPRESENTATION_ITEM()
RATIONAL_B_SPLINE_CURVE((1.0000024358435,1.00000531284613,1.))
REPRESENTATION_ITEM('')
);
#18994=(
BOUNDED_CURVE()
B_SPLINE_CURVE(2,(#72558,#72559,#72560),.UNSPECIFIED.,.F.,.F.)
B_SPLINE_CURVE_WITH_KNOTS((3,3),(0.0217367286901279,0.0948204552983257),
 .UNSPECIFIED.)
CURVE()
GEOMETRIC_REPRESENTATION_ITEM()
RATIONAL_B_SPLINE_CURVE((1.00000243583628,1.00000531283037,1.))
REPRESENTATION_ITEM('')
);
#18995=(
BOUNDED_CURVE()
B_SPLINE_CURVE(2,(#72568,#72569,#72570),.UNSPECIFIED.,.F.,.F.)
B_SPLINE_CURVE_WITH_KNOTS((3,3),(0.0217367286900851,0.0948204552983262),
 .UNSPECIFIED.)
CURVE()
GEOMETRIC_REPRESENTATION_ITEM()
RATIONAL_B_SPLINE_CURVE((1.00000243583421,1.00000531282587,1.))
REPRESENTATION_ITEM('')
);
#18996=(
BOUNDED_CURVE()
B_SPLINE_CURVE(2,(#72578,#72579,#72580),.UNSPECIFIED.,.F.,.F.)
B_SPLINE_CURVE_WITH_KNOTS((3,3),(0.0217367286893238,0.0948204552983258),
 .UNSPECIFIED.)
CURVE()
GEOMETRIC_REPRESENTATION_ITEM()
RATIONAL_B_SPLINE_CURVE((1.000002435848,1.00000531285594,1.))
REPRESENTATION_ITEM('')
);
#18997=(
BOUNDED_CURVE()
B_SPLINE_CURVE(2,(#72588,#72589,#72590),.UNSPECIFIED.,.F.,.F.)
B_SPLINE_CURVE_WITH_KNOTS((3,3),(0.0217367286896447,0.0948204552983257),
 .UNSPECIFIED.)
CURVE()
GEOMETRIC_REPRESENTATION_ITEM()
RATIONAL_B_SPLINE_CURVE((1.00000243584317,1.00000531284541,1.))
REPRESENTATION_ITEM('')
);
#18998=(
BOUNDED_CURVE()
B_SPLINE_CURVE(2,(#72598,#72599,#72600),.UNSPECIFIED.,.F.,.F.)
B_SPLINE_CURVE_WITH_KNOTS((3,3),(0.0217367286897485,0.0948204552983259),
 .UNSPECIFIED.)
CURVE()
GEOMETRIC_REPRESENTATION_ITEM()
RATIONAL_B_SPLINE_CURVE((1.0000024358422,1.0000053128433,1.))
REPRESENTATION_ITEM('')
);
#18999=(
BOUNDED_CURVE()
B_SPLINE_CURVE(2,(#72608,#72609,#72610),.UNSPECIFIED.,.F.,.F.)
B_SPLINE_CURVE_WITH_KNOTS((3,3),(0.0217367286893197,0.0948204552983255),
 .UNSPECIFIED.)
CURVE()
GEOMETRIC_REPRESENTATION_ITEM()
RATIONAL_B_SPLINE_CURVE((1.00000243584811,1.00000531285618,1.))
REPRESENTATION_ITEM('')
);
#19000=(
BOUNDED_CURVE()
B_SPLINE_CURVE(2,(#72618,#72619,#72620),.UNSPECIFIED.,.F.,.F.)
B_SPLINE_CURVE_WITH_KNOTS((3,3),(0.0217367286898305,0.0948204552983257),
 .UNSPECIFIED.)
CURVE()
GEOMETRIC_REPRESENTATION_ITEM()
RATIONAL_B_SPLINE_CURVE((1.00000243584037,1.00000531283929,1.))
REPRESENTATION_ITEM('')
);
#19001=(
BOUNDED_CURVE()
B_SPLINE_CURVE(2,(#72628,#72629,#72630),.UNSPECIFIED.,.F.,.F.)
B_SPLINE_CURVE_WITH_KNOTS((3,3),(0.0217367286898262,0.0948204552983256),
 .UNSPECIFIED.)
CURVE()
GEOMETRIC_REPRESENTATION_ITEM()
RATIONAL_B_SPLINE_CURVE((1.00000243583868,1.00000531283562,1.))
REPRESENTATION_ITEM('')
);
#19002=(
BOUNDED_CURVE()
B_SPLINE_CURVE(2,(#72638,#72639,#72640),.UNSPECIFIED.,.F.,.F.)
B_SPLINE_CURVE_WITH_KNOTS((3,3),(0.0217367286902262,0.0948204552983252),
 .UNSPECIFIED.)
CURVE()
GEOMETRIC_REPRESENTATION_ITEM()
RATIONAL_B_SPLINE_CURVE((1.00000243583729,1.00000531283259,1.))
REPRESENTATION_ITEM('')
);
#19003=(
BOUNDED_CURVE()
B_SPLINE_CURVE(2,(#72648,#72649,#72650),.UNSPECIFIED.,.F.,.F.)
B_SPLINE_CURVE_WITH_KNOTS((3,3),(0.0217367286902091,0.0948204552983257),
 .UNSPECIFIED.)
CURVE()
GEOMETRIC_REPRESENTATION_ITEM()
RATIONAL_B_SPLINE_CURVE((1.00000243583305,1.00000531282334,1.))
REPRESENTATION_ITEM('')
);
#19004=(
BOUNDED_CURVE()
B_SPLINE_CURVE(2,(#72658,#72659,#72660),.UNSPECIFIED.,.F.,.F.)
B_SPLINE_CURVE_WITH_KNOTS((3,3),(0.0217367286892795,0.0948204552983256),
 .UNSPECIFIED.)
CURVE()
GEOMETRIC_REPRESENTATION_ITEM()
RATIONAL_B_SPLINE_CURVE((1.00000243584826,1.00000531285652,1.))
REPRESENTATION_ITEM('')
);
#19005=(
BOUNDED_CURVE()
B_SPLINE_CURVE(2,(#72668,#72669,#72670),.UNSPECIFIED.,.F.,.F.)
B_SPLINE_CURVE_WITH_KNOTS((3,3),(0.0217367286900581,0.0948204552983268),
 .UNSPECIFIED.)
CURVE()
GEOMETRIC_REPRESENTATION_ITEM()
RATIONAL_B_SPLINE_CURVE((1.00000243583706,1.00000531283209,1.))
REPRESENTATION_ITEM('')
);
#19006=(
BOUNDED_CURVE()
B_SPLINE_CURVE(2,(#72678,#72679,#72680),.UNSPECIFIED.,.F.,.F.)
B_SPLINE_CURVE_WITH_KNOTS((3,3),(0.0217367286899271,0.0948204552983257),
 .UNSPECIFIED.)
CURVE()
GEOMETRIC_REPRESENTATION_ITEM()
RATIONAL_B_SPLINE_CURVE((1.00000243583793,1.00000531283399,1.))
REPRESENTATION_ITEM('')
);
#19007=(
BOUNDED_CURVE()
B_SPLINE_CURVE(2,(#72688,#72689,#72690),.UNSPECIFIED.,.F.,.F.)
B_SPLINE_CURVE_WITH_KNOTS((3,3),(0.0217367286897488,0.0948204552983259),
 .UNSPECIFIED.)
CURVE()
GEOMETRIC_REPRESENTATION_ITEM()
RATIONAL_B_SPLINE_CURVE((1.0000024358422,1.0000053128433,1.))
REPRESENTATION_ITEM('')
);
#19008=(
BOUNDED_CURVE()
B_SPLINE_CURVE(2,(#72698,#72699,#72700),.UNSPECIFIED.,.F.,.F.)
B_SPLINE_CURVE_WITH_KNOTS((3,3),(0.0217367286894558,0.0948204552983258),
 .UNSPECIFIED.)
CURVE()
GEOMETRIC_REPRESENTATION_ITEM()
RATIONAL_B_SPLINE_CURVE((1.00000243584193,1.00000531284271,1.))
REPRESENTATION_ITEM('')
);
#19009=(
BOUNDED_CURVE()
B_SPLINE_CURVE(2,(#72708,#72709,#72710),.UNSPECIFIED.,.F.,.F.)
B_SPLINE_CURVE_WITH_KNOTS((3,3),(0.0217367286898531,0.0948204552983254),
 .UNSPECIFIED.)
CURVE()
GEOMETRIC_REPRESENTATION_ITEM()
RATIONAL_B_SPLINE_CURVE((1.00000243584379,1.00000531284676,1.))
REPRESENTATION_ITEM('')
);
#19010=(
BOUNDED_CURVE()
B_SPLINE_CURVE(2,(#72718,#72719,#72720),.UNSPECIFIED.,.F.,.F.)
B_SPLINE_CURVE_WITH_KNOTS((3,3),(0.0217367286900914,0.0948204552983258),
 .UNSPECIFIED.)
CURVE()
GEOMETRIC_REPRESENTATION_ITEM()
RATIONAL_B_SPLINE_CURVE((1.00000243582673,1.00000531280955,1.))
REPRESENTATION_ITEM('')
);
#19011=(
BOUNDED_CURVE()
B_SPLINE_CURVE(2,(#72728,#72729,#72730),.UNSPECIFIED.,.F.,.F.)
B_SPLINE_CURVE_WITH_KNOTS((3,3),(0.0217367286896848,0.0948204552983253),
 .UNSPECIFIED.)
CURVE()
GEOMETRIC_REPRESENTATION_ITEM()
RATIONAL_B_SPLINE_CURVE((1.00000243584611,1.00000531285181,1.))
REPRESENTATION_ITEM('')
);
#19012=(
BOUNDED_CURVE()
B_SPLINE_CURVE(2,(#72738,#72739,#72740),.UNSPECIFIED.,.F.,.F.)
B_SPLINE_CURVE_WITH_KNOTS((3,3),(0.0217367286896856,0.0948204552983257),
 .UNSPECIFIED.)
CURVE()
GEOMETRIC_REPRESENTATION_ITEM()
RATIONAL_B_SPLINE_CURVE((1.00000243583825,1.00000531283468,1.))
REPRESENTATION_ITEM('')
);
#19013=(
BOUNDED_CURVE()
B_SPLINE_CURVE(2,(#72748,#72749,#72750),.UNSPECIFIED.,.F.,.F.)
B_SPLINE_CURVE_WITH_KNOTS((3,3),(0.0217367286899301,0.0948204552983263),
 .UNSPECIFIED.)
CURVE()
GEOMETRIC_REPRESENTATION_ITEM()
RATIONAL_B_SPLINE_CURVE((1.00000243583883,1.00000531283595,1.))
REPRESENTATION_ITEM('')
);
#19014=(
BOUNDED_CURVE()
B_SPLINE_CURVE(2,(#72758,#72759,#72760),.UNSPECIFIED.,.F.,.F.)
B_SPLINE_CURVE_WITH_KNOTS((3,3),(0.0217367286899796,0.0948204552983267),
 .UNSPECIFIED.)
CURVE()
GEOMETRIC_REPRESENTATION_ITEM()
RATIONAL_B_SPLINE_CURVE((1.00000243584071,1.00000531284005,1.))
REPRESENTATION_ITEM('')
);
#19015=(
BOUNDED_CURVE()
B_SPLINE_CURVE(2,(#72768,#72769,#72770),.UNSPECIFIED.,.F.,.F.)
B_SPLINE_CURVE_WITH_KNOTS((3,3),(0.0217367286899505,0.0948204552983261),
 .UNSPECIFIED.)
CURVE()
GEOMETRIC_REPRESENTATION_ITEM()
RATIONAL_B_SPLINE_CURVE((1.00000243583762,1.00000531283331,1.))
REPRESENTATION_ITEM('')
);
#19016=(
BOUNDED_CURVE()
B_SPLINE_CURVE(2,(#72778,#72779,#72780),.UNSPECIFIED.,.F.,.F.)
B_SPLINE_CURVE_WITH_KNOTS((3,3),(0.0217367286898014,0.0948204552983259),
 .UNSPECIFIED.)
CURVE()
GEOMETRIC_REPRESENTATION_ITEM()
RATIONAL_B_SPLINE_CURVE((1.00000243585023,1.0000053128608,1.))
REPRESENTATION_ITEM('')
);
#19017=(
BOUNDED_CURVE()
B_SPLINE_CURVE(2,(#72788,#72789,#72790),.UNSPECIFIED.,.F.,.F.)
B_SPLINE_CURVE_WITH_KNOTS((3,3),(0.0217367286893197,0.0948204552983255),
 .UNSPECIFIED.)
CURVE()
GEOMETRIC_REPRESENTATION_ITEM()
RATIONAL_B_SPLINE_CURVE((1.00000243584811,1.00000531285618,1.))
REPRESENTATION_ITEM('')
);
#19018=(
BOUNDED_CURVE()
B_SPLINE_CURVE(2,(#72798,#72799,#72800),.UNSPECIFIED.,.F.,.F.)
B_SPLINE_CURVE_WITH_KNOTS((3,3),(0.0217367286898152,0.0948204552983257),
 .UNSPECIFIED.)
CURVE()
GEOMETRIC_REPRESENTATION_ITEM()
RATIONAL_B_SPLINE_CURVE((1.0000024358428,1.00000531284459,1.))
REPRESENTATION_ITEM('')
);
#19019=(
BOUNDED_CURVE()
B_SPLINE_CURVE(2,(#72808,#72809,#72810),.UNSPECIFIED.,.F.,.F.)
B_SPLINE_CURVE_WITH_KNOTS((3,3),(0.0217367286898778,0.0948204552983258),
 .UNSPECIFIED.)
CURVE()
GEOMETRIC_REPRESENTATION_ITEM()
RATIONAL_B_SPLINE_CURVE((1.000002435835,1.00000531282759,1.))
REPRESENTATION_ITEM('')
);
#19020=(
BOUNDED_CURVE()
B_SPLINE_CURVE(2,(#72818,#72819,#72820),.UNSPECIFIED.,.F.,.F.)
B_SPLINE_CURVE_WITH_KNOTS((3,3),(0.0217367286899082,0.0948204552983253),
 .UNSPECIFIED.)
CURVE()
GEOMETRIC_REPRESENTATION_ITEM()
RATIONAL_B_SPLINE_CURVE((1.00000243584336,1.00000531284581,1.))
REPRESENTATION_ITEM('')
);
#19021=(
BOUNDED_CURVE()
B_SPLINE_CURVE(2,(#72825,#72826,#72827),.UNSPECIFIED.,.F.,.F.)
B_SPLINE_CURVE_WITH_KNOTS((3,3),(0.258079386101496,0.459416258484591),
 .UNSPECIFIED.)
CURVE()
GEOMETRIC_REPRESENTATION_ITEM()
RATIONAL_B_SPLINE_CURVE((1.00161624157847,1.00189253035136,1.00161624157847))
REPRESENTATION_ITEM('')
);
#19022=(
BOUNDED_CURVE()
B_SPLINE_CURVE(2,(#72975,#72976,#72977),.UNSPECIFIED.,.F.,.F.)
B_SPLINE_CURVE_WITH_KNOTS((3,3),(0.258079386101492,0.459416258484576),
 .UNSPECIFIED.)
CURVE()
GEOMETRIC_REPRESENTATION_ITEM()
RATIONAL_B_SPLINE_CURVE((1.00161624157842,1.00189253035131,1.00161624157842))
REPRESENTATION_ITEM('')
);
#19023=(
BOUNDED_CURVE()
B_SPLINE_CURVE(2,(#72981,#72982,#72983),.UNSPECIFIED.,.F.,.F.)
B_SPLINE_CURVE_WITH_KNOTS((3,3),(0.258079386101496,0.459416258484592),
 .UNSPECIFIED.)
CURVE()
GEOMETRIC_REPRESENTATION_ITEM()
RATIONAL_B_SPLINE_CURVE((1.00161624157848,1.00189253035137,1.00161624157848))
REPRESENTATION_ITEM('')
);
#19024=(
BOUNDED_CURVE()
B_SPLINE_CURVE(2,(#72987,#72988,#72989),.UNSPECIFIED.,.F.,.F.)
B_SPLINE_CURVE_WITH_KNOTS((3,3),(0.258079386101498,0.459416258484592),
 .UNSPECIFIED.)
CURVE()
GEOMETRIC_REPRESENTATION_ITEM()
RATIONAL_B_SPLINE_CURVE((1.00161624157846,1.00189253035135,1.00161624157846))
REPRESENTATION_ITEM('')
);
#19025=(
BOUNDED_CURVE()
B_SPLINE_CURVE(2,(#72993,#72994,#72995),.UNSPECIFIED.,.F.,.F.)
B_SPLINE_CURVE_WITH_KNOTS((3,3),(0.258079386101496,0.45941625848459),
 .UNSPECIFIED.)
CURVE()
GEOMETRIC_REPRESENTATION_ITEM()
RATIONAL_B_SPLINE_CURVE((1.00161624157846,1.00189253035135,1.00161624157846))
REPRESENTATION_ITEM('')
);
#19026=(
BOUNDED_CURVE()
B_SPLINE_CURVE(2,(#72999,#73000,#73001),.UNSPECIFIED.,.F.,.F.)
B_SPLINE_CURVE_WITH_KNOTS((3,3),(0.258079386101498,0.45941625848459),
 .UNSPECIFIED.)
CURVE()
GEOMETRIC_REPRESENTATION_ITEM()
RATIONAL_B_SPLINE_CURVE((1.00161624157846,1.00189253035135,1.00161624157846))
REPRESENTATION_ITEM('')
);
#19027=(
BOUNDED_CURVE()
B_SPLINE_CURVE(2,(#73005,#73006,#73007),.UNSPECIFIED.,.F.,.F.)
B_SPLINE_CURVE_WITH_KNOTS((3,3),(0.258079386101502,0.459416258484588),
 .UNSPECIFIED.)
CURVE()
GEOMETRIC_REPRESENTATION_ITEM()
RATIONAL_B_SPLINE_CURVE((1.00161624157843,1.00189253035131,1.00161624157843))
REPRESENTATION_ITEM('')
);
#19028=(
BOUNDED_CURVE()
B_SPLINE_CURVE(2,(#73011,#73012,#73013),.UNSPECIFIED.,.F.,.F.)
B_SPLINE_CURVE_WITH_KNOTS((3,3),(0.258079386101497,0.459416258484587),
 .UNSPECIFIED.)
CURVE()
GEOMETRIC_REPRESENTATION_ITEM()
RATIONAL_B_SPLINE_CURVE((1.00161624157845,1.00189253035134,1.00161624157845))
REPRESENTATION_ITEM('')
);
#19029=(
BOUNDED_CURVE()
B_SPLINE_CURVE(2,(#73017,#73018,#73019),.UNSPECIFIED.,.F.,.F.)
B_SPLINE_CURVE_WITH_KNOTS((3,3),(0.258079386101498,0.459416258484589),
 .UNSPECIFIED.)
CURVE()
GEOMETRIC_REPRESENTATION_ITEM()
RATIONAL_B_SPLINE_CURVE((1.00161624157846,1.00189253035135,1.00161624157846))
REPRESENTATION_ITEM('')
);
#19030=(
BOUNDED_CURVE()
B_SPLINE_CURVE(2,(#73023,#73024,#73025),.UNSPECIFIED.,.F.,.F.)
B_SPLINE_CURVE_WITH_KNOTS((3,3),(0.258079386101496,0.459416258484592),
 .UNSPECIFIED.)
CURVE()
GEOMETRIC_REPRESENTATION_ITEM()
RATIONAL_B_SPLINE_CURVE((1.00161624157848,1.00189253035137,1.00161624157848))
REPRESENTATION_ITEM('')
);
#19031=(
BOUNDED_CURVE()
B_SPLINE_CURVE(2,(#73029,#73030,#73031),.UNSPECIFIED.,.F.,.F.)
B_SPLINE_CURVE_WITH_KNOTS((3,3),(0.258079386101487,0.459416258484582),
 .UNSPECIFIED.)
CURVE()
GEOMETRIC_REPRESENTATION_ITEM()
RATIONAL_B_SPLINE_CURVE((1.00161624157848,1.00189253035137,1.00161624157848))
REPRESENTATION_ITEM('')
);
#19032=(
BOUNDED_CURVE()
B_SPLINE_CURVE(2,(#73035,#73036,#73037),.UNSPECIFIED.,.F.,.F.)
B_SPLINE_CURVE_WITH_KNOTS((3,3),(0.258079386101498,0.459416258484594),
 .UNSPECIFIED.)
CURVE()
GEOMETRIC_REPRESENTATION_ITEM()
RATIONAL_B_SPLINE_CURVE((1.00161624157848,1.00189253035137,1.00161624157848))
REPRESENTATION_ITEM('')
);
#19033=(
BOUNDED_CURVE()
B_SPLINE_CURVE(2,(#73041,#73042,#73043),.UNSPECIFIED.,.F.,.F.)
B_SPLINE_CURVE_WITH_KNOTS((3,3),(0.258079386101494,0.459416258484593),
 .UNSPECIFIED.)
CURVE()
GEOMETRIC_REPRESENTATION_ITEM()
RATIONAL_B_SPLINE_CURVE((1.00161624157849,1.00189253035139,1.00161624157849))
REPRESENTATION_ITEM('')
);
#19034=(
BOUNDED_CURVE()
B_SPLINE_CURVE(2,(#73047,#73048,#73049),.UNSPECIFIED.,.F.,.F.)
B_SPLINE_CURVE_WITH_KNOTS((3,3),(0.258079386101507,0.459416258484601),
 .UNSPECIFIED.)
CURVE()
GEOMETRIC_REPRESENTATION_ITEM()
RATIONAL_B_SPLINE_CURVE((1.00161624157847,1.00189253035136,1.00161624157847))
REPRESENTATION_ITEM('')
);
#19035=(
BOUNDED_CURVE()
B_SPLINE_CURVE(2,(#73053,#73054,#73055),.UNSPECIFIED.,.F.,.F.)
B_SPLINE_CURVE_WITH_KNOTS((3,3),(0.258079386101498,0.459416258484589),
 .UNSPECIFIED.)
CURVE()
GEOMETRIC_REPRESENTATION_ITEM()
RATIONAL_B_SPLINE_CURVE((1.00161624157845,1.00189253035134,1.00161624157845))
REPRESENTATION_ITEM('')
);
#19036=(
BOUNDED_CURVE()
B_SPLINE_CURVE(2,(#73059,#73060,#73061),.UNSPECIFIED.,.F.,.F.)
B_SPLINE_CURVE_WITH_KNOTS((3,3),(0.258079386101491,0.45941625848459),
 .UNSPECIFIED.)
CURVE()
GEOMETRIC_REPRESENTATION_ITEM()
RATIONAL_B_SPLINE_CURVE((1.00161624157849,1.00189253035139,1.00161624157849))
REPRESENTATION_ITEM('')
);
#19037=(
BOUNDED_CURVE()
B_SPLINE_CURVE(2,(#73065,#73066,#73067),.UNSPECIFIED.,.F.,.F.)
B_SPLINE_CURVE_WITH_KNOTS((3,3),(0.258079386101511,0.459416258484598),
 .UNSPECIFIED.)
CURVE()
GEOMETRIC_REPRESENTATION_ITEM()
RATIONAL_B_SPLINE_CURVE((1.00161624157843,1.00189253035132,1.00161624157843))
REPRESENTATION_ITEM('')
);
#19038=(
BOUNDED_CURVE()
B_SPLINE_CURVE(2,(#73071,#73072,#73073),.UNSPECIFIED.,.F.,.F.)
B_SPLINE_CURVE_WITH_KNOTS((3,3),(0.258079386101497,0.459416258484589),
 .UNSPECIFIED.)
CURVE()
GEOMETRIC_REPRESENTATION_ITEM()
RATIONAL_B_SPLINE_CURVE((1.00161624157846,1.00189253035135,1.00161624157846))
REPRESENTATION_ITEM('')
);
#19039=(
BOUNDED_CURVE()
B_SPLINE_CURVE(2,(#73078,#73079,#73080),.UNSPECIFIED.,.F.,.F.)
B_SPLINE_CURVE_WITH_KNOTS((3,3),(0.358747822293045,0.459416258484592),
 .UNSPECIFIED.)
CURVE()
GEOMETRIC_REPRESENTATION_ITEM()
RATIONAL_B_SPLINE_CURVE((1.00175438596492,1.00175438596492,1.00161624157848))
REPRESENTATION_ITEM('')
);
#19040=(
BOUNDED_CURVE()
B_SPLINE_CURVE(2,(#73081,#73082,#73083),.UNSPECIFIED.,.F.,.F.)
B_SPLINE_CURVE_WITH_KNOTS((3,3),(0.258079386101496,0.358747822293045),
 .UNSPECIFIED.)
CURVE()
GEOMETRIC_REPRESENTATION_ITEM()
RATIONAL_B_SPLINE_CURVE((1.00161624157848,1.00175438596492,1.00175438596492))
REPRESENTATION_ITEM('')
);
#19041=(
BOUNDED_CURVE()
B_SPLINE_CURVE(2,(#73087,#73088,#73089),.UNSPECIFIED.,.F.,.F.)
B_SPLINE_CURVE_WITH_KNOTS((3,3),(0.258079386101499,0.459416258484591),
 .UNSPECIFIED.)
CURVE()
GEOMETRIC_REPRESENTATION_ITEM()
RATIONAL_B_SPLINE_CURVE((1.00161624157846,1.00189253035135,1.00161624157846))
REPRESENTATION_ITEM('')
);
#19042=(
BOUNDED_CURVE()
B_SPLINE_CURVE(2,(#73093,#73094,#73095),.UNSPECIFIED.,.F.,.F.)
B_SPLINE_CURVE_WITH_KNOTS((3,3),(0.258079386101487,0.459416258484581),
 .UNSPECIFIED.)
CURVE()
GEOMETRIC_REPRESENTATION_ITEM()
RATIONAL_B_SPLINE_CURVE((1.00161624157848,1.00189253035137,1.00161624157848))
REPRESENTATION_ITEM('')
);
#19043=(
BOUNDED_CURVE()
B_SPLINE_CURVE(2,(#73099,#73100,#73101),.UNSPECIFIED.,.F.,.F.)
B_SPLINE_CURVE_WITH_KNOTS((3,3),(0.258079386101499,0.459416258484585),
 .UNSPECIFIED.)
CURVE()
GEOMETRIC_REPRESENTATION_ITEM()
RATIONAL_B_SPLINE_CURVE((1.00161624157843,1.00189253035131,1.00161624157843))
REPRESENTATION_ITEM('')
);
#19044=(
BOUNDED_CURVE()
B_SPLINE_CURVE(2,(#73105,#73106,#73107),.UNSPECIFIED.,.F.,.F.)
B_SPLINE_CURVE_WITH_KNOTS((3,3),(0.258079386101507,0.459416258484601),
 .UNSPECIFIED.)
CURVE()
GEOMETRIC_REPRESENTATION_ITEM()
RATIONAL_B_SPLINE_CURVE((1.00161624157847,1.00189253035136,1.00161624157847))
REPRESENTATION_ITEM('')
);
#19045=(
BOUNDED_CURVE()
B_SPLINE_CURVE(2,(#73111,#73112,#73113),.UNSPECIFIED.,.F.,.F.)
B_SPLINE_CURVE_WITH_KNOTS((3,3),(0.258079386101492,0.459416258484594),
 .UNSPECIFIED.)
CURVE()
GEOMETRIC_REPRESENTATION_ITEM()
RATIONAL_B_SPLINE_CURVE((1.0016162415785,1.0018925303514,1.0016162415785))
REPRESENTATION_ITEM('')
);
#19046=(
BOUNDED_CURVE()
B_SPLINE_CURVE(2,(#73117,#73118,#73119),.UNSPECIFIED.,.F.,.F.)
B_SPLINE_CURVE_WITH_KNOTS((3,3),(0.258079386101498,0.459416258484587),
 .UNSPECIFIED.)
CURVE()
GEOMETRIC_REPRESENTATION_ITEM()
RATIONAL_B_SPLINE_CURVE((1.00161624157845,1.00189253035133,1.00161624157845))
REPRESENTATION_ITEM('')
);
#19047=(
BOUNDED_CURVE()
B_SPLINE_CURVE(2,(#73123,#73124,#73125),.UNSPECIFIED.,.F.,.F.)
B_SPLINE_CURVE_WITH_KNOTS((3,3),(0.258079386101511,0.459416258484597),
 .UNSPECIFIED.)
CURVE()
GEOMETRIC_REPRESENTATION_ITEM()
RATIONAL_B_SPLINE_CURVE((1.00161624157843,1.00189253035131,1.00161624157843))
REPRESENTATION_ITEM('')
);
#19048=(
BOUNDED_CURVE()
B_SPLINE_CURVE(2,(#73129,#73130,#73131),.UNSPECIFIED.,.F.,.F.)
B_SPLINE_CURVE_WITH_KNOTS((3,3),(0.258079386101486,0.459416258484581),
 .UNSPECIFIED.)
CURVE()
GEOMETRIC_REPRESENTATION_ITEM()
RATIONAL_B_SPLINE_CURVE((1.00161624157848,1.00189253035137,1.00161624157848))
REPRESENTATION_ITEM('')
);
#19049=(
BOUNDED_CURVE()
B_SPLINE_CURVE(2,(#73135,#73136,#73137),.UNSPECIFIED.,.F.,.F.)
B_SPLINE_CURVE_WITH_KNOTS((3,3),(0.258079386101496,0.459416258484591),
 .UNSPECIFIED.)
CURVE()
GEOMETRIC_REPRESENTATION_ITEM()
RATIONAL_B_SPLINE_CURVE((1.00161624157848,1.00189253035137,1.00161624157848))
REPRESENTATION_ITEM('')
);
#19050=(
BOUNDED_CURVE()
B_SPLINE_CURVE(2,(#73141,#73142,#73143),.UNSPECIFIED.,.F.,.F.)
B_SPLINE_CURVE_WITH_KNOTS((3,3),(0.258079386101487,0.459416258484582),
 .UNSPECIFIED.)
CURVE()
GEOMETRIC_REPRESENTATION_ITEM()
RATIONAL_B_SPLINE_CURVE((1.00161624157848,1.00189253035137,1.00161624157848))
REPRESENTATION_ITEM('')
);
#19051=(
BOUNDED_CURVE()
B_SPLINE_CURVE(2,(#73147,#73148,#73149),.UNSPECIFIED.,.F.,.F.)
B_SPLINE_CURVE_WITH_KNOTS((3,3),(0.258079386101486,0.459416258484582),
 .UNSPECIFIED.)
CURVE()
GEOMETRIC_REPRESENTATION_ITEM()
RATIONAL_B_SPLINE_CURVE((1.00161624157848,1.00189253035137,1.00161624157848))
REPRESENTATION_ITEM('')
);
#19052=(
BOUNDED_CURVE()
B_SPLINE_CURVE(2,(#73153,#73154,#73155),.UNSPECIFIED.,.F.,.F.)
B_SPLINE_CURVE_WITH_KNOTS((3,3),(0.258079386101501,0.459416258484586),
 .UNSPECIFIED.)
CURVE()
GEOMETRIC_REPRESENTATION_ITEM()
RATIONAL_B_SPLINE_CURVE((1.00161624157843,1.00189253035131,1.00161624157843))
REPRESENTATION_ITEM('')
);
#19053=(
BOUNDED_CURVE()
B_SPLINE_CURVE(2,(#73159,#73160,#73161),.UNSPECIFIED.,.F.,.F.)
B_SPLINE_CURVE_WITH_KNOTS((3,3),(0.258079386101494,0.459416258484595),
 .UNSPECIFIED.)
CURVE()
GEOMETRIC_REPRESENTATION_ITEM()
RATIONAL_B_SPLINE_CURVE((1.0016162415785,1.0018925303514,1.0016162415785))
REPRESENTATION_ITEM('')
);
#19054=(
BOUNDED_CURVE()
B_SPLINE_CURVE(2,(#73165,#73166,#73167),.UNSPECIFIED.,.F.,.F.)
B_SPLINE_CURVE_WITH_KNOTS((3,3),(0.258079386101498,0.459416258484589),
 .UNSPECIFIED.)
CURVE()
GEOMETRIC_REPRESENTATION_ITEM()
RATIONAL_B_SPLINE_CURVE((1.00161624157845,1.00189253035134,1.00161624157845))
REPRESENTATION_ITEM('')
);
#19055=(
BOUNDED_CURVE()
B_SPLINE_CURVE(2,(#73171,#73172,#73173),.UNSPECIFIED.,.F.,.F.)
B_SPLINE_CURVE_WITH_KNOTS((3,3),(0.258079386101503,0.459416258484589),
 .UNSPECIFIED.)
CURVE()
GEOMETRIC_REPRESENTATION_ITEM()
RATIONAL_B_SPLINE_CURVE((1.00161624157843,1.00189253035131,1.00161624157843))
REPRESENTATION_ITEM('')
);
#19056=(
BOUNDED_CURVE()
B_SPLINE_CURVE(2,(#73177,#73178,#73179),.UNSPECIFIED.,.F.,.F.)
B_SPLINE_CURVE_WITH_KNOTS((3,3),(0.258079386101511,0.459416258484597),
 .UNSPECIFIED.)
CURVE()
GEOMETRIC_REPRESENTATION_ITEM()
RATIONAL_B_SPLINE_CURVE((1.00161624157843,1.00189253035131,1.00161624157843))
REPRESENTATION_ITEM('')
);
#19057=(
BOUNDED_CURVE()
B_SPLINE_CURVE(2,(#73183,#73184,#73185),.UNSPECIFIED.,.F.,.F.)
B_SPLINE_CURVE_WITH_KNOTS((3,3),(0.258079386101485,0.45941625848458),
 .UNSPECIFIED.)
CURVE()
GEOMETRIC_REPRESENTATION_ITEM()
RATIONAL_B_SPLINE_CURVE((1.00161624157848,1.00189253035137,1.00161624157848))
REPRESENTATION_ITEM('')
);
#19058=(
BOUNDED_CURVE()
B_SPLINE_CURVE(2,(#73189,#73190,#73191),.UNSPECIFIED.,.F.,.F.)
B_SPLINE_CURVE_WITH_KNOTS((3,3),(0.258079386101495,0.459416258484592),
 .UNSPECIFIED.)
CURVE()
GEOMETRIC_REPRESENTATION_ITEM()
RATIONAL_B_SPLINE_CURVE((1.00161624157848,1.00189253035137,1.00161624157848))
REPRESENTATION_ITEM('')
);
#19059=(
BOUNDED_CURVE()
B_SPLINE_CURVE(2,(#73247,#73248,#73249),.UNSPECIFIED.,.F.,.F.)
B_SPLINE_CURVE_WITH_KNOTS((3,3),(0.0217367286895466,0.0948204552983258),
 .UNSPECIFIED.)
CURVE()
GEOMETRIC_REPRESENTATION_ITEM()
RATIONAL_B_SPLINE_CURVE((1.0000024358556,1.00000531287251,1.))
REPRESENTATION_ITEM('')
);
#19060=(
BOUNDED_CURVE()
B_SPLINE_CURVE(2,(#73301,#73302,#73303),.UNSPECIFIED.,.F.,.F.)
B_SPLINE_CURVE_WITH_KNOTS((3,3),(0.258079386101485,0.459416258484579),
 .UNSPECIFIED.)
CURVE()
GEOMETRIC_REPRESENTATION_ITEM()
RATIONAL_B_SPLINE_CURVE((1.00161624157847,1.00189253035136,1.00161624157847))
REPRESENTATION_ITEM('')
);
#19061=(
BOUNDED_CURVE()
B_SPLINE_CURVE(2,(#73309,#73310,#73311),.UNSPECIFIED.,.F.,.F.)
B_SPLINE_CURVE_WITH_KNOTS((3,3),(0.358747822293043,0.459416258484592),
 .UNSPECIFIED.)
CURVE()
GEOMETRIC_REPRESENTATION_ITEM()
RATIONAL_B_SPLINE_CURVE((1.00175438596492,1.00175438596492,1.00161624157847))
REPRESENTATION_ITEM('')
);
#19062=(
BOUNDED_CURVE()
B_SPLINE_CURVE(2,(#73313,#73314,#73315),.UNSPECIFIED.,.F.,.F.)
B_SPLINE_CURVE_WITH_KNOTS((3,3),(0.258079386101507,0.459416258484599),
 .UNSPECIFIED.)
CURVE()
GEOMETRIC_REPRESENTATION_ITEM()
RATIONAL_B_SPLINE_CURVE((1.00161624157844,1.00189253035133,1.00161624157844))
REPRESENTATION_ITEM('')
);
#19063=(
BOUNDED_CURVE()
B_SPLINE_CURVE(2,(#73317,#73318,#73319),.UNSPECIFIED.,.F.,.F.)
B_SPLINE_CURVE_WITH_KNOTS((3,3),(0.258079386101484,0.459416258484585),
 .UNSPECIFIED.)
CURVE()
GEOMETRIC_REPRESENTATION_ITEM()
RATIONAL_B_SPLINE_CURVE((1.0016162415785,1.0018925303514,1.0016162415785))
REPRESENTATION_ITEM('')
);
#19064=(
BOUNDED_CURVE()
B_SPLINE_CURVE(2,(#73321,#73322,#73323),.UNSPECIFIED.,.F.,.F.)
B_SPLINE_CURVE_WITH_KNOTS((3,3),(0.258079386101501,0.459416258484591),
 .UNSPECIFIED.)
CURVE()
GEOMETRIC_REPRESENTATION_ITEM()
RATIONAL_B_SPLINE_CURVE((1.00161624157844,1.00189253035133,1.00161624157844))
REPRESENTATION_ITEM('')
);
#19065=(
BOUNDED_CURVE()
B_SPLINE_CURVE(2,(#73325,#73326,#73327),.UNSPECIFIED.,.F.,.F.)
B_SPLINE_CURVE_WITH_KNOTS((3,3),(0.258079386101505,0.459416258484602),
 .UNSPECIFIED.)
CURVE()
GEOMETRIC_REPRESENTATION_ITEM()
RATIONAL_B_SPLINE_CURVE((1.00161624157847,1.00189253035136,1.00161624157847))
REPRESENTATION_ITEM('')
);
#19066=(
BOUNDED_CURVE()
B_SPLINE_CURVE(2,(#73329,#73330,#73331),.UNSPECIFIED.,.F.,.F.)
B_SPLINE_CURVE_WITH_KNOTS((3,3),(0.258079386101503,0.459416258484604),
 .UNSPECIFIED.)
CURVE()
GEOMETRIC_REPRESENTATION_ITEM()
RATIONAL_B_SPLINE_CURVE((1.0016162415785,1.0018925303514,1.0016162415785))
REPRESENTATION_ITEM('')
);
#19067=(
BOUNDED_CURVE()
B_SPLINE_CURVE(2,(#73333,#73334,#73335),.UNSPECIFIED.,.F.,.F.)
B_SPLINE_CURVE_WITH_KNOTS((3,3),(0.258079386101503,0.459416258484592),
 .UNSPECIFIED.)
CURVE()
GEOMETRIC_REPRESENTATION_ITEM()
RATIONAL_B_SPLINE_CURVE((1.00161624157844,1.00189253035133,1.00161624157844))
REPRESENTATION_ITEM('')
);
#19068=(
BOUNDED_CURVE()
B_SPLINE_CURVE(2,(#73337,#73338,#73339),.UNSPECIFIED.,.F.,.F.)
B_SPLINE_CURVE_WITH_KNOTS((3,3),(0.258079386101509,0.459416258484598),
 .UNSPECIFIED.)
CURVE()
GEOMETRIC_REPRESENTATION_ITEM()
RATIONAL_B_SPLINE_CURVE((1.00161624157844,1.00189253035133,1.00161624157844))
REPRESENTATION_ITEM('')
);
#19069=(
BOUNDED_CURVE()
B_SPLINE_CURVE(2,(#73341,#73342,#73343),.UNSPECIFIED.,.F.,.F.)
B_SPLINE_CURVE_WITH_KNOTS((3,3),(0.258079386101488,0.459416258484583),
 .UNSPECIFIED.)
CURVE()
GEOMETRIC_REPRESENTATION_ITEM()
RATIONAL_B_SPLINE_CURVE((1.00161624157847,1.00189253035136,1.00161624157847))
REPRESENTATION_ITEM('')
);
#19070=(
BOUNDED_CURVE()
B_SPLINE_CURVE(2,(#73345,#73346,#73347),.UNSPECIFIED.,.F.,.F.)
B_SPLINE_CURVE_WITH_KNOTS((3,3),(0.258079386101497,0.459416258484591),
 .UNSPECIFIED.)
CURVE()
GEOMETRIC_REPRESENTATION_ITEM()
RATIONAL_B_SPLINE_CURVE((1.00161624157847,1.00189253035136,1.00161624157847))
REPRESENTATION_ITEM('')
);
#19071=(
BOUNDED_CURVE()
B_SPLINE_CURVE(2,(#73349,#73350,#73351),.UNSPECIFIED.,.F.,.F.)
B_SPLINE_CURVE_WITH_KNOTS((3,3),(0.258079386101488,0.459416258484577),
 .UNSPECIFIED.)
CURVE()
GEOMETRIC_REPRESENTATION_ITEM()
RATIONAL_B_SPLINE_CURVE((1.00161624157844,1.00189253035133,1.00161624157844))
REPRESENTATION_ITEM('')
);
#19072=(
BOUNDED_CURVE()
B_SPLINE_CURVE(2,(#73353,#73354,#73355),.UNSPECIFIED.,.F.,.F.)
B_SPLINE_CURVE_WITH_KNOTS((3,3),(0.258079386101483,0.459416258484584),
 .UNSPECIFIED.)
CURVE()
GEOMETRIC_REPRESENTATION_ITEM()
RATIONAL_B_SPLINE_CURVE((1.0016162415785,1.0018925303514,1.0016162415785))
REPRESENTATION_ITEM('')
);
#19073=(
BOUNDED_CURVE()
B_SPLINE_CURVE(2,(#73357,#73358,#73359),.UNSPECIFIED.,.F.,.F.)
B_SPLINE_CURVE_WITH_KNOTS((3,3),(0.258079386101508,0.459416258484598),
 .UNSPECIFIED.)
CURVE()
GEOMETRIC_REPRESENTATION_ITEM()
RATIONAL_B_SPLINE_CURVE((1.00161624157844,1.00189253035133,1.00161624157844))
REPRESENTATION_ITEM('')
);
#19074=(
BOUNDED_CURVE()
B_SPLINE_CURVE(2,(#73361,#73362,#73363),.UNSPECIFIED.,.F.,.F.)
B_SPLINE_CURVE_WITH_KNOTS((3,3),(0.258079386101503,0.459416258484604),
 .UNSPECIFIED.)
CURVE()
GEOMETRIC_REPRESENTATION_ITEM()
RATIONAL_B_SPLINE_CURVE((1.0016162415785,1.0018925303514,1.0016162415785))
REPRESENTATION_ITEM('')
);
#19075=(
BOUNDED_CURVE()
B_SPLINE_CURVE(2,(#73365,#73366,#73367),.UNSPECIFIED.,.F.,.F.)
B_SPLINE_CURVE_WITH_KNOTS((3,3),(0.258079386101498,0.459416258484587),
 .UNSPECIFIED.)
CURVE()
GEOMETRIC_REPRESENTATION_ITEM()
RATIONAL_B_SPLINE_CURVE((1.00161624157844,1.00189253035133,1.00161624157844))
REPRESENTATION_ITEM('')
);
#19076=(
BOUNDED_CURVE()
B_SPLINE_CURVE(2,(#73369,#73370,#73371),.UNSPECIFIED.,.F.,.F.)
B_SPLINE_CURVE_WITH_KNOTS((3,3),(0.258079386101498,0.459416258484587),
 .UNSPECIFIED.)
CURVE()
GEOMETRIC_REPRESENTATION_ITEM()
RATIONAL_B_SPLINE_CURVE((1.00161624157844,1.00189253035133,1.00161624157844))
REPRESENTATION_ITEM('')
);
#19077=(
BOUNDED_CURVE()
B_SPLINE_CURVE(2,(#73373,#73374,#73375),.UNSPECIFIED.,.F.,.F.)
B_SPLINE_CURVE_WITH_KNOTS((3,3),(0.258079386101507,0.459416258484602),
 .UNSPECIFIED.)
CURVE()
GEOMETRIC_REPRESENTATION_ITEM()
RATIONAL_B_SPLINE_CURVE((1.00161624157847,1.00189253035136,1.00161624157847))
REPRESENTATION_ITEM('')
);
#19078=(
BOUNDED_CURVE()
B_SPLINE_CURVE(2,(#73377,#73378,#73379),.UNSPECIFIED.,.F.,.F.)
B_SPLINE_CURVE_WITH_KNOTS((3,3),(0.258079386101488,0.459416258484583),
 .UNSPECIFIED.)
CURVE()
GEOMETRIC_REPRESENTATION_ITEM()
RATIONAL_B_SPLINE_CURVE((1.00161624157847,1.00189253035136,1.00161624157847))
REPRESENTATION_ITEM('')
);
#19079=(
BOUNDED_CURVE()
B_SPLINE_CURVE(2,(#73382,#73383,#73384),.UNSPECIFIED.,.F.,.F.)
B_SPLINE_CURVE_WITH_KNOTS((3,3),(0.0217367286897871,0.0948204552983253),
 .UNSPECIFIED.)
CURVE()
GEOMETRIC_REPRESENTATION_ITEM()
RATIONAL_B_SPLINE_CURVE((1.00000243583551,1.00000531282869,1.))
REPRESENTATION_ITEM('')
);
#19080=(
BOUNDED_CURVE()
B_SPLINE_CURVE(2,(#73387,#73388,#73389),.UNSPECIFIED.,.F.,.F.)
B_SPLINE_CURVE_WITH_KNOTS((3,3),(0.258079386101499,0.459416258484588),
 .UNSPECIFIED.)
CURVE()
GEOMETRIC_REPRESENTATION_ITEM()
RATIONAL_B_SPLINE_CURVE((1.00161624157844,1.00189253035133,1.00161624157844))
REPRESENTATION_ITEM('')
);
#19081=(
BOUNDED_CURVE()
B_SPLINE_CURVE(2,(#73391,#73392,#73393),.UNSPECIFIED.,.F.,.F.)
B_SPLINE_CURVE_WITH_KNOTS((3,3),(0.258079386101495,0.459416258484591),
 .UNSPECIFIED.)
CURVE()
GEOMETRIC_REPRESENTATION_ITEM()
RATIONAL_B_SPLINE_CURVE((1.00161624157847,1.00189253035136,1.00161624157847))
REPRESENTATION_ITEM('')
);
#19082=(
BOUNDED_CURVE()
B_SPLINE_CURVE(2,(#73395,#73396,#73397),.UNSPECIFIED.,.F.,.F.)
B_SPLINE_CURVE_WITH_KNOTS((3,3),(0.258079386101508,0.459416258484599),
 .UNSPECIFIED.)
CURVE()
GEOMETRIC_REPRESENTATION_ITEM()
RATIONAL_B_SPLINE_CURVE((1.00161624157844,1.00189253035133,1.00161624157844))
REPRESENTATION_ITEM('')
);
#19083=(
BOUNDED_CURVE()
B_SPLINE_CURVE(2,(#73399,#73400,#73401),.UNSPECIFIED.,.F.,.F.)
B_SPLINE_CURVE_WITH_KNOTS((3,3),(0.258079386101511,0.459416258484596),
 .UNSPECIFIED.)
CURVE()
GEOMETRIC_REPRESENTATION_ITEM()
RATIONAL_B_SPLINE_CURVE((1.00161624157842,1.0018925303513,1.00161624157842))
REPRESENTATION_ITEM('')
);
#19084=(
BOUNDED_CURVE()
B_SPLINE_CURVE(2,(#73403,#73404,#73405),.UNSPECIFIED.,.F.,.F.)
B_SPLINE_CURVE_WITH_KNOTS((3,3),(0.25807938610151,0.459416258484599),
 .UNSPECIFIED.)
CURVE()
GEOMETRIC_REPRESENTATION_ITEM()
RATIONAL_B_SPLINE_CURVE((1.00161624157844,1.00189253035133,1.00161624157844))
REPRESENTATION_ITEM('')
);
#19085=(
BOUNDED_CURVE()
B_SPLINE_CURVE(2,(#73407,#73408,#73409),.UNSPECIFIED.,.F.,.F.)
B_SPLINE_CURVE_WITH_KNOTS((3,3),(0.258079386101508,0.459416258484599),
 .UNSPECIFIED.)
CURVE()
GEOMETRIC_REPRESENTATION_ITEM()
RATIONAL_B_SPLINE_CURVE((1.00161624157844,1.00189253035133,1.00161624157844))
REPRESENTATION_ITEM('')
);
#19086=(
BOUNDED_CURVE()
B_SPLINE_CURVE(2,(#73411,#73412,#73413),.UNSPECIFIED.,.F.,.F.)
B_SPLINE_CURVE_WITH_KNOTS((3,3),(0.258079386101509,0.459416258484598),
 .UNSPECIFIED.)
CURVE()
GEOMETRIC_REPRESENTATION_ITEM()
RATIONAL_B_SPLINE_CURVE((1.00161624157844,1.00189253035133,1.00161624157844))
REPRESENTATION_ITEM('')
);
#19087=(
BOUNDED_CURVE()
B_SPLINE_CURVE(2,(#73415,#73416,#73417),.UNSPECIFIED.,.F.,.F.)
B_SPLINE_CURVE_WITH_KNOTS((3,3),(0.258079386101496,0.459416258484592),
 .UNSPECIFIED.)
CURVE()
GEOMETRIC_REPRESENTATION_ITEM()
RATIONAL_B_SPLINE_CURVE((1.00161624157847,1.00189253035136,1.00161624157847))
REPRESENTATION_ITEM('')
);
#19088=(
BOUNDED_CURVE()
B_SPLINE_CURVE(2,(#73419,#73420,#73421),.UNSPECIFIED.,.F.,.F.)
B_SPLINE_CURVE_WITH_KNOTS((3,3),(0.258079386101486,0.45941625848458),
 .UNSPECIFIED.)
CURVE()
GEOMETRIC_REPRESENTATION_ITEM()
RATIONAL_B_SPLINE_CURVE((1.00161624157847,1.00189253035136,1.00161624157847))
REPRESENTATION_ITEM('')
);
#19089=(
BOUNDED_CURVE()
B_SPLINE_CURVE(2,(#73423,#73424,#73425),.UNSPECIFIED.,.F.,.F.)
B_SPLINE_CURVE_WITH_KNOTS((3,3),(0.258079386101509,0.459416258484599),
 .UNSPECIFIED.)
CURVE()
GEOMETRIC_REPRESENTATION_ITEM()
RATIONAL_B_SPLINE_CURVE((1.00161624157844,1.00189253035133,1.00161624157844))
REPRESENTATION_ITEM('')
);
#19090=(
BOUNDED_CURVE()
B_SPLINE_CURVE(2,(#73427,#73428,#73429),.UNSPECIFIED.,.F.,.F.)
B_SPLINE_CURVE_WITH_KNOTS((3,3),(0.258079386101495,0.45941625848459),
 .UNSPECIFIED.)
CURVE()
GEOMETRIC_REPRESENTATION_ITEM()
RATIONAL_B_SPLINE_CURVE((1.00161624157847,1.00189253035136,1.00161624157847))
REPRESENTATION_ITEM('')
);
#19091=(
BOUNDED_CURVE()
B_SPLINE_CURVE(2,(#73431,#73432,#73433),.UNSPECIFIED.,.F.,.F.)
B_SPLINE_CURVE_WITH_KNOTS((3,3),(0.258079386101507,0.459416258484603),
 .UNSPECIFIED.)
CURVE()
GEOMETRIC_REPRESENTATION_ITEM()
RATIONAL_B_SPLINE_CURVE((1.00161624157847,1.00189253035136,1.00161624157847))
REPRESENTATION_ITEM('')
);
#19092=(
BOUNDED_CURVE()
B_SPLINE_CURVE(2,(#73435,#73436,#73437),.UNSPECIFIED.,.F.,.F.)
B_SPLINE_CURVE_WITH_KNOTS((3,3),(0.258079386101498,0.459416258484587),
 .UNSPECIFIED.)
CURVE()
GEOMETRIC_REPRESENTATION_ITEM()
RATIONAL_B_SPLINE_CURVE((1.00161624157844,1.00189253035133,1.00161624157844))
REPRESENTATION_ITEM('')
);
#19093=(
BOUNDED_CURVE()
B_SPLINE_CURVE(2,(#73439,#73440,#73441),.UNSPECIFIED.,.F.,.F.)
B_SPLINE_CURVE_WITH_KNOTS((3,3),(0.258079386101511,0.4594162584846),
 .UNSPECIFIED.)
CURVE()
GEOMETRIC_REPRESENTATION_ITEM()
RATIONAL_B_SPLINE_CURVE((1.00161624157844,1.00189253035133,1.00161624157844))
REPRESENTATION_ITEM('')
);
#19094=(
BOUNDED_CURVE()
B_SPLINE_CURVE(2,(#73443,#73444,#73445),.UNSPECIFIED.,.F.,.F.)
B_SPLINE_CURVE_WITH_KNOTS((3,3),(0.258079386101507,0.459416258484602),
 .UNSPECIFIED.)
CURVE()
GEOMETRIC_REPRESENTATION_ITEM()
RATIONAL_B_SPLINE_CURVE((1.00161624157847,1.00189253035136,1.00161624157847))
REPRESENTATION_ITEM('')
);
#19095=(
BOUNDED_CURVE()
B_SPLINE_CURVE(2,(#73447,#73448,#73449),.UNSPECIFIED.,.F.,.F.)
B_SPLINE_CURVE_WITH_KNOTS((3,3),(0.258079386101496,0.459416258484591),
 .UNSPECIFIED.)
CURVE()
GEOMETRIC_REPRESENTATION_ITEM()
RATIONAL_B_SPLINE_CURVE((1.00161624157847,1.00189253035136,1.00161624157847))
REPRESENTATION_ITEM('')
);
#19096=(
BOUNDED_CURVE()
B_SPLINE_CURVE(2,(#73451,#73452,#73453),.UNSPECIFIED.,.F.,.F.)
B_SPLINE_CURVE_WITH_KNOTS((3,3),(0.258079386101497,0.358747822293043),
 .UNSPECIFIED.)
CURVE()
GEOMETRIC_REPRESENTATION_ITEM()
RATIONAL_B_SPLINE_CURVE((1.00161624157847,1.00175438596492,1.00175438596492))
REPRESENTATION_ITEM('')
);
#19097=(
BOUNDED_CURVE()
B_SPLINE_CURVE(2,(#73511,#73512,#73513),.UNSPECIFIED.,.F.,.F.)
B_SPLINE_CURVE_WITH_KNOTS((3,3),(0.0217367286898259,0.0948204552983258),
 .UNSPECIFIED.)
CURVE()
GEOMETRIC_REPRESENTATION_ITEM()
RATIONAL_B_SPLINE_CURVE((1.00000243584041,1.00000531283939,1.))
REPRESENTATION_ITEM('')
);
#19098=(
BOUNDED_CURVE()
B_SPLINE_CURVE(2,(#73622,#73623,#73624),.UNSPECIFIED.,.F.,.F.)
B_SPLINE_CURVE_WITH_KNOTS((3,3),(0.0217367286902918,0.0948204552983266),
 .UNSPECIFIED.)
CURVE()
GEOMETRIC_REPRESENTATION_ITEM()
RATIONAL_B_SPLINE_CURVE((1.00000243583421,1.00000531282586,1.))
REPRESENTATION_ITEM('')
);
#19099=(
BOUNDED_CURVE()
B_SPLINE_CURVE(2,(#73733,#73734,#73735),.UNSPECIFIED.,.F.,.F.)
B_SPLINE_CURVE_WITH_KNOTS((3,3),(0.0217367286900204,0.0948204552983262),
 .UNSPECIFIED.)
CURVE()
GEOMETRIC_REPRESENTATION_ITEM()
RATIONAL_B_SPLINE_CURVE((1.0000024358438,1.00000531284678,1.))
REPRESENTATION_ITEM('')
);
#19100=(
BOUNDED_CURVE()
B_SPLINE_CURVE(2,(#73844,#73845,#73846),.UNSPECIFIED.,.F.,.F.)
B_SPLINE_CURVE_WITH_KNOTS((3,3),(0.021736728689681,0.0948204552983264),
 .UNSPECIFIED.)
CURVE()
GEOMETRIC_REPRESENTATION_ITEM()
RATIONAL_B_SPLINE_CURVE((1.0000024358479,1.00000531285573,1.))
REPRESENTATION_ITEM('')
);
#19101=(
BOUNDED_CURVE()
B_SPLINE_CURVE(2,(#73955,#73956,#73957),.UNSPECIFIED.,.F.,.F.)
B_SPLINE_CURVE_WITH_KNOTS((3,3),(0.0217367286903269,0.0948204552983259),
 .UNSPECIFIED.)
CURVE()
GEOMETRIC_REPRESENTATION_ITEM()
RATIONAL_B_SPLINE_CURVE((1.00000243583057,1.00000531281792,1.))
REPRESENTATION_ITEM('')
);
#19102=(
BOUNDED_CURVE()
B_SPLINE_CURVE(2,(#74066,#74067,#74068),.UNSPECIFIED.,.F.,.F.)
B_SPLINE_CURVE_WITH_KNOTS((3,3),(0.0217367286899795,0.0948204552983258),
 .UNSPECIFIED.)
CURVE()
GEOMETRIC_REPRESENTATION_ITEM()
RATIONAL_B_SPLINE_CURVE((1.0000024358404,1.00000531283936,1.))
REPRESENTATION_ITEM('')
);
#19103=(
BOUNDED_CURVE()
B_SPLINE_CURVE(2,(#74177,#74178,#74179),.UNSPECIFIED.,.F.,.F.)
B_SPLINE_CURVE_WITH_KNOTS((3,3),(0.021736728689809,0.0948204552983252),
 .UNSPECIFIED.)
CURVE()
GEOMETRIC_REPRESENTATION_ITEM()
RATIONAL_B_SPLINE_CURVE((1.00000243583744,1.00000531283292,1.))
REPRESENTATION_ITEM('')
);
#19104=(
BOUNDED_CURVE()
B_SPLINE_CURVE(2,(#74288,#74289,#74290),.UNSPECIFIED.,.F.,.F.)
B_SPLINE_CURVE_WITH_KNOTS((3,3),(0.0217367286899008,0.0948204552983264),
 .UNSPECIFIED.)
CURVE()
GEOMETRIC_REPRESENTATION_ITEM()
RATIONAL_B_SPLINE_CURVE((1.00000243583837,1.00000531283495,1.))
REPRESENTATION_ITEM('')
);
#19105=(
BOUNDED_CURVE()
B_SPLINE_CURVE(2,(#74399,#74400,#74401),.UNSPECIFIED.,.F.,.F.)
B_SPLINE_CURVE_WITH_KNOTS((3,3),(0.0217367286899683,0.0948204552983256),
 .UNSPECIFIED.)
CURVE()
GEOMETRIC_REPRESENTATION_ITEM()
RATIONAL_B_SPLINE_CURVE((1.00000243584639,1.00000531285242,1.))
REPRESENTATION_ITEM('')
);
#19106=(
BOUNDED_CURVE()
B_SPLINE_CURVE(2,(#74510,#74511,#74512),.UNSPECIFIED.,.F.,.F.)
B_SPLINE_CURVE_WITH_KNOTS((3,3),(0.0217367286898393,0.0948204552983254),
 .UNSPECIFIED.)
CURVE()
GEOMETRIC_REPRESENTATION_ITEM()
RATIONAL_B_SPLINE_CURVE((1.00000243584073,1.00000531284008,1.))
REPRESENTATION_ITEM('')
);
#19107=(
BOUNDED_CURVE()
B_SPLINE_CURVE(2,(#74621,#74622,#74623),.UNSPECIFIED.,.F.,.F.)
B_SPLINE_CURVE_WITH_KNOTS((3,3),(0.0217367286899436,0.0948204552983261),
 .UNSPECIFIED.)
CURVE()
GEOMETRIC_REPRESENTATION_ITEM()
RATIONAL_B_SPLINE_CURVE((1.0000024358327,1.00000531282257,1.))
REPRESENTATION_ITEM('')
);
#19108=(
BOUNDED_CURVE()
B_SPLINE_CURVE(2,(#74732,#74733,#74734),.UNSPECIFIED.,.F.,.F.)
B_SPLINE_CURVE_WITH_KNOTS((3,3),(0.0217367286899227,0.094820455298326),
 .UNSPECIFIED.)
CURVE()
GEOMETRIC_REPRESENTATION_ITEM()
RATIONAL_B_SPLINE_CURVE((1.00000243583775,1.00000531283358,1.))
REPRESENTATION_ITEM('')
);
#19109=(
BOUNDED_CURVE()
B_SPLINE_CURVE(2,(#74843,#74844,#74845),.UNSPECIFIED.,.F.,.F.)
B_SPLINE_CURVE_WITH_KNOTS((3,3),(0.0217367286898759,0.0948204552983263),
 .UNSPECIFIED.)
CURVE()
GEOMETRIC_REPRESENTATION_ITEM()
RATIONAL_B_SPLINE_CURVE((1.00000243584141,1.00000531284156,1.))
REPRESENTATION_ITEM('')
);
#19110=(
BOUNDED_CURVE()
B_SPLINE_CURVE(2,(#74954,#74955,#74956),.UNSPECIFIED.,.F.,.F.)
B_SPLINE_CURVE_WITH_KNOTS((3,3),(0.0217367286898064,0.0948204552983261),
 .UNSPECIFIED.)
CURVE()
GEOMETRIC_REPRESENTATION_ITEM()
RATIONAL_B_SPLINE_CURVE((1.00000243584332,1.00000531284573,1.))
REPRESENTATION_ITEM('')
);
#19111=(
BOUNDED_CURVE()
B_SPLINE_CURVE(2,(#75065,#75066,#75067),.UNSPECIFIED.,.F.,.F.)
B_SPLINE_CURVE_WITH_KNOTS((3,3),(0.0217367286899321,0.0948204552983259),
 .UNSPECIFIED.)
CURVE()
GEOMETRIC_REPRESENTATION_ITEM()
RATIONAL_B_SPLINE_CURVE((1.00000243584617,1.00000531285196,1.))
REPRESENTATION_ITEM('')
);
#19112=(
BOUNDED_CURVE()
B_SPLINE_CURVE(2,(#75176,#75177,#75178),.UNSPECIFIED.,.F.,.F.)
B_SPLINE_CURVE_WITH_KNOTS((3,3),(0.0217367286900994,0.094820455298325),
 .UNSPECIFIED.)
CURVE()
GEOMETRIC_REPRESENTATION_ITEM()
RATIONAL_B_SPLINE_CURVE((1.0000024358338,1.00000531282496,1.))
REPRESENTATION_ITEM('')
);
#19113=(
BOUNDED_CURVE()
B_SPLINE_CURVE(2,(#75287,#75288,#75289),.UNSPECIFIED.,.F.,.F.)
B_SPLINE_CURVE_WITH_KNOTS((3,3),(0.0217367286897137,0.0948204552983262),
 .UNSPECIFIED.)
CURVE()
GEOMETRIC_REPRESENTATION_ITEM()
RATIONAL_B_SPLINE_CURVE((1.00000243584632,1.00000531285229,1.))
REPRESENTATION_ITEM('')
);
#19114=(
BOUNDED_CURVE()
B_SPLINE_CURVE(2,(#75398,#75399,#75400),.UNSPECIFIED.,.F.,.F.)
B_SPLINE_CURVE_WITH_KNOTS((3,3),(0.0217367286899984,0.0948204552983254),
 .UNSPECIFIED.)
CURVE()
GEOMETRIC_REPRESENTATION_ITEM()
RATIONAL_B_SPLINE_CURVE((1.00000243584651,1.0000053128527,1.))
REPRESENTATION_ITEM('')
);
#19115=(
BOUNDED_CURVE()
B_SPLINE_CURVE(2,(#75509,#75510,#75511),.UNSPECIFIED.,.F.,.F.)
B_SPLINE_CURVE_WITH_KNOTS((3,3),(0.0217367286897552,0.0948204552983258),
 .UNSPECIFIED.)
CURVE()
GEOMETRIC_REPRESENTATION_ITEM()
RATIONAL_B_SPLINE_CURVE((1.00000243584045,1.00000531283947,1.))
REPRESENTATION_ITEM('')
);
#19116=(
BOUNDED_CURVE()
B_SPLINE_CURVE(2,(#75620,#75621,#75622),.UNSPECIFIED.,.F.,.F.)
B_SPLINE_CURVE_WITH_KNOTS((3,3),(0.021736728689794,0.0948204552983258),
 .UNSPECIFIED.)
CURVE()
GEOMETRIC_REPRESENTATION_ITEM()
RATIONAL_B_SPLINE_CURVE((1.00000243584253,1.00000531284402,1.))
REPRESENTATION_ITEM('')
);
#19117=(
BOUNDED_CURVE()
B_SPLINE_CURVE(2,(#75731,#75732,#75733),.UNSPECIFIED.,.F.,.F.)
B_SPLINE_CURVE_WITH_KNOTS((3,3),(0.0217367286900131,0.0948204552983256),
 .UNSPECIFIED.)
CURVE()
GEOMETRIC_REPRESENTATION_ITEM()
RATIONAL_B_SPLINE_CURVE((1.00000243583569,1.00000531282909,1.))
REPRESENTATION_ITEM('')
);
#19118=(
BOUNDED_CURVE()
B_SPLINE_CURVE(2,(#75842,#75843,#75844),.UNSPECIFIED.,.F.,.F.)
B_SPLINE_CURVE_WITH_KNOTS((3,3),(0.0217367286898347,0.0948204552983258),
 .UNSPECIFIED.)
CURVE()
GEOMETRIC_REPRESENTATION_ITEM()
RATIONAL_B_SPLINE_CURVE((1.00000243583206,1.00000531282119,1.))
REPRESENTATION_ITEM('')
);
#19119=(
BOUNDED_CURVE()
B_SPLINE_CURVE(2,(#75953,#75954,#75955),.UNSPECIFIED.,.F.,.F.)
B_SPLINE_CURVE_WITH_KNOTS((3,3),(0.021736728689975,0.0948204552983256),
 .UNSPECIFIED.)
CURVE()
GEOMETRIC_REPRESENTATION_ITEM()
RATIONAL_B_SPLINE_CURVE((1.00000243583644,1.00000531283073,1.))
REPRESENTATION_ITEM('')
);
#19120=(
BOUNDED_CURVE()
B_SPLINE_CURVE(2,(#76064,#76065,#76066),.UNSPECIFIED.,.F.,.F.)
B_SPLINE_CURVE_WITH_KNOTS((3,3),(0.0217367286899247,0.0948204552983257),
 .UNSPECIFIED.)
CURVE()
GEOMETRIC_REPRESENTATION_ITEM()
RATIONAL_B_SPLINE_CURVE((1.00000243584565,1.00000531285082,1.))
REPRESENTATION_ITEM('')
);
#19121=(
BOUNDED_CURVE()
B_SPLINE_CURVE(2,(#76175,#76176,#76177),.UNSPECIFIED.,.F.,.F.)
B_SPLINE_CURVE_WITH_KNOTS((3,3),(0.0217367286899464,0.0948204552983249),
 .UNSPECIFIED.)
CURVE()
GEOMETRIC_REPRESENTATION_ITEM()
RATIONAL_B_SPLINE_CURVE((1.0000024358387,1.00000531283565,1.))
REPRESENTATION_ITEM('')
);
#19122=(
BOUNDED_CURVE()
B_SPLINE_CURVE(2,(#76286,#76287,#76288),.UNSPECIFIED.,.F.,.F.)
B_SPLINE_CURVE_WITH_KNOTS((3,3),(0.0217367286898777,0.0948204552983262),
 .UNSPECIFIED.)
CURVE()
GEOMETRIC_REPRESENTATION_ITEM()
RATIONAL_B_SPLINE_CURVE((1.00000243584005,1.00000531283861,1.))
REPRESENTATION_ITEM('')
);
#19123=(
BOUNDED_CURVE()
B_SPLINE_CURVE(2,(#76397,#76398,#76399),.UNSPECIFIED.,.F.,.F.)
B_SPLINE_CURVE_WITH_KNOTS((3,3),(0.0217367286897134,0.0948204552983253),
 .UNSPECIFIED.)
CURVE()
GEOMETRIC_REPRESENTATION_ITEM()
RATIONAL_B_SPLINE_CURVE((1.00000243584478,1.00000531284892,1.))
REPRESENTATION_ITEM('')
);
#19124=(
BOUNDED_CURVE()
B_SPLINE_CURVE(2,(#76508,#76509,#76510),.UNSPECIFIED.,.F.,.F.)
B_SPLINE_CURVE_WITH_KNOTS((3,3),(0.0217367286895846,0.0948204552983254),
 .UNSPECIFIED.)
CURVE()
GEOMETRIC_REPRESENTATION_ITEM()
RATIONAL_B_SPLINE_CURVE((1.0000024358477,1.00000531285529,1.))
REPRESENTATION_ITEM('')
);
#19125=(
BOUNDED_CURVE()
B_SPLINE_CURVE(2,(#76619,#76620,#76621),.UNSPECIFIED.,.F.,.F.)
B_SPLINE_CURVE_WITH_KNOTS((3,3),(0.0217367286901915,0.0948204552983254),
 .UNSPECIFIED.)
CURVE()
GEOMETRIC_REPRESENTATION_ITEM()
RATIONAL_B_SPLINE_CURVE((1.00000243582364,1.00000531280281,1.))
REPRESENTATION_ITEM('')
);
#19126=(
BOUNDED_CURVE()
B_SPLINE_CURVE(2,(#76730,#76731,#76732),.UNSPECIFIED.,.F.,.F.)
B_SPLINE_CURVE_WITH_KNOTS((3,3),(0.0217367286904276,0.0948204552983253),
 .UNSPECIFIED.)
CURVE()
GEOMETRIC_REPRESENTATION_ITEM()
RATIONAL_B_SPLINE_CURVE((1.00000243583521,1.00000531282805,1.))
REPRESENTATION_ITEM('')
);
#19127=(
BOUNDED_CURVE()
B_SPLINE_CURVE(2,(#76841,#76842,#76843),.UNSPECIFIED.,.F.,.F.)
B_SPLINE_CURVE_WITH_KNOTS((3,3),(0.0217367286899727,0.0948204552983254),
 .UNSPECIFIED.)
CURVE()
GEOMETRIC_REPRESENTATION_ITEM()
RATIONAL_B_SPLINE_CURVE((1.00000243583722,1.00000531283242,1.))
REPRESENTATION_ITEM('')
);
#19128=(
BOUNDED_CURVE()
B_SPLINE_CURVE(2,(#76952,#76953,#76954),.UNSPECIFIED.,.F.,.F.)
B_SPLINE_CURVE_WITH_KNOTS((3,3),(0.0217367286895435,0.0948204552983251),
 .UNSPECIFIED.)
CURVE()
GEOMETRIC_REPRESENTATION_ITEM()
RATIONAL_B_SPLINE_CURVE((1.00000243584605,1.0000053128517,1.))
REPRESENTATION_ITEM('')
);
#19129=(
BOUNDED_CURVE()
B_SPLINE_CURVE(2,(#77063,#77064,#77065),.UNSPECIFIED.,.F.,.F.)
B_SPLINE_CURVE_WITH_KNOTS((3,3),(0.021736728689847,0.0948204552983251),
 .UNSPECIFIED.)
CURVE()
GEOMETRIC_REPRESENTATION_ITEM()
RATIONAL_B_SPLINE_CURVE((1.00000243585107,1.00000531286265,1.))
REPRESENTATION_ITEM('')
);
#19130=(
BOUNDED_CURVE()
B_SPLINE_CURVE(2,(#77174,#77175,#77176),.UNSPECIFIED.,.F.,.F.)
B_SPLINE_CURVE_WITH_KNOTS((3,3),(0.0217367286902175,0.0948204552983246),
 .UNSPECIFIED.)
CURVE()
GEOMETRIC_REPRESENTATION_ITEM()
RATIONAL_B_SPLINE_CURVE((1.00000243582944,1.00000531281547,1.))
REPRESENTATION_ITEM('')
);
#19131=(
BOUNDED_CURVE()
B_SPLINE_CURVE(2,(#77339,#77340,#77341),.UNSPECIFIED.,.F.,.F.)
B_SPLINE_CURVE_WITH_KNOTS((3,3),(0.0217367286901568,0.0948204552983253),
 .UNSPECIFIED.)
CURVE()
GEOMETRIC_REPRESENTATION_ITEM()
RATIONAL_B_SPLINE_CURVE((1.00000243582781,1.00000531281191,1.))
REPRESENTATION_ITEM('')
);
#19132=(
BOUNDED_CURVE()
B_SPLINE_CURVE(2,(#77420,#77421,#77422),.UNSPECIFIED.,.F.,.F.)
B_SPLINE_CURVE_WITH_KNOTS((3,3),(0.,0.0709397118056797),.UNSPECIFIED.)
CURVE()
GEOMETRIC_REPRESENTATION_ITEM()
RATIONAL_B_SPLINE_CURVE((1.,1.00002244954425,1.))
REPRESENTATION_ITEM('')
);
#19133=(
BOUNDED_CURVE()
B_SPLINE_CURVE(2,(#77430,#77431,#77432),.UNSPECIFIED.,.F.,.F.)
B_SPLINE_CURVE_WITH_KNOTS((3,3),(0.,0.0709397118056795),.UNSPECIFIED.)
CURVE()
GEOMETRIC_REPRESENTATION_ITEM()
RATIONAL_B_SPLINE_CURVE((1.,1.00002245192274,1.))
REPRESENTATION_ITEM('')
);
#19134=(
BOUNDED_CURVE()
B_SPLINE_CURVE(2,(#77437,#77438,#77439),.UNSPECIFIED.,.F.,.F.)
B_SPLINE_CURVE_WITH_KNOTS((3,3),(0.,0.0709397118056794),.UNSPECIFIED.)
CURVE()
GEOMETRIC_REPRESENTATION_ITEM()
RATIONAL_B_SPLINE_CURVE((1.,1.00002245169207,1.))
REPRESENTATION_ITEM('')
);
#19135=(
BOUNDED_CURVE()
B_SPLINE_CURVE(2,(#77443,#77444,#77445),.UNSPECIFIED.,.F.,.F.)
B_SPLINE_CURVE_WITH_KNOTS((3,3),(0.,0.0709397118056792),.UNSPECIFIED.)
CURVE()
GEOMETRIC_REPRESENTATION_ITEM()
RATIONAL_B_SPLINE_CURVE((1.,1.00002245215096,1.))
REPRESENTATION_ITEM('')
);
#19136=(
BOUNDED_CURVE()
B_SPLINE_CURVE(2,(#77464,#77465,#77466),.UNSPECIFIED.,.F.,.F.)
B_SPLINE_CURVE_WITH_KNOTS((3,3),(0.,0.0709397118056795),.UNSPECIFIED.)
CURVE()
GEOMETRIC_REPRESENTATION_ITEM()
RATIONAL_B_SPLINE_CURVE((1.,1.00002245040396,1.))
REPRESENTATION_ITEM('')
);
#19137=(
BOUNDED_CURVE()
B_SPLINE_CURVE(2,(#77470,#77471,#77472),.UNSPECIFIED.,.F.,.F.)
B_SPLINE_CURVE_WITH_KNOTS((3,3),(0.,0.0424100228697519),.UNSPECIFIED.)
CURVE()
GEOMETRIC_REPRESENTATION_ITEM()
RATIONAL_B_SPLINE_CURVE((1.,1.00001338511468,1.0000107512927))
REPRESENTATION_ITEM('')
);
#19138=(
BOUNDED_CURVE()
B_SPLINE_CURVE(2,(#77474,#77475,#77476),.UNSPECIFIED.,.F.,.F.)
B_SPLINE_CURVE_WITH_KNOTS((3,3),(0.339146964126514,0.668418076018302),
 .UNSPECIFIED.)
CURVE()
GEOMETRIC_REPRESENTATION_ITEM()
RATIONAL_B_SPLINE_CURVE((1.00400190544534,1.00495889669788,1.00400190544534))
REPRESENTATION_ITEM('')
);
#19139=(
BOUNDED_CURVE()
B_SPLINE_CURVE(2,(#77478,#77479,#77480),.UNSPECIFIED.,.F.,.F.)
B_SPLINE_CURVE_WITH_KNOTS((3,3),(0.0284639715386128,0.07087399516029),
 .UNSPECIFIED.)
CURVE()
GEOMETRIC_REPRESENTATION_ITEM()
RATIONAL_B_SPLINE_CURVE((1.00001075071627,1.00001338439739,1.))
REPRESENTATION_ITEM('')
);
#19140=(
BOUNDED_CURVE()
B_SPLINE_CURVE(2,(#77484,#77485,#77486),.UNSPECIFIED.,.F.,.F.)
B_SPLINE_CURVE_WITH_KNOTS((3,3),(0.,0.0424100228448336),.UNSPECIFIED.)
CURVE()
GEOMETRIC_REPRESENTATION_ITEM()
RATIONAL_B_SPLINE_CURVE((1.,1.00001338576537,1.00001075181536))
REPRESENTATION_ITEM('')
);
#19141=(
BOUNDED_CURVE()
B_SPLINE_CURVE(2,(#77488,#77489,#77490),.UNSPECIFIED.,.F.,.F.)
B_SPLINE_CURVE_WITH_KNOTS((3,3),(0.339146964126517,0.668418076018306),
 .UNSPECIFIED.)
CURVE()
GEOMETRIC_REPRESENTATION_ITEM()
RATIONAL_B_SPLINE_CURVE((1.00400190544534,1.00495889669788,1.00400190544534))
REPRESENTATION_ITEM('')
);
#19142=(
BOUNDED_CURVE()
B_SPLINE_CURVE(2,(#77492,#77493,#77494),.UNSPECIFIED.,.F.,.F.)
B_SPLINE_CURVE_WITH_KNOTS((3,3),(0.0284639718304313,0.0708739951602905),
 .UNSPECIFIED.)
CURVE()
GEOMETRIC_REPRESENTATION_ITEM()
RATIONAL_B_SPLINE_CURVE((1.00001075171905,1.00001338564569,1.))
REPRESENTATION_ITEM('')
);
#19143=(
BOUNDED_CURVE()
B_SPLINE_CURVE(2,(#77498,#77499,#77500),.UNSPECIFIED.,.F.,.F.)
B_SPLINE_CURVE_WITH_KNOTS((3,3),(0.,0.0424100233232146),.UNSPECIFIED.)
CURVE()
GEOMETRIC_REPRESENTATION_ITEM()
RATIONAL_B_SPLINE_CURVE((1.,1.00001338411593,1.00001075049031))
REPRESENTATION_ITEM('')
);
#19144=(
BOUNDED_CURVE()
B_SPLINE_CURVE(2,(#77502,#77503,#77504),.UNSPECIFIED.,.F.,.F.)
B_SPLINE_CURVE_WITH_KNOTS((3,3),(0.339146964126517,0.668418076018303),
 .UNSPECIFIED.)
CURVE()
GEOMETRIC_REPRESENTATION_ITEM()
RATIONAL_B_SPLINE_CURVE((1.00400190544534,1.00495889669787,1.00400190544534))
REPRESENTATION_ITEM('')
);
#19145=(
BOUNDED_CURVE()
B_SPLINE_CURVE(2,(#77506,#77507,#77508),.UNSPECIFIED.,.F.,.F.)
B_SPLINE_CURVE_WITH_KNOTS((3,3),(0.0284639713681571,0.0708739951602903),
 .UNSPECIFIED.)
CURVE()
GEOMETRIC_REPRESENTATION_ITEM()
RATIONAL_B_SPLINE_CURVE((1.00001075037836,1.00001338397678,1.))
REPRESENTATION_ITEM('')
);
#19146=(
BOUNDED_CURVE()
B_SPLINE_CURVE(2,(#77512,#77513,#77514),.UNSPECIFIED.,.F.,.F.)
B_SPLINE_CURVE_WITH_KNOTS((3,3),(0.,0.0424100226311801),.UNSPECIFIED.)
CURVE()
GEOMETRIC_REPRESENTATION_ITEM()
RATIONAL_B_SPLINE_CURVE((1.,1.00001338548565,1.00001075159076))
REPRESENTATION_ITEM('')
);
#19147=(
BOUNDED_CURVE()
B_SPLINE_CURVE(2,(#77516,#77517,#77518),.UNSPECIFIED.,.F.,.F.)
B_SPLINE_CURVE_WITH_KNOTS((3,3),(0.339146964126518,0.668418076018302),
 .UNSPECIFIED.)
CURVE()
GEOMETRIC_REPRESENTATION_ITEM()
RATIONAL_B_SPLINE_CURVE((1.00400190544533,1.00495889669787,1.00400190544533))
REPRESENTATION_ITEM('')
);
#19148=(
BOUNDED_CURVE()
B_SPLINE_CURVE(2,(#77520,#77521,#77522),.UNSPECIFIED.,.F.,.F.)
B_SPLINE_CURVE_WITH_KNOTS((3,3),(0.0284639720100238,0.07087399516029),
 .UNSPECIFIED.)
CURVE()
GEOMETRIC_REPRESENTATION_ITEM()
RATIONAL_B_SPLINE_CURVE((1.00001075118356,1.00001338497894,1.))
REPRESENTATION_ITEM('')
);
#19149=(
BOUNDED_CURVE()
B_SPLINE_CURVE(2,(#77526,#77527,#77528),.UNSPECIFIED.,.F.,.F.)
B_SPLINE_CURVE_WITH_KNOTS((3,3),(0.,0.0424100230241298),.UNSPECIFIED.)
CURVE()
GEOMETRIC_REPRESENTATION_ITEM()
RATIONAL_B_SPLINE_CURVE((1.,1.00001338698316,1.00001075279346))
REPRESENTATION_ITEM('')
);
#19150=(
BOUNDED_CURVE()
B_SPLINE_CURVE(2,(#77530,#77531,#77532),.UNSPECIFIED.,.F.,.F.)
B_SPLINE_CURVE_WITH_KNOTS((3,3),(0.339146964126515,0.668418076018307),
 .UNSPECIFIED.)
CURVE()
GEOMETRIC_REPRESENTATION_ITEM()
RATIONAL_B_SPLINE_CURVE((1.00400190544536,1.0049588966979,1.00400190544536))
REPRESENTATION_ITEM('')
);
#19151=(
BOUNDED_CURVE()
B_SPLINE_CURVE(2,(#77534,#77535,#77536),.UNSPECIFIED.,.F.,.F.)
B_SPLINE_CURVE_WITH_KNOTS((3,3),(0.0284639721115161,0.0708739951602901),
 .UNSPECIFIED.)
CURVE()
GEOMETRIC_REPRESENTATION_ITEM()
RATIONAL_B_SPLINE_CURVE((1.00001075066776,1.00001338433673,1.))
REPRESENTATION_ITEM('')
);
#19152=(
BOUNDED_CURVE()
B_SPLINE_CURVE(2,(#77540,#77541,#77542),.UNSPECIFIED.,.F.,.F.)
B_SPLINE_CURVE_WITH_KNOTS((3,3),(0.,0.0424100237464711),.UNSPECIFIED.)
CURVE()
GEOMETRIC_REPRESENTATION_ITEM()
RATIONAL_B_SPLINE_CURVE((1.,1.00001338457639,1.00001075086))
REPRESENTATION_ITEM('')
);
#19153=(
BOUNDED_CURVE()
B_SPLINE_CURVE(2,(#77544,#77545,#77546),.UNSPECIFIED.,.F.,.F.)
B_SPLINE_CURVE_WITH_KNOTS((3,3),(0.339146964126521,0.668418076018307),
 .UNSPECIFIED.)
CURVE()
GEOMETRIC_REPRESENTATION_ITEM()
RATIONAL_B_SPLINE_CURVE((1.00400190544534,1.00495889669787,1.00400190544534))
REPRESENTATION_ITEM('')
);
#19154=(
BOUNDED_CURVE()
B_SPLINE_CURVE(2,(#77548,#77549,#77550),.UNSPECIFIED.,.F.,.F.)
B_SPLINE_CURVE_WITH_KNOTS((3,3),(0.0284639714302619,0.0708739951602905),
 .UNSPECIFIED.)
CURVE()
GEOMETRIC_REPRESENTATION_ITEM()
RATIONAL_B_SPLINE_CURVE((1.00001075131298,1.00001338514034,1.))
REPRESENTATION_ITEM('')
);
#19155=(
BOUNDED_CURVE()
B_SPLINE_CURVE(2,(#77554,#77555,#77556),.UNSPECIFIED.,.F.,.F.)
B_SPLINE_CURVE_WITH_KNOTS((3,3),(0.,0.0424100231669585),.UNSPECIFIED.)
CURVE()
GEOMETRIC_REPRESENTATION_ITEM()
RATIONAL_B_SPLINE_CURVE((1.,1.00001338549266,1.00001075159619))
REPRESENTATION_ITEM('')
);
#19156=(
BOUNDED_CURVE()
B_SPLINE_CURVE(2,(#77558,#77559,#77560),.UNSPECIFIED.,.F.,.F.)
B_SPLINE_CURVE_WITH_KNOTS((3,3),(0.339146964126509,0.668418076018305),
 .UNSPECIFIED.)
CURVE()
GEOMETRIC_REPRESENTATION_ITEM()
RATIONAL_B_SPLINE_CURVE((1.00400190544537,1.00495889669791,1.00400190544537))
REPRESENTATION_ITEM('')
);
#19157=(
BOUNDED_CURVE()
B_SPLINE_CURVE(2,(#77562,#77563,#77564),.UNSPECIFIED.,.F.,.F.)
B_SPLINE_CURVE_WITH_KNOTS((3,3),(0.0284639724895236,0.0708739951602903),
 .UNSPECIFIED.)
CURVE()
GEOMETRIC_REPRESENTATION_ITEM()
RATIONAL_B_SPLINE_CURVE((1.00001075242956,1.00001338652996,1.))
REPRESENTATION_ITEM('')
);
#19158=(
BOUNDED_CURVE()
B_SPLINE_CURVE(2,(#77568,#77569,#77570),.UNSPECIFIED.,.F.,.F.)
B_SPLINE_CURVE_WITH_KNOTS((3,3),(0.,0.0424100230945575),.UNSPECIFIED.)
CURVE()
GEOMETRIC_REPRESENTATION_ITEM()
RATIONAL_B_SPLINE_CURVE((1.,1.00001338444694,1.00001075075626))
REPRESENTATION_ITEM('')
);
#19159=(
BOUNDED_CURVE()
B_SPLINE_CURVE(2,(#77572,#77573,#77574),.UNSPECIFIED.,.F.,.F.)
B_SPLINE_CURVE_WITH_KNOTS((3,3),(0.339146964126516,0.668418076018306),
 .UNSPECIFIED.)
CURVE()
GEOMETRIC_REPRESENTATION_ITEM()
RATIONAL_B_SPLINE_CURVE((1.00400190544535,1.00495889669789,1.00400190544535))
REPRESENTATION_ITEM('')
);
#19160=(
BOUNDED_CURVE()
B_SPLINE_CURVE(2,(#77576,#77577,#77578),.UNSPECIFIED.,.F.,.F.)
B_SPLINE_CURVE_WITH_KNOTS((3,3),(0.0284639718822116,0.0708739951602902),
 .UNSPECIFIED.)
CURVE()
GEOMETRIC_REPRESENTATION_ITEM()
RATIONAL_B_SPLINE_CURVE((1.00001075159531,1.00001338549162,1.))
REPRESENTATION_ITEM('')
);
#19161=(
BOUNDED_CURVE()
B_SPLINE_CURVE(2,(#77582,#77583,#77584),.UNSPECIFIED.,.F.,.F.)
B_SPLINE_CURVE_WITH_KNOTS((3,3),(0.,0.0424100233379413),.UNSPECIFIED.)
CURVE()
GEOMETRIC_REPRESENTATION_ITEM()
RATIONAL_B_SPLINE_CURVE((1.,1.0000133853148,1.00001075145326))
REPRESENTATION_ITEM('')
);
#19162=(
BOUNDED_CURVE()
B_SPLINE_CURVE(2,(#77586,#77587,#77588),.UNSPECIFIED.,.F.,.F.)
B_SPLINE_CURVE_WITH_KNOTS((3,3),(0.339146964126514,0.668418076018307),
 .UNSPECIFIED.)
CURVE()
GEOMETRIC_REPRESENTATION_ITEM()
RATIONAL_B_SPLINE_CURVE((1.00400190544536,1.0049588966979,1.00400190544536))
REPRESENTATION_ITEM('')
);
#19163=(
BOUNDED_CURVE()
B_SPLINE_CURVE(2,(#77590,#77591,#77592),.UNSPECIFIED.,.F.,.F.)
B_SPLINE_CURVE_WITH_KNOTS((3,3),(0.0284639723011819,0.0708739951602902),
 .UNSPECIFIED.)
CURVE()
GEOMETRIC_REPRESENTATION_ITEM()
RATIONAL_B_SPLINE_CURVE((1.00001075145909,1.00001338532183,1.))
REPRESENTATION_ITEM('')
);
#19164=(
BOUNDED_CURVE()
B_SPLINE_CURVE(2,(#77596,#77597,#77598),.UNSPECIFIED.,.F.,.F.)
B_SPLINE_CURVE_WITH_KNOTS((3,3),(0.,0.0424100235660184),.UNSPECIFIED.)
CURVE()
GEOMETRIC_REPRESENTATION_ITEM()
RATIONAL_B_SPLINE_CURVE((1.,1.0000133839457,1.00001075035348))
REPRESENTATION_ITEM('')
);
#19165=(
BOUNDED_CURVE()
B_SPLINE_CURVE(2,(#77600,#77601,#77602),.UNSPECIFIED.,.F.,.F.)
B_SPLINE_CURVE_WITH_KNOTS((3,3),(0.339146964126508,0.668418076018301),
 .UNSPECIFIED.)
CURVE()
GEOMETRIC_REPRESENTATION_ITEM()
RATIONAL_B_SPLINE_CURVE((1.00400190544536,1.0049588966979,1.00400190544536))
REPRESENTATION_ITEM('')
);
#19166=(
BOUNDED_CURVE()
B_SPLINE_CURVE(2,(#77604,#77605,#77606),.UNSPECIFIED.,.F.,.F.)
B_SPLINE_CURVE_WITH_KNOTS((3,3),(0.0284639720583302,0.0708739951602905),
 .UNSPECIFIED.)
CURVE()
GEOMETRIC_REPRESENTATION_ITEM()
RATIONAL_B_SPLINE_CURVE((1.00001075112448,1.00001338490536,1.))
REPRESENTATION_ITEM('')
);
#19167=(
BOUNDED_CURVE()
B_SPLINE_CURVE(2,(#77610,#77611,#77612),.UNSPECIFIED.,.F.,.F.)
B_SPLINE_CURVE_WITH_KNOTS((3,3),(0.,0.0424100228529261),.UNSPECIFIED.)
CURVE()
GEOMETRIC_REPRESENTATION_ITEM()
RATIONAL_B_SPLINE_CURVE((1.,1.00001338602191,1.00001075202142))
REPRESENTATION_ITEM('')
);
#19168=(
BOUNDED_CURVE()
B_SPLINE_CURVE(2,(#77614,#77615,#77616),.UNSPECIFIED.,.F.,.F.)
B_SPLINE_CURVE_WITH_KNOTS((3,3),(0.339146964126517,0.668418076018306),
 .UNSPECIFIED.)
CURVE()
GEOMETRIC_REPRESENTATION_ITEM()
RATIONAL_B_SPLINE_CURVE((1.00400190544534,1.00495889669788,1.00400190544534))
REPRESENTATION_ITEM('')
);
#19169=(
BOUNDED_CURVE()
B_SPLINE_CURVE(2,(#77618,#77619,#77620),.UNSPECIFIED.,.F.,.F.)
B_SPLINE_CURVE_WITH_KNOTS((3,3),(0.028463971052142,0.0708739951602904),
 .UNSPECIFIED.)
CURVE()
GEOMETRIC_REPRESENTATION_ITEM()
RATIONAL_B_SPLINE_CURVE((1.00001075114436,1.00001338493058,1.))
REPRESENTATION_ITEM('')
);
#19170=(
BOUNDED_CURVE()
B_SPLINE_CURVE(2,(#77646,#77647,#77648),.UNSPECIFIED.,.F.,.F.)
B_SPLINE_CURVE_WITH_KNOTS((3,3),(0.,0.0424100231388671),.UNSPECIFIED.)
CURVE()
GEOMETRIC_REPRESENTATION_ITEM()
RATIONAL_B_SPLINE_CURVE((1.,1.00001338664572,1.00001075252237))
REPRESENTATION_ITEM('')
);
#19171=(
BOUNDED_CURVE()
B_SPLINE_CURVE(2,(#77650,#77651,#77652),.UNSPECIFIED.,.F.,.F.)
B_SPLINE_CURVE_WITH_KNOTS((3,3),(0.339146964126515,0.668418076018309),
 .UNSPECIFIED.)
CURVE()
GEOMETRIC_REPRESENTATION_ITEM()
RATIONAL_B_SPLINE_CURVE((1.00400190544536,1.0049588966979,1.00400190544536))
REPRESENTATION_ITEM('')
);
#19172=(
BOUNDED_CURVE()
B_SPLINE_CURVE(2,(#77654,#77655,#77656),.UNSPECIFIED.,.F.,.F.)
B_SPLINE_CURVE_WITH_KNOTS((3,3),(0.0284639723015322,0.0708739951602894),
 .UNSPECIFIED.)
CURVE()
GEOMETRIC_REPRESENTATION_ITEM()
RATIONAL_B_SPLINE_CURVE((1.00001075245622,1.00001338656323,1.))
REPRESENTATION_ITEM('')
);
#19173=(
BOUNDED_CURVE()
B_SPLINE_CURVE(2,(#77660,#77661,#77662),.UNSPECIFIED.,.F.,.F.)
B_SPLINE_CURVE_WITH_KNOTS((3,3),(0.,0.0424100231020988),.UNSPECIFIED.)
CURVE()
GEOMETRIC_REPRESENTATION_ITEM()
RATIONAL_B_SPLINE_CURVE((1.,1.00001338440371,1.00001075072154))
REPRESENTATION_ITEM('')
);
#19174=(
BOUNDED_CURVE()
B_SPLINE_CURVE(2,(#77664,#77665,#77666),.UNSPECIFIED.,.F.,.F.)
B_SPLINE_CURVE_WITH_KNOTS((3,3),(0.339146964126511,0.668418076018296),
 .UNSPECIFIED.)
CURVE()
GEOMETRIC_REPRESENTATION_ITEM()
RATIONAL_B_SPLINE_CURVE((1.00400190544533,1.00495889669787,1.00400190544533))
REPRESENTATION_ITEM('')
);
#19175=(
BOUNDED_CURVE()
B_SPLINE_CURVE(2,(#77668,#77669,#77670),.UNSPECIFIED.,.F.,.F.)
B_SPLINE_CURVE_WITH_KNOTS((3,3),(0.0284639708332421,0.0708739951602892),
 .UNSPECIFIED.)
CURVE()
GEOMETRIC_REPRESENTATION_ITEM()
RATIONAL_B_SPLINE_CURVE((1.00001075092413,1.00001338465651,1.))
REPRESENTATION_ITEM('')
);
#19176=(
BOUNDED_CURVE()
B_SPLINE_CURVE(2,(#77674,#77675,#77676),.UNSPECIFIED.,.F.,.F.)
B_SPLINE_CURVE_WITH_KNOTS((3,3),(0.,0.0424100226742728),.UNSPECIFIED.)
CURVE()
GEOMETRIC_REPRESENTATION_ITEM()
RATIONAL_B_SPLINE_CURVE((1.,1.00001338671076,1.00001075257479))
REPRESENTATION_ITEM('')
);
#19177=(
BOUNDED_CURVE()
B_SPLINE_CURVE(2,(#77678,#77679,#77680),.UNSPECIFIED.,.F.,.F.)
B_SPLINE_CURVE_WITH_KNOTS((3,3),(0.339146964126517,0.668418076018305),
 .UNSPECIFIED.)
CURVE()
GEOMETRIC_REPRESENTATION_ITEM()
RATIONAL_B_SPLINE_CURVE((1.00400190544534,1.00495889669788,1.00400190544534))
REPRESENTATION_ITEM('')
);
#19178=(
BOUNDED_CURVE()
B_SPLINE_CURVE(2,(#77682,#77683,#77684),.UNSPECIFIED.,.F.,.F.)
B_SPLINE_CURVE_WITH_KNOTS((3,3),(0.0284639727500967,0.0708739951602894),
 .UNSPECIFIED.)
CURVE()
GEOMETRIC_REPRESENTATION_ITEM()
RATIONAL_B_SPLINE_CURVE((1.00001075141119,1.00001338526198,1.))
REPRESENTATION_ITEM('')
);
#19179=(
BOUNDED_CURVE()
B_SPLINE_CURVE(2,(#77688,#77689,#77690),.UNSPECIFIED.,.F.,.F.)
B_SPLINE_CURVE_WITH_KNOTS((3,3),(0.,0.0424100234036622),.UNSPECIFIED.)
CURVE()
GEOMETRIC_REPRESENTATION_ITEM()
RATIONAL_B_SPLINE_CURVE((1.,1.00001338508687,1.00001075127016))
REPRESENTATION_ITEM('')
);
#19180=(
BOUNDED_CURVE()
B_SPLINE_CURVE(2,(#77692,#77693,#77694),.UNSPECIFIED.,.F.,.F.)
B_SPLINE_CURVE_WITH_KNOTS((3,3),(0.339146964126515,0.668418076018302),
 .UNSPECIFIED.)
CURVE()
GEOMETRIC_REPRESENTATION_ITEM()
RATIONAL_B_SPLINE_CURVE((1.00400190544534,1.00495889669787,1.00400190544534))
REPRESENTATION_ITEM('')
);
#19181=(
BOUNDED_CURVE()
B_SPLINE_CURVE(2,(#77696,#77697,#77698),.UNSPECIFIED.,.F.,.F.)
B_SPLINE_CURVE_WITH_KNOTS((3,3),(0.0284639712775601,0.0708739951602893),
 .UNSPECIFIED.)
CURVE()
GEOMETRIC_REPRESENTATION_ITEM()
RATIONAL_B_SPLINE_CURVE((1.00001075126605,1.00001338508198,1.))
REPRESENTATION_ITEM('')
);
#19182=(
BOUNDED_CURVE()
B_SPLINE_CURVE(2,(#77702,#77703,#77704),.UNSPECIFIED.,.F.,.F.)
B_SPLINE_CURVE_WITH_KNOTS((3,3),(0.,0.0424100240945264),.UNSPECIFIED.)
CURVE()
GEOMETRIC_REPRESENTATION_ITEM()
RATIONAL_B_SPLINE_CURVE((1.,1.00001338487308,1.00001075109818))
REPRESENTATION_ITEM('')
);
#19183=(
BOUNDED_CURVE()
B_SPLINE_CURVE(2,(#77706,#77707,#77708),.UNSPECIFIED.,.F.,.F.)
B_SPLINE_CURVE_WITH_KNOTS((3,3),(0.339146964126523,0.668418076018308),
 .UNSPECIFIED.)
CURVE()
GEOMETRIC_REPRESENTATION_ITEM()
RATIONAL_B_SPLINE_CURVE((1.00400190544534,1.00495889669787,1.00400190544534))
REPRESENTATION_ITEM('')
);
#19184=(
BOUNDED_CURVE()
B_SPLINE_CURVE(2,(#77710,#77711,#77712),.UNSPECIFIED.,.F.,.F.)
B_SPLINE_CURVE_WITH_KNOTS((3,3),(0.0284639720159432,0.0708739951602889),
 .UNSPECIFIED.)
CURVE()
GEOMETRIC_REPRESENTATION_ITEM()
RATIONAL_B_SPLINE_CURVE((1.00001075167528,1.00001338559111,1.))
REPRESENTATION_ITEM('')
);
#19185=(
BOUNDED_CURVE()
B_SPLINE_CURVE(2,(#77716,#77717,#77718),.UNSPECIFIED.,.F.,.F.)
B_SPLINE_CURVE_WITH_KNOTS((3,3),(0.,0.0424100244249126),.UNSPECIFIED.)
CURVE()
GEOMETRIC_REPRESENTATION_ITEM()
RATIONAL_B_SPLINE_CURVE((1.,1.0000133850762,1.0000107512612))
REPRESENTATION_ITEM('')
);
#19186=(
BOUNDED_CURVE()
B_SPLINE_CURVE(2,(#77720,#77721,#77722),.UNSPECIFIED.,.F.,.F.)
B_SPLINE_CURVE_WITH_KNOTS((3,3),(0.339146964126521,0.668418076018309),
 .UNSPECIFIED.)
CURVE()
GEOMETRIC_REPRESENTATION_ITEM()
RATIONAL_B_SPLINE_CURVE((1.00400190544534,1.00495889669788,1.00400190544534))
REPRESENTATION_ITEM('')
);
#19187=(
BOUNDED_CURVE()
B_SPLINE_CURVE(2,(#77724,#77725,#77726),.UNSPECIFIED.,.F.,.F.)
B_SPLINE_CURVE_WITH_KNOTS((3,3),(0.0284639713982658,0.0708739951602894),
 .UNSPECIFIED.)
CURVE()
GEOMETRIC_REPRESENTATION_ITEM()
RATIONAL_B_SPLINE_CURVE((1.0000107515649,1.00001338545398,1.))
REPRESENTATION_ITEM('')
);
#19188=(
BOUNDED_CURVE()
B_SPLINE_CURVE(2,(#77730,#77731,#77732),.UNSPECIFIED.,.F.,.F.)
B_SPLINE_CURVE_WITH_KNOTS((3,3),(0.,0.0424100230579472),.UNSPECIFIED.)
CURVE()
GEOMETRIC_REPRESENTATION_ITEM()
RATIONAL_B_SPLINE_CURVE((1.,1.00001338543977,1.00001075155375))
REPRESENTATION_ITEM('')
);
#19189=(
BOUNDED_CURVE()
B_SPLINE_CURVE(2,(#77734,#77735,#77736),.UNSPECIFIED.,.F.,.F.)
B_SPLINE_CURVE_WITH_KNOTS((3,3),(0.339146964126514,0.668418076018301),
 .UNSPECIFIED.)
CURVE()
GEOMETRIC_REPRESENTATION_ITEM()
RATIONAL_B_SPLINE_CURVE((1.00400190544534,1.00495889669788,1.00400190544534))
REPRESENTATION_ITEM('')
);
#19190=(
BOUNDED_CURVE()
B_SPLINE_CURVE(2,(#77738,#77739,#77740),.UNSPECIFIED.,.F.,.F.)
B_SPLINE_CURVE_WITH_KNOTS((3,3),(0.0284639721460146,0.0708739951602892),
 .UNSPECIFIED.)
CURVE()
GEOMETRIC_REPRESENTATION_ITEM()
RATIONAL_B_SPLINE_CURVE((1.00001075127041,1.00001338508699,1.))
REPRESENTATION_ITEM('')
);
#19191=(
BOUNDED_CURVE()
B_SPLINE_CURVE(2,(#77744,#77745,#77746),.UNSPECIFIED.,.F.,.F.)
B_SPLINE_CURVE_WITH_KNOTS((3,3),(0.,0.04241002310436),.UNSPECIFIED.)
CURVE()
GEOMETRIC_REPRESENTATION_ITEM()
RATIONAL_B_SPLINE_CURVE((1.,1.00001338427162,1.00001075061544))
REPRESENTATION_ITEM('')
);
#19192=(
BOUNDED_CURVE()
B_SPLINE_CURVE(2,(#77748,#77749,#77750),.UNSPECIFIED.,.F.,.F.)
B_SPLINE_CURVE_WITH_KNOTS((3,3),(0.339146964126508,0.668418076018301),
 .UNSPECIFIED.)
CURVE()
GEOMETRIC_REPRESENTATION_ITEM()
RATIONAL_B_SPLINE_CURVE((1.00400190544536,1.0049588966979,1.00400190544536))
REPRESENTATION_ITEM('')
);
#19193=(
BOUNDED_CURVE()
B_SPLINE_CURVE(2,(#77752,#77753,#77754),.UNSPECIFIED.,.F.,.F.)
B_SPLINE_CURVE_WITH_KNOTS((3,3),(0.0284639718065398,0.0708739951602892),
 .UNSPECIFIED.)
CURVE()
GEOMETRIC_REPRESENTATION_ITEM()
RATIONAL_B_SPLINE_CURVE((1.00001075054903,1.00001338418905,1.))
REPRESENTATION_ITEM('')
);
#19194=(
BOUNDED_CURVE()
B_SPLINE_CURVE(2,(#77758,#77759,#77760),.UNSPECIFIED.,.F.,.F.)
B_SPLINE_CURVE_WITH_KNOTS((3,3),(0.,0.0424100238902531),.UNSPECIFIED.)
CURVE()
GEOMETRIC_REPRESENTATION_ITEM()
RATIONAL_B_SPLINE_CURVE((1.,1.00001338471342,1.00001075097001))
REPRESENTATION_ITEM('')
);
#19195=(
BOUNDED_CURVE()
B_SPLINE_CURVE(2,(#77762,#77763,#77764),.UNSPECIFIED.,.F.,.F.)
B_SPLINE_CURVE_WITH_KNOTS((3,3),(0.339146964126505,0.668418076018296),
 .UNSPECIFIED.)
CURVE()
GEOMETRIC_REPRESENTATION_ITEM()
RATIONAL_B_SPLINE_CURVE((1.00400190544535,1.00495889669789,1.00400190544535))
REPRESENTATION_ITEM('')
);
#19196=(
BOUNDED_CURVE()
B_SPLINE_CURVE(2,(#77766,#77767,#77768),.UNSPECIFIED.,.F.,.F.)
B_SPLINE_CURVE_WITH_KNOTS((3,3),(0.0284639726785229,0.0708739951602891),
 .UNSPECIFIED.)
CURVE()
GEOMETRIC_REPRESENTATION_ITEM()
RATIONAL_B_SPLINE_CURVE((1.00001075174529,1.00001338567796,1.))
REPRESENTATION_ITEM('')
);
#19197=(
BOUNDED_CURVE()
B_SPLINE_CURVE(2,(#77772,#77773,#77774),.UNSPECIFIED.,.F.,.F.)
B_SPLINE_CURVE_WITH_KNOTS((3,3),(0.,0.0424100231217665),.UNSPECIFIED.)
CURVE()
GEOMETRIC_REPRESENTATION_ITEM()
RATIONAL_B_SPLINE_CURVE((1.,1.00001338590548,1.00001075192779))
REPRESENTATION_ITEM('')
);
#19198=(
BOUNDED_CURVE()
B_SPLINE_CURVE(2,(#77776,#77777,#77778),.UNSPECIFIED.,.F.,.F.)
B_SPLINE_CURVE_WITH_KNOTS((3,3),(0.339146964126517,0.668418076018306),
 .UNSPECIFIED.)
CURVE()
GEOMETRIC_REPRESENTATION_ITEM()
RATIONAL_B_SPLINE_CURVE((1.00400190544534,1.00495889669788,1.00400190544534))
REPRESENTATION_ITEM('')
);
#19199=(
BOUNDED_CURVE()
B_SPLINE_CURVE(2,(#77780,#77781,#77782),.UNSPECIFIED.,.F.,.F.)
B_SPLINE_CURVE_WITH_KNOTS((3,3),(0.0284639722994484,0.0708739951602894),
 .UNSPECIFIED.)
CURVE()
GEOMETRIC_REPRESENTATION_ITEM()
RATIONAL_B_SPLINE_CURVE((1.00001075268953,1.0000133868537,1.))
REPRESENTATION_ITEM('')
);
#19200=(
BOUNDED_CURVE()
B_SPLINE_CURVE(2,(#77786,#77787,#77788),.UNSPECIFIED.,.F.,.F.)
B_SPLINE_CURVE_WITH_KNOTS((3,3),(0.,0.0424100235663187),.UNSPECIFIED.)
CURVE()
GEOMETRIC_REPRESENTATION_ITEM()
RATIONAL_B_SPLINE_CURVE((1.,1.00001338431496,1.00001075065008))
REPRESENTATION_ITEM('')
);
#19201=(
BOUNDED_CURVE()
B_SPLINE_CURVE(2,(#77790,#77791,#77792),.UNSPECIFIED.,.F.,.F.)
B_SPLINE_CURVE_WITH_KNOTS((3,3),(0.339146964126511,0.668418076018303),
 .UNSPECIFIED.)
CURVE()
GEOMETRIC_REPRESENTATION_ITEM()
RATIONAL_B_SPLINE_CURVE((1.00400190544536,1.0049588966979,1.00400190544536))
REPRESENTATION_ITEM('')
);
#19202=(
BOUNDED_CURVE()
B_SPLINE_CURVE(2,(#77794,#77795,#77796),.UNSPECIFIED.,.F.,.F.)
B_SPLINE_CURVE_WITH_KNOTS((3,3),(0.0284639715440609,0.0708739951602894),
 .UNSPECIFIED.)
CURVE()
GEOMETRIC_REPRESENTATION_ITEM()
RATIONAL_B_SPLINE_CURVE((1.00001075063711,1.00001338429884,1.))
REPRESENTATION_ITEM('')
);
#19203=(
BOUNDED_CURVE()
B_SPLINE_CURVE(2,(#77799,#77800,#77801),.UNSPECIFIED.,.F.,.F.)
B_SPLINE_CURVE_WITH_KNOTS((3,3),(0.,0.0709397118056797),.UNSPECIFIED.)
CURVE()
GEOMETRIC_REPRESENTATION_ITEM()
RATIONAL_B_SPLINE_CURVE((1.,1.00002245139626,1.))
REPRESENTATION_ITEM('')
);
#19204=(
BOUNDED_CURVE()
B_SPLINE_CURVE(2,(#77804,#77805,#77806),.UNSPECIFIED.,.F.,.F.)
B_SPLINE_CURVE_WITH_KNOTS((3,3),(0.,0.0709397118056796),.UNSPECIFIED.)
CURVE()
GEOMETRIC_REPRESENTATION_ITEM()
RATIONAL_B_SPLINE_CURVE((1.,1.00002245118033,1.))
REPRESENTATION_ITEM('')
);
#19205=(
BOUNDED_CURVE()
B_SPLINE_CURVE(2,(#77810,#77811,#77812),.UNSPECIFIED.,.F.,.F.)
B_SPLINE_CURVE_WITH_KNOTS((3,3),(0.,0.0424100230703566),.UNSPECIFIED.)
CURVE()
GEOMETRIC_REPRESENTATION_ITEM()
RATIONAL_B_SPLINE_CURVE((1.,1.00001338676863,1.00001075262112))
REPRESENTATION_ITEM('')
);
#19206=(
BOUNDED_CURVE()
B_SPLINE_CURVE(2,(#77814,#77815,#77816),.UNSPECIFIED.,.F.,.F.)
B_SPLINE_CURVE_WITH_KNOTS((3,3),(0.339146964126514,0.668418076018302),
 .UNSPECIFIED.)
CURVE()
GEOMETRIC_REPRESENTATION_ITEM()
RATIONAL_B_SPLINE_CURVE((1.00400190544535,1.00495889669788,1.00400190544535))
REPRESENTATION_ITEM('')
);
#19207=(
BOUNDED_CURVE()
B_SPLINE_CURVE(2,(#77818,#77819,#77820),.UNSPECIFIED.,.F.,.F.)
B_SPLINE_CURVE_WITH_KNOTS((3,3),(0.0284639721307315,0.0708739951602897),
 .UNSPECIFIED.)
CURVE()
GEOMETRIC_REPRESENTATION_ITEM()
RATIONAL_B_SPLINE_CURVE((1.00001075251047,1.00001338663085,1.))
REPRESENTATION_ITEM('')
);
#19208=(
BOUNDED_CURVE()
B_SPLINE_CURVE(2,(#77824,#77825,#77826),.UNSPECIFIED.,.F.,.F.)
B_SPLINE_CURVE_WITH_KNOTS((3,3),(0.,0.0424100231451836),.UNSPECIFIED.)
CURVE()
GEOMETRIC_REPRESENTATION_ITEM()
RATIONAL_B_SPLINE_CURVE((1.,1.0000133845857,1.0000107508677))
REPRESENTATION_ITEM('')
);
#19209=(
BOUNDED_CURVE()
B_SPLINE_CURVE(2,(#77828,#77829,#77830),.UNSPECIFIED.,.F.,.F.)
B_SPLINE_CURVE_WITH_KNOTS((3,3),(0.33914696412651,0.668418076018305),
 .UNSPECIFIED.)
CURVE()
GEOMETRIC_REPRESENTATION_ITEM()
RATIONAL_B_SPLINE_CURVE((1.00400190544536,1.0049588966979,1.00400190544536))
REPRESENTATION_ITEM('')
);
#19210=(
BOUNDED_CURVE()
B_SPLINE_CURVE(2,(#77832,#77833,#77834),.UNSPECIFIED.,.F.,.F.)
B_SPLINE_CURVE_WITH_KNOTS((3,3),(0.0284639724981747,0.0708739951602894),
 .UNSPECIFIED.)
CURVE()
GEOMETRIC_REPRESENTATION_ITEM()
RATIONAL_B_SPLINE_CURVE((1.00001075165203,1.00001338556194,1.))
REPRESENTATION_ITEM('')
);
#19211=(
BOUNDED_CURVE()
B_SPLINE_CURVE(2,(#77838,#77839,#77840),.UNSPECIFIED.,.F.,.F.)
B_SPLINE_CURVE_WITH_KNOTS((3,3),(0.,0.0424100229360319),.UNSPECIFIED.)
CURVE()
GEOMETRIC_REPRESENTATION_ITEM()
RATIONAL_B_SPLINE_CURVE((1.,1.00001338532576,1.00001075146222))
REPRESENTATION_ITEM('')
);
#19212=(
BOUNDED_CURVE()
B_SPLINE_CURVE(2,(#77842,#77843,#77844),.UNSPECIFIED.,.F.,.F.)
B_SPLINE_CURVE_WITH_KNOTS((3,3),(0.339146964126522,0.668418076018311),
 .UNSPECIFIED.)
CURVE()
GEOMETRIC_REPRESENTATION_ITEM()
RATIONAL_B_SPLINE_CURVE((1.00400190544535,1.00495889669788,1.00400190544535))
REPRESENTATION_ITEM('')
);
#19213=(
BOUNDED_CURVE()
B_SPLINE_CURVE(2,(#77846,#77847,#77848),.UNSPECIFIED.,.F.,.F.)
B_SPLINE_CURVE_WITH_KNOTS((3,3),(0.0284639726217467,0.0708739951602899),
 .UNSPECIFIED.)
CURVE()
GEOMETRIC_REPRESENTATION_ITEM()
RATIONAL_B_SPLINE_CURVE((1.00001075156159,1.00001338544929,1.))
REPRESENTATION_ITEM('')
);
#19214=(
BOUNDED_CURVE()
B_SPLINE_CURVE(2,(#77852,#77853,#77854),.UNSPECIFIED.,.F.,.F.)
B_SPLINE_CURVE_WITH_KNOTS((3,3),(0.,0.0424100234950521),.UNSPECIFIED.)
CURVE()
GEOMETRIC_REPRESENTATION_ITEM()
RATIONAL_B_SPLINE_CURVE((1.,1.00001338503236,1.00001075122634))
REPRESENTATION_ITEM('')
);
#19215=(
BOUNDED_CURVE()
B_SPLINE_CURVE(2,(#77856,#77857,#77858),.UNSPECIFIED.,.F.,.F.)
B_SPLINE_CURVE_WITH_KNOTS((3,3),(0.339146964126523,0.668418076018307),
 .UNSPECIFIED.)
CURVE()
GEOMETRIC_REPRESENTATION_ITEM()
RATIONAL_B_SPLINE_CURVE((1.00400190544533,1.00495889669786,1.00400190544533))
REPRESENTATION_ITEM('')
);
#19216=(
BOUNDED_CURVE()
B_SPLINE_CURVE(2,(#77860,#77861,#77862),.UNSPECIFIED.,.F.,.F.)
B_SPLINE_CURVE_WITH_KNOTS((3,3),(0.0284639715189242,0.0708739951602895),
 .UNSPECIFIED.)
CURVE()
GEOMETRIC_REPRESENTATION_ITEM()
RATIONAL_B_SPLINE_CURVE((1.00001075178646,1.00001338572976,1.))
REPRESENTATION_ITEM('')
);
#19217=(
BOUNDED_CURVE()
B_SPLINE_CURVE(2,(#77866,#77867,#77868),.UNSPECIFIED.,.F.,.F.)
B_SPLINE_CURVE_WITH_KNOTS((3,3),(0.,0.0424100236202695),.UNSPECIFIED.)
CURVE()
GEOMETRIC_REPRESENTATION_ITEM()
RATIONAL_B_SPLINE_CURVE((1.,1.00001338464189,1.00001075091266))
REPRESENTATION_ITEM('')
);
#19218=(
BOUNDED_CURVE()
B_SPLINE_CURVE(2,(#77870,#77871,#77872),.UNSPECIFIED.,.F.,.F.)
B_SPLINE_CURVE_WITH_KNOTS((3,3),(0.339146964126517,0.668418076018307),
 .UNSPECIFIED.)
CURVE()
GEOMETRIC_REPRESENTATION_ITEM()
RATIONAL_B_SPLINE_CURVE((1.00400190544535,1.00495889669789,1.00400190544535))
REPRESENTATION_ITEM('')
);
#19219=(
BOUNDED_CURVE()
B_SPLINE_CURVE(2,(#77874,#77875,#77876),.UNSPECIFIED.,.F.,.F.)
B_SPLINE_CURVE_WITH_KNOTS((3,3),(0.0284639715457675,0.0708739951602893),
 .UNSPECIFIED.)
CURVE()
GEOMETRIC_REPRESENTATION_ITEM()
RATIONAL_B_SPLINE_CURVE((1.00001075081926,1.00001338452561,1.))
REPRESENTATION_ITEM('')
);
#19220=(
BOUNDED_CURVE()
B_SPLINE_CURVE(2,(#77880,#77881,#77882),.UNSPECIFIED.,.F.,.F.)
B_SPLINE_CURVE_WITH_KNOTS((3,3),(0.,0.0424100233833892),.UNSPECIFIED.)
CURVE()
GEOMETRIC_REPRESENTATION_ITEM()
RATIONAL_B_SPLINE_CURVE((1.,1.00001338550802,1.00001075160844))
REPRESENTATION_ITEM('')
);
#19221=(
BOUNDED_CURVE()
B_SPLINE_CURVE(2,(#77884,#77885,#77886),.UNSPECIFIED.,.F.,.F.)
B_SPLINE_CURVE_WITH_KNOTS((3,3),(0.339146964126518,0.668418076018304),
 .UNSPECIFIED.)
CURVE()
GEOMETRIC_REPRESENTATION_ITEM()
RATIONAL_B_SPLINE_CURVE((1.00400190544534,1.00495889669787,1.00400190544534))
REPRESENTATION_ITEM('')
);
#19222=(
BOUNDED_CURVE()
B_SPLINE_CURVE(2,(#77888,#77889,#77890),.UNSPECIFIED.,.F.,.F.)
B_SPLINE_CURVE_WITH_KNOTS((3,3),(0.0284639718266628,0.0708739951602895),
 .UNSPECIFIED.)
CURVE()
GEOMETRIC_REPRESENTATION_ITEM()
RATIONAL_B_SPLINE_CURVE((1.00001075166489,1.00001338557827,1.))
REPRESENTATION_ITEM('')
);
#19223=(
BOUNDED_CURVE()
B_SPLINE_CURVE(2,(#77894,#77895,#77896),.UNSPECIFIED.,.F.,.F.)
B_SPLINE_CURVE_WITH_KNOTS((3,3),(0.,0.0424100233211347),.UNSPECIFIED.)
CURVE()
GEOMETRIC_REPRESENTATION_ITEM()
RATIONAL_B_SPLINE_CURVE((1.,1.00001338542288,1.00001075154008))
REPRESENTATION_ITEM('')
);
#19224=(
BOUNDED_CURVE()
B_SPLINE_CURVE(2,(#77898,#77899,#77900),.UNSPECIFIED.,.F.,.F.)
B_SPLINE_CURVE_WITH_KNOTS((3,3),(0.339146964126512,0.668418076018303),
 .UNSPECIFIED.)
CURVE()
GEOMETRIC_REPRESENTATION_ITEM()
RATIONAL_B_SPLINE_CURVE((1.00400190544535,1.00495889669789,1.00400190544535))
REPRESENTATION_ITEM('')
);
#19225=(
BOUNDED_CURVE()
B_SPLINE_CURVE(2,(#77902,#77903,#77904),.UNSPECIFIED.,.F.,.F.)
B_SPLINE_CURVE_WITH_KNOTS((3,3),(0.028463972158878,0.0708739951602892),
 .UNSPECIFIED.)
CURVE()
GEOMETRIC_REPRESENTATION_ITEM()
RATIONAL_B_SPLINE_CURVE((1.00001075106213,1.00001338482769,1.))
REPRESENTATION_ITEM('')
);
#19226=(
BOUNDED_CURVE()
B_SPLINE_CURVE(2,(#77908,#77909,#77910),.UNSPECIFIED.,.F.,.F.)
B_SPLINE_CURVE_WITH_KNOTS((3,3),(0.,0.0424100233711627),.UNSPECIFIED.)
CURVE()
GEOMETRIC_REPRESENTATION_ITEM()
RATIONAL_B_SPLINE_CURVE((1.,1.00001338461061,1.00001075088763))
REPRESENTATION_ITEM('')
);
#19227=(
BOUNDED_CURVE()
B_SPLINE_CURVE(2,(#77912,#77913,#77914),.UNSPECIFIED.,.F.,.F.)
B_SPLINE_CURVE_WITH_KNOTS((3,3),(0.339146964126523,0.668418076018308),
 .UNSPECIFIED.)
CURVE()
GEOMETRIC_REPRESENTATION_ITEM()
RATIONAL_B_SPLINE_CURVE((1.00400190544534,1.00495889669787,1.00400190544534))
REPRESENTATION_ITEM('')
);
#19228=(
BOUNDED_CURVE()
B_SPLINE_CURVE(2,(#77916,#77917,#77918),.UNSPECIFIED.,.F.,.F.)
B_SPLINE_CURVE_WITH_KNOTS((3,3),(0.0284639720394568,0.0708739951602894),
 .UNSPECIFIED.)
CURVE()
GEOMETRIC_REPRESENTATION_ITEM()
RATIONAL_B_SPLINE_CURVE((1.00001075151129,1.00001338538694,1.))
REPRESENTATION_ITEM('')
);
#19229=(
BOUNDED_CURVE()
B_SPLINE_CURVE(2,(#77922,#77923,#77924),.UNSPECIFIED.,.F.,.F.)
B_SPLINE_CURVE_WITH_KNOTS((3,3),(0.,0.042410023028666),.UNSPECIFIED.)
CURVE()
GEOMETRIC_REPRESENTATION_ITEM()
RATIONAL_B_SPLINE_CURVE((1.,1.00001338527187,1.0000107514189))
REPRESENTATION_ITEM('')
);
#19230=(
BOUNDED_CURVE()
B_SPLINE_CURVE(2,(#77926,#77927,#77928),.UNSPECIFIED.,.F.,.F.)
B_SPLINE_CURVE_WITH_KNOTS((3,3),(0.339146964126521,0.668418076018309),
 .UNSPECIFIED.)
CURVE()
GEOMETRIC_REPRESENTATION_ITEM()
RATIONAL_B_SPLINE_CURVE((1.00400190544534,1.00495889669788,1.00400190544534))
REPRESENTATION_ITEM('')
);
#19231=(
BOUNDED_CURVE()
B_SPLINE_CURVE(2,(#77930,#77931,#77932),.UNSPECIFIED.,.F.,.F.)
B_SPLINE_CURVE_WITH_KNOTS((3,3),(0.0284639713944435,0.0708739951602898),
 .UNSPECIFIED.)
CURVE()
GEOMETRIC_REPRESENTATION_ITEM()
RATIONAL_B_SPLINE_CURVE((1.00001075185111,1.00001338581031,1.))
REPRESENTATION_ITEM('')
);
#19232=(
BOUNDED_CURVE()
B_SPLINE_CURVE(2,(#77936,#77937,#77938),.UNSPECIFIED.,.F.,.F.)
B_SPLINE_CURVE_WITH_KNOTS((3,3),(0.,0.0424100230585016),.UNSPECIFIED.)
CURVE()
GEOMETRIC_REPRESENTATION_ITEM()
RATIONAL_B_SPLINE_CURVE((1.,1.00001338563914,1.00001075171389))
REPRESENTATION_ITEM('')
);
#19233=(
BOUNDED_CURVE()
B_SPLINE_CURVE(2,(#77940,#77941,#77942),.UNSPECIFIED.,.F.,.F.)
B_SPLINE_CURVE_WITH_KNOTS((3,3),(0.339146964126512,0.668418076018301),
 .UNSPECIFIED.)
CURVE()
GEOMETRIC_REPRESENTATION_ITEM()
RATIONAL_B_SPLINE_CURVE((1.00400190544535,1.00495889669789,1.00400190544535))
REPRESENTATION_ITEM('')
);
#19234=(
BOUNDED_CURVE()
B_SPLINE_CURVE(2,(#77944,#77945,#77946),.UNSPECIFIED.,.F.,.F.)
B_SPLINE_CURVE_WITH_KNOTS((3,3),(0.0284639714315111,0.0708739951602896),
 .UNSPECIFIED.)
CURVE()
GEOMETRIC_REPRESENTATION_ITEM()
RATIONAL_B_SPLINE_CURVE((1.00001075192806,1.00001338590609,1.))
REPRESENTATION_ITEM('')
);
#19235=(
BOUNDED_CURVE()
B_SPLINE_CURVE(2,(#77950,#77951,#77952),.UNSPECIFIED.,.F.,.F.)
B_SPLINE_CURVE_WITH_KNOTS((3,3),(0.,0.0424100231762053),.UNSPECIFIED.)
CURVE()
GEOMETRIC_REPRESENTATION_ITEM()
RATIONAL_B_SPLINE_CURVE((1.,1.00001338544772,1.00001075156009))
REPRESENTATION_ITEM('')
);
#19236=(
BOUNDED_CURVE()
B_SPLINE_CURVE(2,(#77954,#77955,#77956),.UNSPECIFIED.,.F.,.F.)
B_SPLINE_CURVE_WITH_KNOTS((3,3),(0.339146964126514,0.668418076018301),
 .UNSPECIFIED.)
CURVE()
GEOMETRIC_REPRESENTATION_ITEM()
RATIONAL_B_SPLINE_CURVE((1.00400190544534,1.00495889669788,1.00400190544534))
REPRESENTATION_ITEM('')
);
#19237=(
BOUNDED_CURVE()
B_SPLINE_CURVE(2,(#77957,#77958,#77959),.UNSPECIFIED.,.F.,.F.)
B_SPLINE_CURVE_WITH_KNOTS((3,3),(0.0284639718065639,0.070873995160289),
 .UNSPECIFIED.)
CURVE()
GEOMETRIC_REPRESENTATION_ITEM()
RATIONAL_B_SPLINE_CURVE((1.00001075095126,1.00001338468982,1.))
REPRESENTATION_ITEM('')
);
#19238=(
BOUNDED_CURVE()
B_SPLINE_CURVE(2,(#77968,#77969,#77970),.UNSPECIFIED.,.F.,.F.)
B_SPLINE_CURVE_WITH_KNOTS((3,3),(0.,0.0709397118056795),.UNSPECIFIED.)
CURVE()
GEOMETRIC_REPRESENTATION_ITEM()
RATIONAL_B_SPLINE_CURVE((1.,1.00002245218476,1.))
REPRESENTATION_ITEM('')
);
#19239=(
BOUNDED_CURVE()
B_SPLINE_CURVE(2,(#77973,#77974,#77975),.UNSPECIFIED.,.F.,.F.)
B_SPLINE_CURVE_WITH_KNOTS((3,3),(0.,0.0709397118056799),.UNSPECIFIED.)
CURVE()
GEOMETRIC_REPRESENTATION_ITEM()
RATIONAL_B_SPLINE_CURVE((1.,1.00002245184959,1.))
REPRESENTATION_ITEM('')
);
#19240=(
BOUNDED_CURVE()
B_SPLINE_CURVE(2,(#77985,#77986,#77987),.UNSPECIFIED.,.F.,.F.)
B_SPLINE_CURVE_WITH_KNOTS((3,3),(0.,0.0709397118056798),.UNSPECIFIED.)
CURVE()
GEOMETRIC_REPRESENTATION_ITEM()
RATIONAL_B_SPLINE_CURVE((1.,1.00002245136635,1.))
REPRESENTATION_ITEM('')
);
#19241=(
BOUNDED_CURVE()
B_SPLINE_CURVE(2,(#77991,#77992,#77993),.UNSPECIFIED.,.F.,.F.)
B_SPLINE_CURVE_WITH_KNOTS((3,3),(0.,0.0424100231686042),.UNSPECIFIED.)
CURVE()
GEOMETRIC_REPRESENTATION_ITEM()
RATIONAL_B_SPLINE_CURVE((1.,1.00001338527369,1.00001075142031))
REPRESENTATION_ITEM('')
);
#19242=(
BOUNDED_CURVE()
B_SPLINE_CURVE(2,(#77995,#77996,#77997),.UNSPECIFIED.,.F.,.F.)
B_SPLINE_CURVE_WITH_KNOTS((3,3),(0.339146964126513,0.668418076018301),
 .UNSPECIFIED.)
CURVE()
GEOMETRIC_REPRESENTATION_ITEM()
RATIONAL_B_SPLINE_CURVE((1.00400190544534,1.00495889669788,1.00400190544534))
REPRESENTATION_ITEM('')
);
#19243=(
BOUNDED_CURVE()
B_SPLINE_CURVE(2,(#77999,#78000,#78001),.UNSPECIFIED.,.F.,.F.)
B_SPLINE_CURVE_WITH_KNOTS((3,3),(0.0284639717703716,0.0708739951602899),
 .UNSPECIFIED.)
CURVE()
GEOMETRIC_REPRESENTATION_ITEM()
RATIONAL_B_SPLINE_CURVE((1.00001075056076,1.00001338420368,1.))
REPRESENTATION_ITEM('')
);
#19244=(
BOUNDED_CURVE()
B_SPLINE_CURVE(2,(#78005,#78006,#78007),.UNSPECIFIED.,.F.,.F.)
B_SPLINE_CURVE_WITH_KNOTS((3,3),(0.,0.0424100236434718),.UNSPECIFIED.)
CURVE()
GEOMETRIC_REPRESENTATION_ITEM()
RATIONAL_B_SPLINE_CURVE((1.,1.0000133842216,1.00001075057506))
REPRESENTATION_ITEM('')
);
#19245=(
BOUNDED_CURVE()
B_SPLINE_CURVE(2,(#78009,#78010,#78011),.UNSPECIFIED.,.F.,.F.)
B_SPLINE_CURVE_WITH_KNOTS((3,3),(0.339146964126518,0.668418076018304),
 .UNSPECIFIED.)
CURVE()
GEOMETRIC_REPRESENTATION_ITEM()
RATIONAL_B_SPLINE_CURVE((1.00400190544534,1.00495889669787,1.00400190544534))
REPRESENTATION_ITEM('')
);
#19246=(
BOUNDED_CURVE()
B_SPLINE_CURVE(2,(#78013,#78014,#78015),.UNSPECIFIED.,.F.,.F.)
B_SPLINE_CURVE_WITH_KNOTS((3,3),(0.0284639718440856,0.0708739951602902),
 .UNSPECIFIED.)
CURVE()
GEOMETRIC_REPRESENTATION_ITEM()
RATIONAL_B_SPLINE_CURVE((1.00001075101626,1.00001338477073,1.))
REPRESENTATION_ITEM('')
);
#19247=(
BOUNDED_CURVE()
B_SPLINE_CURVE(2,(#78019,#78020,#78021),.UNSPECIFIED.,.F.,.F.)
B_SPLINE_CURVE_WITH_KNOTS((3,3),(0.,0.0424100231103199),.UNSPECIFIED.)
CURVE()
GEOMETRIC_REPRESENTATION_ITEM()
RATIONAL_B_SPLINE_CURVE((1.,1.00001338475467,1.00001075100344))
REPRESENTATION_ITEM('')
);
#19248=(
BOUNDED_CURVE()
B_SPLINE_CURVE(2,(#78023,#78024,#78025),.UNSPECIFIED.,.F.,.F.)
B_SPLINE_CURVE_WITH_KNOTS((3,3),(0.339146964126514,0.668418076018306),
 .UNSPECIFIED.)
CURVE()
GEOMETRIC_REPRESENTATION_ITEM()
RATIONAL_B_SPLINE_CURVE((1.00400190544536,1.0049588966979,1.00400190544536))
REPRESENTATION_ITEM('')
);
#19249=(
BOUNDED_CURVE()
B_SPLINE_CURVE(2,(#78027,#78028,#78029),.UNSPECIFIED.,.F.,.F.)
B_SPLINE_CURVE_WITH_KNOTS((3,3),(0.0284639723140838,0.0708739951602902),
 .UNSPECIFIED.)
CURVE()
GEOMETRIC_REPRESENTATION_ITEM()
RATIONAL_B_SPLINE_CURVE((1.00001075055174,1.00001338419219,1.))
REPRESENTATION_ITEM('')
);
#19250=(
BOUNDED_CURVE()
B_SPLINE_CURVE(2,(#78033,#78034,#78035),.UNSPECIFIED.,.F.,.F.)
B_SPLINE_CURVE_WITH_KNOTS((3,3),(0.,0.0424100235660184),.UNSPECIFIED.)
CURVE()
GEOMETRIC_REPRESENTATION_ITEM()
RATIONAL_B_SPLINE_CURVE((1.,1.0000133839457,1.00001075035348))
REPRESENTATION_ITEM('')
);
#19251=(
BOUNDED_CURVE()
B_SPLINE_CURVE(2,(#78037,#78038,#78039),.UNSPECIFIED.,.F.,.F.)
B_SPLINE_CURVE_WITH_KNOTS((3,3),(0.339146964126508,0.668418076018301),
 .UNSPECIFIED.)
CURVE()
GEOMETRIC_REPRESENTATION_ITEM()
RATIONAL_B_SPLINE_CURVE((1.00400190544536,1.0049588966979,1.00400190544536))
REPRESENTATION_ITEM('')
);
#19252=(
BOUNDED_CURVE()
B_SPLINE_CURVE(2,(#78041,#78042,#78043),.UNSPECIFIED.,.F.,.F.)
B_SPLINE_CURVE_WITH_KNOTS((3,3),(0.0284639720583302,0.0708739951602905),
 .UNSPECIFIED.)
CURVE()
GEOMETRIC_REPRESENTATION_ITEM()
RATIONAL_B_SPLINE_CURVE((1.00001075112448,1.00001338490536,1.))
REPRESENTATION_ITEM('')
);
#19253=(
BOUNDED_CURVE()
B_SPLINE_CURVE(2,(#78047,#78048,#78049),.UNSPECIFIED.,.F.,.F.)
B_SPLINE_CURVE_WITH_KNOTS((3,3),(0.,0.0424100220617497),.UNSPECIFIED.)
CURVE()
GEOMETRIC_REPRESENTATION_ITEM()
RATIONAL_B_SPLINE_CURVE((1.,1.00001338539763,1.00001075152027))
REPRESENTATION_ITEM('')
);
#19254=(
BOUNDED_CURVE()
B_SPLINE_CURVE(2,(#78051,#78052,#78053),.UNSPECIFIED.,.F.,.F.)
B_SPLINE_CURVE_WITH_KNOTS((3,3),(0.339146964126514,0.668418076018307),
 .UNSPECIFIED.)
CURVE()
GEOMETRIC_REPRESENTATION_ITEM()
RATIONAL_B_SPLINE_CURVE((1.00400190544536,1.0049588966979,1.00400190544536))
REPRESENTATION_ITEM('')
);
#19255=(
BOUNDED_CURVE()
B_SPLINE_CURVE(2,(#78055,#78056,#78057),.UNSPECIFIED.,.F.,.F.)
B_SPLINE_CURVE_WITH_KNOTS((3,3),(0.0284639715520864,0.07087399516029),
 .UNSPECIFIED.)
CURVE()
GEOMETRIC_REPRESENTATION_ITEM()
RATIONAL_B_SPLINE_CURVE((1.00001075068925,1.00001338436375,1.))
REPRESENTATION_ITEM('')
);
#19256=(
BOUNDED_CURVE()
B_SPLINE_CURVE(2,(#78061,#78062,#78063),.UNSPECIFIED.,.F.,.F.)
B_SPLINE_CURVE_WITH_KNOTS((3,3),(0.,0.04241002248244),.UNSPECIFIED.)
CURVE()
GEOMETRIC_REPRESENTATION_ITEM()
RATIONAL_B_SPLINE_CURVE((1.,1.00001338499034,1.00001075119297))
REPRESENTATION_ITEM('')
);
#19257=(
BOUNDED_CURVE()
B_SPLINE_CURVE(2,(#78065,#78066,#78067),.UNSPECIFIED.,.F.,.F.)
B_SPLINE_CURVE_WITH_KNOTS((3,3),(0.339146964126512,0.668418076018301),
 .UNSPECIFIED.)
CURVE()
GEOMETRIC_REPRESENTATION_ITEM()
RATIONAL_B_SPLINE_CURVE((1.00400190544534,1.00495889669788,1.00400190544534))
REPRESENTATION_ITEM('')
);
#19258=(
BOUNDED_CURVE()
B_SPLINE_CURVE(2,(#78069,#78070,#78071),.UNSPECIFIED.,.F.,.F.)
B_SPLINE_CURVE_WITH_KNOTS((3,3),(0.0284639721565262,0.0708739951602904),
 .UNSPECIFIED.)
CURVE()
GEOMETRIC_REPRESENTATION_ITEM()
RATIONAL_B_SPLINE_CURVE((1.0000107506802,1.00001338435219,1.))
REPRESENTATION_ITEM('')
);
#19259=(
BOUNDED_CURVE()
B_SPLINE_CURVE(2,(#78075,#78076,#78077),.UNSPECIFIED.,.F.,.F.)
B_SPLINE_CURVE_WITH_KNOTS((3,3),(0.,0.0424100240923756),.UNSPECIFIED.)
CURVE()
GEOMETRIC_REPRESENTATION_ITEM()
RATIONAL_B_SPLINE_CURVE((1.,1.0000133837799,1.00001075022011))
REPRESENTATION_ITEM('')
);
#19260=(
BOUNDED_CURVE()
B_SPLINE_CURVE(2,(#78079,#78080,#78081),.UNSPECIFIED.,.F.,.F.)
B_SPLINE_CURVE_WITH_KNOTS((3,3),(0.339146964126516,0.668418076018305),
 .UNSPECIFIED.)
CURVE()
GEOMETRIC_REPRESENTATION_ITEM()
RATIONAL_B_SPLINE_CURVE((1.00400190544534,1.00495889669788,1.00400190544534))
REPRESENTATION_ITEM('')
);
#19261=(
BOUNDED_CURVE()
B_SPLINE_CURVE(2,(#78083,#78084,#78085),.UNSPECIFIED.,.F.,.F.)
B_SPLINE_CURVE_WITH_KNOTS((3,3),(0.028463971978143,0.0708739951602902),
 .UNSPECIFIED.)
CURVE()
GEOMETRIC_REPRESENTATION_ITEM()
RATIONAL_B_SPLINE_CURVE((1.00001075215987,1.00001338619444,1.))
REPRESENTATION_ITEM('')
);
#19262=(
BOUNDED_CURVE()
B_SPLINE_CURVE(2,(#78089,#78090,#78091),.UNSPECIFIED.,.F.,.F.)
B_SPLINE_CURVE_WITH_KNOTS((3,3),(0.,0.0424100230241919),.UNSPECIFIED.)
CURVE()
GEOMETRIC_REPRESENTATION_ITEM()
RATIONAL_B_SPLINE_CURVE((1.,1.00001338577696,1.0000107518246))
REPRESENTATION_ITEM('')
);
#19263=(
BOUNDED_CURVE()
B_SPLINE_CURVE(2,(#78093,#78094,#78095),.UNSPECIFIED.,.F.,.F.)
B_SPLINE_CURVE_WITH_KNOTS((3,3),(0.339146964126515,0.668418076018303),
 .UNSPECIFIED.)
CURVE()
GEOMETRIC_REPRESENTATION_ITEM()
RATIONAL_B_SPLINE_CURVE((1.00400190544534,1.00495889669788,1.00400190544534))
REPRESENTATION_ITEM('')
);
#19264=(
BOUNDED_CURVE()
B_SPLINE_CURVE(2,(#78097,#78098,#78099),.UNSPECIFIED.,.F.,.F.)
B_SPLINE_CURVE_WITH_KNOTS((3,3),(0.0284639714085394,0.0708739951602901),
 .UNSPECIFIED.)
CURVE()
GEOMETRIC_REPRESENTATION_ITEM()
RATIONAL_B_SPLINE_CURVE((1.00001075029138,1.00001338386847,1.))
REPRESENTATION_ITEM('')
);
#19265=(
BOUNDED_CURVE()
B_SPLINE_CURVE(2,(#78103,#78104,#78105),.UNSPECIFIED.,.F.,.F.)
B_SPLINE_CURVE_WITH_KNOTS((3,3),(0.,0.0424100237528121),.UNSPECIFIED.)
CURVE()
GEOMETRIC_REPRESENTATION_ITEM()
RATIONAL_B_SPLINE_CURVE((1.,1.00001338452937,1.00001075082223))
REPRESENTATION_ITEM('')
);
#19266=(
BOUNDED_CURVE()
B_SPLINE_CURVE(2,(#78107,#78108,#78109),.UNSPECIFIED.,.F.,.F.)
B_SPLINE_CURVE_WITH_KNOTS((3,3),(0.33914696412652,0.668418076018306),
 .UNSPECIFIED.)
CURVE()
GEOMETRIC_REPRESENTATION_ITEM()
RATIONAL_B_SPLINE_CURVE((1.00400190544534,1.00495889669787,1.00400190544534))
REPRESENTATION_ITEM('')
);
#19267=(
BOUNDED_CURVE()
B_SPLINE_CURVE(2,(#78111,#78112,#78113),.UNSPECIFIED.,.F.,.F.)
B_SPLINE_CURVE_WITH_KNOTS((3,3),(0.0284639714357814,0.0708739951602905),
 .UNSPECIFIED.)
CURVE()
GEOMETRIC_REPRESENTATION_ITEM()
RATIONAL_B_SPLINE_CURVE((1.00001075147797,1.00001338534574,1.))
REPRESENTATION_ITEM('')
);
#19268=(
BOUNDED_CURVE()
B_SPLINE_CURVE(2,(#78117,#78118,#78119),.UNSPECIFIED.,.F.,.F.)
B_SPLINE_CURVE_WITH_KNOTS((3,3),(0.,0.0424100231755104),.UNSPECIFIED.)
CURVE()
GEOMETRIC_REPRESENTATION_ITEM()
RATIONAL_B_SPLINE_CURVE((1.,1.0000133853411,1.00001075147445))
REPRESENTATION_ITEM('')
);
#19269=(
BOUNDED_CURVE()
B_SPLINE_CURVE(2,(#78121,#78122,#78123),.UNSPECIFIED.,.F.,.F.)
B_SPLINE_CURVE_WITH_KNOTS((3,3),(0.339146964126517,0.668418076018305),
 .UNSPECIFIED.)
CURVE()
GEOMETRIC_REPRESENTATION_ITEM()
RATIONAL_B_SPLINE_CURVE((1.00400190544534,1.00495889669788,1.00400190544534))
REPRESENTATION_ITEM('')
);
#19270=(
BOUNDED_CURVE()
B_SPLINE_CURVE(2,(#78125,#78126,#78127),.UNSPECIFIED.,.F.,.F.)
B_SPLINE_CURVE_WITH_KNOTS((3,3),(0.0284639717634429,0.0708739951602899),
 .UNSPECIFIED.)
CURVE()
GEOMETRIC_REPRESENTATION_ITEM()
RATIONAL_B_SPLINE_CURVE((1.00001075157258,1.00001338546337,1.))
REPRESENTATION_ITEM('')
);
#19271=(
BOUNDED_CURVE()
B_SPLINE_CURVE(2,(#78131,#78132,#78133),.UNSPECIFIED.,.F.,.F.)
B_SPLINE_CURVE_WITH_KNOTS((3,3),(0.,0.0424100230054134),.UNSPECIFIED.)
CURVE()
GEOMETRIC_REPRESENTATION_ITEM()
RATIONAL_B_SPLINE_CURVE((1.,1.00001338465159,1.00001075092068))
REPRESENTATION_ITEM('')
);
#19272=(
BOUNDED_CURVE()
B_SPLINE_CURVE(2,(#78135,#78136,#78137),.UNSPECIFIED.,.F.,.F.)
B_SPLINE_CURVE_WITH_KNOTS((3,3),(0.339146964126518,0.668418076018304),
 .UNSPECIFIED.)
CURVE()
GEOMETRIC_REPRESENTATION_ITEM()
RATIONAL_B_SPLINE_CURVE((1.00400190544534,1.00495889669787,1.00400190544534))
REPRESENTATION_ITEM('')
);
#19273=(
BOUNDED_CURVE()
B_SPLINE_CURVE(2,(#78139,#78140,#78141),.UNSPECIFIED.,.F.,.F.)
B_SPLINE_CURVE_WITH_KNOTS((3,3),(0.0284639725451214,0.0708739951602902),
 .UNSPECIFIED.)
CURVE()
GEOMETRIC_REPRESENTATION_ITEM()
RATIONAL_B_SPLINE_CURVE((1.00001075152758,1.00001338540698,1.))
REPRESENTATION_ITEM('')
);
#19274=(
BOUNDED_CURVE()
B_SPLINE_CURVE(2,(#78145,#78146,#78147),.UNSPECIFIED.,.F.,.F.)
B_SPLINE_CURVE_WITH_KNOTS((3,3),(0.,0.042410022661541),.UNSPECIFIED.)
CURVE()
GEOMETRIC_REPRESENTATION_ITEM()
RATIONAL_B_SPLINE_CURVE((1.,1.00001338471694,1.0000107509733))
REPRESENTATION_ITEM('')
);
#19275=(
BOUNDED_CURVE()
B_SPLINE_CURVE(2,(#78149,#78150,#78151),.UNSPECIFIED.,.F.,.F.)
B_SPLINE_CURVE_WITH_KNOTS((3,3),(0.339146964126513,0.668418076018301),
 .UNSPECIFIED.)
CURVE()
GEOMETRIC_REPRESENTATION_ITEM()
RATIONAL_B_SPLINE_CURVE((1.00400190544534,1.00495889669788,1.00400190544534))
REPRESENTATION_ITEM('')
);
#19276=(
BOUNDED_CURVE()
B_SPLINE_CURVE(2,(#78153,#78154,#78155),.UNSPECIFIED.,.F.,.F.)
B_SPLINE_CURVE_WITH_KNOTS((3,3),(0.0284639712817304,0.0708739951602903),
 .UNSPECIFIED.)
CURVE()
GEOMETRIC_REPRESENTATION_ITEM()
RATIONAL_B_SPLINE_CURVE((1.00001075092078,1.00001338465212,1.))
REPRESENTATION_ITEM('')
);
#19277=(
BOUNDED_CURVE()
B_SPLINE_CURVE(2,(#78159,#78160,#78161),.UNSPECIFIED.,.F.,.F.)
B_SPLINE_CURVE_WITH_KNOTS((3,3),(0.,0.0424100230249418),.UNSPECIFIED.)
CURVE()
GEOMETRIC_REPRESENTATION_ITEM()
RATIONAL_B_SPLINE_CURVE((1.,1.00001338592286,1.0000107519418))
REPRESENTATION_ITEM('')
);
#19278=(
BOUNDED_CURVE()
B_SPLINE_CURVE(2,(#78163,#78164,#78165),.UNSPECIFIED.,.F.,.F.)
B_SPLINE_CURVE_WITH_KNOTS((3,3),(0.339146964126504,0.668418076018296),
 .UNSPECIFIED.)
CURVE()
GEOMETRIC_REPRESENTATION_ITEM()
RATIONAL_B_SPLINE_CURVE((1.00400190544536,1.0049588966979,1.00400190544536))
REPRESENTATION_ITEM('')
);
#19279=(
BOUNDED_CURVE()
B_SPLINE_CURVE(2,(#78167,#78168,#78169),.UNSPECIFIED.,.F.,.F.)
B_SPLINE_CURVE_WITH_KNOTS((3,3),(0.0284639714045715,0.0708739951602901),
 .UNSPECIFIED.)
CURVE()
GEOMETRIC_REPRESENTATION_ITEM()
RATIONAL_B_SPLINE_CURVE((1.00001075086984,1.00001338458864,1.))
REPRESENTATION_ITEM('')
);
#19280=(
BOUNDED_CURVE()
B_SPLINE_CURVE(2,(#78173,#78174,#78175),.UNSPECIFIED.,.F.,.F.)
B_SPLINE_CURVE_WITH_KNOTS((3,3),(0.,0.042410023759092),.UNSPECIFIED.)
CURVE()
GEOMETRIC_REPRESENTATION_ITEM()
RATIONAL_B_SPLINE_CURVE((1.,1.00001338518135,1.00001075134592))
REPRESENTATION_ITEM('')
);
#19281=(
BOUNDED_CURVE()
B_SPLINE_CURVE(2,(#78177,#78178,#78179),.UNSPECIFIED.,.F.,.F.)
B_SPLINE_CURVE_WITH_KNOTS((3,3),(0.339146964126521,0.668418076018308),
 .UNSPECIFIED.)
CURVE()
GEOMETRIC_REPRESENTATION_ITEM()
RATIONAL_B_SPLINE_CURVE((1.00400190544534,1.00495889669787,1.00400190544534))
REPRESENTATION_ITEM('')
);
#19282=(
BOUNDED_CURVE()
B_SPLINE_CURVE(2,(#78181,#78182,#78183),.UNSPECIFIED.,.F.,.F.)
B_SPLINE_CURVE_WITH_KNOTS((3,3),(0.0284639721328031,0.0708739951602905),
 .UNSPECIFIED.)
CURVE()
GEOMETRIC_REPRESENTATION_ITEM()
RATIONAL_B_SPLINE_CURVE((1.00001075159191,1.00001338548726,1.))
REPRESENTATION_ITEM('')
);
#19283=(
BOUNDED_CURVE()
B_SPLINE_CURVE(2,(#78187,#78188,#78189),.UNSPECIFIED.,.F.,.F.)
B_SPLINE_CURVE_WITH_KNOTS((3,3),(0.,0.0424100231470919),.UNSPECIFIED.)
CURVE()
GEOMETRIC_REPRESENTATION_ITEM()
RATIONAL_B_SPLINE_CURVE((1.,1.00001338447535,1.00001075077907))
REPRESENTATION_ITEM('')
);
#19284=(
BOUNDED_CURVE()
B_SPLINE_CURVE(2,(#78191,#78192,#78193),.UNSPECIFIED.,.F.,.F.)
B_SPLINE_CURVE_WITH_KNOTS((3,3),(0.339146964126509,0.668418076018305),
 .UNSPECIFIED.)
CURVE()
GEOMETRIC_REPRESENTATION_ITEM()
RATIONAL_B_SPLINE_CURVE((1.00400190544537,1.00495889669791,1.00400190544537))
REPRESENTATION_ITEM('')
);
#19285=(
BOUNDED_CURVE()
B_SPLINE_CURVE(2,(#78195,#78196,#78197),.UNSPECIFIED.,.F.,.F.)
B_SPLINE_CURVE_WITH_KNOTS((3,3),(0.0284639710994826,0.0708739951602903),
 .UNSPECIFIED.)
CURVE()
GEOMETRIC_REPRESENTATION_ITEM()
RATIONAL_B_SPLINE_CURVE((1.00001075063279,1.00001338429367,1.))
REPRESENTATION_ITEM('')
);
#19286=(
BOUNDED_CURVE()
B_SPLINE_CURVE(2,(#78201,#78202,#78203),.UNSPECIFIED.,.F.,.F.)
B_SPLINE_CURVE_WITH_KNOTS((3,3),(0.,0.0424100229366385),.UNSPECIFIED.)
CURVE()
GEOMETRIC_REPRESENTATION_ITEM()
RATIONAL_B_SPLINE_CURVE((1.,1.00001338458235,1.00001075086509))
REPRESENTATION_ITEM('')
);
#19287=(
BOUNDED_CURVE()
B_SPLINE_CURVE(2,(#78205,#78206,#78207),.UNSPECIFIED.,.F.,.F.)
B_SPLINE_CURVE_WITH_KNOTS((3,3),(0.339146964126511,0.668418076018304),
 .UNSPECIFIED.)
CURVE()
GEOMETRIC_REPRESENTATION_ITEM()
RATIONAL_B_SPLINE_CURVE((1.00400190544536,1.0049588966979,1.00400190544536))
REPRESENTATION_ITEM('')
);
#19288=(
BOUNDED_CURVE()
B_SPLINE_CURVE(2,(#78209,#78210,#78211),.UNSPECIFIED.,.F.,.F.)
B_SPLINE_CURVE_WITH_KNOTS((3,3),(0.0284639718437778,0.0708739951602902),
 .UNSPECIFIED.)
CURVE()
GEOMETRIC_REPRESENTATION_ITEM()
RATIONAL_B_SPLINE_CURVE((1.00001075112877,1.00001338491081,1.))
REPRESENTATION_ITEM('')
);
#19289=(
BOUNDED_CURVE()
B_SPLINE_CURVE(2,(#78215,#78216,#78217),.UNSPECIFIED.,.F.,.F.)
B_SPLINE_CURVE_WITH_KNOTS((3,3),(0.,0.0424100231273197),.UNSPECIFIED.)
CURVE()
GEOMETRIC_REPRESENTATION_ITEM()
RATIONAL_B_SPLINE_CURVE((1.,1.00001338514488,1.00001075131686))
REPRESENTATION_ITEM('')
);
#19290=(
BOUNDED_CURVE()
B_SPLINE_CURVE(2,(#78219,#78220,#78221),.UNSPECIFIED.,.F.,.F.)
B_SPLINE_CURVE_WITH_KNOTS((3,3),(0.339146964126517,0.668418076018305),
 .UNSPECIFIED.)
CURVE()
GEOMETRIC_REPRESENTATION_ITEM()
RATIONAL_B_SPLINE_CURVE((1.00400190544534,1.00495889669788,1.00400190544534))
REPRESENTATION_ITEM('')
);
#19291=(
BOUNDED_CURVE()
B_SPLINE_CURVE(2,(#78223,#78224,#78225),.UNSPECIFIED.,.F.,.F.)
B_SPLINE_CURVE_WITH_KNOTS((3,3),(0.028463971590667,0.0708739951602901),
 .UNSPECIFIED.)
CURVE()
GEOMETRIC_REPRESENTATION_ITEM()
RATIONAL_B_SPLINE_CURVE((1.00001075154508,1.00001338542922,1.))
REPRESENTATION_ITEM('')
);
#19292=(
BOUNDED_CURVE()
B_SPLINE_CURVE(2,(#78229,#78230,#78231),.UNSPECIFIED.,.F.,.F.)
B_SPLINE_CURVE_WITH_KNOTS((3,3),(0.,0.042410023865277),.UNSPECIFIED.)
CURVE()
GEOMETRIC_REPRESENTATION_ITEM()
RATIONAL_B_SPLINE_CURVE((1.,1.00001338530686,1.00001075144669))
REPRESENTATION_ITEM('')
);
#19293=(
BOUNDED_CURVE()
B_SPLINE_CURVE(2,(#78233,#78234,#78235),.UNSPECIFIED.,.F.,.F.)
B_SPLINE_CURVE_WITH_KNOTS((3,3),(0.339146964126508,0.668418076018304),
 .UNSPECIFIED.)
CURVE()
GEOMETRIC_REPRESENTATION_ITEM()
RATIONAL_B_SPLINE_CURVE((1.00400190544537,1.00495889669791,1.00400190544537))
REPRESENTATION_ITEM('')
);
#19294=(
BOUNDED_CURVE()
B_SPLINE_CURVE(2,(#78237,#78238,#78239),.UNSPECIFIED.,.F.,.F.)
B_SPLINE_CURVE_WITH_KNOTS((3,3),(0.0284639715344571,0.0708739951602902),
 .UNSPECIFIED.)
CURVE()
GEOMETRIC_REPRESENTATION_ITEM()
RATIONAL_B_SPLINE_CURVE((1.0000107510557,1.00001338481998,1.))
REPRESENTATION_ITEM('')
);
#19295=(
BOUNDED_CURVE()
B_SPLINE_CURVE(2,(#78243,#78244,#78245),.UNSPECIFIED.,.F.,.F.)
B_SPLINE_CURVE_WITH_KNOTS((3,3),(0.,0.0424100228518102),.UNSPECIFIED.)
CURVE()
GEOMETRIC_REPRESENTATION_ITEM()
RATIONAL_B_SPLINE_CURVE((1.,1.00001338581925,1.00001075185864))
REPRESENTATION_ITEM('')
);
#19296=(
BOUNDED_CURVE()
B_SPLINE_CURVE(2,(#78247,#78248,#78249),.UNSPECIFIED.,.F.,.F.)
B_SPLINE_CURVE_WITH_KNOTS((3,3),(0.339146964126521,0.668418076018307),
 .UNSPECIFIED.)
CURVE()
GEOMETRIC_REPRESENTATION_ITEM()
RATIONAL_B_SPLINE_CURVE((1.00400190544534,1.00495889669787,1.00400190544534))
REPRESENTATION_ITEM('')
);
#19297=(
BOUNDED_CURVE()
B_SPLINE_CURVE(2,(#78251,#78252,#78253),.UNSPECIFIED.,.F.,.F.)
B_SPLINE_CURVE_WITH_KNOTS((3,3),(0.0284639711204301,0.0708739951602906),
 .UNSPECIFIED.)
CURVE()
GEOMETRIC_REPRESENTATION_ITEM()
RATIONAL_B_SPLINE_CURVE((1.00001075034871,1.00001338393999,1.))
REPRESENTATION_ITEM('')
);
#19298=(
BOUNDED_CURVE()
B_SPLINE_CURVE(2,(#78257,#78258,#78259),.UNSPECIFIED.,.F.,.F.)
B_SPLINE_CURVE_WITH_KNOTS((3,3),(0.,0.0424100240197507),.UNSPECIFIED.)
CURVE()
GEOMETRIC_REPRESENTATION_ITEM()
RATIONAL_B_SPLINE_CURVE((1.,1.00001338509862,1.00001075127937))
REPRESENTATION_ITEM('')
);
#19299=(
BOUNDED_CURVE()
B_SPLINE_CURVE(2,(#78261,#78262,#78263),.UNSPECIFIED.,.F.,.F.)
B_SPLINE_CURVE_WITH_KNOTS((3,3),(0.339146964126524,0.668418076018308),
 .UNSPECIFIED.)
CURVE()
GEOMETRIC_REPRESENTATION_ITEM()
RATIONAL_B_SPLINE_CURVE((1.00400190544533,1.00495889669787,1.00400190544533))
REPRESENTATION_ITEM('')
);
#19300=(
BOUNDED_CURVE()
B_SPLINE_CURVE(2,(#78265,#78266,#78267),.UNSPECIFIED.,.F.,.F.)
B_SPLINE_CURVE_WITH_KNOTS((3,3),(0.0284639714437082,0.0708739951602905),
 .UNSPECIFIED.)
CURVE()
GEOMETRIC_REPRESENTATION_ITEM()
RATIONAL_B_SPLINE_CURVE((1.00001075074537,1.00001338443367,1.))
REPRESENTATION_ITEM('')
);
#19301=(
BOUNDED_CURVE()
B_SPLINE_CURVE(2,(#78271,#78272,#78273),.UNSPECIFIED.,.F.,.F.)
B_SPLINE_CURVE_WITH_KNOTS((3,3),(0.,0.0424100234119021),.UNSPECIFIED.)
CURVE()
GEOMETRIC_REPRESENTATION_ITEM()
RATIONAL_B_SPLINE_CURVE((1.,1.00001338567679,1.000010751744))
REPRESENTATION_ITEM('')
);
#19302=(
BOUNDED_CURVE()
B_SPLINE_CURVE(2,(#78275,#78276,#78277),.UNSPECIFIED.,.F.,.F.)
B_SPLINE_CURVE_WITH_KNOTS((3,3),(0.339146964126514,0.668418076018306),
 .UNSPECIFIED.)
CURVE()
GEOMETRIC_REPRESENTATION_ITEM()
RATIONAL_B_SPLINE_CURVE((1.00400190544536,1.0049588966979,1.00400190544536))
REPRESENTATION_ITEM('')
);
#19303=(
BOUNDED_CURVE()
B_SPLINE_CURVE(2,(#78279,#78280,#78281),.UNSPECIFIED.,.F.,.F.)
B_SPLINE_CURVE_WITH_KNOTS((3,3),(0.0284639720122614,0.0708739951602903),
 .UNSPECIFIED.)
CURVE()
GEOMETRIC_REPRESENTATION_ITEM()
RATIONAL_B_SPLINE_CURVE((1.00001075146677,1.00001338533152,1.))
REPRESENTATION_ITEM('')
);
#19304=(
BOUNDED_CURVE()
B_SPLINE_CURVE(2,(#78285,#78286,#78287),.UNSPECIFIED.,.F.,.F.)
B_SPLINE_CURVE_WITH_KNOTS((3,3),(0.,0.0424100244197339),.UNSPECIFIED.)
CURVE()
GEOMETRIC_REPRESENTATION_ITEM()
RATIONAL_B_SPLINE_CURVE((1.,1.00001338512157,1.00001075129765))
REPRESENTATION_ITEM('')
);
#19305=(
BOUNDED_CURVE()
B_SPLINE_CURVE(2,(#78289,#78290,#78291),.UNSPECIFIED.,.F.,.F.)
B_SPLINE_CURVE_WITH_KNOTS((3,3),(0.339146964126511,0.668418076018303),
 .UNSPECIFIED.)
CURVE()
GEOMETRIC_REPRESENTATION_ITEM()
RATIONAL_B_SPLINE_CURVE((1.00400190544536,1.0049588966979,1.00400190544536))
REPRESENTATION_ITEM('')
);
#19306=(
BOUNDED_CURVE()
B_SPLINE_CURVE(2,(#78293,#78294,#78295),.UNSPECIFIED.,.F.,.F.)
B_SPLINE_CURVE_WITH_KNOTS((3,3),(0.0284639714088168,0.0708739951602901),
 .UNSPECIFIED.)
CURVE()
GEOMETRIC_REPRESENTATION_ITEM()
RATIONAL_B_SPLINE_CURVE((1.00001075122115,1.00001338502601,1.))
REPRESENTATION_ITEM('')
);
#19307=(
BOUNDED_CURVE()
B_SPLINE_CURVE(2,(#78299,#78300,#78301),.UNSPECIFIED.,.F.,.F.)
B_SPLINE_CURVE_WITH_KNOTS((3,3),(0.,0.0709397118056798),.UNSPECIFIED.)
CURVE()
GEOMETRIC_REPRESENTATION_ITEM()
RATIONAL_B_SPLINE_CURVE((1.,1.0000224517311,1.))
REPRESENTATION_ITEM('')
);
#19308=(
BOUNDED_CURVE()
B_SPLINE_CURVE(2,(#78309,#78310,#78311),.UNSPECIFIED.,.F.,.F.)
B_SPLINE_CURVE_WITH_KNOTS((3,3),(0.,0.0424100231806302),.UNSPECIFIED.)
CURVE()
GEOMETRIC_REPRESENTATION_ITEM()
RATIONAL_B_SPLINE_CURVE((1.,1.00001338421203,1.00001075056755))
REPRESENTATION_ITEM('')
);
#19309=(
BOUNDED_CURVE()
B_SPLINE_CURVE(2,(#78313,#78314,#78315),.UNSPECIFIED.,.F.,.F.)
B_SPLINE_CURVE_WITH_KNOTS((3,3),(0.339146964126513,0.668418076018302),
 .UNSPECIFIED.)
CURVE()
GEOMETRIC_REPRESENTATION_ITEM()
RATIONAL_B_SPLINE_CURVE((1.00400190544535,1.00495889669789,1.00400190544535))
REPRESENTATION_ITEM('')
);
#19310=(
BOUNDED_CURVE()
B_SPLINE_CURVE(2,(#78317,#78318,#78319),.UNSPECIFIED.,.F.,.F.)
B_SPLINE_CURVE_WITH_KNOTS((3,3),(0.0284639714379858,0.0708739951602898),
 .UNSPECIFIED.)
CURVE()
GEOMETRIC_REPRESENTATION_ITEM()
RATIONAL_B_SPLINE_CURVE((1.00001075041393,1.00001338402103,1.))
REPRESENTATION_ITEM('')
);
#19311=(
BOUNDED_CURVE()
B_SPLINE_CURVE(2,(#78323,#78324,#78325),.UNSPECIFIED.,.F.,.F.)
B_SPLINE_CURVE_WITH_KNOTS((3,3),(0.,0.0424100233991719),.UNSPECIFIED.)
CURVE()
GEOMETRIC_REPRESENTATION_ITEM()
RATIONAL_B_SPLINE_CURVE((1.,1.00001338583662,1.00001075187238))
REPRESENTATION_ITEM('')
);
#19312=(
BOUNDED_CURVE()
B_SPLINE_CURVE(2,(#78327,#78328,#78329),.UNSPECIFIED.,.F.,.F.)
B_SPLINE_CURVE_WITH_KNOTS((3,3),(0.339146964126513,0.668418076018302),
 .UNSPECIFIED.)
CURVE()
GEOMETRIC_REPRESENTATION_ITEM()
RATIONAL_B_SPLINE_CURVE((1.00400190544535,1.00495889669789,1.00400190544535))
REPRESENTATION_ITEM('')
);
#19313=(
BOUNDED_CURVE()
B_SPLINE_CURVE(2,(#78331,#78332,#78333),.UNSPECIFIED.,.F.,.F.)
B_SPLINE_CURVE_WITH_KNOTS((3,3),(0.0284639720344373,0.0708739951602892),
 .UNSPECIFIED.)
CURVE()
GEOMETRIC_REPRESENTATION_ITEM()
RATIONAL_B_SPLINE_CURVE((1.00001075214126,1.00001338617124,1.))
REPRESENTATION_ITEM('')
);
#19314=(
BOUNDED_CURVE()
B_SPLINE_CURVE(2,(#78337,#78338,#78339),.UNSPECIFIED.,.F.,.F.)
B_SPLINE_CURVE_WITH_KNOTS((3,3),(0.,0.0424100237328626),.UNSPECIFIED.)
CURVE()
GEOMETRIC_REPRESENTATION_ITEM()
RATIONAL_B_SPLINE_CURVE((1.,1.00001338671567,1.00001075257833))
REPRESENTATION_ITEM('')
);
#19315=(
BOUNDED_CURVE()
B_SPLINE_CURVE(2,(#78341,#78342,#78343),.UNSPECIFIED.,.F.,.F.)
B_SPLINE_CURVE_WITH_KNOTS((3,3),(0.339146964126522,0.668418076018309),
 .UNSPECIFIED.)
CURVE()
GEOMETRIC_REPRESENTATION_ITEM()
RATIONAL_B_SPLINE_CURVE((1.00400190544534,1.00495889669788,1.00400190544534))
REPRESENTATION_ITEM('')
);
#19316=(
BOUNDED_CURVE()
B_SPLINE_CURVE(2,(#78345,#78346,#78347),.UNSPECIFIED.,.F.,.F.)
B_SPLINE_CURVE_WITH_KNOTS((3,3),(0.0284639721094118,0.0708739951602891),
 .UNSPECIFIED.)
CURVE()
GEOMETRIC_REPRESENTATION_ITEM()
RATIONAL_B_SPLINE_CURVE((1.00001075120572,1.00001338500648,1.))
REPRESENTATION_ITEM('')
);
#19317=(
BOUNDED_CURVE()
B_SPLINE_CURVE(2,(#78351,#78352,#78353),.UNSPECIFIED.,.F.,.F.)
B_SPLINE_CURVE_WITH_KNOTS((3,3),(0.,0.0424100230569424),.UNSPECIFIED.)
CURVE()
GEOMETRIC_REPRESENTATION_ITEM()
RATIONAL_B_SPLINE_CURVE((1.,1.00001338564898,1.00001075172179))
REPRESENTATION_ITEM('')
);
#19318=(
BOUNDED_CURVE()
B_SPLINE_CURVE(2,(#78355,#78356,#78357),.UNSPECIFIED.,.F.,.F.)
B_SPLINE_CURVE_WITH_KNOTS((3,3),(0.339146964126515,0.668418076018298),
 .UNSPECIFIED.)
CURVE()
GEOMETRIC_REPRESENTATION_ITEM()
RATIONAL_B_SPLINE_CURVE((1.00400190544533,1.00495889669786,1.00400190544533))
REPRESENTATION_ITEM('')
);
#19319=(
BOUNDED_CURVE()
B_SPLINE_CURVE(2,(#78359,#78360,#78361),.UNSPECIFIED.,.F.,.F.)
B_SPLINE_CURVE_WITH_KNOTS((3,3),(0.0284639721324363,0.0708739951602891),
 .UNSPECIFIED.)
CURVE()
GEOMETRIC_REPRESENTATION_ITEM()
RATIONAL_B_SPLINE_CURVE((1.00001075234275,1.00001338642205,1.))
REPRESENTATION_ITEM('')
);
#19320=(
BOUNDED_CURVE()
B_SPLINE_CURVE(2,(#78365,#78366,#78367),.UNSPECIFIED.,.F.,.F.)
B_SPLINE_CURVE_WITH_KNOTS((3,3),(0.,0.0424100231045523),.UNSPECIFIED.)
CURVE()
GEOMETRIC_REPRESENTATION_ITEM()
RATIONAL_B_SPLINE_CURVE((1.,1.00001338428089,1.00001075062289))
REPRESENTATION_ITEM('')
);
#19321=(
BOUNDED_CURVE()
B_SPLINE_CURVE(2,(#78369,#78370,#78371),.UNSPECIFIED.,.F.,.F.)
B_SPLINE_CURVE_WITH_KNOTS((3,3),(0.339146964126512,0.668418076018305),
 .UNSPECIFIED.)
CURVE()
GEOMETRIC_REPRESENTATION_ITEM()
RATIONAL_B_SPLINE_CURVE((1.00400190544536,1.0049588966979,1.00400190544536))
REPRESENTATION_ITEM('')
);
#19322=(
BOUNDED_CURVE()
B_SPLINE_CURVE(2,(#78373,#78374,#78375),.UNSPECIFIED.,.F.,.F.)
B_SPLINE_CURVE_WITH_KNOTS((3,3),(0.0284639718061504,0.0708739951602889),
 .UNSPECIFIED.)
CURVE()
GEOMETRIC_REPRESENTATION_ITEM()
RATIONAL_B_SPLINE_CURVE((1.0000107509097,1.00001338463808,1.))
REPRESENTATION_ITEM('')
);
#19323=(
BOUNDED_CURVE()
B_SPLINE_CURVE(2,(#78379,#78380,#78381),.UNSPECIFIED.,.F.,.F.)
B_SPLINE_CURVE_WITH_KNOTS((3,3),(0.,0.0424100237189079),.UNSPECIFIED.)
CURVE()
GEOMETRIC_REPRESENTATION_ITEM()
RATIONAL_B_SPLINE_CURVE((1.,1.00001338362396,1.00001075009499))
REPRESENTATION_ITEM('')
);
#19324=(
BOUNDED_CURVE()
B_SPLINE_CURVE(2,(#78383,#78384,#78385),.UNSPECIFIED.,.F.,.F.)
B_SPLINE_CURVE_WITH_KNOTS((3,3),(0.339146964126514,0.668418076018301),
 .UNSPECIFIED.)
CURVE()
GEOMETRIC_REPRESENTATION_ITEM()
RATIONAL_B_SPLINE_CURVE((1.00400190544534,1.00495889669788,1.00400190544534))
REPRESENTATION_ITEM('')
);
#19325=(
BOUNDED_CURVE()
B_SPLINE_CURVE(2,(#78387,#78388,#78389),.UNSPECIFIED.,.F.,.F.)
B_SPLINE_CURVE_WITH_KNOTS((3,3),(0.0284639710964825,0.0708739951602894),
 .UNSPECIFIED.)
CURVE()
GEOMETRIC_REPRESENTATION_ITEM()
RATIONAL_B_SPLINE_CURVE((1.00001075212803,1.00001338615521,1.))
REPRESENTATION_ITEM('')
);
#19326=(
BOUNDED_CURVE()
B_SPLINE_CURVE(2,(#78393,#78394,#78395),.UNSPECIFIED.,.F.,.F.)
B_SPLINE_CURVE_WITH_KNOTS((3,3),(0.,0.0424100233501915),.UNSPECIFIED.)
CURVE()
GEOMETRIC_REPRESENTATION_ITEM()
RATIONAL_B_SPLINE_CURVE((1.,1.00001338506266,1.00001075125073))
REPRESENTATION_ITEM('')
);
#19327=(
BOUNDED_CURVE()
B_SPLINE_CURVE(2,(#78397,#78398,#78399),.UNSPECIFIED.,.F.,.F.)
B_SPLINE_CURVE_WITH_KNOTS((3,3),(0.339146964126518,0.668418076018306),
 .UNSPECIFIED.)
CURVE()
GEOMETRIC_REPRESENTATION_ITEM()
RATIONAL_B_SPLINE_CURVE((1.00400190544534,1.00495889669788,1.00400190544534))
REPRESENTATION_ITEM('')
);
#19328=(
BOUNDED_CURVE()
B_SPLINE_CURVE(2,(#78401,#78402,#78403),.UNSPECIFIED.,.F.,.F.)
B_SPLINE_CURVE_WITH_KNOTS((3,3),(0.0284639717818257,0.0708739951602895),
 .UNSPECIFIED.)
CURVE()
GEOMETRIC_REPRESENTATION_ITEM()
RATIONAL_B_SPLINE_CURVE((1.00001075166044,1.00001338557275,1.))
REPRESENTATION_ITEM('')
);
#19329=(
BOUNDED_CURVE()
B_SPLINE_CURVE(2,(#78407,#78408,#78409),.UNSPECIFIED.,.F.,.F.)
B_SPLINE_CURVE_WITH_KNOTS((3,3),(0.,0.0424100231031821),.UNSPECIFIED.)
CURVE()
GEOMETRIC_REPRESENTATION_ITEM()
RATIONAL_B_SPLINE_CURVE((1.,1.00001338538099,1.00001075150652))
REPRESENTATION_ITEM('')
);
#19330=(
BOUNDED_CURVE()
B_SPLINE_CURVE(2,(#78411,#78412,#78413),.UNSPECIFIED.,.F.,.F.)
B_SPLINE_CURVE_WITH_KNOTS((3,3),(0.339146964126511,0.668418076018296),
 .UNSPECIFIED.)
CURVE()
GEOMETRIC_REPRESENTATION_ITEM()
RATIONAL_B_SPLINE_CURVE((1.00400190544533,1.00495889669787,1.00400190544533))
REPRESENTATION_ITEM('')
);
#19331=(
BOUNDED_CURVE()
B_SPLINE_CURVE(2,(#78415,#78416,#78417),.UNSPECIFIED.,.F.,.F.)
B_SPLINE_CURVE_WITH_KNOTS((3,3),(0.0284639708342344,0.0708739951602889),
 .UNSPECIFIED.)
CURVE()
GEOMETRIC_REPRESENTATION_ITEM()
RATIONAL_B_SPLINE_CURVE((1.00001075087742,1.00001338459835,1.))
REPRESENTATION_ITEM('')
);
#19332=(
BOUNDED_CURVE()
B_SPLINE_CURVE(2,(#78421,#78422,#78423),.UNSPECIFIED.,.F.,.F.)
B_SPLINE_CURVE_WITH_KNOTS((3,3),(0.,0.0424100228599136),.UNSPECIFIED.)
CURVE()
GEOMETRIC_REPRESENTATION_ITEM()
RATIONAL_B_SPLINE_CURVE((1.,1.00001338560217,1.00001075168427))
REPRESENTATION_ITEM('')
);
#19333=(
BOUNDED_CURVE()
B_SPLINE_CURVE(2,(#78425,#78426,#78427),.UNSPECIFIED.,.F.,.F.)
B_SPLINE_CURVE_WITH_KNOTS((3,3),(0.339146964126524,0.668418076018308),
 .UNSPECIFIED.)
CURVE()
GEOMETRIC_REPRESENTATION_ITEM()
RATIONAL_B_SPLINE_CURVE((1.00400190544533,1.00495889669787,1.00400190544533))
REPRESENTATION_ITEM('')
);
#19334=(
BOUNDED_CURVE()
B_SPLINE_CURVE(2,(#78429,#78430,#78431),.UNSPECIFIED.,.F.,.F.)
B_SPLINE_CURVE_WITH_KNOTS((3,3),(0.0284639720345148,0.0708739951602895),
 .UNSPECIFIED.)
CURVE()
GEOMETRIC_REPRESENTATION_ITEM()
RATIONAL_B_SPLINE_CURVE((1.00001075173436,1.00001338566466,1.))
REPRESENTATION_ITEM('')
);
#19335=(
BOUNDED_CURVE()
B_SPLINE_CURVE(2,(#78435,#78436,#78437),.UNSPECIFIED.,.F.,.F.)
B_SPLINE_CURVE_WITH_KNOTS((3,3),(0.,0.0424100233282264),.UNSPECIFIED.)
CURVE()
GEOMETRIC_REPRESENTATION_ITEM()
RATIONAL_B_SPLINE_CURVE((1.,1.00001338433303,1.00001075066468))
REPRESENTATION_ITEM('')
);
#19336=(
BOUNDED_CURVE()
B_SPLINE_CURVE(2,(#78439,#78440,#78441),.UNSPECIFIED.,.F.,.F.)
B_SPLINE_CURVE_WITH_KNOTS((3,3),(0.339146964126518,0.668418076018304),
 .UNSPECIFIED.)
CURVE()
GEOMETRIC_REPRESENTATION_ITEM()
RATIONAL_B_SPLINE_CURVE((1.00400190544534,1.00495889669788,1.00400190544534))
REPRESENTATION_ITEM('')
);
#19337=(
BOUNDED_CURVE()
B_SPLINE_CURVE(2,(#78443,#78444,#78445),.UNSPECIFIED.,.F.,.F.)
B_SPLINE_CURVE_WITH_KNOTS((3,3),(0.028463971433294,0.0708739951602898),
 .UNSPECIFIED.)
CURVE()
GEOMETRIC_REPRESENTATION_ITEM()
RATIONAL_B_SPLINE_CURVE((1.00001075098432,1.00001338473115,1.))
REPRESENTATION_ITEM('')
);
#19338=(
BOUNDED_CURVE()
B_SPLINE_CURVE(2,(#78449,#78450,#78451),.UNSPECIFIED.,.F.,.F.)
B_SPLINE_CURVE_WITH_KNOTS((3,3),(0.,0.042410024098998),.UNSPECIFIED.)
CURVE()
GEOMETRIC_REPRESENTATION_ITEM()
RATIONAL_B_SPLINE_CURVE((1.,1.00001338512572,1.0000107513011))
REPRESENTATION_ITEM('')
);
#19339=(
BOUNDED_CURVE()
B_SPLINE_CURVE(2,(#78453,#78454,#78455),.UNSPECIFIED.,.F.,.F.)
B_SPLINE_CURVE_WITH_KNOTS((3,3),(0.33914696412651,0.668418076018299),
 .UNSPECIFIED.)
CURVE()
GEOMETRIC_REPRESENTATION_ITEM()
RATIONAL_B_SPLINE_CURVE((1.00400190544535,1.00495889669788,1.00400190544535))
REPRESENTATION_ITEM('')
);
#19340=(
BOUNDED_CURVE()
B_SPLINE_CURVE(2,(#78457,#78458,#78459),.UNSPECIFIED.,.F.,.F.)
B_SPLINE_CURVE_WITH_KNOTS((3,3),(0.0284639719730562,0.0708739951602891),
 .UNSPECIFIED.)
CURVE()
GEOMETRIC_REPRESENTATION_ITEM()
RATIONAL_B_SPLINE_CURVE((1.00001075041269,1.00001338401924,1.))
REPRESENTATION_ITEM('')
);
#19341=(
BOUNDED_CURVE()
B_SPLINE_CURVE(2,(#78462,#78463,#78464),.UNSPECIFIED.,.F.,.F.)
B_SPLINE_CURVE_WITH_KNOTS((3,3),(0.,0.0709397118056796),.UNSPECIFIED.)
CURVE()
GEOMETRIC_REPRESENTATION_ITEM()
RATIONAL_B_SPLINE_CURVE((1.,1.00002245188718,1.))
REPRESENTATION_ITEM('')
);
#19342=(
BOUNDED_CURVE()
B_SPLINE_CURVE(2,(#78482,#78483,#78484),.UNSPECIFIED.,.F.,.F.)
B_SPLINE_CURVE_WITH_KNOTS((3,3),(0.072859873218516,0.164428174992087),
 .UNSPECIFIED.)
CURVE()
GEOMETRIC_REPRESENTATION_ITEM()
RATIONAL_B_SPLINE_CURVE((1.00004422028548,1.00004989756719,1.))
REPRESENTATION_ITEM('')
);
#19343=(
BOUNDED_CURVE()
B_SPLINE_CURVE(2,(#78486,#78487,#78488),.UNSPECIFIED.,.F.,.F.)
B_SPLINE_CURVE_WITH_KNOTS((3,3),(0.526544758504317,0.808610241550327),
 .UNSPECIFIED.)
CURVE()
GEOMETRIC_REPRESENTATION_ITEM()
RATIONAL_B_SPLINE_CURVE((1.00594694470058,1.00650257927329,1.00594694470058))
REPRESENTATION_ITEM('')
);
#19344=(
BOUNDED_CURVE()
B_SPLINE_CURVE(2,(#78490,#78491,#78492),.UNSPECIFIED.,.F.,.F.)
B_SPLINE_CURVE_WITH_KNOTS((3,3),(0.,0.0915683011616728),.UNSPECIFIED.)
CURVE()
GEOMETRIC_REPRESENTATION_ITEM()
RATIONAL_B_SPLINE_CURVE((1.,1.00004989745095,1.00004422018284))
REPRESENTATION_ITEM('')
);
#19345=(
BOUNDED_CURVE()
B_SPLINE_CURVE(2,(#78497,#78498,#78499),.UNSPECIFIED.,.F.,.F.)
B_SPLINE_CURVE_WITH_KNOTS((3,3),(0.0728598736698146,0.164428174992088),
 .UNSPECIFIED.)
CURVE()
GEOMETRIC_REPRESENTATION_ITEM()
RATIONAL_B_SPLINE_CURVE((1.00004421982567,1.00004989704804,1.))
REPRESENTATION_ITEM('')
);
#19346=(
BOUNDED_CURVE()
B_SPLINE_CURVE(2,(#78501,#78502,#78503),.UNSPECIFIED.,.F.,.F.)
B_SPLINE_CURVE_WITH_KNOTS((3,3),(0.526544758504314,0.808610241550329),
 .UNSPECIFIED.)
CURVE()
GEOMETRIC_REPRESENTATION_ITEM()
RATIONAL_B_SPLINE_CURVE((1.00594694470059,1.00650257927331,1.00594694470059))
REPRESENTATION_ITEM('')
);
#19347=(
BOUNDED_CURVE()
B_SPLINE_CURVE(2,(#78505,#78506,#78507),.UNSPECIFIED.,.F.,.F.)
B_SPLINE_CURVE_WITH_KNOTS((3,3),(0.,0.09156830116281),.UNSPECIFIED.)
CURVE()
GEOMETRIC_REPRESENTATION_ITEM()
RATIONAL_B_SPLINE_CURVE((1.,1.00004989701499,1.00004421979647))
REPRESENTATION_ITEM('')
);
#19348=(
BOUNDED_CURVE()
B_SPLINE_CURVE(2,(#78512,#78513,#78514),.UNSPECIFIED.,.F.,.F.)
B_SPLINE_CURVE_WITH_KNOTS((3,3),(0.0728598735675412,0.164428174992088),
 .UNSPECIFIED.)
CURVE()
GEOMETRIC_REPRESENTATION_ITEM()
RATIONAL_B_SPLINE_CURVE((1.00004422027197,1.00004989755171,1.))
REPRESENTATION_ITEM('')
);
#19349=(
BOUNDED_CURVE()
B_SPLINE_CURVE(2,(#78516,#78517,#78518),.UNSPECIFIED.,.F.,.F.)
B_SPLINE_CURVE_WITH_KNOTS((3,3),(0.526544758504315,0.808610241550327),
 .UNSPECIFIED.)
CURVE()
GEOMETRIC_REPRESENTATION_ITEM()
RATIONAL_B_SPLINE_CURVE((1.00594694470059,1.0065025792733,1.00594694470059))
REPRESENTATION_ITEM('')
);
#19350=(
BOUNDED_CURVE()
B_SPLINE_CURVE(2,(#78520,#78521,#78522),.UNSPECIFIED.,.F.,.F.)
B_SPLINE_CURVE_WITH_KNOTS((3,3),(0.,0.0915683022545724),.UNSPECIFIED.)
CURVE()
GEOMETRIC_REPRESENTATION_ITEM()
RATIONAL_B_SPLINE_CURVE((1.,1.00004989734545,1.00004422008868))
REPRESENTATION_ITEM('')
);
#19351=(
BOUNDED_CURVE()
B_SPLINE_CURVE(2,(#78527,#78528,#78529),.UNSPECIFIED.,.F.,.F.)
B_SPLINE_CURVE_WITH_KNOTS((3,3),(0.0728598733693843,0.164428174992087),
 .UNSPECIFIED.)
CURVE()
GEOMETRIC_REPRESENTATION_ITEM()
RATIONAL_B_SPLINE_CURVE((1.0000442202851,1.00004989756666,1.))
REPRESENTATION_ITEM('')
);
#19352=(
BOUNDED_CURVE()
B_SPLINE_CURVE(2,(#78531,#78532,#78533),.UNSPECIFIED.,.F.,.F.)
B_SPLINE_CURVE_WITH_KNOTS((3,3),(0.526544758504307,0.808610241550322),
 .UNSPECIFIED.)
CURVE()
GEOMETRIC_REPRESENTATION_ITEM()
RATIONAL_B_SPLINE_CURVE((1.00594694470059,1.00650257927331,1.00594694470059))
REPRESENTATION_ITEM('')
);
#19353=(
BOUNDED_CURVE()
B_SPLINE_CURVE(2,(#78535,#78536,#78537),.UNSPECIFIED.,.F.,.F.)
B_SPLINE_CURVE_WITH_KNOTS((3,3),(0.,0.091568301844154),.UNSPECIFIED.)
CURVE()
GEOMETRIC_REPRESENTATION_ITEM()
RATIONAL_B_SPLINE_CURVE((1.,1.00004989738211,1.00004422012141))
REPRESENTATION_ITEM('')
);
#19354=(
BOUNDED_CURVE()
B_SPLINE_CURVE(2,(#78542,#78543,#78544),.UNSPECIFIED.,.F.,.F.)
B_SPLINE_CURVE_WITH_KNOTS((3,3),(0.0728598727493186,0.164428174992087),
 .UNSPECIFIED.)
CURVE()
GEOMETRIC_REPRESENTATION_ITEM()
RATIONAL_B_SPLINE_CURVE((1.00004422024106,1.00004989751739,1.))
REPRESENTATION_ITEM('')
);
#19355=(
BOUNDED_CURVE()
B_SPLINE_CURVE(2,(#78546,#78547,#78548),.UNSPECIFIED.,.F.,.F.)
B_SPLINE_CURVE_WITH_KNOTS((3,3),(0.526544758504317,0.808610241550328),
 .UNSPECIFIED.)
CURVE()
GEOMETRIC_REPRESENTATION_ITEM()
RATIONAL_B_SPLINE_CURVE((1.00594694470058,1.0065025792733,1.00594694470058))
REPRESENTATION_ITEM('')
);
#19356=(
BOUNDED_CURVE()
B_SPLINE_CURVE(2,(#78550,#78551,#78552),.UNSPECIFIED.,.F.,.F.)
B_SPLINE_CURVE_WITH_KNOTS((3,3),(0.,0.0915683005636383),.UNSPECIFIED.)
CURVE()
GEOMETRIC_REPRESENTATION_ITEM()
RATIONAL_B_SPLINE_CURVE((1.,1.00004989687733,1.00004421967485))
REPRESENTATION_ITEM('')
);
#19357=(
BOUNDED_CURVE()
B_SPLINE_CURVE(2,(#78557,#78558,#78559),.UNSPECIFIED.,.F.,.F.)
B_SPLINE_CURVE_WITH_KNOTS((3,3),(0.0728598739393654,0.164428174992088),
 .UNSPECIFIED.)
CURVE()
GEOMETRIC_REPRESENTATION_ITEM()
RATIONAL_B_SPLINE_CURVE((1.00004421961259,1.00004989680742,1.))
REPRESENTATION_ITEM('')
);
#19358=(
BOUNDED_CURVE()
B_SPLINE_CURVE(2,(#78561,#78562,#78563),.UNSPECIFIED.,.F.,.F.)
B_SPLINE_CURVE_WITH_KNOTS((3,3),(0.526544758504316,0.808610241550329),
 .UNSPECIFIED.)
CURVE()
GEOMETRIC_REPRESENTATION_ITEM()
RATIONAL_B_SPLINE_CURVE((1.00594694470059,1.0065025792733,1.00594694470059))
REPRESENTATION_ITEM('')
);
#19359=(
BOUNDED_CURVE()
B_SPLINE_CURVE(2,(#78565,#78566,#78567),.UNSPECIFIED.,.F.,.F.)
B_SPLINE_CURVE_WITH_KNOTS((3,3),(0.,0.0915683013365669),.UNSPECIFIED.)
CURVE()
GEOMETRIC_REPRESENTATION_ITEM()
RATIONAL_B_SPLINE_CURVE((1.,1.00004989717223,1.00004421993572))
REPRESENTATION_ITEM('')
);
#19360=(
BOUNDED_CURVE()
B_SPLINE_CURVE(2,(#78572,#78573,#78574),.UNSPECIFIED.,.F.,.F.)
B_SPLINE_CURVE_WITH_KNOTS((3,3),(0.0728598751585041,0.164428174992087),
 .UNSPECIFIED.)
CURVE()
GEOMETRIC_REPRESENTATION_ITEM()
RATIONAL_B_SPLINE_CURVE((1.00004421967368,1.00004989687551,1.))
REPRESENTATION_ITEM('')
);
#19361=(
BOUNDED_CURVE()
B_SPLINE_CURVE(2,(#78576,#78577,#78578),.UNSPECIFIED.,.F.,.F.)
B_SPLINE_CURVE_WITH_KNOTS((3,3),(0.526544758504317,0.808610241550327),
 .UNSPECIFIED.)
CURVE()
GEOMETRIC_REPRESENTATION_ITEM()
RATIONAL_B_SPLINE_CURVE((1.00594694470058,1.00650257927329,1.00594694470058))
REPRESENTATION_ITEM('')
);
#19362=(
BOUNDED_CURVE()
B_SPLINE_CURVE(2,(#78580,#78581,#78582),.UNSPECIFIED.,.F.,.F.)
B_SPLINE_CURVE_WITH_KNOTS((3,3),(0.,0.0915683017593413),.UNSPECIFIED.)
CURVE()
GEOMETRIC_REPRESENTATION_ITEM()
RATIONAL_B_SPLINE_CURVE((1.,1.00004989738203,1.00004422012139))
REPRESENTATION_ITEM('')
);
#19363=(
BOUNDED_CURVE()
B_SPLINE_CURVE(2,(#78587,#78588,#78589),.UNSPECIFIED.,.F.,.F.)
B_SPLINE_CURVE_WITH_KNOTS((3,3),(0.0728598743955349,0.164428174992088),
 .UNSPECIFIED.)
CURVE()
GEOMETRIC_REPRESENTATION_ITEM()
RATIONAL_B_SPLINE_CURVE((1.00004422007075,1.00004989732408,1.))
REPRESENTATION_ITEM('')
);
#19364=(
BOUNDED_CURVE()
B_SPLINE_CURVE(2,(#78591,#78592,#78593),.UNSPECIFIED.,.F.,.F.)
B_SPLINE_CURVE_WITH_KNOTS((3,3),(0.526544758504317,0.808610241550327),
 .UNSPECIFIED.)
CURVE()
GEOMETRIC_REPRESENTATION_ITEM()
RATIONAL_B_SPLINE_CURVE((1.00594694470058,1.00650257927329,1.00594694470058))
REPRESENTATION_ITEM('')
);
#19365=(
BOUNDED_CURVE()
B_SPLINE_CURVE(2,(#78595,#78596,#78597),.UNSPECIFIED.,.F.,.F.)
B_SPLINE_CURVE_WITH_KNOTS((3,3),(0.,0.0915683011593544),.UNSPECIFIED.)
CURVE()
GEOMETRIC_REPRESENTATION_ITEM()
RATIONAL_B_SPLINE_CURVE((1.,1.00004989717994,1.00004421994266))
REPRESENTATION_ITEM('')
);
#19366=(
BOUNDED_CURVE()
B_SPLINE_CURVE(2,(#78602,#78603,#78604),.UNSPECIFIED.,.F.,.F.)
B_SPLINE_CURVE_WITH_KNOTS((3,3),(0.0728598745472918,0.164428174992087),
 .UNSPECIFIED.)
CURVE()
GEOMETRIC_REPRESENTATION_ITEM()
RATIONAL_B_SPLINE_CURVE((1.00004422005424,1.00004989730536,1.))
REPRESENTATION_ITEM('')
);
#19367=(
BOUNDED_CURVE()
B_SPLINE_CURVE(2,(#78606,#78607,#78608),.UNSPECIFIED.,.F.,.F.)
B_SPLINE_CURVE_WITH_KNOTS((3,3),(0.526544758504319,0.808610241550335),
 .UNSPECIFIED.)
CURVE()
GEOMETRIC_REPRESENTATION_ITEM()
RATIONAL_B_SPLINE_CURVE((1.0059469447006,1.00650257927331,1.0059469447006))
REPRESENTATION_ITEM('')
);
#19368=(
BOUNDED_CURVE()
B_SPLINE_CURVE(2,(#78610,#78611,#78612),.UNSPECIFIED.,.F.,.F.)
B_SPLINE_CURVE_WITH_KNOTS((3,3),(0.,0.0915683006206516),.UNSPECIFIED.)
CURVE()
GEOMETRIC_REPRESENTATION_ITEM()
RATIONAL_B_SPLINE_CURVE((1.,1.00004989694253,1.00004421973259))
REPRESENTATION_ITEM('')
);
#19369=(
BOUNDED_CURVE()
B_SPLINE_CURVE(2,(#78617,#78618,#78619),.UNSPECIFIED.,.F.,.F.)
B_SPLINE_CURVE_WITH_KNOTS((3,3),(0.0728598732187887,0.164428174992087),
 .UNSPECIFIED.)
CURVE()
GEOMETRIC_REPRESENTATION_ITEM()
RATIONAL_B_SPLINE_CURVE((1.00004422023233,1.00004989750722,1.))
REPRESENTATION_ITEM('')
);
#19370=(
BOUNDED_CURVE()
B_SPLINE_CURVE(2,(#78621,#78622,#78623),.UNSPECIFIED.,.F.,.F.)
B_SPLINE_CURVE_WITH_KNOTS((3,3),(0.526544758504317,0.808610241550327),
 .UNSPECIFIED.)
CURVE()
GEOMETRIC_REPRESENTATION_ITEM()
RATIONAL_B_SPLINE_CURVE((1.00594694470058,1.00650257927329,1.00594694470058))
REPRESENTATION_ITEM('')
);
#19371=(
BOUNDED_CURVE()
B_SPLINE_CURVE(2,(#78625,#78626,#78627),.UNSPECIFIED.,.F.,.F.)
B_SPLINE_CURVE_WITH_KNOTS((3,3),(0.,0.0915683011622659),.UNSPECIFIED.)
CURVE()
GEOMETRIC_REPRESENTATION_ITEM()
RATIONAL_B_SPLINE_CURVE((1.,1.00004989751462,1.00004422023926))
REPRESENTATION_ITEM('')
);
#19372=(
BOUNDED_CURVE()
B_SPLINE_CURVE(2,(#78632,#78633,#78634),.UNSPECIFIED.,.F.,.F.)
B_SPLINE_CURVE_WITH_KNOTS((3,3),(0.0728598743613769,0.164428174992088),
 .UNSPECIFIED.)
CURVE()
GEOMETRIC_REPRESENTATION_ITEM()
RATIONAL_B_SPLINE_CURVE((1.00004421988312,1.0000498971124,1.))
REPRESENTATION_ITEM('')
);
#19373=(
BOUNDED_CURVE()
B_SPLINE_CURVE(2,(#78636,#78637,#78638),.UNSPECIFIED.,.F.,.F.)
B_SPLINE_CURVE_WITH_KNOTS((3,3),(0.526544758504314,0.808610241550329),
 .UNSPECIFIED.)
CURVE()
GEOMETRIC_REPRESENTATION_ITEM()
RATIONAL_B_SPLINE_CURVE((1.00594694470059,1.00650257927331,1.00594694470059))
REPRESENTATION_ITEM('')
);
#19374=(
BOUNDED_CURVE()
B_SPLINE_CURVE(2,(#78640,#78641,#78642),.UNSPECIFIED.,.F.,.F.)
B_SPLINE_CURVE_WITH_KNOTS((3,3),(0.,0.0915683004683977),.UNSPECIFIED.)
CURVE()
GEOMETRIC_REPRESENTATION_ITEM()
RATIONAL_B_SPLINE_CURVE((1.,1.00004989675431,1.00004421956588))
REPRESENTATION_ITEM('')
);
#19375=(
BOUNDED_CURVE()
B_SPLINE_CURVE(2,(#78647,#78648,#78649),.UNSPECIFIED.,.F.,.F.)
B_SPLINE_CURVE_WITH_KNOTS((3,3),(0.0728598726718109,0.164428174992088),
 .UNSPECIFIED.)
CURVE()
GEOMETRIC_REPRESENTATION_ITEM()
RATIONAL_B_SPLINE_CURVE((1.00004422040501,1.00004989770244,1.))
REPRESENTATION_ITEM('')
);
#19376=(
BOUNDED_CURVE()
B_SPLINE_CURVE(2,(#78651,#78652,#78653),.UNSPECIFIED.,.F.,.F.)
B_SPLINE_CURVE_WITH_KNOTS((3,3),(0.526544758504306,0.808610241550323),
 .UNSPECIFIED.)
CURVE()
GEOMETRIC_REPRESENTATION_ITEM()
RATIONAL_B_SPLINE_CURVE((1.0059469447006,1.00650257927332,1.0059469447006))
REPRESENTATION_ITEM('')
);
#19377=(
BOUNDED_CURVE()
B_SPLINE_CURVE(2,(#78655,#78656,#78657),.UNSPECIFIED.,.F.,.F.)
B_SPLINE_CURVE_WITH_KNOTS((3,3),(0.,0.0915683018343069),.UNSPECIFIED.)
CURVE()
GEOMETRIC_REPRESENTATION_ITEM()
RATIONAL_B_SPLINE_CURVE((1.,1.00004989767869,1.00004422038426))
REPRESENTATION_ITEM('')
);
#19378=(
BOUNDED_CURVE()
B_SPLINE_CURVE(2,(#78662,#78663,#78664),.UNSPECIFIED.,.F.,.F.)
B_SPLINE_CURVE_WITH_KNOTS((3,3),(0.0728598734298788,0.164428174992087),
 .UNSPECIFIED.)
CURVE()
GEOMETRIC_REPRESENTATION_ITEM()
RATIONAL_B_SPLINE_CURVE((1.00004422015244,1.00004989741692,1.))
REPRESENTATION_ITEM('')
);
#19379=(
BOUNDED_CURVE()
B_SPLINE_CURVE(2,(#78666,#78667,#78668),.UNSPECIFIED.,.F.,.F.)
B_SPLINE_CURVE_WITH_KNOTS((3,3),(0.526544758504322,0.808610241550332),
 .UNSPECIFIED.)
CURVE()
GEOMETRIC_REPRESENTATION_ITEM()
RATIONAL_B_SPLINE_CURVE((1.00594694470058,1.00650257927329,1.00594694470058))
REPRESENTATION_ITEM('')
);
#19380=(
BOUNDED_CURVE()
B_SPLINE_CURVE(2,(#78670,#78671,#78672),.UNSPECIFIED.,.F.,.F.)
B_SPLINE_CURVE_WITH_KNOTS((3,3),(0.,0.0915683005750663),.UNSPECIFIED.)
CURVE()
GEOMETRIC_REPRESENTATION_ITEM()
RATIONAL_B_SPLINE_CURVE((1.,1.0000498970517,1.00004421982937))
REPRESENTATION_ITEM('')
);
#19381=(
BOUNDED_CURVE()
B_SPLINE_CURVE(2,(#78677,#78678,#78679),.UNSPECIFIED.,.F.,.F.)
B_SPLINE_CURVE_WITH_KNOTS((3,3),(0.0728598737528459,0.164428174992088),
 .UNSPECIFIED.)
CURVE()
GEOMETRIC_REPRESENTATION_ITEM()
RATIONAL_B_SPLINE_CURVE((1.00004421990677,1.0000498971395,1.))
REPRESENTATION_ITEM('')
);
#19382=(
BOUNDED_CURVE()
B_SPLINE_CURVE(2,(#78681,#78682,#78683),.UNSPECIFIED.,.F.,.F.)
B_SPLINE_CURVE_WITH_KNOTS((3,3),(0.526544758504314,0.808610241550329),
 .UNSPECIFIED.)
CURVE()
GEOMETRIC_REPRESENTATION_ITEM()
RATIONAL_B_SPLINE_CURVE((1.00594694470059,1.00650257927331,1.00594694470059))
REPRESENTATION_ITEM('')
);
#19383=(
BOUNDED_CURVE()
B_SPLINE_CURVE(2,(#78685,#78686,#78687),.UNSPECIFIED.,.F.,.F.)
B_SPLINE_CURVE_WITH_KNOTS((3,3),(0.,0.0915683018875454),.UNSPECIFIED.)
CURVE()
GEOMETRIC_REPRESENTATION_ITEM()
RATIONAL_B_SPLINE_CURVE((1.,1.00004989719222,1.0000442199531))
REPRESENTATION_ITEM('')
);
#19384=(
BOUNDED_CURVE()
B_SPLINE_CURVE(2,(#78692,#78693,#78694),.UNSPECIFIED.,.F.,.F.)
B_SPLINE_CURVE_WITH_KNOTS((3,3),(0.0728598745151923,0.164428174992087),
 .UNSPECIFIED.)
CURVE()
GEOMETRIC_REPRESENTATION_ITEM()
RATIONAL_B_SPLINE_CURVE((1.00004421966589,1.00004989686717,1.))
REPRESENTATION_ITEM('')
);
#19385=(
BOUNDED_CURVE()
B_SPLINE_CURVE(2,(#78696,#78697,#78698),.UNSPECIFIED.,.F.,.F.)
B_SPLINE_CURVE_WITH_KNOTS((3,3),(0.526544758504313,0.808610241550331),
 .UNSPECIFIED.)
CURVE()
GEOMETRIC_REPRESENTATION_ITEM()
RATIONAL_B_SPLINE_CURVE((1.0059469447006,1.00650257927332,1.0059469447006))
REPRESENTATION_ITEM('')
);
#19386=(
BOUNDED_CURVE()
B_SPLINE_CURVE(2,(#78700,#78701,#78702),.UNSPECIFIED.,.F.,.F.)
B_SPLINE_CURVE_WITH_KNOTS((3,3),(0.,0.0915683010779811),.UNSPECIFIED.)
CURVE()
GEOMETRIC_REPRESENTATION_ITEM()
RATIONAL_B_SPLINE_CURVE((1.,1.00004989711025,1.00004421988095))
REPRESENTATION_ITEM('')
);
#19387=(
BOUNDED_CURVE()
B_SPLINE_CURVE(2,(#78707,#78708,#78709),.UNSPECIFIED.,.F.,.F.)
B_SPLINE_CURVE_WITH_KNOTS((3,3),(0.0728598743365227,0.164428174992087),
 .UNSPECIFIED.)
CURVE()
GEOMETRIC_REPRESENTATION_ITEM()
RATIONAL_B_SPLINE_CURVE((1.00004422013591,1.00004989739766,1.))
REPRESENTATION_ITEM('')
);
#19388=(
BOUNDED_CURVE()
B_SPLINE_CURVE(2,(#78711,#78712,#78713),.UNSPECIFIED.,.F.,.F.)
B_SPLINE_CURVE_WITH_KNOTS((3,3),(0.526544758504318,0.808610241550326),
 .UNSPECIFIED.)
CURVE()
GEOMETRIC_REPRESENTATION_ITEM()
RATIONAL_B_SPLINE_CURVE((1.00594694470057,1.00650257927328,1.00594694470057))
REPRESENTATION_ITEM('')
);
#19389=(
BOUNDED_CURVE()
B_SPLINE_CURVE(2,(#78715,#78716,#78717),.UNSPECIFIED.,.F.,.F.)
B_SPLINE_CURVE_WITH_KNOTS((3,3),(0.,0.0915682998237193),.UNSPECIFIED.)
CURVE()
GEOMETRIC_REPRESENTATION_ITEM()
RATIONAL_B_SPLINE_CURVE((1.,1.00004989671321,1.00004421952985))
REPRESENTATION_ITEM('')
);
#19390=(
BOUNDED_CURVE()
B_SPLINE_CURVE(2,(#78722,#78723,#78724),.UNSPECIFIED.,.F.,.F.)
B_SPLINE_CURVE_WITH_KNOTS((3,3),(0.0728598745249184,0.164428174992087),
 .UNSPECIFIED.)
CURVE()
GEOMETRIC_REPRESENTATION_ITEM()
RATIONAL_B_SPLINE_CURVE((1.00004421993429,1.00004989717003,1.))
REPRESENTATION_ITEM('')
);
#19391=(
BOUNDED_CURVE()
B_SPLINE_CURVE(2,(#78726,#78727,#78728),.UNSPECIFIED.,.F.,.F.)
B_SPLINE_CURVE_WITH_KNOTS((3,3),(0.52654475850432,0.808610241550335),
 .UNSPECIFIED.)
CURVE()
GEOMETRIC_REPRESENTATION_ITEM()
RATIONAL_B_SPLINE_CURVE((1.0059469447006,1.00650257927331,1.0059469447006))
REPRESENTATION_ITEM('')
);
#19392=(
BOUNDED_CURVE()
B_SPLINE_CURVE(2,(#78730,#78731,#78732),.UNSPECIFIED.,.F.,.F.)
B_SPLINE_CURVE_WITH_KNOTS((3,3),(0.,0.0915683006102755),.UNSPECIFIED.)
CURVE()
GEOMETRIC_REPRESENTATION_ITEM()
RATIONAL_B_SPLINE_CURVE((1.,1.000049897179,1.00004421994216))
REPRESENTATION_ITEM('')
);
#19393=(
BOUNDED_CURVE()
B_SPLINE_CURVE(2,(#78737,#78738,#78739),.UNSPECIFIED.,.F.,.F.)
B_SPLINE_CURVE_WITH_KNOTS((3,3),(0.0728598745442839,0.164428174992087),
 .UNSPECIFIED.)
CURVE()
GEOMETRIC_REPRESENTATION_ITEM()
RATIONAL_B_SPLINE_CURVE((1.0000442198851,1.00004989711451,1.))
REPRESENTATION_ITEM('')
);
#19394=(
BOUNDED_CURVE()
B_SPLINE_CURVE(2,(#78741,#78742,#78743),.UNSPECIFIED.,.F.,.F.)
B_SPLINE_CURVE_WITH_KNOTS((3,3),(0.526544758504317,0.808610241550327),
 .UNSPECIFIED.)
CURVE()
GEOMETRIC_REPRESENTATION_ITEM()
RATIONAL_B_SPLINE_CURVE((1.00594694470058,1.00650257927329,1.00594694470058))
REPRESENTATION_ITEM('')
);
#19395=(
BOUNDED_CURVE()
B_SPLINE_CURVE(2,(#78745,#78746,#78747),.UNSPECIFIED.,.F.,.F.)
B_SPLINE_CURVE_WITH_KNOTS((3,3),(0.,0.0915683018203568),.UNSPECIFIED.)
CURVE()
GEOMETRIC_REPRESENTATION_ITEM()
RATIONAL_B_SPLINE_CURVE((1.,1.00004989789332,1.00004422057448))
REPRESENTATION_ITEM('')
);
#19396=(
BOUNDED_CURVE()
B_SPLINE_CURVE(2,(#78752,#78753,#78754),.UNSPECIFIED.,.F.,.F.)
B_SPLINE_CURVE_WITH_KNOTS((3,3),(0.0728598737856223,0.164428174992088),
 .UNSPECIFIED.)
CURVE()
GEOMETRIC_REPRESENTATION_ITEM()
RATIONAL_B_SPLINE_CURVE((1.00004421995822,1.00004989719753,1.))
REPRESENTATION_ITEM('')
);
#19397=(
BOUNDED_CURVE()
B_SPLINE_CURVE(2,(#78756,#78757,#78758),.UNSPECIFIED.,.F.,.F.)
B_SPLINE_CURVE_WITH_KNOTS((3,3),(0.52654475850432,0.808610241550332),
 .UNSPECIFIED.)
CURVE()
GEOMETRIC_REPRESENTATION_ITEM()
RATIONAL_B_SPLINE_CURVE((1.00594694470059,1.0065025792733,1.00594694470059))
REPRESENTATION_ITEM('')
);
#19398=(
BOUNDED_CURVE()
B_SPLINE_CURVE(2,(#78760,#78761,#78762),.UNSPECIFIED.,.F.,.F.)
B_SPLINE_CURVE_WITH_KNOTS((3,3),(0.,0.0915683018433535),.UNSPECIFIED.)
CURVE()
GEOMETRIC_REPRESENTATION_ITEM()
RATIONAL_B_SPLINE_CURVE((1.,1.00004989711595,1.00004421988554))
REPRESENTATION_ITEM('')
);
#19399=(
BOUNDED_CURVE()
B_SPLINE_CURVE(2,(#78767,#78768,#78769),.UNSPECIFIED.,.F.,.F.)
B_SPLINE_CURVE_WITH_KNOTS((3,3),(0.0728598735563218,0.164428174992087),
 .UNSPECIFIED.)
CURVE()
GEOMETRIC_REPRESENTATION_ITEM()
RATIONAL_B_SPLINE_CURVE((1.00004422001458,1.00004989726128,1.))
REPRESENTATION_ITEM('')
);
#19400=(
BOUNDED_CURVE()
B_SPLINE_CURVE(2,(#78771,#78772,#78773),.UNSPECIFIED.,.F.,.F.)
B_SPLINE_CURVE_WITH_KNOTS((3,3),(0.526544758504322,0.808610241550332),
 .UNSPECIFIED.)
CURVE()
GEOMETRIC_REPRESENTATION_ITEM()
RATIONAL_B_SPLINE_CURVE((1.00594694470058,1.00650257927329,1.00594694470058))
REPRESENTATION_ITEM('')
);
#19401=(
BOUNDED_CURVE()
B_SPLINE_CURVE(2,(#78775,#78776,#78777),.UNSPECIFIED.,.F.,.F.)
B_SPLINE_CURVE_WITH_KNOTS((3,3),(0.,0.0915682994549458),.UNSPECIFIED.)
CURVE()
GEOMETRIC_REPRESENTATION_ITEM()
RATIONAL_B_SPLINE_CURVE((1.,1.00004989645929,1.00004421930504))
REPRESENTATION_ITEM('')
);
#19402=(
BOUNDED_CURVE()
B_SPLINE_CURVE(2,(#78782,#78783,#78784),.UNSPECIFIED.,.F.,.F.)
B_SPLINE_CURVE_WITH_KNOTS((3,3),(0.0728598733693843,0.164428174992087),
 .UNSPECIFIED.)
CURVE()
GEOMETRIC_REPRESENTATION_ITEM()
RATIONAL_B_SPLINE_CURVE((1.0000442202851,1.00004989756666,1.))
REPRESENTATION_ITEM('')
);
#19403=(
BOUNDED_CURVE()
B_SPLINE_CURVE(2,(#78786,#78787,#78788),.UNSPECIFIED.,.F.,.F.)
B_SPLINE_CURVE_WITH_KNOTS((3,3),(0.526544758504307,0.808610241550322),
 .UNSPECIFIED.)
CURVE()
GEOMETRIC_REPRESENTATION_ITEM()
RATIONAL_B_SPLINE_CURVE((1.00594694470059,1.00650257927331,1.00594694470059))
REPRESENTATION_ITEM('')
);
#19404=(
BOUNDED_CURVE()
B_SPLINE_CURVE(2,(#78790,#78791,#78792),.UNSPECIFIED.,.F.,.F.)
B_SPLINE_CURVE_WITH_KNOTS((3,3),(0.,0.091568301844154),.UNSPECIFIED.)
CURVE()
GEOMETRIC_REPRESENTATION_ITEM()
RATIONAL_B_SPLINE_CURVE((1.,1.00004989738211,1.00004422012141))
REPRESENTATION_ITEM('')
);
#19405=(
BOUNDED_CURVE()
B_SPLINE_CURVE(2,(#78797,#78798,#78799),.UNSPECIFIED.,.F.,.F.)
B_SPLINE_CURVE_WITH_KNOTS((3,3),(0.0728598732916255,0.164428174992087),
 .UNSPECIFIED.)
CURVE()
GEOMETRIC_REPRESENTATION_ITEM()
RATIONAL_B_SPLINE_CURVE((1.00004422000312,1.00004989724853,1.))
REPRESENTATION_ITEM('')
);
#19406=(
BOUNDED_CURVE()
B_SPLINE_CURVE(2,(#78801,#78802,#78803),.UNSPECIFIED.,.F.,.F.)
B_SPLINE_CURVE_WITH_KNOTS((3,3),(0.526544758504322,0.808610241550332),
 .UNSPECIFIED.)
CURVE()
GEOMETRIC_REPRESENTATION_ITEM()
RATIONAL_B_SPLINE_CURVE((1.00594694470058,1.00650257927329,1.00594694470058))
REPRESENTATION_ITEM('')
);
#19407=(
BOUNDED_CURVE()
B_SPLINE_CURVE(2,(#78805,#78806,#78807),.UNSPECIFIED.,.F.,.F.)
B_SPLINE_CURVE_WITH_KNOTS((3,3),(0.,0.0915683005619487),.UNSPECIFIED.)
CURVE()
GEOMETRIC_REPRESENTATION_ITEM()
RATIONAL_B_SPLINE_CURVE((1.,1.00004989697534,1.0000442197617))
REPRESENTATION_ITEM('')
);
#19408=(
BOUNDED_CURVE()
B_SPLINE_CURVE(2,(#78812,#78813,#78814),.UNSPECIFIED.,.F.,.F.)
B_SPLINE_CURVE_WITH_KNOTS((3,3),(0.0728598731686667,0.164428174992087),
 .UNSPECIFIED.)
CURVE()
GEOMETRIC_REPRESENTATION_ITEM()
RATIONAL_B_SPLINE_CURVE((1.00004421982523,1.00004989704789,1.))
REPRESENTATION_ITEM('')
);
#19409=(
BOUNDED_CURVE()
B_SPLINE_CURVE(2,(#78816,#78817,#78818),.UNSPECIFIED.,.F.,.F.)
B_SPLINE_CURVE_WITH_KNOTS((3,3),(0.526544758504316,0.808610241550328),
 .UNSPECIFIED.)
CURVE()
GEOMETRIC_REPRESENTATION_ITEM()
RATIONAL_B_SPLINE_CURVE((1.00594694470059,1.0065025792733,1.00594694470059))
REPRESENTATION_ITEM('')
);
#19410=(
BOUNDED_CURVE()
B_SPLINE_CURVE(2,(#78820,#78821,#78822),.UNSPECIFIED.,.F.,.F.)
B_SPLINE_CURVE_WITH_KNOTS((3,3),(0.,0.0915683024294117),.UNSPECIFIED.)
CURVE()
GEOMETRIC_REPRESENTATION_ITEM()
RATIONAL_B_SPLINE_CURVE((1.,1.00004989771985,1.00004422042037))
REPRESENTATION_ITEM('')
);
#19411=(
BOUNDED_CURVE()
B_SPLINE_CURVE(2,(#78827,#78828,#78829),.UNSPECIFIED.,.F.,.F.)
B_SPLINE_CURVE_WITH_KNOTS((3,3),(0.0728598730627314,0.164428174992087),
 .UNSPECIFIED.)
CURVE()
GEOMETRIC_REPRESENTATION_ITEM()
RATIONAL_B_SPLINE_CURVE((1.00004422011343,1.00004989737316,1.))
REPRESENTATION_ITEM('')
);
#19412=(
BOUNDED_CURVE()
B_SPLINE_CURVE(2,(#78831,#78832,#78833),.UNSPECIFIED.,.F.,.F.)
B_SPLINE_CURVE_WITH_KNOTS((3,3),(0.526544758504317,0.808610241550327),
 .UNSPECIFIED.)
CURVE()
GEOMETRIC_REPRESENTATION_ITEM()
RATIONAL_B_SPLINE_CURVE((1.00594694470058,1.00650257927329,1.00594694470058))
REPRESENTATION_ITEM('')
);
#19413=(
BOUNDED_CURVE()
B_SPLINE_CURVE(2,(#78835,#78836,#78837),.UNSPECIFIED.,.F.,.F.)
B_SPLINE_CURVE_WITH_KNOTS((3,3),(0.,0.0915683011593819),.UNSPECIFIED.)
CURVE()
GEOMETRIC_REPRESENTATION_ITEM()
RATIONAL_B_SPLINE_CURVE((1.,1.00004989718316,1.00004421994552))
REPRESENTATION_ITEM('')
);
#19414=(
BOUNDED_CURVE()
B_SPLINE_CURVE(2,(#78842,#78843,#78844),.UNSPECIFIED.,.F.,.F.)
B_SPLINE_CURVE_WITH_KNOTS((3,3),(0.0728598745376772,0.164428174992087),
 .UNSPECIFIED.)
CURVE()
GEOMETRIC_REPRESENTATION_ITEM()
RATIONAL_B_SPLINE_CURVE((1.00004421990789,1.00004989714022,1.))
REPRESENTATION_ITEM('')
);
#19415=(
BOUNDED_CURVE()
B_SPLINE_CURVE(2,(#78846,#78847,#78848),.UNSPECIFIED.,.F.,.F.)
B_SPLINE_CURVE_WITH_KNOTS((3,3),(0.526544758504319,0.808610241550335),
 .UNSPECIFIED.)
CURVE()
GEOMETRIC_REPRESENTATION_ITEM()
RATIONAL_B_SPLINE_CURVE((1.0059469447006,1.00650257927331,1.0059469447006))
REPRESENTATION_ITEM('')
);
#19416=(
BOUNDED_CURVE()
B_SPLINE_CURVE(2,(#78850,#78851,#78852),.UNSPECIFIED.,.F.,.F.)
B_SPLINE_CURVE_WITH_KNOTS((3,3),(0.,0.0915683006214894),.UNSPECIFIED.)
CURVE()
GEOMETRIC_REPRESENTATION_ITEM()
RATIONAL_B_SPLINE_CURVE((1.,1.00004989740271,1.00004422014041))
REPRESENTATION_ITEM('')
);
#19417=(
BOUNDED_CURVE()
B_SPLINE_CURVE(2,(#78857,#78858,#78859),.UNSPECIFIED.,.F.,.F.)
B_SPLINE_CURVE_WITH_KNOTS((3,3),(0.0728598745473656,0.164428174992088),
 .UNSPECIFIED.)
CURVE()
GEOMETRIC_REPRESENTATION_ITEM()
RATIONAL_B_SPLINE_CURVE((1.00004421990015,1.00004989713148,1.))
REPRESENTATION_ITEM('')
);
#19418=(
BOUNDED_CURVE()
B_SPLINE_CURVE(2,(#78861,#78862,#78863),.UNSPECIFIED.,.F.,.F.)
B_SPLINE_CURVE_WITH_KNOTS((3,3),(0.526544758504317,0.808610241550327),
 .UNSPECIFIED.)
CURVE()
GEOMETRIC_REPRESENTATION_ITEM()
RATIONAL_B_SPLINE_CURVE((1.00594694470058,1.00650257927329,1.00594694470058))
REPRESENTATION_ITEM('')
);
#19419=(
BOUNDED_CURVE()
B_SPLINE_CURVE(2,(#78865,#78866,#78867),.UNSPECIFIED.,.F.,.F.)
B_SPLINE_CURVE_WITH_KNOTS((3,3),(0.,0.0915683004967461),.UNSPECIFIED.)
CURVE()
GEOMETRIC_REPRESENTATION_ITEM()
RATIONAL_B_SPLINE_CURVE((1.,1.00004989676149,1.00004421957222))
REPRESENTATION_ITEM('')
);
#19420=(
BOUNDED_CURVE()
B_SPLINE_CURVE(2,(#78872,#78873,#78874),.UNSPECIFIED.,.F.,.F.)
B_SPLINE_CURVE_WITH_KNOTS((3,3),(0.0728598736647092,0.164428174992087),
 .UNSPECIFIED.)
CURVE()
GEOMETRIC_REPRESENTATION_ITEM()
RATIONAL_B_SPLINE_CURVE((1.00004422012316,1.00004989738373,1.))
REPRESENTATION_ITEM('')
);
#19421=(
BOUNDED_CURVE()
B_SPLINE_CURVE(2,(#78876,#78877,#78878),.UNSPECIFIED.,.F.,.F.)
B_SPLINE_CURVE_WITH_KNOTS((3,3),(0.526544758504317,0.808610241550327),
 .UNSPECIFIED.)
CURVE()
GEOMETRIC_REPRESENTATION_ITEM()
RATIONAL_B_SPLINE_CURVE((1.00594694470058,1.00650257927329,1.00594694470058))
REPRESENTATION_ITEM('')
);
#19422=(
BOUNDED_CURVE()
B_SPLINE_CURVE(2,(#78880,#78881,#78882),.UNSPECIFIED.,.F.,.F.)
B_SPLINE_CURVE_WITH_KNOTS((3,3),(0.,0.0915683012539948),.UNSPECIFIED.)
CURVE()
GEOMETRIC_REPRESENTATION_ITEM()
RATIONAL_B_SPLINE_CURVE((1.,1.0000498973998,1.00004422013745))
REPRESENTATION_ITEM('')
);
#19423=(
BOUNDED_CURVE()
B_SPLINE_CURVE(2,(#78887,#78888,#78889),.UNSPECIFIED.,.F.,.F.)
B_SPLINE_CURVE_WITH_KNOTS((3,3),(0.0728598742416343,0.164428174992088),
 .UNSPECIFIED.)
CURVE()
GEOMETRIC_REPRESENTATION_ITEM()
RATIONAL_B_SPLINE_CURVE((1.00004421960735,1.0000498968013,1.))
REPRESENTATION_ITEM('')
);
#19424=(
BOUNDED_CURVE()
B_SPLINE_CURVE(2,(#78891,#78892,#78893),.UNSPECIFIED.,.F.,.F.)
B_SPLINE_CURVE_WITH_KNOTS((3,3),(0.526544758504316,0.808610241550327),
 .UNSPECIFIED.)
CURVE()
GEOMETRIC_REPRESENTATION_ITEM()
RATIONAL_B_SPLINE_CURVE((1.00594694470059,1.0065025792733,1.00594694470059))
REPRESENTATION_ITEM('')
);
#19425=(
BOUNDED_CURVE()
B_SPLINE_CURVE(2,(#78895,#78896,#78897),.UNSPECIFIED.,.F.,.F.)
B_SPLINE_CURVE_WITH_KNOTS((3,3),(0.,0.0915683010196277),.UNSPECIFIED.)
CURVE()
GEOMETRIC_REPRESENTATION_ITEM()
RATIONAL_B_SPLINE_CURVE((1.,1.00004989727193,1.00004422002427))
REPRESENTATION_ITEM('')
);
#19426=(
BOUNDED_CURVE()
B_SPLINE_CURVE(2,(#78902,#78903,#78904),.UNSPECIFIED.,.F.,.F.)
B_SPLINE_CURVE_WITH_KNOTS((3,3),(0.0728598731345689,0.164428174992088),
 .UNSPECIFIED.)
CURVE()
GEOMETRIC_REPRESENTATION_ITEM()
RATIONAL_B_SPLINE_CURVE((1.00004422008966,1.00004989734629,1.))
REPRESENTATION_ITEM('')
);
#19427=(
BOUNDED_CURVE()
B_SPLINE_CURVE(2,(#78906,#78907,#78908),.UNSPECIFIED.,.F.,.F.)
B_SPLINE_CURVE_WITH_KNOTS((3,3),(0.526544758504308,0.80861024155032),
 .UNSPECIFIED.)
CURVE()
GEOMETRIC_REPRESENTATION_ITEM()
RATIONAL_B_SPLINE_CURVE((1.00594694470059,1.0065025792733,1.00594694470059))
REPRESENTATION_ITEM('')
);
#19428=(
BOUNDED_CURVE()
B_SPLINE_CURVE(2,(#78910,#78911,#78912),.UNSPECIFIED.,.F.,.F.)
B_SPLINE_CURVE_WITH_KNOTS((3,3),(0.,0.0915683023201614),.UNSPECIFIED.)
CURVE()
GEOMETRIC_REPRESENTATION_ITEM()
RATIONAL_B_SPLINE_CURVE((1.,1.00004989756362,1.00004422028198))
REPRESENTATION_ITEM('')
);
#19429=(
BOUNDED_CURVE()
B_SPLINE_CURVE(2,(#78917,#78918,#78919),.UNSPECIFIED.,.F.,.F.)
B_SPLINE_CURVE_WITH_KNOTS((3,3),(0.0728598741432394,0.164428174992087),
 .UNSPECIFIED.)
CURVE()
GEOMETRIC_REPRESENTATION_ITEM()
RATIONAL_B_SPLINE_CURVE((1.0000442198169,1.00004989703782,1.))
REPRESENTATION_ITEM('')
);
#19430=(
BOUNDED_CURVE()
B_SPLINE_CURVE(2,(#78921,#78922,#78923),.UNSPECIFIED.,.F.,.F.)
B_SPLINE_CURVE_WITH_KNOTS((3,3),(0.526544758504322,0.808610241550331),
 .UNSPECIFIED.)
CURVE()
GEOMETRIC_REPRESENTATION_ITEM()
RATIONAL_B_SPLINE_CURVE((1.00594694470057,1.00650257927328,1.00594694470057))
REPRESENTATION_ITEM('')
);
#19431=(
BOUNDED_CURVE()
B_SPLINE_CURVE(2,(#78925,#78926,#78927),.UNSPECIFIED.,.F.,.F.)
B_SPLINE_CURVE_WITH_KNOTS((3,3),(0.,0.091568300071012),.UNSPECIFIED.)
CURVE()
GEOMETRIC_REPRESENTATION_ITEM()
RATIONAL_B_SPLINE_CURVE((1.,1.00004989671001,1.00004421952686))
REPRESENTATION_ITEM('')
);
#19432=(
BOUNDED_CURVE()
B_SPLINE_CURVE(2,(#78932,#78933,#78934),.UNSPECIFIED.,.F.,.F.)
B_SPLINE_CURVE_WITH_KNOTS((3,3),(0.072859874431626,0.164428174992088),
 .UNSPECIFIED.)
CURVE()
GEOMETRIC_REPRESENTATION_ITEM()
RATIONAL_B_SPLINE_CURVE((1.00004421999585,1.00004989723955,1.))
REPRESENTATION_ITEM('')
);
#19433=(
BOUNDED_CURVE()
B_SPLINE_CURVE(2,(#78936,#78937,#78938),.UNSPECIFIED.,.F.,.F.)
B_SPLINE_CURVE_WITH_KNOTS((3,3),(0.526544758504315,0.80861024155033),
 .UNSPECIFIED.)
CURVE()
GEOMETRIC_REPRESENTATION_ITEM()
RATIONAL_B_SPLINE_CURVE((1.00594694470059,1.00650257927331,1.00594694470059))
REPRESENTATION_ITEM('')
);
#19434=(
BOUNDED_CURVE()
B_SPLINE_CURVE(2,(#78940,#78941,#78942),.UNSPECIFIED.,.F.,.F.)
B_SPLINE_CURVE_WITH_KNOTS((3,3),(0.,0.0915683013824899),.UNSPECIFIED.)
CURVE()
GEOMETRIC_REPRESENTATION_ITEM()
RATIONAL_B_SPLINE_CURVE((1.,1.00004989718276,1.00004421994503))
REPRESENTATION_ITEM('')
);
#19435=(
BOUNDED_CURVE()
B_SPLINE_CURVE(2,(#78947,#78948,#78949),.UNSPECIFIED.,.F.,.F.)
B_SPLINE_CURVE_WITH_KNOTS((3,3),(0.0728598738602229,0.164428174992088),
 .UNSPECIFIED.)
CURVE()
GEOMETRIC_REPRESENTATION_ITEM()
RATIONAL_B_SPLINE_CURVE((1.00004421989654,1.00004989712788,1.))
REPRESENTATION_ITEM('')
);
#19436=(
BOUNDED_CURVE()
B_SPLINE_CURVE(2,(#78951,#78952,#78953),.UNSPECIFIED.,.F.,.F.)
B_SPLINE_CURVE_WITH_KNOTS((3,3),(0.526544758504319,0.808610241550335),
 .UNSPECIFIED.)
CURVE()
GEOMETRIC_REPRESENTATION_ITEM()
RATIONAL_B_SPLINE_CURVE((1.0059469447006,1.00650257927331,1.0059469447006))
REPRESENTATION_ITEM('')
);
#19437=(
BOUNDED_CURVE()
B_SPLINE_CURVE(2,(#78955,#78956,#78957),.UNSPECIFIED.,.F.,.F.)
B_SPLINE_CURVE_WITH_KNOTS((3,3),(0.,0.0915683010770035),.UNSPECIFIED.)
CURVE()
GEOMETRIC_REPRESENTATION_ITEM()
RATIONAL_B_SPLINE_CURVE((1.,1.00004989738745,1.00004422012661))
REPRESENTATION_ITEM('')
);
#19438=(
BOUNDED_CURVE()
B_SPLINE_CURVE(2,(#78962,#78963,#78964),.UNSPECIFIED.,.F.,.F.)
B_SPLINE_CURVE_WITH_KNOTS((3,3),(0.0728598737013136,0.164428174992087),
 .UNSPECIFIED.)
CURVE()
GEOMETRIC_REPRESENTATION_ITEM()
RATIONAL_B_SPLINE_CURVE((1.00004421995655,1.0000498971957,1.))
REPRESENTATION_ITEM('')
);
#19439=(
BOUNDED_CURVE()
B_SPLINE_CURVE(2,(#78966,#78967,#78968),.UNSPECIFIED.,.F.,.F.)
B_SPLINE_CURVE_WITH_KNOTS((3,3),(0.526544758504317,0.808610241550327),
 .UNSPECIFIED.)
CURVE()
GEOMETRIC_REPRESENTATION_ITEM()
RATIONAL_B_SPLINE_CURVE((1.00594694470058,1.00650257927329,1.00594694470058))
REPRESENTATION_ITEM('')
);
#19440=(
BOUNDED_CURVE()
B_SPLINE_CURVE(2,(#78970,#78971,#78972),.UNSPECIFIED.,.F.,.F.)
B_SPLINE_CURVE_WITH_KNOTS((3,3),(0.,0.0915683004544683),.UNSPECIFIED.)
CURVE()
GEOMETRIC_REPRESENTATION_ITEM()
RATIONAL_B_SPLINE_CURVE((1.,1.00004989698968,1.00004421977447))
REPRESENTATION_ITEM('')
);
#19441=(
BOUNDED_CURVE()
B_SPLINE_CURVE(2,(#78978,#78979,#78980),.UNSPECIFIED.,.F.,.F.)
B_SPLINE_CURVE_WITH_KNOTS((3,3),(0.0728598745393818,0.164428174992087),
 .UNSPECIFIED.)
CURVE()
GEOMETRIC_REPRESENTATION_ITEM()
RATIONAL_B_SPLINE_CURVE((1.00004421963559,1.00004989683296,1.))
REPRESENTATION_ITEM('')
);
#19442=(
BOUNDED_CURVE()
B_SPLINE_CURVE(2,(#78991,#78992,#78993),.UNSPECIFIED.,.F.,.F.)
B_SPLINE_CURVE_WITH_KNOTS((3,3),(0.526544758504312,0.808610241550332),
 .UNSPECIFIED.)
CURVE()
GEOMETRIC_REPRESENTATION_ITEM()
RATIONAL_B_SPLINE_CURVE((1.00594694470061,1.00650257927333,1.00594694470061))
REPRESENTATION_ITEM('')
);
#19443=(
BOUNDED_CURVE()
B_SPLINE_CURVE(2,(#78998,#78999,#79000),.UNSPECIFIED.,.F.,.F.)
B_SPLINE_CURVE_WITH_KNOTS((3,3),(0.0728598752332843,0.164428174992088),
 .UNSPECIFIED.)
CURVE()
GEOMETRIC_REPRESENTATION_ITEM()
RATIONAL_B_SPLINE_CURVE((1.00004421930454,1.00004989645893,1.))
REPRESENTATION_ITEM('')
);
#19444=(
BOUNDED_CURVE()
B_SPLINE_CURVE(2,(#79011,#79012,#79013),.UNSPECIFIED.,.F.,.F.)
B_SPLINE_CURVE_WITH_KNOTS((3,3),(0.52654475850433,0.808610241550344),
 .UNSPECIFIED.)
CURVE()
GEOMETRIC_REPRESENTATION_ITEM()
RATIONAL_B_SPLINE_CURVE((1.00594694470059,1.00650257927331,1.00594694470059))
REPRESENTATION_ITEM('')
);
#19445=(
BOUNDED_CURVE()
B_SPLINE_CURVE(2,(#79018,#79019,#79020),.UNSPECIFIED.,.F.,.F.)
B_SPLINE_CURVE_WITH_KNOTS((3,3),(0.072859875072559,0.164428174992087),
 .UNSPECIFIED.)
CURVE()
GEOMETRIC_REPRESENTATION_ITEM()
RATIONAL_B_SPLINE_CURVE((1.00004421966611,1.00004989686704,1.))
REPRESENTATION_ITEM('')
);
#19446=(
BOUNDED_CURVE()
B_SPLINE_CURVE(2,(#79031,#79032,#79033),.UNSPECIFIED.,.F.,.F.)
B_SPLINE_CURVE_WITH_KNOTS((3,3),(0.526544758504327,0.808610241550334),
 .UNSPECIFIED.)
CURVE()
GEOMETRIC_REPRESENTATION_ITEM()
RATIONAL_B_SPLINE_CURVE((1.00594694470057,1.00650257927328,1.00594694470057))
REPRESENTATION_ITEM('')
);
#19447=(
BOUNDED_CURVE()
B_SPLINE_CURVE(2,(#79038,#79039,#79040),.UNSPECIFIED.,.F.,.F.)
B_SPLINE_CURVE_WITH_KNOTS((3,3),(0.0728598742504614,0.164428174992087),
 .UNSPECIFIED.)
CURVE()
GEOMETRIC_REPRESENTATION_ITEM()
RATIONAL_B_SPLINE_CURVE((1.0000442198312,1.00004989705388,1.))
REPRESENTATION_ITEM('')
);
#19448=(
BOUNDED_CURVE()
B_SPLINE_CURVE(2,(#79051,#79052,#79053),.UNSPECIFIED.,.F.,.F.)
B_SPLINE_CURVE_WITH_KNOTS((3,3),(0.526544758504325,0.808610241550338),
 .UNSPECIFIED.)
CURVE()
GEOMETRIC_REPRESENTATION_ITEM()
RATIONAL_B_SPLINE_CURVE((1.00594694470059,1.0065025792733,1.00594694470059))
REPRESENTATION_ITEM('')
);
#19449=(
BOUNDED_CURVE()
B_SPLINE_CURVE(2,(#79058,#79059,#79060),.UNSPECIFIED.,.F.,.F.)
B_SPLINE_CURVE_WITH_KNOTS((3,3),(0.0728598740519051,0.164428174992087),
 .UNSPECIFIED.)
CURVE()
GEOMETRIC_REPRESENTATION_ITEM()
RATIONAL_B_SPLINE_CURVE((1.00004421980835,1.00004989702823,1.))
REPRESENTATION_ITEM('')
);
#19450=(
BOUNDED_CURVE()
B_SPLINE_CURVE(2,(#79071,#79072,#79073),.UNSPECIFIED.,.F.,.F.)
B_SPLINE_CURVE_WITH_KNOTS((3,3),(0.526544758504316,0.808610241550331),
 .UNSPECIFIED.)
CURVE()
GEOMETRIC_REPRESENTATION_ITEM()
RATIONAL_B_SPLINE_CURVE((1.0059469447006,1.00650257927331,1.0059469447006))
REPRESENTATION_ITEM('')
);
#19451=(
BOUNDED_CURVE()
B_SPLINE_CURVE(2,(#79078,#79079,#79080),.UNSPECIFIED.,.F.,.F.)
B_SPLINE_CURVE_WITH_KNOTS((3,3),(0.0728598732895676,0.164428174992087),
 .UNSPECIFIED.)
CURVE()
GEOMETRIC_REPRESENTATION_ITEM()
RATIONAL_B_SPLINE_CURVE((1.00004422030706,1.0000498975915,1.))
REPRESENTATION_ITEM('')
);
#19452=(
BOUNDED_CURVE()
B_SPLINE_CURVE(2,(#79091,#79092,#79093),.UNSPECIFIED.,.F.,.F.)
B_SPLINE_CURVE_WITH_KNOTS((3,3),(0.526544758504325,0.808610241550338),
 .UNSPECIFIED.)
CURVE()
GEOMETRIC_REPRESENTATION_ITEM()
RATIONAL_B_SPLINE_CURVE((1.00594694470059,1.0065025792733,1.00594694470059))
REPRESENTATION_ITEM('')
);
#19453=(
BOUNDED_CURVE()
B_SPLINE_CURVE(2,(#79098,#79099,#79100),.UNSPECIFIED.,.F.,.F.)
B_SPLINE_CURVE_WITH_KNOTS((3,3),(0.0728598732782704,0.164428174992087),
 .UNSPECIFIED.)
CURVE()
GEOMETRIC_REPRESENTATION_ITEM()
RATIONAL_B_SPLINE_CURVE((1.00004422011247,1.00004989737192,1.))
REPRESENTATION_ITEM('')
);
#19454=(
BOUNDED_CURVE()
B_SPLINE_CURVE(2,(#79111,#79112,#79113),.UNSPECIFIED.,.F.,.F.)
B_SPLINE_CURVE_WITH_KNOTS((3,3),(0.526544758504328,0.808610241550337),
 .UNSPECIFIED.)
CURVE()
GEOMETRIC_REPRESENTATION_ITEM()
RATIONAL_B_SPLINE_CURVE((1.00594694470057,1.00650257927329,1.00594694470057))
REPRESENTATION_ITEM('')
);
#19455=(
BOUNDED_CURVE()
B_SPLINE_CURVE(2,(#79118,#79119,#79120),.UNSPECIFIED.,.F.,.F.)
B_SPLINE_CURVE_WITH_KNOTS((3,3),(0.0728598738456803,0.164428174992088),
 .UNSPECIFIED.)
CURVE()
GEOMETRIC_REPRESENTATION_ITEM()
RATIONAL_B_SPLINE_CURVE((1.0000442203771,1.00004989767014,1.))
REPRESENTATION_ITEM('')
);
#19456=(
BOUNDED_CURVE()
B_SPLINE_CURVE(2,(#79131,#79132,#79133),.UNSPECIFIED.,.F.,.F.)
B_SPLINE_CURVE_WITH_KNOTS((3,3),(0.526544758504326,0.808610241550336),
 .UNSPECIFIED.)
CURVE()
GEOMETRIC_REPRESENTATION_ITEM()
RATIONAL_B_SPLINE_CURVE((1.00594694470058,1.00650257927329,1.00594694470058))
REPRESENTATION_ITEM('')
);
#19457=(
BOUNDED_CURVE()
B_SPLINE_CURVE(2,(#79138,#79139,#79140),.UNSPECIFIED.,.F.,.F.)
B_SPLINE_CURVE_WITH_KNOTS((3,3),(0.0728598743728024,0.164428174992087),
 .UNSPECIFIED.)
CURVE()
GEOMETRIC_REPRESENTATION_ITEM()
RATIONAL_B_SPLINE_CURVE((1.00004421963814,1.00004989683596,1.))
REPRESENTATION_ITEM('')
);
#19458=(
BOUNDED_CURVE()
B_SPLINE_CURVE(2,(#79151,#79152,#79153),.UNSPECIFIED.,.F.,.F.)
B_SPLINE_CURVE_WITH_KNOTS((3,3),(0.526544758504329,0.808610241550345),
 .UNSPECIFIED.)
CURVE()
GEOMETRIC_REPRESENTATION_ITEM()
RATIONAL_B_SPLINE_CURVE((1.0059469447006,1.00650257927331,1.0059469447006))
REPRESENTATION_ITEM('')
);
#19459=(
BOUNDED_CURVE()
B_SPLINE_CURVE(2,(#79158,#79159,#79160),.UNSPECIFIED.,.F.,.F.)
B_SPLINE_CURVE_WITH_KNOTS((3,3),(0.0728598738250905,0.164428174992087),
 .UNSPECIFIED.)
CURVE()
GEOMETRIC_REPRESENTATION_ITEM()
RATIONAL_B_SPLINE_CURVE((1.00004422075857,1.0000498981006,1.))
REPRESENTATION_ITEM('')
);
#19460=(
BOUNDED_CURVE()
B_SPLINE_CURVE(2,(#79171,#79172,#79173),.UNSPECIFIED.,.F.,.F.)
B_SPLINE_CURVE_WITH_KNOTS((3,3),(0.526544758504326,0.808610241550335),
 .UNSPECIFIED.)
CURVE()
GEOMETRIC_REPRESENTATION_ITEM()
RATIONAL_B_SPLINE_CURVE((1.00594694470058,1.00650257927329,1.00594694470058))
REPRESENTATION_ITEM('')
);
#19461=(
BOUNDED_CURVE()
B_SPLINE_CURVE(2,(#79178,#79179,#79180),.UNSPECIFIED.,.F.,.F.)
B_SPLINE_CURVE_WITH_KNOTS((3,3),(0.0728598725540691,0.164428174992087),
 .UNSPECIFIED.)
CURVE()
GEOMETRIC_REPRESENTATION_ITEM()
RATIONAL_B_SPLINE_CURVE((1.00004422004749,1.00004989729911,1.))
REPRESENTATION_ITEM('')
);
#19462=(
BOUNDED_CURVE()
B_SPLINE_CURVE(2,(#79191,#79192,#79193),.UNSPECIFIED.,.F.,.F.)
B_SPLINE_CURVE_WITH_KNOTS((3,3),(0.526544758504315,0.808610241550331),
 .UNSPECIFIED.)
CURVE()
GEOMETRIC_REPRESENTATION_ITEM()
RATIONAL_B_SPLINE_CURVE((1.0059469447006,1.00650257927331,1.0059469447006))
REPRESENTATION_ITEM('')
);
#19463=(
BOUNDED_CURVE()
B_SPLINE_CURVE(2,(#79198,#79199,#79200),.UNSPECIFIED.,.F.,.F.)
B_SPLINE_CURVE_WITH_KNOTS((3,3),(0.0728598737482156,0.164428174992087),
 .UNSPECIFIED.)
CURVE()
GEOMETRIC_REPRESENTATION_ITEM()
RATIONAL_B_SPLINE_CURVE((1.00004421992039,1.00004989715487,1.))
REPRESENTATION_ITEM('')
);
#19464=(
BOUNDED_CURVE()
B_SPLINE_CURVE(2,(#79211,#79212,#79213),.UNSPECIFIED.,.F.,.F.)
B_SPLINE_CURVE_WITH_KNOTS((3,3),(0.52654475850433,0.808610241550342),
 .UNSPECIFIED.)
CURVE()
GEOMETRIC_REPRESENTATION_ITEM()
RATIONAL_B_SPLINE_CURVE((1.00594694470058,1.0065025792733,1.00594694470058))
REPRESENTATION_ITEM('')
);
#19465=(
BOUNDED_CURVE()
B_SPLINE_CURVE(2,(#79218,#79219,#79220),.UNSPECIFIED.,.F.,.F.)
B_SPLINE_CURVE_WITH_KNOTS((3,3),(0.07285987336842,0.164428174992087),
 .UNSPECIFIED.)
CURVE()
GEOMETRIC_REPRESENTATION_ITEM()
RATIONAL_B_SPLINE_CURVE((1.00004422018813,1.00004989745724,1.))
REPRESENTATION_ITEM('')
);
#19466=(
BOUNDED_CURVE()
B_SPLINE_CURVE(2,(#79231,#79232,#79233),.UNSPECIFIED.,.F.,.F.)
B_SPLINE_CURVE_WITH_KNOTS((3,3),(0.526544758504316,0.808610241550331),
 .UNSPECIFIED.)
CURVE()
GEOMETRIC_REPRESENTATION_ITEM()
RATIONAL_B_SPLINE_CURVE((1.0059469447006,1.00650257927331,1.0059469447006))
REPRESENTATION_ITEM('')
);
#19467=(
BOUNDED_CURVE()
B_SPLINE_CURVE(2,(#79238,#79239,#79240),.UNSPECIFIED.,.F.,.F.)
B_SPLINE_CURVE_WITH_KNOTS((3,3),(0.0728598727455658,0.164428174992087),
 .UNSPECIFIED.)
CURVE()
GEOMETRIC_REPRESENTATION_ITEM()
RATIONAL_B_SPLINE_CURVE((1.00004422062249,1.00004989794779,1.))
REPRESENTATION_ITEM('')
);
#19468=(
BOUNDED_CURVE()
B_SPLINE_CURVE(2,(#79251,#79252,#79253),.UNSPECIFIED.,.F.,.F.)
B_SPLINE_CURVE_WITH_KNOTS((3,3),(0.526544758504326,0.808610241550338),
 .UNSPECIFIED.)
CURVE()
GEOMETRIC_REPRESENTATION_ITEM()
RATIONAL_B_SPLINE_CURVE((1.00594694470059,1.0065025792733,1.00594694470059))
REPRESENTATION_ITEM('')
);
#19469=(
BOUNDED_CURVE()
B_SPLINE_CURVE(2,(#79258,#79259,#79260),.UNSPECIFIED.,.F.,.F.)
B_SPLINE_CURVE_WITH_KNOTS((3,3),(0.0728598739743273,0.164428174992087),
 .UNSPECIFIED.)
CURVE()
GEOMETRIC_REPRESENTATION_ITEM()
RATIONAL_B_SPLINE_CURVE((1.00004421975389,1.00004989696683,1.))
REPRESENTATION_ITEM('')
);
#19470=(
BOUNDED_CURVE()
B_SPLINE_CURVE(2,(#79271,#79272,#79273),.UNSPECIFIED.,.F.,.F.)
B_SPLINE_CURVE_WITH_KNOTS((3,3),(0.52654475850433,0.808610241550343),
 .UNSPECIFIED.)
CURVE()
GEOMETRIC_REPRESENTATION_ITEM()
RATIONAL_B_SPLINE_CURVE((1.00594694470059,1.0065025792733,1.00594694470059))
REPRESENTATION_ITEM('')
);
#19471=(
BOUNDED_CURVE()
B_SPLINE_CURVE(2,(#79278,#79279,#79280),.UNSPECIFIED.,.F.,.F.)
B_SPLINE_CURVE_WITH_KNOTS((3,3),(0.0728598738465884,0.164428174992087),
 .UNSPECIFIED.)
CURVE()
GEOMETRIC_REPRESENTATION_ITEM()
RATIONAL_B_SPLINE_CURVE((1.0000442201497,1.00004989741356,1.))
REPRESENTATION_ITEM('')
);
#19472=(
BOUNDED_CURVE()
B_SPLINE_CURVE(2,(#79291,#79292,#79293),.UNSPECIFIED.,.F.,.F.)
B_SPLINE_CURVE_WITH_KNOTS((3,3),(0.526544758504314,0.80861024155033),
 .UNSPECIFIED.)
CURVE()
GEOMETRIC_REPRESENTATION_ITEM()
RATIONAL_B_SPLINE_CURVE((1.0059469447006,1.00650257927332,1.0059469447006))
REPRESENTATION_ITEM('')
);
#19473=(
BOUNDED_CURVE()
B_SPLINE_CURVE(2,(#79298,#79299,#79300),.UNSPECIFIED.,.F.,.F.)
B_SPLINE_CURVE_WITH_KNOTS((3,3),(0.0728598743812492,0.164428174992087),
 .UNSPECIFIED.)
CURVE()
GEOMETRIC_REPRESENTATION_ITEM()
RATIONAL_B_SPLINE_CURVE((1.00004422004264,1.00004989729238,1.))
REPRESENTATION_ITEM('')
);
#19474=(
BOUNDED_CURVE()
B_SPLINE_CURVE(2,(#79311,#79312,#79313),.UNSPECIFIED.,.F.,.F.)
B_SPLINE_CURVE_WITH_KNOTS((3,3),(0.526544758504329,0.808610241550345),
 .UNSPECIFIED.)
CURVE()
GEOMETRIC_REPRESENTATION_ITEM()
RATIONAL_B_SPLINE_CURVE((1.0059469447006,1.00650257927331,1.0059469447006))
REPRESENTATION_ITEM('')
);
#19475=(
BOUNDED_CURVE()
B_SPLINE_CURVE(2,(#79318,#79319,#79320),.UNSPECIFIED.,.F.,.F.)
B_SPLINE_CURVE_WITH_KNOTS((3,3),(0.0728598751562594,0.164428174992087),
 .UNSPECIFIED.)
CURVE()
GEOMETRIC_REPRESENTATION_ITEM()
RATIONAL_B_SPLINE_CURVE((1.00004421953408,1.000049896718,1.))
REPRESENTATION_ITEM('')
);
#19476=(
BOUNDED_CURVE()
B_SPLINE_CURVE(2,(#79331,#79332,#79333),.UNSPECIFIED.,.F.,.F.)
B_SPLINE_CURVE_WITH_KNOTS((3,3),(0.526544758504326,0.808610241550335),
 .UNSPECIFIED.)
CURVE()
GEOMETRIC_REPRESENTATION_ITEM()
RATIONAL_B_SPLINE_CURVE((1.00594694470057,1.00650257927328,1.00594694470057))
REPRESENTATION_ITEM('')
);
#19477=(
BOUNDED_CURVE()
B_SPLINE_CURVE(2,(#79338,#79339,#79340),.UNSPECIFIED.,.F.,.F.)
B_SPLINE_CURVE_WITH_KNOTS((3,3),(0.0728598745734469,0.164428174992087),
 .UNSPECIFIED.)
CURVE()
GEOMETRIC_REPRESENTATION_ITEM()
RATIONAL_B_SPLINE_CURVE((1.00004421949713,1.0000498966767,1.))
REPRESENTATION_ITEM('')
);
#19478=(
BOUNDED_CURVE()
B_SPLINE_CURVE(2,(#79351,#79352,#79353),.UNSPECIFIED.,.F.,.F.)
B_SPLINE_CURVE_WITH_KNOTS((3,3),(0.526544758504326,0.808610241550333),
 .UNSPECIFIED.)
CURVE()
GEOMETRIC_REPRESENTATION_ITEM()
RATIONAL_B_SPLINE_CURVE((1.00594694470057,1.00650257927328,1.00594694470057))
REPRESENTATION_ITEM('')
);
#19479=(
BOUNDED_CURVE()
B_SPLINE_CURVE(2,(#79358,#79359,#79360),.UNSPECIFIED.,.F.,.F.)
B_SPLINE_CURVE_WITH_KNOTS((3,3),(0.0728598743491898,0.164428174992087),
 .UNSPECIFIED.)
CURVE()
GEOMETRIC_REPRESENTATION_ITEM()
RATIONAL_B_SPLINE_CURVE((1.00004421963837,1.00004989683623,1.))
REPRESENTATION_ITEM('')
);
#19480=(
BOUNDED_CURVE()
B_SPLINE_CURVE(2,(#79371,#79372,#79373),.UNSPECIFIED.,.F.,.F.)
B_SPLINE_CURVE_WITH_KNOTS((3,3),(0.526544758504326,0.808610241550337),
 .UNSPECIFIED.)
CURVE()
GEOMETRIC_REPRESENTATION_ITEM()
RATIONAL_B_SPLINE_CURVE((1.00594694470058,1.0065025792733,1.00594694470058))
REPRESENTATION_ITEM('')
);
#19481=(
BOUNDED_CURVE()
B_SPLINE_CURVE(2,(#79378,#79379,#79380),.UNSPECIFIED.,.F.,.F.)
B_SPLINE_CURVE_WITH_KNOTS((3,3),(0.0728598737483212,0.164428174992087),
 .UNSPECIFIED.)
CURVE()
GEOMETRIC_REPRESENTATION_ITEM()
RATIONAL_B_SPLINE_CURVE((1.00004421992501,1.00004989716008,1.))
REPRESENTATION_ITEM('')
);
#19482=(
BOUNDED_CURVE()
B_SPLINE_CURVE(2,(#79391,#79392,#79393),.UNSPECIFIED.,.F.,.F.)
B_SPLINE_CURVE_WITH_KNOTS((3,3),(0.526544758504331,0.808610241550341),
 .UNSPECIFIED.)
CURVE()
GEOMETRIC_REPRESENTATION_ITEM()
RATIONAL_B_SPLINE_CURVE((1.00594694470057,1.00650257927329,1.00594694470057))
REPRESENTATION_ITEM('')
);
#19483=(
BOUNDED_CURVE()
B_SPLINE_CURVE(2,(#79398,#79399,#79400),.UNSPECIFIED.,.F.,.F.)
B_SPLINE_CURVE_WITH_KNOTS((3,3),(0.0728598731298684,0.164428174992087),
 .UNSPECIFIED.)
CURVE()
GEOMETRIC_REPRESENTATION_ITEM()
RATIONAL_B_SPLINE_CURVE((1.00004422024797,1.00004989752493,1.))
REPRESENTATION_ITEM('')
);
#19484=(
BOUNDED_CURVE()
B_SPLINE_CURVE(2,(#79411,#79412,#79413),.UNSPECIFIED.,.F.,.F.)
B_SPLINE_CURVE_WITH_KNOTS((3,3),(0.526544758504314,0.80861024155033),
 .UNSPECIFIED.)
CURVE()
GEOMETRIC_REPRESENTATION_ITEM()
RATIONAL_B_SPLINE_CURVE((1.0059469447006,1.00650257927331,1.0059469447006))
REPRESENTATION_ITEM('')
);
#19485=(
BOUNDED_CURVE()
B_SPLINE_CURVE(2,(#79418,#79419,#79420),.UNSPECIFIED.,.F.,.F.)
B_SPLINE_CURVE_WITH_KNOTS((3,3),(0.0728598731596,0.164428174992087),
 .UNSPECIFIED.)
CURVE()
GEOMETRIC_REPRESENTATION_ITEM()
RATIONAL_B_SPLINE_CURVE((1.00004421993844,1.00004989717563,1.))
REPRESENTATION_ITEM('')
);
#19486=(
BOUNDED_CURVE()
B_SPLINE_CURVE(2,(#79431,#79432,#79433),.UNSPECIFIED.,.F.,.F.)
B_SPLINE_CURVE_WITH_KNOTS((3,3),(0.526544758504325,0.808610241550336),
 .UNSPECIFIED.)
CURVE()
GEOMETRIC_REPRESENTATION_ITEM()
RATIONAL_B_SPLINE_CURVE((1.00594694470058,1.00650257927329,1.00594694470058))
REPRESENTATION_ITEM('')
);
#19487=(
BOUNDED_CURVE()
B_SPLINE_CURVE(2,(#79438,#79439,#79440),.UNSPECIFIED.,.F.,.F.)
B_SPLINE_CURVE_WITH_KNOTS((3,3),(0.0728598731840463,0.164428174992087),
 .UNSPECIFIED.)
CURVE()
GEOMETRIC_REPRESENTATION_ITEM()
RATIONAL_B_SPLINE_CURVE((1.00004422050293,1.00004989781259,1.))
REPRESENTATION_ITEM('')
);
#19488=(
BOUNDED_CURVE()
B_SPLINE_CURVE(2,(#79451,#79452,#79453),.UNSPECIFIED.,.F.,.F.)
B_SPLINE_CURVE_WITH_KNOTS((3,3),(0.526544758504328,0.808610241550335),
 .UNSPECIFIED.)
CURVE()
GEOMETRIC_REPRESENTATION_ITEM()
RATIONAL_B_SPLINE_CURVE((1.00594694470057,1.00650257927328,1.00594694470057))
REPRESENTATION_ITEM('')
);
#19489=(
BOUNDED_CURVE()
B_SPLINE_CURVE(2,(#79458,#79459,#79460),.UNSPECIFIED.,.F.,.F.)
B_SPLINE_CURVE_WITH_KNOTS((3,3),(0.0728598743730364,0.164428174992087),
 .UNSPECIFIED.)
CURVE()
GEOMETRIC_REPRESENTATION_ITEM()
RATIONAL_B_SPLINE_CURVE((1.00004421961452,1.0000498968093,1.))
REPRESENTATION_ITEM('')
);
#19490=(
BOUNDED_CURVE()
B_SPLINE_CURVE(2,(#79471,#79472,#79473),.UNSPECIFIED.,.F.,.F.)
B_SPLINE_CURVE_WITH_KNOTS((3,3),(0.526544758504321,0.80861024155034),
 .UNSPECIFIED.)
CURVE()
GEOMETRIC_REPRESENTATION_ITEM()
RATIONAL_B_SPLINE_CURVE((1.00594694470061,1.00650257927332,1.00594694470061))
REPRESENTATION_ITEM('')
);
#19491=(
BOUNDED_CURVE()
B_SPLINE_CURVE(2,(#79478,#79479,#79480),.UNSPECIFIED.,.F.,.F.)
B_SPLINE_CURVE_WITH_KNOTS((3,3),(0.0728598738321962,0.164428174992087),
 .UNSPECIFIED.)
CURVE()
GEOMETRIC_REPRESENTATION_ITEM()
RATIONAL_B_SPLINE_CURVE((1.00004422004048,1.00004989729031,1.))
REPRESENTATION_ITEM('')
);
#19492=(
BOUNDED_CURVE()
B_SPLINE_CURVE(2,(#79491,#79492,#79493),.UNSPECIFIED.,.F.,.F.)
B_SPLINE_CURVE_WITH_KNOTS((3,3),(0.526544758504326,0.808610241550336),
 .UNSPECIFIED.)
CURVE()
GEOMETRIC_REPRESENTATION_ITEM()
RATIONAL_B_SPLINE_CURVE((1.00594694470058,1.00650257927329,1.00594694470058))
REPRESENTATION_ITEM('')
);
#19493=(
BOUNDED_CURVE()
B_SPLINE_CURVE(2,(#79498,#79499,#79500),.UNSPECIFIED.,.F.,.F.)
B_SPLINE_CURVE_WITH_KNOTS((3,3),(0.0728598739247914,0.164428174992087),
 .UNSPECIFIED.)
CURVE()
GEOMETRIC_REPRESENTATION_ITEM()
RATIONAL_B_SPLINE_CURVE((1.00004422012998,1.00004989739124,1.))
REPRESENTATION_ITEM('')
);
#19494=(
BOUNDED_CURVE()
B_SPLINE_CURVE(2,(#79511,#79512,#79513),.UNSPECIFIED.,.F.,.F.)
B_SPLINE_CURVE_WITH_KNOTS((3,3),(0.526544758504326,0.808610241550334),
 .UNSPECIFIED.)
CURVE()
GEOMETRIC_REPRESENTATION_ITEM()
RATIONAL_B_SPLINE_CURVE((1.00594694470057,1.00650257927328,1.00594694470057))
REPRESENTATION_ITEM('')
);
#19495=(
BOUNDED_CURVE()
B_SPLINE_CURVE(2,(#79518,#79519,#79520),.UNSPECIFIED.,.F.,.F.)
B_SPLINE_CURVE_WITH_KNOTS((3,3),(0.0728598736288243,0.164428174992087),
 .UNSPECIFIED.)
CURVE()
GEOMETRIC_REPRESENTATION_ITEM()
RATIONAL_B_SPLINE_CURVE((1.00004422053539,1.00004989784891,1.))
REPRESENTATION_ITEM('')
);
#19496=(
BOUNDED_CURVE()
B_SPLINE_CURVE(2,(#79531,#79532,#79533),.UNSPECIFIED.,.F.,.F.)
B_SPLINE_CURVE_WITH_KNOTS((3,3),(0.526544758504324,0.808610241550337),
 .UNSPECIFIED.)
CURVE()
GEOMETRIC_REPRESENTATION_ITEM()
RATIONAL_B_SPLINE_CURVE((1.00594694470059,1.0065025792733,1.00594694470059))
REPRESENTATION_ITEM('')
);
#19497=(
BOUNDED_CURVE()
B_SPLINE_CURVE(2,(#79538,#79539,#79540),.UNSPECIFIED.,.F.,.F.)
B_SPLINE_CURVE_WITH_KNOTS((3,3),(0.0728598730615147,0.164428174992087),
 .UNSPECIFIED.)
CURVE()
GEOMETRIC_REPRESENTATION_ITEM()
RATIONAL_B_SPLINE_CURVE((1.00004422030862,1.00004989759341,1.))
REPRESENTATION_ITEM('')
);
#19498=(
BOUNDED_CURVE()
B_SPLINE_CURVE(2,(#79551,#79552,#79553),.UNSPECIFIED.,.F.,.F.)
B_SPLINE_CURVE_WITH_KNOTS((3,3),(0.526544758504332,0.808610241550341),
 .UNSPECIFIED.)
CURVE()
GEOMETRIC_REPRESENTATION_ITEM()
RATIONAL_B_SPLINE_CURVE((1.00594694470057,1.00650257927329,1.00594694470057))
REPRESENTATION_ITEM('')
);
#19499=(
BOUNDED_CURVE()
B_SPLINE_CURVE(2,(#79558,#79559,#79560),.UNSPECIFIED.,.F.,.F.)
B_SPLINE_CURVE_WITH_KNOTS((3,3),(0.07285987336842,0.164428174992087),
 .UNSPECIFIED.)
CURVE()
GEOMETRIC_REPRESENTATION_ITEM()
RATIONAL_B_SPLINE_CURVE((1.00004422018813,1.00004989745724,1.))
REPRESENTATION_ITEM('')
);
#19500=(
BOUNDED_CURVE()
B_SPLINE_CURVE(2,(#79571,#79572,#79573),.UNSPECIFIED.,.F.,.F.)
B_SPLINE_CURVE_WITH_KNOTS((3,3),(0.526544758504316,0.808610241550331),
 .UNSPECIFIED.)
CURVE()
GEOMETRIC_REPRESENTATION_ITEM()
RATIONAL_B_SPLINE_CURVE((1.0059469447006,1.00650257927331,1.0059469447006))
REPRESENTATION_ITEM('')
);
#19501=(
BOUNDED_CURVE()
B_SPLINE_CURVE(2,(#79578,#79579,#79580),.UNSPECIFIED.,.F.,.F.)
B_SPLINE_CURVE_WITH_KNOTS((3,3),(0.0728598741162188,0.164428174992087),
 .UNSPECIFIED.)
CURVE()
GEOMETRIC_REPRESENTATION_ITEM()
RATIONAL_B_SPLINE_CURVE((1.00004421986125,1.00004989708788,1.))
REPRESENTATION_ITEM('')
);
#19502=(
BOUNDED_CURVE()
B_SPLINE_CURVE(2,(#79591,#79592,#79593),.UNSPECIFIED.,.F.,.F.)
B_SPLINE_CURVE_WITH_KNOTS((3,3),(0.526544758504326,0.808610241550337),
 .UNSPECIFIED.)
CURVE()
GEOMETRIC_REPRESENTATION_ITEM()
RATIONAL_B_SPLINE_CURVE((1.00594694470058,1.00650257927329,1.00594694470058))
REPRESENTATION_ITEM('')
);
#19503=(
BOUNDED_CURVE()
B_SPLINE_CURVE(2,(#79598,#79599,#79600),.UNSPECIFIED.,.F.,.F.)
B_SPLINE_CURVE_WITH_KNOTS((3,3),(0.0728598752298607,0.164428174992087),
 .UNSPECIFIED.)
CURVE()
GEOMETRIC_REPRESENTATION_ITEM()
RATIONAL_B_SPLINE_CURVE((1.00004421980288,1.00004989702126,1.))
REPRESENTATION_ITEM('')
);
#19504=(
BOUNDED_CURVE()
B_SPLINE_CURVE(2,(#79611,#79612,#79613),.UNSPECIFIED.,.F.,.F.)
B_SPLINE_CURVE_WITH_KNOTS((3,3),(0.526544758504327,0.808610241550334),
 .UNSPECIFIED.)
CURVE()
GEOMETRIC_REPRESENTATION_ITEM()
RATIONAL_B_SPLINE_CURVE((1.00594694470057,1.00650257927328,1.00594694470057))
REPRESENTATION_ITEM('')
);
#19505=(
BOUNDED_CURVE()
B_SPLINE_CURVE(2,(#79618,#79619,#79620),.UNSPECIFIED.,.F.,.F.)
B_SPLINE_CURVE_WITH_KNOTS((3,3),(0.0728598738446078,0.164428174992087),
 .UNSPECIFIED.)
CURVE()
GEOMETRIC_REPRESENTATION_ITEM()
RATIONAL_B_SPLINE_CURVE((1.00004422018383,1.00004989745207,1.))
REPRESENTATION_ITEM('')
);
#19506=(
BOUNDED_CURVE()
B_SPLINE_CURVE(2,(#79631,#79632,#79633),.UNSPECIFIED.,.F.,.F.)
B_SPLINE_CURVE_WITH_KNOTS((3,3),(0.526544758504328,0.808610241550334),
 .UNSPECIFIED.)
CURVE()
GEOMETRIC_REPRESENTATION_ITEM()
RATIONAL_B_SPLINE_CURVE((1.00594694470057,1.00650257927328,1.00594694470057))
REPRESENTATION_ITEM('')
);
#19507=(
BOUNDED_CURVE()
B_SPLINE_CURVE(2,(#79636,#79637,#79638),.UNSPECIFIED.,.F.,.F.)
B_SPLINE_CURVE_WITH_KNOTS((3,3),(0.,0.0915683004209703),.UNSPECIFIED.)
CURVE()
GEOMETRIC_REPRESENTATION_ITEM()
RATIONAL_B_SPLINE_CURVE((1.,1.00004989694773,1.00004421973732))
REPRESENTATION_ITEM('')
);
#19508=(
BOUNDED_CURVE()
B_SPLINE_CURVE(2,(#79642,#79643,#79644),.UNSPECIFIED.,.F.,.F.)
B_SPLINE_CURVE_WITH_KNOTS((3,3),(0.,0.0915683013231767),.UNSPECIFIED.)
CURVE()
GEOMETRIC_REPRESENTATION_ITEM()
RATIONAL_B_SPLINE_CURVE((1.,1.00004989713748,1.00004421990493))
REPRESENTATION_ITEM('')
);
#19509=(
BOUNDED_CURVE()
B_SPLINE_CURVE(2,(#79648,#79649,#79650),.UNSPECIFIED.,.F.,.F.)
B_SPLINE_CURVE_WITH_KNOTS((3,3),(0.,0.0915683016069819),.UNSPECIFIED.)
CURVE()
GEOMETRIC_REPRESENTATION_ITEM()
RATIONAL_B_SPLINE_CURVE((1.,1.00004989745717,1.00004422018807))
REPRESENTATION_ITEM('')
);
#19510=(
BOUNDED_CURVE()
B_SPLINE_CURVE(2,(#79654,#79655,#79656),.UNSPECIFIED.,.F.,.F.)
B_SPLINE_CURVE_WITH_KNOTS((3,3),(0.,0.0915683018592699),.UNSPECIFIED.)
CURVE()
GEOMETRIC_REPRESENTATION_ITEM()
RATIONAL_B_SPLINE_CURVE((1.,1.00004989730699,1.00004422005483))
REPRESENTATION_ITEM('')
);
#19511=(
BOUNDED_CURVE()
B_SPLINE_CURVE(2,(#79660,#79661,#79662),.UNSPECIFIED.,.F.,.F.)
B_SPLINE_CURVE_WITH_KNOTS((3,3),(0.,0.0915683015335247),.UNSPECIFIED.)
CURVE()
GEOMETRIC_REPRESENTATION_ITEM()
RATIONAL_B_SPLINE_CURVE((1.,1.00004989745986,1.00004422019051))
REPRESENTATION_ITEM('')
);
#19512=(
BOUNDED_CURVE()
B_SPLINE_CURVE(2,(#79666,#79667,#79668),.UNSPECIFIED.,.F.,.F.)
B_SPLINE_CURVE_WITH_KNOTS((3,3),(0.,0.0915683019494071),.UNSPECIFIED.)
CURVE()
GEOMETRIC_REPRESENTATION_ITEM()
RATIONAL_B_SPLINE_CURVE((1.,1.00004989707043,1.00004421984513))
REPRESENTATION_ITEM('')
);
#19513=(
BOUNDED_CURVE()
B_SPLINE_CURVE(2,(#79672,#79673,#79674),.UNSPECIFIED.,.F.,.F.)
B_SPLINE_CURVE_WITH_KNOTS((3,3),(0.,0.0915683011311358),.UNSPECIFIED.)
CURVE()
GEOMETRIC_REPRESENTATION_ITEM()
RATIONAL_B_SPLINE_CURVE((1.,1.00004989683837,1.00004421963997))
REPRESENTATION_ITEM('')
);
#19514=(
BOUNDED_CURVE()
B_SPLINE_CURVE(2,(#79678,#79679,#79680),.UNSPECIFIED.,.F.,.F.)
B_SPLINE_CURVE_WITH_KNOTS((3,3),(0.,0.091568300610644),.UNSPECIFIED.)
CURVE()
GEOMETRIC_REPRESENTATION_ITEM()
RATIONAL_B_SPLINE_CURVE((1.,1.0000498971937,1.00004421995519))
REPRESENTATION_ITEM('')
);
#19515=(
BOUNDED_CURVE()
B_SPLINE_CURVE(2,(#79684,#79685,#79686),.UNSPECIFIED.,.F.,.F.)
B_SPLINE_CURVE_WITH_KNOTS((3,3),(0.,0.0915683011636906),.UNSPECIFIED.)
CURVE()
GEOMETRIC_REPRESENTATION_ITEM()
RATIONAL_B_SPLINE_CURVE((1.,1.00004989770404,1.00004422040713))
REPRESENTATION_ITEM('')
);
#19516=(
BOUNDED_CURVE()
B_SPLINE_CURVE(2,(#79690,#79691,#79692),.UNSPECIFIED.,.F.,.F.)
B_SPLINE_CURVE_WITH_KNOTS((3,3),(0.,0.09156830042059),.UNSPECIFIED.)
CURVE()
GEOMETRIC_REPRESENTATION_ITEM()
RATIONAL_B_SPLINE_CURVE((1.,1.00004989687363,1.00004421967165))
REPRESENTATION_ITEM('')
);
#19517=(
BOUNDED_CURVE()
B_SPLINE_CURVE(2,(#79696,#79697,#79698),.UNSPECIFIED.,.F.,.F.)
B_SPLINE_CURVE_WITH_KNOTS((3,3),(0.,0.0915683014739308),.UNSPECIFIED.)
CURVE()
GEOMETRIC_REPRESENTATION_ITEM()
RATIONAL_B_SPLINE_CURVE((1.,1.00004989729695,1.00004422004617))
REPRESENTATION_ITEM('')
);
#19518=(
BOUNDED_CURVE()
B_SPLINE_CURVE(2,(#79702,#79703,#79704),.UNSPECIFIED.,.F.,.F.)
B_SPLINE_CURVE_WITH_KNOTS((3,3),(0.,0.0915683011482813),.UNSPECIFIED.)
CURVE()
GEOMETRIC_REPRESENTATION_ITEM()
RATIONAL_B_SPLINE_CURVE((1.,1.00004989719406,1.00004421995518))
REPRESENTATION_ITEM('')
);
#19519=(
BOUNDED_CURVE()
B_SPLINE_CURVE(2,(#79708,#79709,#79710),.UNSPECIFIED.,.F.,.F.)
B_SPLINE_CURVE_WITH_KNOTS((3,3),(0.,0.0915683008241534),.UNSPECIFIED.)
CURVE()
GEOMETRIC_REPRESENTATION_ITEM()
RATIONAL_B_SPLINE_CURVE((1.,1.00004989687854,1.00004421967576))
REPRESENTATION_ITEM('')
);
#19520=(
BOUNDED_CURVE()
B_SPLINE_CURVE(2,(#79714,#79715,#79716),.UNSPECIFIED.,.F.,.F.)
B_SPLINE_CURVE_WITH_KNOTS((3,3),(0.,0.0915683018469464),.UNSPECIFIED.)
CURVE()
GEOMETRIC_REPRESENTATION_ITEM()
RATIONAL_B_SPLINE_CURVE((1.,1.00004989759971,1.00004422031425))
REPRESENTATION_ITEM('')
);
#19521=(
BOUNDED_CURVE()
B_SPLINE_CURVE(2,(#79720,#79721,#79722),.UNSPECIFIED.,.F.,.F.)
B_SPLINE_CURVE_WITH_KNOTS((3,3),(0.,0.0915683017817766),.UNSPECIFIED.)
CURVE()
GEOMETRIC_REPRESENTATION_ITEM()
RATIONAL_B_SPLINE_CURVE((1.,1.0000498971653,1.00004421992931))
REPRESENTATION_ITEM('')
);
#19522=(
BOUNDED_CURVE()
B_SPLINE_CURVE(2,(#79726,#79727,#79728),.UNSPECIFIED.,.F.,.F.)
B_SPLINE_CURVE_WITH_KNOTS((3,3),(0.,0.0915683006548595),.UNSPECIFIED.)
CURVE()
GEOMETRIC_REPRESENTATION_ITEM()
RATIONAL_B_SPLINE_CURVE((1.,1.0000498974359,1.0000442201698))
REPRESENTATION_ITEM('')
);
#19523=(
BOUNDED_CURVE()
B_SPLINE_CURVE(2,(#79732,#79733,#79734),.UNSPECIFIED.,.F.,.F.)
B_SPLINE_CURVE_WITH_KNOTS((3,3),(0.,0.0915683004665198),.UNSPECIFIED.)
CURVE()
GEOMETRIC_REPRESENTATION_ITEM()
RATIONAL_B_SPLINE_CURVE((1.,1.00004989714855,1.00004421991526))
REPRESENTATION_ITEM('')
);
#19524=(
BOUNDED_CURVE()
B_SPLINE_CURVE(2,(#79738,#79739,#79740),.UNSPECIFIED.,.F.,.F.)
B_SPLINE_CURVE_WITH_KNOTS((3,3),(0.,0.0915683004318276),.UNSPECIFIED.)
CURVE()
GEOMETRIC_REPRESENTATION_ITEM()
RATIONAL_B_SPLINE_CURVE((1.,1.00004989712855,1.00004421989756))
REPRESENTATION_ITEM('')
);
#19525=(
BOUNDED_CURVE()
B_SPLINE_CURVE(2,(#79744,#79745,#79746),.UNSPECIFIED.,.F.,.F.)
B_SPLINE_CURVE_WITH_KNOTS((3,3),(0.,0.0915683013234486),.UNSPECIFIED.)
CURVE()
GEOMETRIC_REPRESENTATION_ITEM()
RATIONAL_B_SPLINE_CURVE((1.,1.00004989715502,1.00004421992048))
REPRESENTATION_ITEM('')
);
#19526=(
BOUNDED_CURVE()
B_SPLINE_CURVE(2,(#79750,#79751,#79752),.UNSPECIFIED.,.F.,.F.)
B_SPLINE_CURVE_WITH_KNOTS((3,3),(0.,0.0915683014442284),.UNSPECIFIED.)
CURVE()
GEOMETRIC_REPRESENTATION_ITEM()
RATIONAL_B_SPLINE_CURVE((1.,1.00004989755638,1.00004422027609))
REPRESENTATION_ITEM('')
);
#19527=(
BOUNDED_CURVE()
B_SPLINE_CURVE(2,(#79756,#79757,#79758),.UNSPECIFIED.,.F.,.F.)
B_SPLINE_CURVE_WITH_KNOTS((3,3),(0.,0.0915683018592699),.UNSPECIFIED.)
CURVE()
GEOMETRIC_REPRESENTATION_ITEM()
RATIONAL_B_SPLINE_CURVE((1.,1.00004989730699,1.00004422005483))
REPRESENTATION_ITEM('')
);
#19528=(
BOUNDED_CURVE()
B_SPLINE_CURVE(2,(#79762,#79763,#79764),.UNSPECIFIED.,.F.,.F.)
B_SPLINE_CURVE_WITH_KNOTS((3,3),(0.,0.0915683008497595),.UNSPECIFIED.)
CURVE()
GEOMETRIC_REPRESENTATION_ITEM()
RATIONAL_B_SPLINE_CURVE((1.,1.00004989695215,1.00004421974097))
REPRESENTATION_ITEM('')
);
#19529=(
BOUNDED_CURVE()
B_SPLINE_CURVE(2,(#79768,#79769,#79770),.UNSPECIFIED.,.F.,.F.)
B_SPLINE_CURVE_WITH_KNOTS((3,3),(0.,0.0915683018022691),.UNSPECIFIED.)
CURVE()
GEOMETRIC_REPRESENTATION_ITEM()
RATIONAL_B_SPLINE_CURVE((1.,1.00004989750928,1.00004422023414))
REPRESENTATION_ITEM('')
);
#19530=(
BOUNDED_CURVE()
B_SPLINE_CURVE(2,(#79774,#79775,#79776),.UNSPECIFIED.,.F.,.F.)
B_SPLINE_CURVE_WITH_KNOTS((3,3),(0.,0.0915683019430039),.UNSPECIFIED.)
CURVE()
GEOMETRIC_REPRESENTATION_ITEM()
RATIONAL_B_SPLINE_CURVE((1.,1.00004989754698,1.00004422026747))
REPRESENTATION_ITEM('')
);
#19531=(
BOUNDED_CURVE()
B_SPLINE_CURVE(2,(#79780,#79781,#79782),.UNSPECIFIED.,.F.,.F.)
B_SPLINE_CURVE_WITH_KNOTS((3,3),(0.,0.0915683004685661),.UNSPECIFIED.)
CURVE()
GEOMETRIC_REPRESENTATION_ITEM()
RATIONAL_B_SPLINE_CURVE((1.,1.00004989737201,1.0000442201133))
REPRESENTATION_ITEM('')
);
#19532=(
BOUNDED_CURVE()
B_SPLINE_CURVE(2,(#79786,#79787,#79788),.UNSPECIFIED.,.F.,.F.)
B_SPLINE_CURVE_WITH_KNOTS((3,3),(0.,0.0915683004311751),.UNSPECIFIED.)
CURVE()
GEOMETRIC_REPRESENTATION_ITEM()
RATIONAL_B_SPLINE_CURVE((1.,1.00004989703817,1.00004421981746))
REPRESENTATION_ITEM('')
);
#19533=(
BOUNDED_CURVE()
B_SPLINE_CURVE(2,(#79792,#79793,#79794),.UNSPECIFIED.,.F.,.F.)
B_SPLINE_CURVE_WITH_KNOTS((3,3),(0.,0.0915683015082938),.UNSPECIFIED.)
CURVE()
GEOMETRIC_REPRESENTATION_ITEM()
RATIONAL_B_SPLINE_CURVE((1.,1.00004989736684,1.00004422010808))
REPRESENTATION_ITEM('')
);
#19534=(
BOUNDED_CURVE()
B_SPLINE_CURVE(2,(#79798,#79799,#79800),.UNSPECIFIED.,.F.,.F.)
B_SPLINE_CURVE_WITH_KNOTS((3,3),(0.,0.0915683021230445),.UNSPECIFIED.)
CURVE()
GEOMETRIC_REPRESENTATION_ITEM()
RATIONAL_B_SPLINE_CURVE((1.,1.0000498975049,1.00004422023007))
REPRESENTATION_ITEM('')
);
#19535=(
BOUNDED_CURVE()
B_SPLINE_CURVE(2,(#79804,#79805,#79806),.UNSPECIFIED.,.F.,.F.)
B_SPLINE_CURVE_WITH_KNOTS((3,3),(0.,0.0915683025371453),.UNSPECIFIED.)
CURVE()
GEOMETRIC_REPRESENTATION_ITEM()
RATIONAL_B_SPLINE_CURVE((1.,1.00004989764124,1.00004422035064))
REPRESENTATION_ITEM('')
);
#19536=(
BOUNDED_CURVE()
B_SPLINE_CURVE(2,(#79810,#79811,#79812),.UNSPECIFIED.,.F.,.F.)
B_SPLINE_CURVE_WITH_KNOTS((3,3),(0.,0.0915683008645893),.UNSPECIFIED.)
CURVE()
GEOMETRIC_REPRESENTATION_ITEM()
RATIONAL_B_SPLINE_CURVE((1.,1.00004989751924,1.00004422024354))
REPRESENTATION_ITEM('')
);
#19537=(
BOUNDED_CURVE()
B_SPLINE_CURVE(2,(#79816,#79817,#79818),.UNSPECIFIED.,.F.,.F.)
B_SPLINE_CURVE_WITH_KNOTS((3,3),(0.,0.0915683010569264),.UNSPECIFIED.)
CURVE()
GEOMETRIC_REPRESENTATION_ITEM()
RATIONAL_B_SPLINE_CURVE((1.,1.00004989699498,1.00004421977881))
REPRESENTATION_ITEM('')
);
#19538=(
BOUNDED_CURVE()
B_SPLINE_CURVE(2,(#79822,#79823,#79824),.UNSPECIFIED.,.F.,.F.)
B_SPLINE_CURVE_WITH_KNOTS((3,3),(0.,0.0915683011449946),.UNSPECIFIED.)
CURVE()
GEOMETRIC_REPRESENTATION_ITEM()
RATIONAL_B_SPLINE_CURVE((1.,1.00004989725244,1.00004422000692))
REPRESENTATION_ITEM('')
);
#19539=(
BOUNDED_CURVE()
B_SPLINE_CURVE(2,(#79828,#79829,#79830),.UNSPECIFIED.,.F.,.F.)
B_SPLINE_CURVE_WITH_KNOTS((3,3),(0.,0.0915683013065163),.UNSPECIFIED.)
CURVE()
GEOMETRIC_REPRESENTATION_ITEM()
RATIONAL_B_SPLINE_CURVE((1.,1.00004989753082,1.00004422025353))
REPRESENTATION_ITEM('')
);
#19540=(
BOUNDED_CURVE()
B_SPLINE_CURVE(2,(#87418,#87419,#87420),.UNSPECIFIED.,.F.,.F.)
B_SPLINE_CURVE_WITH_KNOTS((3,3),(0.,0.0725293307675455),.UNSPECIFIED.)
CURVE()
GEOMETRIC_REPRESENTATION_ITEM()
RATIONAL_B_SPLINE_CURVE((1.,1.00078463175291,1.))
REPRESENTATION_ITEM('')
);
#19541=(
BOUNDED_CURVE()
B_SPLINE_CURVE(2,(#87424,#87425,#87426),.UNSPECIFIED.,.F.,.F.)
B_SPLINE_CURVE_WITH_KNOTS((3,3),(0.,0.0240722006597559),.UNSPECIFIED.)
CURVE()
GEOMETRIC_REPRESENTATION_ITEM()
RATIONAL_B_SPLINE_CURVE((1.,1.00002397294334,1.))
REPRESENTATION_ITEM('')
);
#19542=(
BOUNDED_CURVE()
B_SPLINE_CURVE(2,(#87430,#87431,#87432),.UNSPECIFIED.,.F.,.F.)
B_SPLINE_CURVE_WITH_KNOTS((3,3),(0.,0.022704443195243),.UNSPECIFIED.)
CURVE()
GEOMETRIC_REPRESENTATION_ITEM()
RATIONAL_B_SPLINE_CURVE((1.,1.00002331266599,1.))
REPRESENTATION_ITEM('')
);
#19543=(
BOUNDED_CURVE()
B_SPLINE_CURVE(2,(#87435,#87436,#87437),.UNSPECIFIED.,.F.,.F.)
B_SPLINE_CURVE_WITH_KNOTS((3,3),(0.,0.0781071789666387),.UNSPECIFIED.)
CURVE()
GEOMETRIC_REPRESENTATION_ITEM()
RATIONAL_B_SPLINE_CURVE((1.,1.00073443968728,1.))
REPRESENTATION_ITEM('')
);
#19544=(
BOUNDED_CURVE()
B_SPLINE_CURVE(2,(#87441,#87442,#87443),.UNSPECIFIED.,.F.,.F.)
B_SPLINE_CURVE_WITH_KNOTS((3,3),(0.,0.0738858532870895),.UNSPECIFIED.)
CURVE()
GEOMETRIC_REPRESENTATION_ITEM()
RATIONAL_B_SPLINE_CURVE((1.,1.00074677418322,1.))
REPRESENTATION_ITEM('')
);
#19545=(
BOUNDED_CURVE()
B_SPLINE_CURVE(2,(#87447,#87448,#87449),.UNSPECIFIED.,.F.,.F.)
B_SPLINE_CURVE_WITH_KNOTS((3,3),(0.,0.0758535488683919),.UNSPECIFIED.)
CURVE()
GEOMETRIC_REPRESENTATION_ITEM()
RATIONAL_B_SPLINE_CURVE((1.,1.00072976064601,1.))
REPRESENTATION_ITEM('')
);
#19546=(
BOUNDED_CURVE()
B_SPLINE_CURVE(2,(#87452,#87453,#87454),.UNSPECIFIED.,.F.,.F.)
B_SPLINE_CURVE_WITH_KNOTS((3,3),(0.,0.0230800535081001),.UNSPECIFIED.)
CURVE()
GEOMETRIC_REPRESENTATION_ITEM()
RATIONAL_B_SPLINE_CURVE((1.,1.0000232977523,1.))
REPRESENTATION_ITEM('')
);
#19547=(
BOUNDED_CURVE()
B_SPLINE_CURVE(2,(#87456,#87457,#87458),.UNSPECIFIED.,.F.,.F.)
B_SPLINE_CURVE_WITH_KNOTS((3,3),(0.,0.0235661439474371),.UNSPECIFIED.)
CURVE()
GEOMETRIC_REPRESENTATION_ITEM()
RATIONAL_B_SPLINE_CURVE((1.,1.00002352982172,1.))
REPRESENTATION_ITEM('')
);
#19548=(
BOUNDED_CURVE()
B_SPLINE_CURVE(2,(#93987,#93988,#93989),.UNSPECIFIED.,.F.,.F.)
B_SPLINE_CURVE_WITH_KNOTS((3,3),(0.0802593534055511,0.873558161927064),
 .UNSPECIFIED.)
CURVE()
GEOMETRIC_REPRESENTATION_ITEM()
RATIONAL_B_SPLINE_CURVE((1.03570012424137,1.19592349106096,1.03570012424137))
REPRESENTATION_ITEM('')
);
#19549=(
BOUNDED_CURVE()
B_SPLINE_CURVE(2,(#93991,#93992,#93993),.UNSPECIFIED.,.F.,.F.)
B_SPLINE_CURVE_WITH_KNOTS((3,3),(0.0802593534055511,0.873558161927064),
 .UNSPECIFIED.)
CURVE()
GEOMETRIC_REPRESENTATION_ITEM()
RATIONAL_B_SPLINE_CURVE((1.03570012424137,1.19592349106096,1.03570012424137))
REPRESENTATION_ITEM('')
);
#19550=(
BOUNDED_CURVE()
B_SPLINE_CURVE(2,(#93995,#93996,#93997),.UNSPECIFIED.,.F.,.F.)
B_SPLINE_CURVE_WITH_KNOTS((3,3),(0.0802593534055514,0.873558161927064),
 .UNSPECIFIED.)
CURVE()
GEOMETRIC_REPRESENTATION_ITEM()
RATIONAL_B_SPLINE_CURVE((1.03570012424137,1.19592349106096,1.03570012424137))
REPRESENTATION_ITEM('')
);
#19551=(
BOUNDED_CURVE()
B_SPLINE_CURVE(2,(#93999,#94000,#94001),.UNSPECIFIED.,.F.,.F.)
B_SPLINE_CURVE_WITH_KNOTS((3,3),(0.0802593534055513,0.873558161927064),
 .UNSPECIFIED.)
CURVE()
GEOMETRIC_REPRESENTATION_ITEM()
RATIONAL_B_SPLINE_CURVE((1.03570012424137,1.19592349106096,1.03570012424137))
REPRESENTATION_ITEM('')
);
#19552=(
BOUNDED_CURVE()
B_SPLINE_CURVE(2,(#94003,#94004,#94005),.UNSPECIFIED.,.F.,.F.)
B_SPLINE_CURVE_WITH_KNOTS((3,3),(0.080259353405551,0.873558161927064),
 .UNSPECIFIED.)
CURVE()
GEOMETRIC_REPRESENTATION_ITEM()
RATIONAL_B_SPLINE_CURVE((1.03570012424137,1.19592349106096,1.03570012424137))
REPRESENTATION_ITEM('')
);
#19553=(
BOUNDED_CURVE()
B_SPLINE_CURVE(2,(#94009,#94010,#94011),.UNSPECIFIED.,.F.,.F.)
B_SPLINE_CURVE_WITH_KNOTS((3,3),(0.0802593534055507,0.873558161927063),
 .UNSPECIFIED.)
CURVE()
GEOMETRIC_REPRESENTATION_ITEM()
RATIONAL_B_SPLINE_CURVE((1.03570012424137,1.19592349106096,1.03570012424137))
REPRESENTATION_ITEM('')
);
#19554=(
BOUNDED_CURVE()
B_SPLINE_CURVE(2,(#94091,#94092,#94093),.UNSPECIFIED.,.F.,.F.)
B_SPLINE_CURVE_WITH_KNOTS((3,3),(0.,0.0721484594100608),.UNSPECIFIED.)
CURVE()
GEOMETRIC_REPRESENTATION_ITEM()
RATIONAL_B_SPLINE_CURVE((1.,1.00124478006548,1.))
REPRESENTATION_ITEM('')
);
#19555=(
BOUNDED_CURVE()
B_SPLINE_CURVE(2,(#94097,#94098,#94099),.UNSPECIFIED.,.F.,.F.)
B_SPLINE_CURVE_WITH_KNOTS((3,3),(0.,0.0242606382665389),.UNSPECIFIED.)
CURVE()
GEOMETRIC_REPRESENTATION_ITEM()
RATIONAL_B_SPLINE_CURVE((1.,1.00003629689575,1.))
REPRESENTATION_ITEM('')
);
#19556=(
BOUNDED_CURVE()
B_SPLINE_CURVE(2,(#94103,#94104,#94105),.UNSPECIFIED.,.F.,.F.)
B_SPLINE_CURVE_WITH_KNOTS((3,3),(0.,0.022659739228849),.UNSPECIFIED.)
CURVE()
GEOMETRIC_REPRESENTATION_ITEM()
RATIONAL_B_SPLINE_CURVE((1.,1.00003502487514,1.))
REPRESENTATION_ITEM('')
);
#19557=(
BOUNDED_CURVE()
B_SPLINE_CURVE(2,(#94109,#94110,#94111),.UNSPECIFIED.,.F.,.F.)
B_SPLINE_CURVE_WITH_KNOTS((3,3),(0.,0.0785853165973684),.UNSPECIFIED.)
CURVE()
GEOMETRIC_REPRESENTATION_ITEM()
RATIONAL_B_SPLINE_CURVE((1.,1.00114268434673,1.))
REPRESENTATION_ITEM('')
);
#19558=(
BOUNDED_CURVE()
B_SPLINE_CURVE(2,(#94116,#94117,#94118),.UNSPECIFIED.,.F.,.F.)
B_SPLINE_CURVE_WITH_KNOTS((3,3),(0.,0.0737421516508094),.UNSPECIFIED.)
CURVE()
GEOMETRIC_REPRESENTATION_ITEM()
RATIONAL_B_SPLINE_CURVE((1.,1.00116107240881,1.))
REPRESENTATION_ITEM('')
);
#19559=(
BOUNDED_CURVE()
B_SPLINE_CURVE(2,(#94122,#94123,#94124),.UNSPECIFIED.,.F.,.F.)
B_SPLINE_CURVE_WITH_KNOTS((3,3),(0.,0.0757335241689913),.UNSPECIFIED.)
CURVE()
GEOMETRIC_REPRESENTATION_ITEM()
RATIONAL_B_SPLINE_CURVE((1.,1.00113125487949,1.))
REPRESENTATION_ITEM('')
);
#19560=(
BOUNDED_CURVE()
B_SPLINE_CURVE(2,(#94127,#94128,#94129),.UNSPECIFIED.,.F.,.F.)
B_SPLINE_CURVE_WITH_KNOTS((3,3),(0.,0.0231191378819049),.UNSPECIFIED.)
CURVE()
GEOMETRIC_REPRESENTATION_ITEM()
RATIONAL_B_SPLINE_CURVE((1.,1.00003499126588,1.))
REPRESENTATION_ITEM('')
);
#19561=(
BOUNDED_CURVE()
B_SPLINE_CURVE(2,(#94131,#94132,#94133),.UNSPECIFIED.,.F.,.F.)
B_SPLINE_CURVE_WITH_KNOTS((3,3),(0.,0.0236194283361202),.UNSPECIFIED.)
CURVE()
GEOMETRIC_REPRESENTATION_ITEM()
RATIONAL_B_SPLINE_CURVE((1.,1.0000353828725,1.))
REPRESENTATION_ITEM('')
);
#19562=(
BOUNDED_CURVE()
B_SPLINE_CURVE(2,(#94172,#94173,#94174),.UNSPECIFIED.,.F.,.F.)
B_SPLINE_CURVE_WITH_KNOTS((3,3),(0.0802593534055512,0.873558161927064),
 .UNSPECIFIED.)
CURVE()
GEOMETRIC_REPRESENTATION_ITEM()
RATIONAL_B_SPLINE_CURVE((1.03570012424137,1.19592349106096,1.03570012424137))
REPRESENTATION_ITEM('')
);
#19563=(
BOUNDED_CURVE()
B_SPLINE_CURVE(2,(#94176,#94177,#94178),.UNSPECIFIED.,.F.,.F.)
B_SPLINE_CURVE_WITH_KNOTS((3,3),(0.0802593534055512,0.873558161927064),
 .UNSPECIFIED.)
CURVE()
GEOMETRIC_REPRESENTATION_ITEM()
RATIONAL_B_SPLINE_CURVE((1.03570012424137,1.19592349106096,1.03570012424137))
REPRESENTATION_ITEM('')
);
#19564=(
BOUNDED_CURVE()
B_SPLINE_CURVE(2,(#94180,#94181,#94182),.UNSPECIFIED.,.F.,.F.)
B_SPLINE_CURVE_WITH_KNOTS((3,3),(0.0802593534055512,0.873558161927064),
 .UNSPECIFIED.)
CURVE()
GEOMETRIC_REPRESENTATION_ITEM()
RATIONAL_B_SPLINE_CURVE((1.03570012424137,1.19592349106096,1.03570012424137))
REPRESENTATION_ITEM('')
);
#19565=(
BOUNDED_CURVE()
B_SPLINE_CURVE(2,(#94184,#94185,#94186),.UNSPECIFIED.,.F.,.F.)
B_SPLINE_CURVE_WITH_KNOTS((3,3),(0.0802593534055512,0.873558161927064),
 .UNSPECIFIED.)
CURVE()
GEOMETRIC_REPRESENTATION_ITEM()
RATIONAL_B_SPLINE_CURVE((1.03570012424137,1.19592349106096,1.03570012424137))
REPRESENTATION_ITEM('')
);
#19566=(
BOUNDED_CURVE()
B_SPLINE_CURVE(2,(#94188,#94189,#94190),.UNSPECIFIED.,.F.,.F.)
B_SPLINE_CURVE_WITH_KNOTS((3,3),(0.0802593534055512,0.873558161927064),
 .UNSPECIFIED.)
CURVE()
GEOMETRIC_REPRESENTATION_ITEM()
RATIONAL_B_SPLINE_CURVE((1.03570012424137,1.19592349106096,1.03570012424137))
REPRESENTATION_ITEM('')
);
#19567=(
BOUNDED_CURVE()
B_SPLINE_CURVE(2,(#94191,#94192,#94193),.UNSPECIFIED.,.F.,.F.)
B_SPLINE_CURVE_WITH_KNOTS((3,3),(0.0802593534055513,0.873558161927064),
 .UNSPECIFIED.)
CURVE()
GEOMETRIC_REPRESENTATION_ITEM()
RATIONAL_B_SPLINE_CURVE((1.03570012424137,1.19592349106096,1.03570012424137))
REPRESENTATION_ITEM('')
);
#19568=(
BOUNDED_CURVE()
B_SPLINE_CURVE(2,(#94198,#94199,#94200),.UNSPECIFIED.,.F.,.F.)
B_SPLINE_CURVE_WITH_KNOTS((3,3),(0.080259353405551,0.873558161927064),
 .UNSPECIFIED.)
CURVE()
GEOMETRIC_REPRESENTATION_ITEM()
RATIONAL_B_SPLINE_CURVE((1.03570012424137,1.19592349106097,1.03570012424137))
REPRESENTATION_ITEM('')
);
#19569=(
BOUNDED_CURVE()
B_SPLINE_CURVE(2,(#94205,#94206,#94207),.UNSPECIFIED.,.F.,.F.)
B_SPLINE_CURVE_WITH_KNOTS((3,3),(0.0802593534055512,0.873558161927064),
 .UNSPECIFIED.)
CURVE()
GEOMETRIC_REPRESENTATION_ITEM()
RATIONAL_B_SPLINE_CURVE((1.03570012424137,1.19592349106096,1.03570012424137))
REPRESENTATION_ITEM('')
);
#19570=(
BOUNDED_CURVE()
B_SPLINE_CURVE(2,(#94211,#94212,#94213),.UNSPECIFIED.,.F.,.F.)
B_SPLINE_CURVE_WITH_KNOTS((3,3),(0.0802593534055513,0.873558161927064),
 .UNSPECIFIED.)
CURVE()
GEOMETRIC_REPRESENTATION_ITEM()
RATIONAL_B_SPLINE_CURVE((1.03570012424137,1.19592349106096,1.03570012424137))
REPRESENTATION_ITEM('')
);
#19571=(
BOUNDED_CURVE()
B_SPLINE_CURVE(2,(#94216,#94217,#94218),.UNSPECIFIED.,.F.,.F.)
B_SPLINE_CURVE_WITH_KNOTS((3,3),(0.0802593534055513,0.873558161927064),
 .UNSPECIFIED.)
CURVE()
GEOMETRIC_REPRESENTATION_ITEM()
RATIONAL_B_SPLINE_CURVE((1.03570012424137,1.19592349106096,1.03570012424137))
REPRESENTATION_ITEM('')
);
#19572=(
BOUNDED_CURVE()
B_SPLINE_CURVE(2,(#94220,#94221,#94222),.UNSPECIFIED.,.F.,.F.)
B_SPLINE_CURVE_WITH_KNOTS((3,3),(0.0802593534055512,0.873558161927064),
 .UNSPECIFIED.)
CURVE()
GEOMETRIC_REPRESENTATION_ITEM()
RATIONAL_B_SPLINE_CURVE((1.03570012424137,1.19592349106096,1.03570012424137))
REPRESENTATION_ITEM('')
);
#19573=(
BOUNDED_CURVE()
B_SPLINE_CURVE(2,(#94226,#94227,#94228),.UNSPECIFIED.,.F.,.F.)
B_SPLINE_CURVE_WITH_KNOTS((3,3),(0.0802593534055509,0.873558161927063),
 .UNSPECIFIED.)
CURVE()
GEOMETRIC_REPRESENTATION_ITEM()
RATIONAL_B_SPLINE_CURVE((1.03570012424137,1.19592349106096,1.03570012424137))
REPRESENTATION_ITEM('')
);
#19574=CIRCLE('',#51190,39.6);
#19575=CIRCLE('',#51192,39.6);
#19576=CIRCLE('',#51194,39.6);
#19577=CIRCLE('',#51196,39.6);
#19578=CIRCLE('',#51198,39.6);
#19579=CIRCLE('',#51200,39.6);
#19580=CIRCLE('',#51202,39.6);
#19581=CIRCLE('',#51204,39.6);
#19582=CIRCLE('',#51206,39.6);
#19583=CIRCLE('',#51208,39.6);
#19584=CIRCLE('',#51210,39.6);
#19585=CIRCLE('',#51212,39.6);
#19586=CIRCLE('',#51214,39.6);
#19587=CIRCLE('',#51216,39.6);
#19588=CIRCLE('',#51218,39.6);
#19589=CIRCLE('',#51220,39.6);
#19590=CIRCLE('',#51222,39.6);
#19591=CIRCLE('',#51224,39.6);
#19592=CIRCLE('',#51226,39.6);
#19593=CIRCLE('',#51228,39.6);
#19594=CIRCLE('',#51230,39.6);
#19595=CIRCLE('',#51232,39.6);
#19596=CIRCLE('',#51234,39.6);
#19597=CIRCLE('',#51236,39.6);
#19598=CIRCLE('',#51238,39.6);
#19599=CIRCLE('',#51240,39.6);
#19600=CIRCLE('',#51242,39.6);
#19601=CIRCLE('',#51244,39.6);
#19602=CIRCLE('',#51246,39.6);
#19603=CIRCLE('',#51248,39.6);
#19604=CIRCLE('',#51250,39.6);
#19605=CIRCLE('',#51252,39.6);
#19606=CIRCLE('',#51254,39.6);
#19607=CIRCLE('',#51256,39.6);
#19608=CIRCLE('',#51258,39.6);
#19609=CIRCLE('',#51260,39.6);
#19610=CIRCLE('',#51370,39.6);
#19611=CIRCLE('',#51372,39.6);
#19612=CIRCLE('',#51374,39.6);
#19613=CIRCLE('',#51376,39.6);
#19614=CIRCLE('',#51378,39.6);
#19615=CIRCLE('',#51380,39.6);
#19616=CIRCLE('',#51382,39.6);
#19617=CIRCLE('',#51384,39.6);
#19618=CIRCLE('',#51386,39.6);
#19619=CIRCLE('',#51388,39.6);
#19620=CIRCLE('',#51390,39.6);
#19621=CIRCLE('',#51392,39.6);
#19622=CIRCLE('',#51394,39.6);
#19623=CIRCLE('',#51396,39.6);
#19624=CIRCLE('',#51398,39.6);
#19625=CIRCLE('',#51400,39.6);
#19626=CIRCLE('',#51402,39.6);
#19627=CIRCLE('',#51404,39.6);
#19628=CIRCLE('',#51406,39.6);
#19629=CIRCLE('',#51408,39.6);
#19630=CIRCLE('',#51410,39.6);
#19631=CIRCLE('',#51412,39.6);
#19632=CIRCLE('',#51414,39.6);
#19633=CIRCLE('',#51416,39.6);
#19634=CIRCLE('',#51418,39.6);
#19635=CIRCLE('',#51420,39.6);
#19636=CIRCLE('',#51422,39.6);
#19637=CIRCLE('',#51424,39.6);
#19638=CIRCLE('',#51426,39.6);
#19639=CIRCLE('',#51428,39.6);
#19640=CIRCLE('',#51430,39.6);
#19641=CIRCLE('',#51432,39.6);
#19642=CIRCLE('',#51434,39.6);
#19643=CIRCLE('',#51436,39.6);
#19644=CIRCLE('',#51438,39.6);
#19645=CIRCLE('',#51440,39.6);
#19646=CIRCLE('',#51742,42.9);
#19647=CIRCLE('',#51743,42.3);
#19648=CIRCLE('',#51744,42.3);
#19649=CIRCLE('',#51745,42.3);
#19650=CIRCLE('',#51746,42.3);
#19651=CIRCLE('',#51747,42.3);
#19652=CIRCLE('',#51748,42.3);
#19653=CIRCLE('',#51749,42.3);
#19654=CIRCLE('',#51750,42.3);
#19655=CIRCLE('',#51751,42.3);
#19656=CIRCLE('',#51752,42.3);
#19657=CIRCLE('',#51753,42.3);
#19658=CIRCLE('',#51754,42.3);
#19659=CIRCLE('',#51755,42.3);
#19660=CIRCLE('',#51756,42.3);
#19661=CIRCLE('',#51757,42.3);
#19662=CIRCLE('',#51758,42.3);
#19663=CIRCLE('',#51759,42.3);
#19664=CIRCLE('',#51760,42.3);
#19665=CIRCLE('',#51761,42.3);
#19666=CIRCLE('',#51762,42.3);
#19667=CIRCLE('',#51763,42.3);
#19668=CIRCLE('',#51764,42.3);
#19669=CIRCLE('',#51765,42.3);
#19670=CIRCLE('',#51766,42.3);
#19671=CIRCLE('',#51767,42.3);
#19672=CIRCLE('',#51768,42.3);
#19673=CIRCLE('',#51769,42.3);
#19674=CIRCLE('',#51770,42.3);
#19675=CIRCLE('',#51771,42.3);
#19676=CIRCLE('',#51772,42.3);
#19677=CIRCLE('',#51773,42.3);
#19678=CIRCLE('',#51774,42.3);
#19679=CIRCLE('',#51775,42.3);
#19680=CIRCLE('',#51776,42.3);
#19681=CIRCLE('',#51777,42.3);
#19682=CIRCLE('',#51778,42.3);
#19683=CIRCLE('',#51780,42.3);
#19684=CIRCLE('',#51831,42.3);
#19685=CIRCLE('',#51882,42.3);
#19686=CIRCLE('',#51933,42.3);
#19687=CIRCLE('',#51984,42.3);
#19688=CIRCLE('',#52035,42.3);
#19689=CIRCLE('',#52086,42.3);
#19690=CIRCLE('',#52137,42.3);
#19691=CIRCLE('',#52188,42.3);
#19692=CIRCLE('',#52239,42.3);
#19693=CIRCLE('',#52290,42.3);
#19694=CIRCLE('',#52341,42.3);
#19695=CIRCLE('',#52392,42.3);
#19696=CIRCLE('',#52443,42.3);
#19697=CIRCLE('',#52494,42.3);
#19698=CIRCLE('',#52545,42.3);
#19699=CIRCLE('',#52596,42.3);
#19700=CIRCLE('',#52647,42.3);
#19701=CIRCLE('',#52698,42.3);
#19702=CIRCLE('',#52749,42.3);
#19703=CIRCLE('',#52800,42.3);
#19704=CIRCLE('',#52851,42.3);
#19705=CIRCLE('',#52902,42.3);
#19706=CIRCLE('',#52953,42.3);
#19707=CIRCLE('',#53004,42.3);
#19708=CIRCLE('',#53055,42.3);
#19709=CIRCLE('',#53106,42.3);
#19710=CIRCLE('',#53157,42.3);
#19711=CIRCLE('',#53208,42.3);
#19712=CIRCLE('',#53259,42.3);
#19713=CIRCLE('',#53310,42.3);
#19714=CIRCLE('',#53361,42.3);
#19715=CIRCLE('',#53412,42.3);
#19716=CIRCLE('',#53463,42.3);
#19717=CIRCLE('',#53514,42.3);
#19718=CIRCLE('',#53566,42.3);
#19719=CIRCLE('',#53567,42.9);
#19720=CIRCLE('',#53569,47.1);
#19721=CIRCLE('',#53570,47.6321401698912);
#19722=CIRCLE('',#53571,47.6321401698912);
#19723=CIRCLE('',#53573,50.6631501381961);
#19724=CIRCLE('',#53574,50.6631501381961);
#19725=CIRCLE('',#53577,6.);
#19726=CIRCLE('',#53578,51.);
#19727=CIRCLE('',#53579,51.);
#19728=CIRCLE('',#53581,51.);
#19729=CIRCLE('',#53583,46.5);
#19730=CIRCLE('',#53584,0.4);
#19731=CIRCLE('',#53585,46.9);
#19732=CIRCLE('',#53586,46.5);
#19733=CIRCLE('',#53588,46.5);
#19734=CIRCLE('',#53589,46.5);
#19735=CIRCLE('',#53591,50.4);
#19736=CIRCLE('',#53593,46.9);
#19737=CIRCLE('',#53594,0.4);
#19738=CIRCLE('',#53596,50.);
#19739=CIRCLE('',#53599,49.7);
#19740=CIRCLE('',#53601,50.5);
#19741=CIRCLE('',#53603,50.5);
#19742=CIRCLE('',#53606,50.4);
#19743=CIRCLE('',#53613,37.8);
#19744=CIRCLE('',#53614,37.8);
#19745=CIRCLE('',#53616,37.3);
#19746=CIRCLE('',#53617,37.8);
#19747=CIRCLE('',#53618,37.8);
#19748=CIRCLE('',#53619,37.8);
#19749=CIRCLE('',#53620,37.8);
#19750=CIRCLE('',#53621,37.8);
#19751=CIRCLE('',#53622,37.8);
#19752=CIRCLE('',#53623,37.8);
#19753=CIRCLE('',#53624,37.8);
#19754=CIRCLE('',#53625,37.8);
#19755=CIRCLE('',#53626,37.8);
#19756=CIRCLE('',#53627,37.8);
#19757=CIRCLE('',#53628,37.8);
#19758=CIRCLE('',#53630,37.3);
#19759=CIRCLE('',#53631,37.3);
#19760=CIRCLE('',#53632,37.3);
#19761=CIRCLE('',#53633,34.);
#19762=CIRCLE('',#53635,37.8);
#19763=CIRCLE('',#53636,37.8);
#19764=CIRCLE('',#53637,37.8);
#19765=CIRCLE('',#53638,37.8);
#19766=CIRCLE('',#53639,37.8);
#19767=CIRCLE('',#53640,37.8);
#19768=CIRCLE('',#53641,37.8);
#19769=CIRCLE('',#53642,37.8);
#19770=CIRCLE('',#53643,37.8);
#19771=CIRCLE('',#53644,37.8);
#19772=CIRCLE('',#53645,37.8);
#19773=CIRCLE('',#53646,37.8);
#19774=CIRCLE('',#53648,37.8);
#19775=CIRCLE('',#53649,37.8);
#19776=CIRCLE('',#53650,37.8);
#19777=CIRCLE('',#53651,37.8);
#19778=CIRCLE('',#53652,37.8);
#19779=CIRCLE('',#53653,37.8);
#19780=CIRCLE('',#53654,37.8);
#19781=CIRCLE('',#53655,37.8);
#19782=CIRCLE('',#53656,37.8);
#19783=CIRCLE('',#53657,37.8);
#19784=CIRCLE('',#53658,37.8);
#19785=CIRCLE('',#53663,37.3);
#19786=CIRCLE('',#53664,37.8);
#19787=CIRCLE('',#53665,37.8);
#19788=CIRCLE('',#53666,37.8);
#19789=CIRCLE('',#53667,37.8);
#19790=CIRCLE('',#53668,37.8);
#19791=CIRCLE('',#53669,37.8);
#19792=CIRCLE('',#53670,37.8);
#19793=CIRCLE('',#53671,37.8);
#19794=CIRCLE('',#53672,37.8);
#19795=CIRCLE('',#53673,37.8);
#19796=CIRCLE('',#53674,37.8);
#19797=CIRCLE('',#53675,37.8);
#19798=CIRCLE('',#53677,37.8);
#19799=CIRCLE('',#53678,37.8);
#19800=CIRCLE('',#53679,37.8);
#19801=CIRCLE('',#53680,37.8);
#19802=CIRCLE('',#53681,37.8);
#19803=CIRCLE('',#53682,37.8);
#19804=CIRCLE('',#53683,37.8);
#19805=CIRCLE('',#53684,37.8);
#19806=CIRCLE('',#53685,37.8);
#19807=CIRCLE('',#53686,37.8);
#19808=CIRCLE('',#53687,37.8);
#19809=CIRCLE('',#53688,37.3);
#19810=CIRCLE('',#53691,37.8);
#19811=CIRCLE('',#53692,37.8);
#19812=CIRCLE('',#53693,37.8);
#19813=CIRCLE('',#53694,37.8);
#19814=CIRCLE('',#53695,37.8);
#19815=CIRCLE('',#53696,37.8);
#19816=CIRCLE('',#53697,37.8);
#19817=CIRCLE('',#53698,37.8);
#19818=CIRCLE('',#53699,37.8);
#19819=CIRCLE('',#53700,37.8);
#19820=CIRCLE('',#53701,37.8);
#19821=CIRCLE('',#53702,37.8);
#19822=CIRCLE('',#53708,41.43);
#19823=CIRCLE('',#53710,41.43);
#19824=CIRCLE('',#53712,41.43);
#19825=CIRCLE('',#53714,41.43);
#19826=CIRCLE('',#53716,41.43);
#19827=CIRCLE('',#53718,41.43);
#19828=CIRCLE('',#53720,41.43);
#19829=CIRCLE('',#53722,41.43);
#19830=CIRCLE('',#53724,41.43);
#19831=CIRCLE('',#53726,41.43);
#19832=CIRCLE('',#53728,41.43);
#19833=CIRCLE('',#53730,41.43);
#19834=CIRCLE('',#53732,41.43);
#19835=CIRCLE('',#53734,41.43);
#19836=CIRCLE('',#53736,41.43);
#19837=CIRCLE('',#53738,41.43);
#19838=CIRCLE('',#53740,41.43);
#19839=CIRCLE('',#53742,41.43);
#19840=CIRCLE('',#53744,41.43);
#19841=CIRCLE('',#53746,41.43);
#19842=CIRCLE('',#53748,41.43);
#19843=CIRCLE('',#53750,41.43);
#19844=CIRCLE('',#53752,41.43);
#19845=CIRCLE('',#53754,41.43);
#19846=CIRCLE('',#53756,41.43);
#19847=CIRCLE('',#53758,41.43);
#19848=CIRCLE('',#53760,41.43);
#19849=CIRCLE('',#53762,41.43);
#19850=CIRCLE('',#53764,41.43);
#19851=CIRCLE('',#53766,41.43);
#19852=CIRCLE('',#53768,41.43);
#19853=CIRCLE('',#53770,41.43);
#19854=CIRCLE('',#53772,41.43);
#19855=CIRCLE('',#53840,41.43);
#19856=CIRCLE('',#53842,41.43);
#19857=CIRCLE('',#53844,41.43);
#19858=CIRCLE('',#53846,41.43);
#19859=CIRCLE('',#53848,41.43);
#19860=CIRCLE('',#53850,41.43);
#19861=CIRCLE('',#53852,41.43);
#19862=CIRCLE('',#53854,41.43);
#19863=CIRCLE('',#53856,41.43);
#19864=CIRCLE('',#53858,41.43);
#19865=CIRCLE('',#53860,41.43);
#19866=CIRCLE('',#53862,41.43);
#19867=CIRCLE('',#53864,41.43);
#19868=CIRCLE('',#53866,41.43);
#19869=CIRCLE('',#53868,41.43);
#19870=CIRCLE('',#53870,41.43);
#19871=CIRCLE('',#53872,41.43);
#19872=CIRCLE('',#53874,41.43);
#19873=CIRCLE('',#53876,41.43);
#19874=CIRCLE('',#53878,41.43);
#19875=CIRCLE('',#53880,41.43);
#19876=CIRCLE('',#53882,41.43);
#19877=CIRCLE('',#53884,41.43);
#19878=CIRCLE('',#53886,41.43);
#19879=CIRCLE('',#53888,41.43);
#19880=CIRCLE('',#53890,41.43);
#19881=CIRCLE('',#53892,41.43);
#19882=CIRCLE('',#53894,41.43);
#19883=CIRCLE('',#53896,41.43);
#19884=CIRCLE('',#53898,41.43);
#19885=CIRCLE('',#53900,41.43);
#19886=CIRCLE('',#53902,41.43);
#19887=CIRCLE('',#53904,41.43);
#19888=CIRCLE('',#54104,34.);
#19889=CIRCLE('',#54105,1.);
#19890=CIRCLE('',#54106,33.);
#19891=CIRCLE('',#54107,34.);
#19892=CIRCLE('',#54109,25.);
#19893=CIRCLE('',#54111,34.);
#19894=CIRCLE('',#54113,33.);
#19895=CIRCLE('',#54114,1.);
#19896=CIRCLE('',#54115,34.);
#19897=CIRCLE('',#54116,34.);
#19898=CIRCLE('',#54118,25.);
#19899=CIRCLE('',#54121,1.);
#19900=CIRCLE('',#54122,24.);
#19901=CIRCLE('',#54123,24.);
#19902=CIRCLE('',#54125,24.);
#19903=CIRCLE('',#54127,24.);
#19904=CIRCLE('',#54128,1.);
#19905=CIRCLE('',#54129,24.);
#19906=CIRCLE('',#54131,24.);
#19907=CIRCLE('',#54133,15.01);
#19908=CIRCLE('',#54134,15.01);
#19909=CIRCLE('',#54136,15.81);
#19910=CIRCLE('',#54140,15.81);
#19911=CIRCLE('',#54144,3.3);
#19912=CIRCLE('',#54145,3.);
#19913=CIRCLE('',#54147,47.);
#19914=CIRCLE('',#54148,3.3);
#19915=CIRCLE('',#54149,5.5);
#19916=CIRCLE('',#54150,5.5);
#19917=CIRCLE('',#54151,5.5);
#19918=CIRCLE('',#54152,5.5);
#19919=CIRCLE('',#54153,21.5);
#19920=CIRCLE('',#54155,3.);
#19921=CIRCLE('',#54157,3.);
#19922=CIRCLE('',#54159,3.);
#19923=CIRCLE('',#54161,3.3);
#19924=CIRCLE('',#54162,3.3);
#19925=CIRCLE('',#54164,3.3);
#19926=CIRCLE('',#54165,3.3);
#19927=CIRCLE('',#54167,3.3);
#19928=CIRCLE('',#54168,3.3);
#19929=CIRCLE('',#54170,3.3);
#19930=CIRCLE('',#54171,3.3);
#19931=CIRCLE('',#54173,5.5);
#19932=CIRCLE('',#54176,5.5);
#19933=CIRCLE('',#54179,5.5);
#19934=CIRCLE('',#54182,5.5);
#19935=CIRCLE('',#54185,5.05);
#19936=CIRCLE('',#54187,5.05);
#19937=CIRCLE('',#54189,5.55);
#19938=CIRCLE('',#54191,1.5);
#19939=CIRCLE('',#54192,20.);
#19940=CIRCLE('',#54193,20.);
#19941=CIRCLE('',#54195,20.);
#19942=CIRCLE('',#54197,19.5);
#19943=CIRCLE('',#54199,20.);
#19944=CIRCLE('',#54201,20.);
#19945=CIRCLE('',#54203,47.);
#19946=CIRCLE('',#54205,48.);
#19947=CIRCLE('',#54207,48.);
#19948=CIRCLE('',#54210,14.995);
#19949=CIRCLE('',#54212,14.995);
#19950=CIRCLE('',#54214,13.995);
#19951=CIRCLE('',#54369,5.);
#19952=CIRCLE('',#54370,4.5);
#19953=CIRCLE('',#54372,4.5);
#19954=CIRCLE('',#54374,9.);
#19955=CIRCLE('',#54375,9.);
#19956=CIRCLE('',#54376,9.);
#19957=CIRCLE('',#54377,9.);
#19958=CIRCLE('',#54378,5.);
#19959=CIRCLE('',#54379,3.3);
#19960=CIRCLE('',#54380,3.3);
#19961=CIRCLE('',#54381,3.3);
#19962=CIRCLE('',#54382,3.3);
#19963=CIRCLE('',#54383,20.025);
#19964=CIRCLE('',#54384,3.);
#19965=CIRCLE('',#54385,3.);
#19966=CIRCLE('',#54386,5.);
#19967=CIRCLE('',#54387,5.);
#19968=CIRCLE('',#54389,5.);
#19969=CIRCLE('',#54391,9.5);
#19970=CIRCLE('',#54392,9.5);
#19971=CIRCLE('',#54393,9.5);
#19972=CIRCLE('',#54394,9.5);
#19973=CIRCLE('',#54395,5.);
#19974=CIRCLE('',#54396,5.);
#19975=CIRCLE('',#54397,5.);
#19976=CIRCLE('',#54399,4.5);
#19977=CIRCLE('',#54401,4.5);
#19978=CIRCLE('',#54404,4.5);
#19979=CIRCLE('',#54406,4.5);
#19980=CIRCLE('',#54409,4.5);
#19981=CIRCLE('',#54411,4.5);
#19982=CIRCLE('',#54414,3.);
#19983=CIRCLE('',#54417,3.);
#19984=CIRCLE('',#54420,3.05);
#19985=CIRCLE('',#54422,3.05);
#19986=CIRCLE('',#54425,3.05);
#19987=CIRCLE('',#54427,3.05);
#19988=CIRCLE('',#54430,3.05);
#19989=CIRCLE('',#54432,3.05);
#19990=CIRCLE('',#54435,3.05);
#19991=CIRCLE('',#54437,3.05);
#19992=CIRCLE('',#54440,20.025);
#19993=CIRCLE('',#54443,10.);
#19994=CIRCLE('',#54446,10.);
#19995=CIRCLE('',#54449,10.);
#19996=CIRCLE('',#54452,10.);
#19997=CIRCLE('',#54456,10.);
#19998=CIRCLE('',#54459,10.);
#19999=CIRCLE('',#54466,10.);
#20000=CIRCLE('',#54469,10.);
#20001=CIRCLE('',#54476,5.5);
#20002=CIRCLE('',#54477,5.5);
#20003=CIRCLE('',#54479,6.);
#20004=CIRCLE('',#54481,27.5);
#20005=CIRCLE('',#54483,28.);
#20006=CIRCLE('',#54485,28.);
#20007=CIRCLE('',#54487,27.);
#20008=CIRCLE('',#54489,6.);
#20009=CIRCLE('',#54493,4.925);
#20010=CIRCLE('',#54510,4.0705);
#20011=CIRCLE('',#54512,4.0705);
#20012=CIRCLE('',#54528,4.925);
#20013=CIRCLE('',#54529,4.925);
#20014=CIRCLE('',#54531,4.925);
#20015=CIRCLE('',#54532,4.925);
#20016=CIRCLE('',#54533,4.0705);
#20017=CIRCLE('',#54536,0.4);
#20018=CIRCLE('',#54537,5.325);
#20019=CIRCLE('',#54538,4.925);
#20020=CIRCLE('',#54541,8.);
#20021=CIRCLE('',#54544,8.);
#20022=CIRCLE('',#54547,8.);
#20023=CIRCLE('',#54550,8.);
#20024=CIRCLE('',#54553,8.);
#20025=CIRCLE('',#54556,8.);
#20026=CIRCLE('',#54559,8.);
#20027=CIRCLE('',#54562,8.);
#20028=CIRCLE('',#54565,8.);
#20029=CIRCLE('',#54568,8.);
#20030=CIRCLE('',#54571,8.);
#20031=CIRCLE('',#54574,8.);
#20032=CIRCLE('',#54577,8.);
#20033=CIRCLE('',#54580,8.);
#20034=CIRCLE('',#54583,8.);
#20035=CIRCLE('',#54586,8.);
#20036=CIRCLE('',#54589,8.);
#20037=CIRCLE('',#54592,8.);
#20038=CIRCLE('',#54595,8.);
#20039=CIRCLE('',#54598,8.);
#20040=CIRCLE('',#54601,8.);
#20041=CIRCLE('',#54604,8.);
#20042=CIRCLE('',#54607,8.);
#20043=CIRCLE('',#54610,8.);
#20044=CIRCLE('',#54613,8.);
#20045=CIRCLE('',#54616,8.);
#20046=CIRCLE('',#54619,8.);
#20047=CIRCLE('',#54622,8.);
#20048=CIRCLE('',#54625,8.);
#20049=CIRCLE('',#54628,8.);
#20050=CIRCLE('',#54631,8.);
#20051=CIRCLE('',#54634,8.);
#20052=CIRCLE('',#54637,8.);
#20053=CIRCLE('',#54640,8.);
#20054=CIRCLE('',#54643,8.);
#20055=CIRCLE('',#54646,8.);
#20056=CIRCLE('',#54647,8.);
#20057=CIRCLE('',#54650,8.);
#20058=CIRCLE('',#54651,8.);
#20059=CIRCLE('',#54654,8.);
#20060=CIRCLE('',#54657,8.);
#20061=CIRCLE('',#54660,8.);
#20062=CIRCLE('',#54663,8.);
#20063=CIRCLE('',#54666,8.);
#20064=CIRCLE('',#54669,8.);
#20065=CIRCLE('',#54672,8.);
#20066=CIRCLE('',#54675,8.);
#20067=CIRCLE('',#54678,8.);
#20068=CIRCLE('',#54681,8.);
#20069=CIRCLE('',#54684,8.);
#20070=CIRCLE('',#54687,8.);
#20071=CIRCLE('',#54690,8.);
#20072=CIRCLE('',#54693,8.);
#20073=CIRCLE('',#54696,8.);
#20074=CIRCLE('',#54699,8.);
#20075=CIRCLE('',#54702,8.);
#20076=CIRCLE('',#54705,8.);
#20077=CIRCLE('',#54708,8.);
#20078=CIRCLE('',#54711,8.);
#20079=CIRCLE('',#54714,8.);
#20080=CIRCLE('',#54717,8.);
#20081=CIRCLE('',#54720,8.);
#20082=CIRCLE('',#54723,8.);
#20083=CIRCLE('',#54726,8.);
#20084=CIRCLE('',#54729,8.);
#20085=CIRCLE('',#54732,8.);
#20086=CIRCLE('',#54735,8.);
#20087=CIRCLE('',#54738,8.);
#20088=CIRCLE('',#54741,8.);
#20089=CIRCLE('',#54744,8.);
#20090=CIRCLE('',#54747,8.);
#20091=CIRCLE('',#54750,8.);
#20092=CIRCLE('',#54753,8.);
#20093=CIRCLE('',#54755,8.);
#20094=CIRCLE('',#54759,8.);
#20095=CIRCLE('',#54761,3.98342616391485);
#20096=CIRCLE('',#54770,4.);
#20097=CIRCLE('',#54773,8.);
#20098=CIRCLE('',#54774,8.);
#20099=CIRCLE('',#54775,8.);
#20100=CIRCLE('',#54776,8.);
#20101=CIRCLE('',#54777,8.);
#20102=CIRCLE('',#54778,8.);
#20103=CIRCLE('',#54779,8.);
#20104=CIRCLE('',#54780,8.);
#20105=CIRCLE('',#54781,8.);
#20106=CIRCLE('',#54782,8.);
#20107=CIRCLE('',#54783,8.);
#20108=CIRCLE('',#54784,8.);
#20109=CIRCLE('',#54785,8.);
#20110=CIRCLE('',#54786,8.);
#20111=CIRCLE('',#54787,8.);
#20112=CIRCLE('',#54788,8.);
#20113=CIRCLE('',#54789,8.);
#20114=CIRCLE('',#54790,8.);
#20115=CIRCLE('',#54791,8.);
#20116=CIRCLE('',#54792,8.);
#20117=CIRCLE('',#54793,8.);
#20118=CIRCLE('',#54794,8.);
#20119=CIRCLE('',#54795,8.);
#20120=CIRCLE('',#54796,8.);
#20121=CIRCLE('',#54797,8.);
#20122=CIRCLE('',#54798,8.);
#20123=CIRCLE('',#54799,8.);
#20124=CIRCLE('',#54800,8.);
#20125=CIRCLE('',#54801,8.);
#20126=CIRCLE('',#54802,8.);
#20127=CIRCLE('',#54803,8.);
#20128=CIRCLE('',#54804,8.);
#20129=CIRCLE('',#54805,8.);
#20130=CIRCLE('',#54806,8.);
#20131=CIRCLE('',#54807,8.);
#20132=CIRCLE('',#54808,8.);
#20133=CIRCLE('',#54810,7.);
#20134=CIRCLE('',#54814,10.);
#20135=CIRCLE('',#54815,9.8);
#20136=CIRCLE('',#54817,10.);
#20137=CIRCLE('',#54819,9.8);
#20138=CIRCLE('',#54821,5.45);
#20139=CIRCLE('',#54823,5.25);
#20140=CIRCLE('',#54825,5.25);
#20141=CIRCLE('',#54827,5.45);
#20142=CIRCLE('',#54831,5.1);
#20143=CIRCLE('',#54833,5.1);
#20144=CIRCLE('',#54835,9.05);
#20145=CIRCLE('',#54837,9.05);
#20146=CIRCLE('',#54843,9.05);
#20147=CIRCLE('',#54844,8.9);
#20148=CIRCLE('',#54846,9.05);
#20149=CIRCLE('',#54848,8.9);
#20150=CIRCLE('',#54850,5.6);
#20151=CIRCLE('',#54852,5.1);
#20152=CIRCLE('',#54854,5.1);
#20153=CIRCLE('',#54856,5.6);
#20154=CIRCLE('',#54860,2.942);
#20155=CIRCLE('',#54876,2.942);
#20156=CIRCLE('',#54878,2.37175);
#20157=CIRCLE('',#54894,2.942);
#20158=CIRCLE('',#54895,2.942);
#20159=CIRCLE('',#54897,2.942);
#20160=CIRCLE('',#54898,2.942);
#20161=CIRCLE('',#54899,2.37175);
#20162=CIRCLE('',#54902,2.942);
#20163=CIRCLE('',#54903,0.25);
#20164=CIRCLE('',#54904,3.192);
#20165=CIRCLE('',#54907,5.);
#20166=CIRCLE('',#54910,5.);
#20167=CIRCLE('',#54913,5.);
#20168=CIRCLE('',#54916,5.);
#20169=CIRCLE('',#54919,5.);
#20170=CIRCLE('',#54922,5.);
#20171=CIRCLE('',#54925,5.);
#20172=CIRCLE('',#54928,5.);
#20173=CIRCLE('',#54931,5.);
#20174=CIRCLE('',#54934,5.);
#20175=CIRCLE('',#54937,5.);
#20176=CIRCLE('',#54940,5.);
#20177=CIRCLE('',#54943,5.);
#20178=CIRCLE('',#54946,5.);
#20179=CIRCLE('',#54949,5.);
#20180=CIRCLE('',#54952,5.);
#20181=CIRCLE('',#54955,5.);
#20182=CIRCLE('',#54958,5.);
#20183=CIRCLE('',#54961,5.);
#20184=CIRCLE('',#54964,5.);
#20185=CIRCLE('',#54967,5.);
#20186=CIRCLE('',#54970,5.);
#20187=CIRCLE('',#54973,5.);
#20188=CIRCLE('',#54976,5.);
#20189=CIRCLE('',#54979,5.);
#20190=CIRCLE('',#54982,5.);
#20191=CIRCLE('',#54985,5.);
#20192=CIRCLE('',#54988,5.);
#20193=CIRCLE('',#54991,5.);
#20194=CIRCLE('',#54994,5.);
#20195=CIRCLE('',#54997,5.);
#20196=CIRCLE('',#55000,5.);
#20197=CIRCLE('',#55003,5.);
#20198=CIRCLE('',#55006,5.);
#20199=CIRCLE('',#55009,5.);
#20200=CIRCLE('',#55012,5.);
#20201=CIRCLE('',#55013,5.);
#20202=CIRCLE('',#55016,5.);
#20203=CIRCLE('',#55017,5.);
#20204=CIRCLE('',#55020,5.);
#20205=CIRCLE('',#55023,5.);
#20206=CIRCLE('',#55026,5.);
#20207=CIRCLE('',#55029,5.);
#20208=CIRCLE('',#55032,5.);
#20209=CIRCLE('',#55035,5.);
#20210=CIRCLE('',#55038,5.);
#20211=CIRCLE('',#55041,5.);
#20212=CIRCLE('',#55044,5.);
#20213=CIRCLE('',#55047,5.);
#20214=CIRCLE('',#55050,5.);
#20215=CIRCLE('',#55053,5.);
#20216=CIRCLE('',#55056,5.);
#20217=CIRCLE('',#55059,5.);
#20218=CIRCLE('',#55062,5.);
#20219=CIRCLE('',#55065,5.);
#20220=CIRCLE('',#55068,5.);
#20221=CIRCLE('',#55071,5.);
#20222=CIRCLE('',#55074,5.);
#20223=CIRCLE('',#55077,5.);
#20224=CIRCLE('',#55080,5.);
#20225=CIRCLE('',#55083,5.);
#20226=CIRCLE('',#55086,5.);
#20227=CIRCLE('',#55089,5.);
#20228=CIRCLE('',#55092,5.);
#20229=CIRCLE('',#55095,5.);
#20230=CIRCLE('',#55098,5.);
#20231=CIRCLE('',#55101,5.);
#20232=CIRCLE('',#55104,5.);
#20233=CIRCLE('',#55107,5.);
#20234=CIRCLE('',#55110,5.);
#20235=CIRCLE('',#55113,5.);
#20236=CIRCLE('',#55116,5.);
#20237=CIRCLE('',#55119,5.);
#20238=CIRCLE('',#55121,5.);
#20239=CIRCLE('',#55125,5.);
#20240=CIRCLE('',#55127,2.48346726553949);
#20241=CIRCLE('',#55136,2.4);
#20242=CIRCLE('',#55139,5.);
#20243=CIRCLE('',#55140,5.);
#20244=CIRCLE('',#55141,5.);
#20245=CIRCLE('',#55142,5.);
#20246=CIRCLE('',#55143,5.);
#20247=CIRCLE('',#55144,5.);
#20248=CIRCLE('',#55145,5.);
#20249=CIRCLE('',#55146,5.);
#20250=CIRCLE('',#55147,5.);
#20251=CIRCLE('',#55148,5.);
#20252=CIRCLE('',#55149,5.);
#20253=CIRCLE('',#55150,5.);
#20254=CIRCLE('',#55151,5.);
#20255=CIRCLE('',#55152,5.);
#20256=CIRCLE('',#55153,5.);
#20257=CIRCLE('',#55154,5.);
#20258=CIRCLE('',#55155,5.);
#20259=CIRCLE('',#55156,5.);
#20260=CIRCLE('',#55157,5.);
#20261=CIRCLE('',#55158,5.);
#20262=CIRCLE('',#55159,5.);
#20263=CIRCLE('',#55160,5.);
#20264=CIRCLE('',#55161,5.);
#20265=CIRCLE('',#55162,5.);
#20266=CIRCLE('',#55163,5.);
#20267=CIRCLE('',#55164,5.);
#20268=CIRCLE('',#55165,5.);
#20269=CIRCLE('',#55166,5.);
#20270=CIRCLE('',#55167,5.);
#20271=CIRCLE('',#55168,5.);
#20272=CIRCLE('',#55169,5.);
#20273=CIRCLE('',#55170,5.);
#20274=CIRCLE('',#55171,5.);
#20275=CIRCLE('',#55172,5.);
#20276=CIRCLE('',#55173,5.);
#20277=CIRCLE('',#55174,5.);
#20278=CIRCLE('',#55176,4.4);
#20279=CIRCLE('',#55180,2.06862915010152);
#20280=CIRCLE('',#55181,0.8);
#20281=CIRCLE('',#55182,2.63431457505076);
#20282=CIRCLE('',#55183,2.63431457505076);
#20283=CIRCLE('',#55185,3.);
#20284=CIRCLE('',#55188,2.4);
#20285=CIRCLE('',#55190,3.);
#20286=CIRCLE('',#55194,3.933);
#20287=CIRCLE('',#55218,3.22275);
#20288=CIRCLE('',#55242,3.933);
#20289=CIRCLE('',#55243,3.933);
#20290=CIRCLE('',#55245,3.933);
#20291=CIRCLE('',#55246,3.933);
#20292=CIRCLE('',#55247,3.22275);
#20293=CIRCLE('',#55250,0.4);
#20294=CIRCLE('',#55251,4.333);
#20295=CIRCLE('',#55252,3.933);
#20296=CIRCLE('',#55255,5.8);
#20297=CIRCLE('',#55257,6.33323321723195);
#20298=CIRCLE('',#55262,5.8);
#20299=CIRCLE('',#55264,3.2);
#20300=CIRCLE('',#55273,8.);
#20301=CIRCLE('',#55274,7.8);
#20302=CIRCLE('',#55276,8.);
#20303=CIRCLE('',#55278,7.8);
#20304=CIRCLE('',#55280,4.4);
#20305=CIRCLE('',#55282,4.2);
#20306=CIRCLE('',#55284,4.2);
#20307=CIRCLE('',#55286,4.4);
#20308=CIRCLE('',#55290,7.4);
#20309=CIRCLE('',#55292,7.4);
#20310=CIRCLE('',#55299,7.4);
#20311=CIRCLE('',#55300,7.25);
#20312=CIRCLE('',#55302,7.4);
#20313=CIRCLE('',#55304,7.25);
#20314=CIRCLE('',#55306,4.55);
#20315=CIRCLE('',#55308,4.05);
#20316=CIRCLE('',#55310,4.05);
#20317=CIRCLE('',#55312,4.55);
#20318=CIRCLE('',#55316,4.69285714285714);
#20319=CIRCLE('',#55317,4.05);
#20320=CIRCLE('',#55319,4.05);
#20321=CIRCLE('',#55321,4.69285714285714);
#20322=CIRCLE('',#55323,6.33323321723195);
#20323=CIRCLE('',#55328,6.33323321723195);
#20324=VERTEX_POINT('',#68261);
#20325=VERTEX_POINT('',#68262);
#20326=VERTEX_POINT('',#68264);
#20327=VERTEX_POINT('',#68268);
#20328=VERTEX_POINT('',#68276);
#20329=VERTEX_POINT('',#68277);
#20330=VERTEX_POINT('',#68279);
#20331=VERTEX_POINT('',#68283);
#20332=VERTEX_POINT('',#68291);
#20333=VERTEX_POINT('',#68292);
#20334=VERTEX_POINT('',#68294);
#20335=VERTEX_POINT('',#68298);
#20336=VERTEX_POINT('',#68306);
#20337=VERTEX_POINT('',#68307);
#20338=VERTEX_POINT('',#68309);
#20339=VERTEX_POINT('',#68313);
#20340=VERTEX_POINT('',#68321);
#20341=VERTEX_POINT('',#68322);
#20342=VERTEX_POINT('',#68324);
#20343=VERTEX_POINT('',#68328);
#20344=VERTEX_POINT('',#68336);
#20345=VERTEX_POINT('',#68337);
#20346=VERTEX_POINT('',#68339);
#20347=VERTEX_POINT('',#68343);
#20348=VERTEX_POINT('',#68351);
#20349=VERTEX_POINT('',#68352);
#20350=VERTEX_POINT('',#68354);
#20351=VERTEX_POINT('',#68358);
#20352=VERTEX_POINT('',#68366);
#20353=VERTEX_POINT('',#68367);
#20354=VERTEX_POINT('',#68369);
#20355=VERTEX_POINT('',#68373);
#20356=VERTEX_POINT('',#68381);
#20357=VERTEX_POINT('',#68382);
#20358=VERTEX_POINT('',#68384);
#20359=VERTEX_POINT('',#68388);
#20360=VERTEX_POINT('',#68396);
#20361=VERTEX_POINT('',#68397);
#20362=VERTEX_POINT('',#68399);
#20363=VERTEX_POINT('',#68403);
#20364=VERTEX_POINT('',#68411);
#20365=VERTEX_POINT('',#68412);
#20366=VERTEX_POINT('',#68414);
#20367=VERTEX_POINT('',#68418);
#20368=VERTEX_POINT('',#68426);
#20369=VERTEX_POINT('',#68427);
#20370=VERTEX_POINT('',#68429);
#20371=VERTEX_POINT('',#68433);
#20372=VERTEX_POINT('',#68441);
#20373=VERTEX_POINT('',#68442);
#20374=VERTEX_POINT('',#68444);
#20375=VERTEX_POINT('',#68448);
#20376=VERTEX_POINT('',#68456);
#20377=VERTEX_POINT('',#68457);
#20378=VERTEX_POINT('',#68459);
#20379=VERTEX_POINT('',#68463);
#20380=VERTEX_POINT('',#68471);
#20381=VERTEX_POINT('',#68472);
#20382=VERTEX_POINT('',#68474);
#20383=VERTEX_POINT('',#68478);
#20384=VERTEX_POINT('',#68486);
#20385=VERTEX_POINT('',#68487);
#20386=VERTEX_POINT('',#68489);
#20387=VERTEX_POINT('',#68493);
#20388=VERTEX_POINT('',#68501);
#20389=VERTEX_POINT('',#68502);
#20390=VERTEX_POINT('',#68504);
#20391=VERTEX_POINT('',#68508);
#20392=VERTEX_POINT('',#68516);
#20393=VERTEX_POINT('',#68517);
#20394=VERTEX_POINT('',#68519);
#20395=VERTEX_POINT('',#68523);
#20396=VERTEX_POINT('',#68531);
#20397=VERTEX_POINT('',#68532);
#20398=VERTEX_POINT('',#68534);
#20399=VERTEX_POINT('',#68538);
#20400=VERTEX_POINT('',#68546);
#20401=VERTEX_POINT('',#68547);
#20402=VERTEX_POINT('',#68549);
#20403=VERTEX_POINT('',#68553);
#20404=VERTEX_POINT('',#68561);
#20405=VERTEX_POINT('',#68562);
#20406=VERTEX_POINT('',#68564);
#20407=VERTEX_POINT('',#68568);
#20408=VERTEX_POINT('',#68576);
#20409=VERTEX_POINT('',#68577);
#20410=VERTEX_POINT('',#68579);
#20411=VERTEX_POINT('',#68583);
#20412=VERTEX_POINT('',#68591);
#20413=VERTEX_POINT('',#68592);
#20414=VERTEX_POINT('',#68594);
#20415=VERTEX_POINT('',#68598);
#20416=VERTEX_POINT('',#68606);
#20417=VERTEX_POINT('',#68607);
#20418=VERTEX_POINT('',#68609);
#20419=VERTEX_POINT('',#68613);
#20420=VERTEX_POINT('',#68621);
#20421=VERTEX_POINT('',#68622);
#20422=VERTEX_POINT('',#68624);
#20423=VERTEX_POINT('',#68628);
#20424=VERTEX_POINT('',#68636);
#20425=VERTEX_POINT('',#68637);
#20426=VERTEX_POINT('',#68639);
#20427=VERTEX_POINT('',#68643);
#20428=VERTEX_POINT('',#68651);
#20429=VERTEX_POINT('',#68652);
#20430=VERTEX_POINT('',#68654);
#20431=VERTEX_POINT('',#68658);
#20432=VERTEX_POINT('',#68666);
#20433=VERTEX_POINT('',#68667);
#20434=VERTEX_POINT('',#68669);
#20435=VERTEX_POINT('',#68673);
#20436=VERTEX_POINT('',#68681);
#20437=VERTEX_POINT('',#68682);
#20438=VERTEX_POINT('',#68684);
#20439=VERTEX_POINT('',#68688);
#20440=VERTEX_POINT('',#68696);
#20441=VERTEX_POINT('',#68697);
#20442=VERTEX_POINT('',#68699);
#20443=VERTEX_POINT('',#68703);
#20444=VERTEX_POINT('',#68711);
#20445=VERTEX_POINT('',#68712);
#20446=VERTEX_POINT('',#68714);
#20447=VERTEX_POINT('',#68718);
#20448=VERTEX_POINT('',#68726);
#20449=VERTEX_POINT('',#68727);
#20450=VERTEX_POINT('',#68729);
#20451=VERTEX_POINT('',#68733);
#20452=VERTEX_POINT('',#68741);
#20453=VERTEX_POINT('',#68742);
#20454=VERTEX_POINT('',#68744);
#20455=VERTEX_POINT('',#68748);
#20456=VERTEX_POINT('',#68756);
#20457=VERTEX_POINT('',#68757);
#20458=VERTEX_POINT('',#68759);
#20459=VERTEX_POINT('',#68763);
#20460=VERTEX_POINT('',#68771);
#20461=VERTEX_POINT('',#68772);
#20462=VERTEX_POINT('',#68774);
#20463=VERTEX_POINT('',#68778);
#20464=VERTEX_POINT('',#68786);
#20465=VERTEX_POINT('',#68787);
#20466=VERTEX_POINT('',#68789);
#20467=VERTEX_POINT('',#68793);
#20468=VERTEX_POINT('',#68801);
#20469=VERTEX_POINT('',#68803);
#20470=VERTEX_POINT('',#68805);
#20471=VERTEX_POINT('',#68807);
#20472=VERTEX_POINT('',#68809);
#20473=VERTEX_POINT('',#68811);
#20474=VERTEX_POINT('',#68813);
#20475=VERTEX_POINT('',#68815);
#20476=VERTEX_POINT('',#68817);
#20477=VERTEX_POINT('',#68819);
#20478=VERTEX_POINT('',#68821);
#20479=VERTEX_POINT('',#68823);
#20480=VERTEX_POINT('',#68825);
#20481=VERTEX_POINT('',#68827);
#20482=VERTEX_POINT('',#68829);
#20483=VERTEX_POINT('',#68831);
#20484=VERTEX_POINT('',#68835);
#20485=VERTEX_POINT('',#68837);
#20486=VERTEX_POINT('',#68839);
#20487=VERTEX_POINT('',#68841);
#20488=VERTEX_POINT('',#68843);
#20489=VERTEX_POINT('',#68845);
#20490=VERTEX_POINT('',#68847);
#20491=VERTEX_POINT('',#68849);
#20492=VERTEX_POINT('',#68851);
#20493=VERTEX_POINT('',#68853);
#20494=VERTEX_POINT('',#68855);
#20495=VERTEX_POINT('',#68857);
#20496=VERTEX_POINT('',#68859);
#20497=VERTEX_POINT('',#68861);
#20498=VERTEX_POINT('',#68865);
#20499=VERTEX_POINT('',#68867);
#20500=VERTEX_POINT('',#68869);
#20501=VERTEX_POINT('',#68873);
#20502=VERTEX_POINT('',#68877);
#20503=VERTEX_POINT('',#68879);
#20504=VERTEX_POINT('',#68881);
#20505=VERTEX_POINT('',#68883);
#20506=VERTEX_POINT('',#68885);
#20507=VERTEX_POINT('',#68887);
#20508=VERTEX_POINT('',#68889);
#20509=VERTEX_POINT('',#68891);
#20510=VERTEX_POINT('',#68893);
#20511=VERTEX_POINT('',#68895);
#20512=VERTEX_POINT('',#68897);
#20513=VERTEX_POINT('',#68899);
#20514=VERTEX_POINT('',#68901);
#20515=VERTEX_POINT('',#68903);
#20516=VERTEX_POINT('',#68905);
#20517=VERTEX_POINT('',#68907);
#20518=VERTEX_POINT('',#68911);
#20519=VERTEX_POINT('',#68913);
#20520=VERTEX_POINT('',#68915);
#20521=VERTEX_POINT('',#68917);
#20522=VERTEX_POINT('',#68919);
#20523=VERTEX_POINT('',#68921);
#20524=VERTEX_POINT('',#68923);
#20525=VERTEX_POINT('',#68925);
#20526=VERTEX_POINT('',#68927);
#20527=VERTEX_POINT('',#68929);
#20528=VERTEX_POINT('',#68931);
#20529=VERTEX_POINT('',#68933);
#20530=VERTEX_POINT('',#68935);
#20531=VERTEX_POINT('',#68937);
#20532=VERTEX_POINT('',#68941);
#20533=VERTEX_POINT('',#68943);
#20534=VERTEX_POINT('',#68945);
#20535=VERTEX_POINT('',#68949);
#20536=VERTEX_POINT('',#68953);
#20537=VERTEX_POINT('',#68955);
#20538=VERTEX_POINT('',#68957);
#20539=VERTEX_POINT('',#68959);
#20540=VERTEX_POINT('',#68961);
#20541=VERTEX_POINT('',#68963);
#20542=VERTEX_POINT('',#68965);
#20543=VERTEX_POINT('',#68967);
#20544=VERTEX_POINT('',#68969);
#20545=VERTEX_POINT('',#68971);
#20546=VERTEX_POINT('',#68973);
#20547=VERTEX_POINT('',#68975);
#20548=VERTEX_POINT('',#68977);
#20549=VERTEX_POINT('',#68979);
#20550=VERTEX_POINT('',#68981);
#20551=VERTEX_POINT('',#68983);
#20552=VERTEX_POINT('',#68987);
#20553=VERTEX_POINT('',#68989);
#20554=VERTEX_POINT('',#68991);
#20555=VERTEX_POINT('',#68993);
#20556=VERTEX_POINT('',#68995);
#20557=VERTEX_POINT('',#68997);
#20558=VERTEX_POINT('',#68999);
#20559=VERTEX_POINT('',#69001);
#20560=VERTEX_POINT('',#69003);
#20561=VERTEX_POINT('',#69005);
#20562=VERTEX_POINT('',#69007);
#20563=VERTEX_POINT('',#69009);
#20564=VERTEX_POINT('',#69011);
#20565=VERTEX_POINT('',#69013);
#20566=VERTEX_POINT('',#69017);
#20567=VERTEX_POINT('',#69019);
#20568=VERTEX_POINT('',#69021);
#20569=VERTEX_POINT('',#69025);
#20570=VERTEX_POINT('',#69029);
#20571=VERTEX_POINT('',#69031);
#20572=VERTEX_POINT('',#69033);
#20573=VERTEX_POINT('',#69035);
#20574=VERTEX_POINT('',#69037);
#20575=VERTEX_POINT('',#69039);
#20576=VERTEX_POINT('',#69041);
#20577=VERTEX_POINT('',#69043);
#20578=VERTEX_POINT('',#69045);
#20579=VERTEX_POINT('',#69047);
#20580=VERTEX_POINT('',#69049);
#20581=VERTEX_POINT('',#69051);
#20582=VERTEX_POINT('',#69053);
#20583=VERTEX_POINT('',#69055);
#20584=VERTEX_POINT('',#69057);
#20585=VERTEX_POINT('',#69059);
#20586=VERTEX_POINT('',#69063);
#20587=VERTEX_POINT('',#69065);
#20588=VERTEX_POINT('',#69067);
#20589=VERTEX_POINT('',#69069);
#20590=VERTEX_POINT('',#69071);
#20591=VERTEX_POINT('',#69073);
#20592=VERTEX_POINT('',#69075);
#20593=VERTEX_POINT('',#69077);
#20594=VERTEX_POINT('',#69079);
#20595=VERTEX_POINT('',#69081);
#20596=VERTEX_POINT('',#69083);
#20597=VERTEX_POINT('',#69085);
#20598=VERTEX_POINT('',#69087);
#20599=VERTEX_POINT('',#69089);
#20600=VERTEX_POINT('',#69093);
#20601=VERTEX_POINT('',#69095);
#20602=VERTEX_POINT('',#69097);
#20603=VERTEX_POINT('',#69101);
#20604=VERTEX_POINT('',#69105);
#20605=VERTEX_POINT('',#69107);
#20606=VERTEX_POINT('',#69109);
#20607=VERTEX_POINT('',#69111);
#20608=VERTEX_POINT('',#69113);
#20609=VERTEX_POINT('',#69115);
#20610=VERTEX_POINT('',#69117);
#20611=VERTEX_POINT('',#69119);
#20612=VERTEX_POINT('',#69121);
#20613=VERTEX_POINT('',#69123);
#20614=VERTEX_POINT('',#69125);
#20615=VERTEX_POINT('',#69127);
#20616=VERTEX_POINT('',#69129);
#20617=VERTEX_POINT('',#69131);
#20618=VERTEX_POINT('',#69133);
#20619=VERTEX_POINT('',#69135);
#20620=VERTEX_POINT('',#69139);
#20621=VERTEX_POINT('',#69141);
#20622=VERTEX_POINT('',#69143);
#20623=VERTEX_POINT('',#69145);
#20624=VERTEX_POINT('',#69147);
#20625=VERTEX_POINT('',#69149);
#20626=VERTEX_POINT('',#69151);
#20627=VERTEX_POINT('',#69153);
#20628=VERTEX_POINT('',#69155);
#20629=VERTEX_POINT('',#69157);
#20630=VERTEX_POINT('',#69159);
#20631=VERTEX_POINT('',#69161);
#20632=VERTEX_POINT('',#69163);
#20633=VERTEX_POINT('',#69165);
#20634=VERTEX_POINT('',#69169);
#20635=VERTEX_POINT('',#69171);
#20636=VERTEX_POINT('',#69173);
#20637=VERTEX_POINT('',#69177);
#20638=VERTEX_POINT('',#69181);
#20639=VERTEX_POINT('',#69183);
#20640=VERTEX_POINT('',#69185);
#20641=VERTEX_POINT('',#69187);
#20642=VERTEX_POINT('',#69189);
#20643=VERTEX_POINT('',#69191);
#20644=VERTEX_POINT('',#69193);
#20645=VERTEX_POINT('',#69195);
#20646=VERTEX_POINT('',#69197);
#20647=VERTEX_POINT('',#69199);
#20648=VERTEX_POINT('',#69201);
#20649=VERTEX_POINT('',#69203);
#20650=VERTEX_POINT('',#69205);
#20651=VERTEX_POINT('',#69207);
#20652=VERTEX_POINT('',#69209);
#20653=VERTEX_POINT('',#69211);
#20654=VERTEX_POINT('',#69215);
#20655=VERTEX_POINT('',#69217);
#20656=VERTEX_POINT('',#69219);
#20657=VERTEX_POINT('',#69221);
#20658=VERTEX_POINT('',#69223);
#20659=VERTEX_POINT('',#69225);
#20660=VERTEX_POINT('',#69227);
#20661=VERTEX_POINT('',#69229);
#20662=VERTEX_POINT('',#69231);
#20663=VERTEX_POINT('',#69233);
#20664=VERTEX_POINT('',#69235);
#20665=VERTEX_POINT('',#69237);
#20666=VERTEX_POINT('',#69239);
#20667=VERTEX_POINT('',#69241);
#20668=VERTEX_POINT('',#69245);
#20669=VERTEX_POINT('',#69247);
#20670=VERTEX_POINT('',#69249);
#20671=VERTEX_POINT('',#69253);
#20672=VERTEX_POINT('',#69257);
#20673=VERTEX_POINT('',#69259);
#20674=VERTEX_POINT('',#69261);
#20675=VERTEX_POINT('',#69263);
#20676=VERTEX_POINT('',#69265);
#20677=VERTEX_POINT('',#69267);
#20678=VERTEX_POINT('',#69269);
#20679=VERTEX_POINT('',#69271);
#20680=VERTEX_POINT('',#69273);
#20681=VERTEX_POINT('',#69275);
#20682=VERTEX_POINT('',#69277);
#20683=VERTEX_POINT('',#69279);
#20684=VERTEX_POINT('',#69281);
#20685=VERTEX_POINT('',#69283);
#20686=VERTEX_POINT('',#69285);
#20687=VERTEX_POINT('',#69287);
#20688=VERTEX_POINT('',#69291);
#20689=VERTEX_POINT('',#69293);
#20690=VERTEX_POINT('',#69295);
#20691=VERTEX_POINT('',#69297);
#20692=VERTEX_POINT('',#69299);
#20693=VERTEX_POINT('',#69301);
#20694=VERTEX_POINT('',#69303);
#20695=VERTEX_POINT('',#69305);
#20696=VERTEX_POINT('',#69307);
#20697=VERTEX_POINT('',#69309);
#20698=VERTEX_POINT('',#69311);
#20699=VERTEX_POINT('',#69313);
#20700=VERTEX_POINT('',#69315);
#20701=VERTEX_POINT('',#69317);
#20702=VERTEX_POINT('',#69321);
#20703=VERTEX_POINT('',#69323);
#20704=VERTEX_POINT('',#69325);
#20705=VERTEX_POINT('',#69329);
#20706=VERTEX_POINT('',#69333);
#20707=VERTEX_POINT('',#69335);
#20708=VERTEX_POINT('',#69337);
#20709=VERTEX_POINT('',#69339);
#20710=VERTEX_POINT('',#69341);
#20711=VERTEX_POINT('',#69343);
#20712=VERTEX_POINT('',#69345);
#20713=VERTEX_POINT('',#69347);
#20714=VERTEX_POINT('',#69349);
#20715=VERTEX_POINT('',#69351);
#20716=VERTEX_POINT('',#69353);
#20717=VERTEX_POINT('',#69355);
#20718=VERTEX_POINT('',#69357);
#20719=VERTEX_POINT('',#69359);
#20720=VERTEX_POINT('',#69361);
#20721=VERTEX_POINT('',#69363);
#20722=VERTEX_POINT('',#69367);
#20723=VERTEX_POINT('',#69369);
#20724=VERTEX_POINT('',#69371);
#20725=VERTEX_POINT('',#69373);
#20726=VERTEX_POINT('',#69375);
#20727=VERTEX_POINT('',#69377);
#20728=VERTEX_POINT('',#69379);
#20729=VERTEX_POINT('',#69381);
#20730=VERTEX_POINT('',#69383);
#20731=VERTEX_POINT('',#69385);
#20732=VERTEX_POINT('',#69387);
#20733=VERTEX_POINT('',#69389);
#20734=VERTEX_POINT('',#69391);
#20735=VERTEX_POINT('',#69393);
#20736=VERTEX_POINT('',#69397);
#20737=VERTEX_POINT('',#69399);
#20738=VERTEX_POINT('',#69401);
#20739=VERTEX_POINT('',#69405);
#20740=VERTEX_POINT('',#69409);
#20741=VERTEX_POINT('',#69411);
#20742=VERTEX_POINT('',#69413);
#20743=VERTEX_POINT('',#69415);
#20744=VERTEX_POINT('',#69417);
#20745=VERTEX_POINT('',#69419);
#20746=VERTEX_POINT('',#69421);
#20747=VERTEX_POINT('',#69423);
#20748=VERTEX_POINT('',#69425);
#20749=VERTEX_POINT('',#69427);
#20750=VERTEX_POINT('',#69429);
#20751=VERTEX_POINT('',#69431);
#20752=VERTEX_POINT('',#69433);
#20753=VERTEX_POINT('',#69435);
#20754=VERTEX_POINT('',#69437);
#20755=VERTEX_POINT('',#69439);
#20756=VERTEX_POINT('',#69443);
#20757=VERTEX_POINT('',#69445);
#20758=VERTEX_POINT('',#69447);
#20759=VERTEX_POINT('',#69449);
#20760=VERTEX_POINT('',#69451);
#20761=VERTEX_POINT('',#69453);
#20762=VERTEX_POINT('',#69455);
#20763=VERTEX_POINT('',#69457);
#20764=VERTEX_POINT('',#69459);
#20765=VERTEX_POINT('',#69461);
#20766=VERTEX_POINT('',#69463);
#20767=VERTEX_POINT('',#69465);
#20768=VERTEX_POINT('',#69467);
#20769=VERTEX_POINT('',#69469);
#20770=VERTEX_POINT('',#69473);
#20771=VERTEX_POINT('',#69475);
#20772=VERTEX_POINT('',#69477);
#20773=VERTEX_POINT('',#69481);
#20774=VERTEX_POINT('',#69485);
#20775=VERTEX_POINT('',#69487);
#20776=VERTEX_POINT('',#69489);
#20777=VERTEX_POINT('',#69491);
#20778=VERTEX_POINT('',#69493);
#20779=VERTEX_POINT('',#69495);
#20780=VERTEX_POINT('',#69497);
#20781=VERTEX_POINT('',#69499);
#20782=VERTEX_POINT('',#69501);
#20783=VERTEX_POINT('',#69503);
#20784=VERTEX_POINT('',#69505);
#20785=VERTEX_POINT('',#69507);
#20786=VERTEX_POINT('',#69509);
#20787=VERTEX_POINT('',#69511);
#20788=VERTEX_POINT('',#69513);
#20789=VERTEX_POINT('',#69515);
#20790=VERTEX_POINT('',#69519);
#20791=VERTEX_POINT('',#69521);
#20792=VERTEX_POINT('',#69523);
#20793=VERTEX_POINT('',#69525);
#20794=VERTEX_POINT('',#69527);
#20795=VERTEX_POINT('',#69529);
#20796=VERTEX_POINT('',#69531);
#20797=VERTEX_POINT('',#69533);
#20798=VERTEX_POINT('',#69535);
#20799=VERTEX_POINT('',#69537);
#20800=VERTEX_POINT('',#69539);
#20801=VERTEX_POINT('',#69541);
#20802=VERTEX_POINT('',#69543);
#20803=VERTEX_POINT('',#69545);
#20804=VERTEX_POINT('',#69549);
#20805=VERTEX_POINT('',#69551);
#20806=VERTEX_POINT('',#69553);
#20807=VERTEX_POINT('',#69557);
#20808=VERTEX_POINT('',#69561);
#20809=VERTEX_POINT('',#69563);
#20810=VERTEX_POINT('',#69565);
#20811=VERTEX_POINT('',#69567);
#20812=VERTEX_POINT('',#69569);
#20813=VERTEX_POINT('',#69571);
#20814=VERTEX_POINT('',#69573);
#20815=VERTEX_POINT('',#69575);
#20816=VERTEX_POINT('',#69577);
#20817=VERTEX_POINT('',#69579);
#20818=VERTEX_POINT('',#69581);
#20819=VERTEX_POINT('',#69583);
#20820=VERTEX_POINT('',#69585);
#20821=VERTEX_POINT('',#69587);
#20822=VERTEX_POINT('',#69589);
#20823=VERTEX_POINT('',#69591);
#20824=VERTEX_POINT('',#69595);
#20825=VERTEX_POINT('',#69597);
#20826=VERTEX_POINT('',#69599);
#20827=VERTEX_POINT('',#69601);
#20828=VERTEX_POINT('',#69603);
#20829=VERTEX_POINT('',#69605);
#20830=VERTEX_POINT('',#69607);
#20831=VERTEX_POINT('',#69609);
#20832=VERTEX_POINT('',#69611);
#20833=VERTEX_POINT('',#69613);
#20834=VERTEX_POINT('',#69615);
#20835=VERTEX_POINT('',#69617);
#20836=VERTEX_POINT('',#69619);
#20837=VERTEX_POINT('',#69621);
#20838=VERTEX_POINT('',#69625);
#20839=VERTEX_POINT('',#69627);
#20840=VERTEX_POINT('',#69629);
#20841=VERTEX_POINT('',#69633);
#20842=VERTEX_POINT('',#69637);
#20843=VERTEX_POINT('',#69639);
#20844=VERTEX_POINT('',#69641);
#20845=VERTEX_POINT('',#69643);
#20846=VERTEX_POINT('',#69645);
#20847=VERTEX_POINT('',#69647);
#20848=VERTEX_POINT('',#69649);
#20849=VERTEX_POINT('',#69651);
#20850=VERTEX_POINT('',#69653);
#20851=VERTEX_POINT('',#69655);
#20852=VERTEX_POINT('',#69657);
#20853=VERTEX_POINT('',#69659);
#20854=VERTEX_POINT('',#69661);
#20855=VERTEX_POINT('',#69663);
#20856=VERTEX_POINT('',#69665);
#20857=VERTEX_POINT('',#69667);
#20858=VERTEX_POINT('',#69671);
#20859=VERTEX_POINT('',#69673);
#20860=VERTEX_POINT('',#69675);
#20861=VERTEX_POINT('',#69677);
#20862=VERTEX_POINT('',#69679);
#20863=VERTEX_POINT('',#69681);
#20864=VERTEX_POINT('',#69683);
#20865=VERTEX_POINT('',#69685);
#20866=VERTEX_POINT('',#69687);
#20867=VERTEX_POINT('',#69689);
#20868=VERTEX_POINT('',#69691);
#20869=VERTEX_POINT('',#69693);
#20870=VERTEX_POINT('',#69695);
#20871=VERTEX_POINT('',#69697);
#20872=VERTEX_POINT('',#69701);
#20873=VERTEX_POINT('',#69703);
#20874=VERTEX_POINT('',#69705);
#20875=VERTEX_POINT('',#69709);
#20876=VERTEX_POINT('',#69713);
#20877=VERTEX_POINT('',#69715);
#20878=VERTEX_POINT('',#69717);
#20879=VERTEX_POINT('',#69719);
#20880=VERTEX_POINT('',#69721);
#20881=VERTEX_POINT('',#69723);
#20882=VERTEX_POINT('',#69725);
#20883=VERTEX_POINT('',#69727);
#20884=VERTEX_POINT('',#69729);
#20885=VERTEX_POINT('',#69731);
#20886=VERTEX_POINT('',#69733);
#20887=VERTEX_POINT('',#69735);
#20888=VERTEX_POINT('',#69737);
#20889=VERTEX_POINT('',#69739);
#20890=VERTEX_POINT('',#69741);
#20891=VERTEX_POINT('',#69743);
#20892=VERTEX_POINT('',#69747);
#20893=VERTEX_POINT('',#69749);
#20894=VERTEX_POINT('',#69751);
#20895=VERTEX_POINT('',#69753);
#20896=VERTEX_POINT('',#69755);
#20897=VERTEX_POINT('',#69757);
#20898=VERTEX_POINT('',#69759);
#20899=VERTEX_POINT('',#69761);
#20900=VERTEX_POINT('',#69763);
#20901=VERTEX_POINT('',#69765);
#20902=VERTEX_POINT('',#69767);
#20903=VERTEX_POINT('',#69769);
#20904=VERTEX_POINT('',#69771);
#20905=VERTEX_POINT('',#69773);
#20906=VERTEX_POINT('',#69777);
#20907=VERTEX_POINT('',#69779);
#20908=VERTEX_POINT('',#69781);
#20909=VERTEX_POINT('',#69785);
#20910=VERTEX_POINT('',#69789);
#20911=VERTEX_POINT('',#69791);
#20912=VERTEX_POINT('',#69793);
#20913=VERTEX_POINT('',#69795);
#20914=VERTEX_POINT('',#69797);
#20915=VERTEX_POINT('',#69799);
#20916=VERTEX_POINT('',#69801);
#20917=VERTEX_POINT('',#69803);
#20918=VERTEX_POINT('',#69805);
#20919=VERTEX_POINT('',#69807);
#20920=VERTEX_POINT('',#69809);
#20921=VERTEX_POINT('',#69811);
#20922=VERTEX_POINT('',#69813);
#20923=VERTEX_POINT('',#69815);
#20924=VERTEX_POINT('',#69817);
#20925=VERTEX_POINT('',#69819);
#20926=VERTEX_POINT('',#69823);
#20927=VERTEX_POINT('',#69825);
#20928=VERTEX_POINT('',#69827);
#20929=VERTEX_POINT('',#69829);
#20930=VERTEX_POINT('',#69831);
#20931=VERTEX_POINT('',#69833);
#20932=VERTEX_POINT('',#69835);
#20933=VERTEX_POINT('',#69837);
#20934=VERTEX_POINT('',#69839);
#20935=VERTEX_POINT('',#69841);
#20936=VERTEX_POINT('',#69843);
#20937=VERTEX_POINT('',#69845);
#20938=VERTEX_POINT('',#69847);
#20939=VERTEX_POINT('',#69849);
#20940=VERTEX_POINT('',#69853);
#20941=VERTEX_POINT('',#69855);
#20942=VERTEX_POINT('',#69857);
#20943=VERTEX_POINT('',#69861);
#20944=VERTEX_POINT('',#69865);
#20945=VERTEX_POINT('',#69867);
#20946=VERTEX_POINT('',#69869);
#20947=VERTEX_POINT('',#69871);
#20948=VERTEX_POINT('',#69873);
#20949=VERTEX_POINT('',#69875);
#20950=VERTEX_POINT('',#69877);
#20951=VERTEX_POINT('',#69879);
#20952=VERTEX_POINT('',#69881);
#20953=VERTEX_POINT('',#69883);
#20954=VERTEX_POINT('',#69885);
#20955=VERTEX_POINT('',#69887);
#20956=VERTEX_POINT('',#69889);
#20957=VERTEX_POINT('',#69891);
#20958=VERTEX_POINT('',#69893);
#20959=VERTEX_POINT('',#69895);
#20960=VERTEX_POINT('',#69899);
#20961=VERTEX_POINT('',#69901);
#20962=VERTEX_POINT('',#69903);
#20963=VERTEX_POINT('',#69905);
#20964=VERTEX_POINT('',#69907);
#20965=VERTEX_POINT('',#69909);
#20966=VERTEX_POINT('',#69911);
#20967=VERTEX_POINT('',#69913);
#20968=VERTEX_POINT('',#69915);
#20969=VERTEX_POINT('',#69917);
#20970=VERTEX_POINT('',#69919);
#20971=VERTEX_POINT('',#69921);
#20972=VERTEX_POINT('',#69923);
#20973=VERTEX_POINT('',#69925);
#20974=VERTEX_POINT('',#69929);
#20975=VERTEX_POINT('',#69931);
#20976=VERTEX_POINT('',#69933);
#20977=VERTEX_POINT('',#69937);
#20978=VERTEX_POINT('',#69941);
#20979=VERTEX_POINT('',#69943);
#20980=VERTEX_POINT('',#69945);
#20981=VERTEX_POINT('',#69947);
#20982=VERTEX_POINT('',#69949);
#20983=VERTEX_POINT('',#69951);
#20984=VERTEX_POINT('',#69953);
#20985=VERTEX_POINT('',#69955);
#20986=VERTEX_POINT('',#69957);
#20987=VERTEX_POINT('',#69959);
#20988=VERTEX_POINT('',#69961);
#20989=VERTEX_POINT('',#69963);
#20990=VERTEX_POINT('',#69965);
#20991=VERTEX_POINT('',#69967);
#20992=VERTEX_POINT('',#69969);
#20993=VERTEX_POINT('',#69971);
#20994=VERTEX_POINT('',#69975);
#20995=VERTEX_POINT('',#69977);
#20996=VERTEX_POINT('',#69979);
#20997=VERTEX_POINT('',#69981);
#20998=VERTEX_POINT('',#69983);
#20999=VERTEX_POINT('',#69985);
#21000=VERTEX_POINT('',#69987);
#21001=VERTEX_POINT('',#69989);
#21002=VERTEX_POINT('',#69991);
#21003=VERTEX_POINT('',#69993);
#21004=VERTEX_POINT('',#69995);
#21005=VERTEX_POINT('',#69997);
#21006=VERTEX_POINT('',#69999);
#21007=VERTEX_POINT('',#70001);
#21008=VERTEX_POINT('',#70005);
#21009=VERTEX_POINT('',#70007);
#21010=VERTEX_POINT('',#70009);
#21011=VERTEX_POINT('',#70013);
#21012=VERTEX_POINT('',#70017);
#21013=VERTEX_POINT('',#70019);
#21014=VERTEX_POINT('',#70021);
#21015=VERTEX_POINT('',#70023);
#21016=VERTEX_POINT('',#70025);
#21017=VERTEX_POINT('',#70027);
#21018=VERTEX_POINT('',#70029);
#21019=VERTEX_POINT('',#70031);
#21020=VERTEX_POINT('',#70033);
#21021=VERTEX_POINT('',#70035);
#21022=VERTEX_POINT('',#70037);
#21023=VERTEX_POINT('',#70039);
#21024=VERTEX_POINT('',#70041);
#21025=VERTEX_POINT('',#70043);
#21026=VERTEX_POINT('',#70045);
#21027=VERTEX_POINT('',#70047);
#21028=VERTEX_POINT('',#70051);
#21029=VERTEX_POINT('',#70053);
#21030=VERTEX_POINT('',#70055);
#21031=VERTEX_POINT('',#70057);
#21032=VERTEX_POINT('',#70059);
#21033=VERTEX_POINT('',#70061);
#21034=VERTEX_POINT('',#70063);
#21035=VERTEX_POINT('',#70065);
#21036=VERTEX_POINT('',#70067);
#21037=VERTEX_POINT('',#70069);
#21038=VERTEX_POINT('',#70071);
#21039=VERTEX_POINT('',#70073);
#21040=VERTEX_POINT('',#70075);
#21041=VERTEX_POINT('',#70077);
#21042=VERTEX_POINT('',#70081);
#21043=VERTEX_POINT('',#70083);
#21044=VERTEX_POINT('',#70085);
#21045=VERTEX_POINT('',#70089);
#21046=VERTEX_POINT('',#70093);
#21047=VERTEX_POINT('',#70095);
#21048=VERTEX_POINT('',#70097);
#21049=VERTEX_POINT('',#70099);
#21050=VERTEX_POINT('',#70101);
#21051=VERTEX_POINT('',#70103);
#21052=VERTEX_POINT('',#70105);
#21053=VERTEX_POINT('',#70107);
#21054=VERTEX_POINT('',#70109);
#21055=VERTEX_POINT('',#70111);
#21056=VERTEX_POINT('',#70113);
#21057=VERTEX_POINT('',#70115);
#21058=VERTEX_POINT('',#70117);
#21059=VERTEX_POINT('',#70119);
#21060=VERTEX_POINT('',#70121);
#21061=VERTEX_POINT('',#70123);
#21062=VERTEX_POINT('',#70127);
#21063=VERTEX_POINT('',#70129);
#21064=VERTEX_POINT('',#70131);
#21065=VERTEX_POINT('',#70133);
#21066=VERTEX_POINT('',#70135);
#21067=VERTEX_POINT('',#70137);
#21068=VERTEX_POINT('',#70139);
#21069=VERTEX_POINT('',#70141);
#21070=VERTEX_POINT('',#70143);
#21071=VERTEX_POINT('',#70145);
#21072=VERTEX_POINT('',#70147);
#21073=VERTEX_POINT('',#70149);
#21074=VERTEX_POINT('',#70151);
#21075=VERTEX_POINT('',#70153);
#21076=VERTEX_POINT('',#70157);
#21077=VERTEX_POINT('',#70159);
#21078=VERTEX_POINT('',#70161);
#21079=VERTEX_POINT('',#70165);
#21080=VERTEX_POINT('',#70169);
#21081=VERTEX_POINT('',#70171);
#21082=VERTEX_POINT('',#70173);
#21083=VERTEX_POINT('',#70175);
#21084=VERTEX_POINT('',#70177);
#21085=VERTEX_POINT('',#70179);
#21086=VERTEX_POINT('',#70181);
#21087=VERTEX_POINT('',#70183);
#21088=VERTEX_POINT('',#70185);
#21089=VERTEX_POINT('',#70187);
#21090=VERTEX_POINT('',#70189);
#21091=VERTEX_POINT('',#70191);
#21092=VERTEX_POINT('',#70193);
#21093=VERTEX_POINT('',#70195);
#21094=VERTEX_POINT('',#70197);
#21095=VERTEX_POINT('',#70199);
#21096=VERTEX_POINT('',#70203);
#21097=VERTEX_POINT('',#70205);
#21098=VERTEX_POINT('',#70207);
#21099=VERTEX_POINT('',#70209);
#21100=VERTEX_POINT('',#70211);
#21101=VERTEX_POINT('',#70213);
#21102=VERTEX_POINT('',#70215);
#21103=VERTEX_POINT('',#70217);
#21104=VERTEX_POINT('',#70219);
#21105=VERTEX_POINT('',#70221);
#21106=VERTEX_POINT('',#70223);
#21107=VERTEX_POINT('',#70225);
#21108=VERTEX_POINT('',#70227);
#21109=VERTEX_POINT('',#70229);
#21110=VERTEX_POINT('',#70233);
#21111=VERTEX_POINT('',#70235);
#21112=VERTEX_POINT('',#70237);
#21113=VERTEX_POINT('',#70241);
#21114=VERTEX_POINT('',#70245);
#21115=VERTEX_POINT('',#70247);
#21116=VERTEX_POINT('',#70249);
#21117=VERTEX_POINT('',#70251);
#21118=VERTEX_POINT('',#70253);
#21119=VERTEX_POINT('',#70255);
#21120=VERTEX_POINT('',#70257);
#21121=VERTEX_POINT('',#70259);
#21122=VERTEX_POINT('',#70261);
#21123=VERTEX_POINT('',#70263);
#21124=VERTEX_POINT('',#70265);
#21125=VERTEX_POINT('',#70267);
#21126=VERTEX_POINT('',#70269);
#21127=VERTEX_POINT('',#70271);
#21128=VERTEX_POINT('',#70273);
#21129=VERTEX_POINT('',#70275);
#21130=VERTEX_POINT('',#70279);
#21131=VERTEX_POINT('',#70281);
#21132=VERTEX_POINT('',#70283);
#21133=VERTEX_POINT('',#70285);
#21134=VERTEX_POINT('',#70287);
#21135=VERTEX_POINT('',#70289);
#21136=VERTEX_POINT('',#70291);
#21137=VERTEX_POINT('',#70293);
#21138=VERTEX_POINT('',#70295);
#21139=VERTEX_POINT('',#70297);
#21140=VERTEX_POINT('',#70299);
#21141=VERTEX_POINT('',#70301);
#21142=VERTEX_POINT('',#70303);
#21143=VERTEX_POINT('',#70305);
#21144=VERTEX_POINT('',#70309);
#21145=VERTEX_POINT('',#70311);
#21146=VERTEX_POINT('',#70313);
#21147=VERTEX_POINT('',#70317);
#21148=VERTEX_POINT('',#70321);
#21149=VERTEX_POINT('',#70323);
#21150=VERTEX_POINT('',#70325);
#21151=VERTEX_POINT('',#70327);
#21152=VERTEX_POINT('',#70329);
#21153=VERTEX_POINT('',#70331);
#21154=VERTEX_POINT('',#70333);
#21155=VERTEX_POINT('',#70335);
#21156=VERTEX_POINT('',#70337);
#21157=VERTEX_POINT('',#70339);
#21158=VERTEX_POINT('',#70341);
#21159=VERTEX_POINT('',#70343);
#21160=VERTEX_POINT('',#70345);
#21161=VERTEX_POINT('',#70347);
#21162=VERTEX_POINT('',#70349);
#21163=VERTEX_POINT('',#70351);
#21164=VERTEX_POINT('',#70355);
#21165=VERTEX_POINT('',#70357);
#21166=VERTEX_POINT('',#70359);
#21167=VERTEX_POINT('',#70361);
#21168=VERTEX_POINT('',#70363);
#21169=VERTEX_POINT('',#70365);
#21170=VERTEX_POINT('',#70367);
#21171=VERTEX_POINT('',#70369);
#21172=VERTEX_POINT('',#70371);
#21173=VERTEX_POINT('',#70373);
#21174=VERTEX_POINT('',#70375);
#21175=VERTEX_POINT('',#70377);
#21176=VERTEX_POINT('',#70379);
#21177=VERTEX_POINT('',#70381);
#21178=VERTEX_POINT('',#70385);
#21179=VERTEX_POINT('',#70387);
#21180=VERTEX_POINT('',#70389);
#21181=VERTEX_POINT('',#70393);
#21182=VERTEX_POINT('',#70397);
#21183=VERTEX_POINT('',#70399);
#21184=VERTEX_POINT('',#70401);
#21185=VERTEX_POINT('',#70403);
#21186=VERTEX_POINT('',#70405);
#21187=VERTEX_POINT('',#70407);
#21188=VERTEX_POINT('',#70409);
#21189=VERTEX_POINT('',#70411);
#21190=VERTEX_POINT('',#70413);
#21191=VERTEX_POINT('',#70415);
#21192=VERTEX_POINT('',#70417);
#21193=VERTEX_POINT('',#70419);
#21194=VERTEX_POINT('',#70421);
#21195=VERTEX_POINT('',#70423);
#21196=VERTEX_POINT('',#70425);
#21197=VERTEX_POINT('',#70427);
#21198=VERTEX_POINT('',#70431);
#21199=VERTEX_POINT('',#70433);
#21200=VERTEX_POINT('',#70435);
#21201=VERTEX_POINT('',#70437);
#21202=VERTEX_POINT('',#70439);
#21203=VERTEX_POINT('',#70441);
#21204=VERTEX_POINT('',#70443);
#21205=VERTEX_POINT('',#70445);
#21206=VERTEX_POINT('',#70447);
#21207=VERTEX_POINT('',#70449);
#21208=VERTEX_POINT('',#70451);
#21209=VERTEX_POINT('',#70453);
#21210=VERTEX_POINT('',#70455);
#21211=VERTEX_POINT('',#70457);
#21212=VERTEX_POINT('',#70461);
#21213=VERTEX_POINT('',#70463);
#21214=VERTEX_POINT('',#70465);
#21215=VERTEX_POINT('',#70469);
#21216=VERTEX_POINT('',#70473);
#21217=VERTEX_POINT('',#70475);
#21218=VERTEX_POINT('',#70477);
#21219=VERTEX_POINT('',#70479);
#21220=VERTEX_POINT('',#70481);
#21221=VERTEX_POINT('',#70483);
#21222=VERTEX_POINT('',#70485);
#21223=VERTEX_POINT('',#70487);
#21224=VERTEX_POINT('',#70489);
#21225=VERTEX_POINT('',#70491);
#21226=VERTEX_POINT('',#70493);
#21227=VERTEX_POINT('',#70495);
#21228=VERTEX_POINT('',#70497);
#21229=VERTEX_POINT('',#70499);
#21230=VERTEX_POINT('',#70501);
#21231=VERTEX_POINT('',#70503);
#21232=VERTEX_POINT('',#70507);
#21233=VERTEX_POINT('',#70509);
#21234=VERTEX_POINT('',#70511);
#21235=VERTEX_POINT('',#70513);
#21236=VERTEX_POINT('',#70515);
#21237=VERTEX_POINT('',#70517);
#21238=VERTEX_POINT('',#70519);
#21239=VERTEX_POINT('',#70521);
#21240=VERTEX_POINT('',#70523);
#21241=VERTEX_POINT('',#70525);
#21242=VERTEX_POINT('',#70527);
#21243=VERTEX_POINT('',#70529);
#21244=VERTEX_POINT('',#70531);
#21245=VERTEX_POINT('',#70533);
#21246=VERTEX_POINT('',#70537);
#21247=VERTEX_POINT('',#70539);
#21248=VERTEX_POINT('',#70541);
#21249=VERTEX_POINT('',#70545);
#21250=VERTEX_POINT('',#70549);
#21251=VERTEX_POINT('',#70551);
#21252=VERTEX_POINT('',#70553);
#21253=VERTEX_POINT('',#70555);
#21254=VERTEX_POINT('',#70557);
#21255=VERTEX_POINT('',#70559);
#21256=VERTEX_POINT('',#70561);
#21257=VERTEX_POINT('',#70563);
#21258=VERTEX_POINT('',#70565);
#21259=VERTEX_POINT('',#70567);
#21260=VERTEX_POINT('',#70569);
#21261=VERTEX_POINT('',#70571);
#21262=VERTEX_POINT('',#70573);
#21263=VERTEX_POINT('',#70575);
#21264=VERTEX_POINT('',#70577);
#21265=VERTEX_POINT('',#70579);
#21266=VERTEX_POINT('',#70583);
#21267=VERTEX_POINT('',#70585);
#21268=VERTEX_POINT('',#70587);
#21269=VERTEX_POINT('',#70589);
#21270=VERTEX_POINT('',#70591);
#21271=VERTEX_POINT('',#70593);
#21272=VERTEX_POINT('',#70595);
#21273=VERTEX_POINT('',#70597);
#21274=VERTEX_POINT('',#70599);
#21275=VERTEX_POINT('',#70601);
#21276=VERTEX_POINT('',#70603);
#21277=VERTEX_POINT('',#70605);
#21278=VERTEX_POINT('',#70607);
#21279=VERTEX_POINT('',#70609);
#21280=VERTEX_POINT('',#70613);
#21281=VERTEX_POINT('',#70615);
#21282=VERTEX_POINT('',#70617);
#21283=VERTEX_POINT('',#70621);
#21284=VERTEX_POINT('',#70625);
#21285=VERTEX_POINT('',#70627);
#21286=VERTEX_POINT('',#70629);
#21287=VERTEX_POINT('',#70631);
#21288=VERTEX_POINT('',#70633);
#21289=VERTEX_POINT('',#70635);
#21290=VERTEX_POINT('',#70637);
#21291=VERTEX_POINT('',#70639);
#21292=VERTEX_POINT('',#70641);
#21293=VERTEX_POINT('',#70643);
#21294=VERTEX_POINT('',#70645);
#21295=VERTEX_POINT('',#70647);
#21296=VERTEX_POINT('',#70649);
#21297=VERTEX_POINT('',#70651);
#21298=VERTEX_POINT('',#70653);
#21299=VERTEX_POINT('',#70655);
#21300=VERTEX_POINT('',#70659);
#21301=VERTEX_POINT('',#70661);
#21302=VERTEX_POINT('',#70663);
#21303=VERTEX_POINT('',#70665);
#21304=VERTEX_POINT('',#70667);
#21305=VERTEX_POINT('',#70669);
#21306=VERTEX_POINT('',#70671);
#21307=VERTEX_POINT('',#70673);
#21308=VERTEX_POINT('',#70675);
#21309=VERTEX_POINT('',#70677);
#21310=VERTEX_POINT('',#70679);
#21311=VERTEX_POINT('',#70681);
#21312=VERTEX_POINT('',#70683);
#21313=VERTEX_POINT('',#70685);
#21314=VERTEX_POINT('',#70689);
#21315=VERTEX_POINT('',#70691);
#21316=VERTEX_POINT('',#70693);
#21317=VERTEX_POINT('',#70697);
#21318=VERTEX_POINT('',#70701);
#21319=VERTEX_POINT('',#70703);
#21320=VERTEX_POINT('',#70705);
#21321=VERTEX_POINT('',#70707);
#21322=VERTEX_POINT('',#70709);
#21323=VERTEX_POINT('',#70711);
#21324=VERTEX_POINT('',#70713);
#21325=VERTEX_POINT('',#70715);
#21326=VERTEX_POINT('',#70717);
#21327=VERTEX_POINT('',#70719);
#21328=VERTEX_POINT('',#70721);
#21329=VERTEX_POINT('',#70723);
#21330=VERTEX_POINT('',#70725);
#21331=VERTEX_POINT('',#70727);
#21332=VERTEX_POINT('',#70729);
#21333=VERTEX_POINT('',#70731);
#21334=VERTEX_POINT('',#70735);
#21335=VERTEX_POINT('',#70737);
#21336=VERTEX_POINT('',#70739);
#21337=VERTEX_POINT('',#70741);
#21338=VERTEX_POINT('',#70743);
#21339=VERTEX_POINT('',#70745);
#21340=VERTEX_POINT('',#70747);
#21341=VERTEX_POINT('',#70749);
#21342=VERTEX_POINT('',#70751);
#21343=VERTEX_POINT('',#70753);
#21344=VERTEX_POINT('',#70755);
#21345=VERTEX_POINT('',#70757);
#21346=VERTEX_POINT('',#70759);
#21347=VERTEX_POINT('',#70761);
#21348=VERTEX_POINT('',#70765);
#21349=VERTEX_POINT('',#70767);
#21350=VERTEX_POINT('',#70769);
#21351=VERTEX_POINT('',#70773);
#21352=VERTEX_POINT('',#70777);
#21353=VERTEX_POINT('',#70779);
#21354=VERTEX_POINT('',#70781);
#21355=VERTEX_POINT('',#70783);
#21356=VERTEX_POINT('',#70785);
#21357=VERTEX_POINT('',#70787);
#21358=VERTEX_POINT('',#70789);
#21359=VERTEX_POINT('',#70791);
#21360=VERTEX_POINT('',#70793);
#21361=VERTEX_POINT('',#70795);
#21362=VERTEX_POINT('',#70797);
#21363=VERTEX_POINT('',#70799);
#21364=VERTEX_POINT('',#70801);
#21365=VERTEX_POINT('',#70803);
#21366=VERTEX_POINT('',#70805);
#21367=VERTEX_POINT('',#70807);
#21368=VERTEX_POINT('',#70811);
#21369=VERTEX_POINT('',#70813);
#21370=VERTEX_POINT('',#70815);
#21371=VERTEX_POINT('',#70817);
#21372=VERTEX_POINT('',#70819);
#21373=VERTEX_POINT('',#70821);
#21374=VERTEX_POINT('',#70823);
#21375=VERTEX_POINT('',#70825);
#21376=VERTEX_POINT('',#70827);
#21377=VERTEX_POINT('',#70829);
#21378=VERTEX_POINT('',#70831);
#21379=VERTEX_POINT('',#70833);
#21380=VERTEX_POINT('',#70835);
#21381=VERTEX_POINT('',#70837);
#21382=VERTEX_POINT('',#70841);
#21383=VERTEX_POINT('',#70843);
#21384=VERTEX_POINT('',#70845);
#21385=VERTEX_POINT('',#70849);
#21386=VERTEX_POINT('',#70853);
#21387=VERTEX_POINT('',#70855);
#21388=VERTEX_POINT('',#70857);
#21389=VERTEX_POINT('',#70859);
#21390=VERTEX_POINT('',#70861);
#21391=VERTEX_POINT('',#70863);
#21392=VERTEX_POINT('',#70865);
#21393=VERTEX_POINT('',#70867);
#21394=VERTEX_POINT('',#70869);
#21395=VERTEX_POINT('',#70871);
#21396=VERTEX_POINT('',#70873);
#21397=VERTEX_POINT('',#70875);
#21398=VERTEX_POINT('',#70877);
#21399=VERTEX_POINT('',#70879);
#21400=VERTEX_POINT('',#70881);
#21401=VERTEX_POINT('',#70883);
#21402=VERTEX_POINT('',#70887);
#21403=VERTEX_POINT('',#70889);
#21404=VERTEX_POINT('',#70891);
#21405=VERTEX_POINT('',#70893);
#21406=VERTEX_POINT('',#70895);
#21407=VERTEX_POINT('',#70897);
#21408=VERTEX_POINT('',#70899);
#21409=VERTEX_POINT('',#70901);
#21410=VERTEX_POINT('',#70903);
#21411=VERTEX_POINT('',#70905);
#21412=VERTEX_POINT('',#70907);
#21413=VERTEX_POINT('',#70909);
#21414=VERTEX_POINT('',#70911);
#21415=VERTEX_POINT('',#70913);
#21416=VERTEX_POINT('',#70917);
#21417=VERTEX_POINT('',#70919);
#21418=VERTEX_POINT('',#70921);
#21419=VERTEX_POINT('',#70925);
#21420=VERTEX_POINT('',#70929);
#21421=VERTEX_POINT('',#70931);
#21422=VERTEX_POINT('',#70933);
#21423=VERTEX_POINT('',#70935);
#21424=VERTEX_POINT('',#70937);
#21425=VERTEX_POINT('',#70939);
#21426=VERTEX_POINT('',#70941);
#21427=VERTEX_POINT('',#70943);
#21428=VERTEX_POINT('',#70945);
#21429=VERTEX_POINT('',#70947);
#21430=VERTEX_POINT('',#70949);
#21431=VERTEX_POINT('',#70951);
#21432=VERTEX_POINT('',#70953);
#21433=VERTEX_POINT('',#70955);
#21434=VERTEX_POINT('',#70957);
#21435=VERTEX_POINT('',#70959);
#21436=VERTEX_POINT('',#70963);
#21437=VERTEX_POINT('',#70965);
#21438=VERTEX_POINT('',#70967);
#21439=VERTEX_POINT('',#70969);
#21440=VERTEX_POINT('',#70971);
#21441=VERTEX_POINT('',#70973);
#21442=VERTEX_POINT('',#70975);
#21443=VERTEX_POINT('',#70977);
#21444=VERTEX_POINT('',#70979);
#21445=VERTEX_POINT('',#70981);
#21446=VERTEX_POINT('',#70983);
#21447=VERTEX_POINT('',#70985);
#21448=VERTEX_POINT('',#70987);
#21449=VERTEX_POINT('',#70989);
#21450=VERTEX_POINT('',#70993);
#21451=VERTEX_POINT('',#70995);
#21452=VERTEX_POINT('',#70997);
#21453=VERTEX_POINT('',#71001);
#21454=VERTEX_POINT('',#71005);
#21455=VERTEX_POINT('',#71007);
#21456=VERTEX_POINT('',#71009);
#21457=VERTEX_POINT('',#71011);
#21458=VERTEX_POINT('',#71013);
#21459=VERTEX_POINT('',#71015);
#21460=VERTEX_POINT('',#71017);
#21461=VERTEX_POINT('',#71019);
#21462=VERTEX_POINT('',#71021);
#21463=VERTEX_POINT('',#71023);
#21464=VERTEX_POINT('',#71025);
#21465=VERTEX_POINT('',#71027);
#21466=VERTEX_POINT('',#71029);
#21467=VERTEX_POINT('',#71031);
#21468=VERTEX_POINT('',#71033);
#21469=VERTEX_POINT('',#71035);
#21470=VERTEX_POINT('',#71039);
#21471=VERTEX_POINT('',#71041);
#21472=VERTEX_POINT('',#71043);
#21473=VERTEX_POINT('',#71045);
#21474=VERTEX_POINT('',#71047);
#21475=VERTEX_POINT('',#71049);
#21476=VERTEX_POINT('',#71051);
#21477=VERTEX_POINT('',#71053);
#21478=VERTEX_POINT('',#71055);
#21479=VERTEX_POINT('',#71057);
#21480=VERTEX_POINT('',#71059);
#21481=VERTEX_POINT('',#71061);
#21482=VERTEX_POINT('',#71063);
#21483=VERTEX_POINT('',#71065);
#21484=VERTEX_POINT('',#71069);
#21485=VERTEX_POINT('',#71071);
#21486=VERTEX_POINT('',#71073);
#21487=VERTEX_POINT('',#71077);
#21488=VERTEX_POINT('',#71081);
#21489=VERTEX_POINT('',#71083);
#21490=VERTEX_POINT('',#71085);
#21491=VERTEX_POINT('',#71087);
#21492=VERTEX_POINT('',#71089);
#21493=VERTEX_POINT('',#71091);
#21494=VERTEX_POINT('',#71093);
#21495=VERTEX_POINT('',#71095);
#21496=VERTEX_POINT('',#71097);
#21497=VERTEX_POINT('',#71099);
#21498=VERTEX_POINT('',#71101);
#21499=VERTEX_POINT('',#71103);
#21500=VERTEX_POINT('',#71105);
#21501=VERTEX_POINT('',#71107);
#21502=VERTEX_POINT('',#71109);
#21503=VERTEX_POINT('',#71111);
#21504=VERTEX_POINT('',#71115);
#21505=VERTEX_POINT('',#71117);
#21506=VERTEX_POINT('',#71119);
#21507=VERTEX_POINT('',#71121);
#21508=VERTEX_POINT('',#71123);
#21509=VERTEX_POINT('',#71125);
#21510=VERTEX_POINT('',#71127);
#21511=VERTEX_POINT('',#71129);
#21512=VERTEX_POINT('',#71131);
#21513=VERTEX_POINT('',#71133);
#21514=VERTEX_POINT('',#71135);
#21515=VERTEX_POINT('',#71137);
#21516=VERTEX_POINT('',#71139);
#21517=VERTEX_POINT('',#71141);
#21518=VERTEX_POINT('',#71145);
#21519=VERTEX_POINT('',#71147);
#21520=VERTEX_POINT('',#71149);
#21521=VERTEX_POINT('',#71153);
#21522=VERTEX_POINT('',#71157);
#21523=VERTEX_POINT('',#71159);
#21524=VERTEX_POINT('',#71161);
#21525=VERTEX_POINT('',#71163);
#21526=VERTEX_POINT('',#71165);
#21527=VERTEX_POINT('',#71167);
#21528=VERTEX_POINT('',#71169);
#21529=VERTEX_POINT('',#71171);
#21530=VERTEX_POINT('',#71173);
#21531=VERTEX_POINT('',#71175);
#21532=VERTEX_POINT('',#71177);
#21533=VERTEX_POINT('',#71179);
#21534=VERTEX_POINT('',#71181);
#21535=VERTEX_POINT('',#71183);
#21536=VERTEX_POINT('',#71185);
#21537=VERTEX_POINT('',#71187);
#21538=VERTEX_POINT('',#71191);
#21539=VERTEX_POINT('',#71193);
#21540=VERTEX_POINT('',#71195);
#21541=VERTEX_POINT('',#71197);
#21542=VERTEX_POINT('',#71199);
#21543=VERTEX_POINT('',#71201);
#21544=VERTEX_POINT('',#71203);
#21545=VERTEX_POINT('',#71205);
#21546=VERTEX_POINT('',#71207);
#21547=VERTEX_POINT('',#71209);
#21548=VERTEX_POINT('',#71211);
#21549=VERTEX_POINT('',#71213);
#21550=VERTEX_POINT('',#71215);
#21551=VERTEX_POINT('',#71217);
#21552=VERTEX_POINT('',#71221);
#21553=VERTEX_POINT('',#71223);
#21554=VERTEX_POINT('',#71225);
#21555=VERTEX_POINT('',#71229);
#21556=VERTEX_POINT('',#71233);
#21557=VERTEX_POINT('',#71235);
#21558=VERTEX_POINT('',#71237);
#21559=VERTEX_POINT('',#71239);
#21560=VERTEX_POINT('',#71241);
#21561=VERTEX_POINT('',#71243);
#21562=VERTEX_POINT('',#71245);
#21563=VERTEX_POINT('',#71247);
#21564=VERTEX_POINT('',#71249);
#21565=VERTEX_POINT('',#71251);
#21566=VERTEX_POINT('',#71253);
#21567=VERTEX_POINT('',#71255);
#21568=VERTEX_POINT('',#71257);
#21569=VERTEX_POINT('',#71259);
#21570=VERTEX_POINT('',#71261);
#21571=VERTEX_POINT('',#71263);
#21572=VERTEX_POINT('',#71267);
#21573=VERTEX_POINT('',#71269);
#21574=VERTEX_POINT('',#71271);
#21575=VERTEX_POINT('',#71273);
#21576=VERTEX_POINT('',#71275);
#21577=VERTEX_POINT('',#71277);
#21578=VERTEX_POINT('',#71279);
#21579=VERTEX_POINT('',#71281);
#21580=VERTEX_POINT('',#71283);
#21581=VERTEX_POINT('',#71285);
#21582=VERTEX_POINT('',#71287);
#21583=VERTEX_POINT('',#71289);
#21584=VERTEX_POINT('',#71291);
#21585=VERTEX_POINT('',#71293);
#21586=VERTEX_POINT('',#71297);
#21587=VERTEX_POINT('',#71299);
#21588=VERTEX_POINT('',#71301);
#21589=VERTEX_POINT('',#71305);
#21590=VERTEX_POINT('',#71309);
#21591=VERTEX_POINT('',#71311);
#21592=VERTEX_POINT('',#71313);
#21593=VERTEX_POINT('',#71315);
#21594=VERTEX_POINT('',#71317);
#21595=VERTEX_POINT('',#71319);
#21596=VERTEX_POINT('',#71321);
#21597=VERTEX_POINT('',#71323);
#21598=VERTEX_POINT('',#71325);
#21599=VERTEX_POINT('',#71327);
#21600=VERTEX_POINT('',#71329);
#21601=VERTEX_POINT('',#71331);
#21602=VERTEX_POINT('',#71333);
#21603=VERTEX_POINT('',#71335);
#21604=VERTEX_POINT('',#71337);
#21605=VERTEX_POINT('',#71339);
#21606=VERTEX_POINT('',#71343);
#21607=VERTEX_POINT('',#71345);
#21608=VERTEX_POINT('',#71347);
#21609=VERTEX_POINT('',#71349);
#21610=VERTEX_POINT('',#71351);
#21611=VERTEX_POINT('',#71353);
#21612=VERTEX_POINT('',#71355);
#21613=VERTEX_POINT('',#71357);
#21614=VERTEX_POINT('',#71359);
#21615=VERTEX_POINT('',#71361);
#21616=VERTEX_POINT('',#71363);
#21617=VERTEX_POINT('',#71365);
#21618=VERTEX_POINT('',#71367);
#21619=VERTEX_POINT('',#71369);
#21620=VERTEX_POINT('',#71373);
#21621=VERTEX_POINT('',#71375);
#21622=VERTEX_POINT('',#71377);
#21623=VERTEX_POINT('',#71381);
#21624=VERTEX_POINT('',#71385);
#21625=VERTEX_POINT('',#71387);
#21626=VERTEX_POINT('',#71389);
#21627=VERTEX_POINT('',#71391);
#21628=VERTEX_POINT('',#71393);
#21629=VERTEX_POINT('',#71395);
#21630=VERTEX_POINT('',#71397);
#21631=VERTEX_POINT('',#71399);
#21632=VERTEX_POINT('',#71401);
#21633=VERTEX_POINT('',#71403);
#21634=VERTEX_POINT('',#71405);
#21635=VERTEX_POINT('',#71407);
#21636=VERTEX_POINT('',#71409);
#21637=VERTEX_POINT('',#71411);
#21638=VERTEX_POINT('',#71413);
#21639=VERTEX_POINT('',#71415);
#21640=VERTEX_POINT('',#71419);
#21641=VERTEX_POINT('',#71421);
#21642=VERTEX_POINT('',#71423);
#21643=VERTEX_POINT('',#71425);
#21644=VERTEX_POINT('',#71427);
#21645=VERTEX_POINT('',#71429);
#21646=VERTEX_POINT('',#71431);
#21647=VERTEX_POINT('',#71433);
#21648=VERTEX_POINT('',#71435);
#21649=VERTEX_POINT('',#71437);
#21650=VERTEX_POINT('',#71439);
#21651=VERTEX_POINT('',#71441);
#21652=VERTEX_POINT('',#71443);
#21653=VERTEX_POINT('',#71445);
#21654=VERTEX_POINT('',#71449);
#21655=VERTEX_POINT('',#71451);
#21656=VERTEX_POINT('',#71453);
#21657=VERTEX_POINT('',#71457);
#21658=VERTEX_POINT('',#71461);
#21659=VERTEX_POINT('',#71463);
#21660=VERTEX_POINT('',#71465);
#21661=VERTEX_POINT('',#71467);
#21662=VERTEX_POINT('',#71469);
#21663=VERTEX_POINT('',#71471);
#21664=VERTEX_POINT('',#71473);
#21665=VERTEX_POINT('',#71475);
#21666=VERTEX_POINT('',#71477);
#21667=VERTEX_POINT('',#71479);
#21668=VERTEX_POINT('',#71481);
#21669=VERTEX_POINT('',#71483);
#21670=VERTEX_POINT('',#71485);
#21671=VERTEX_POINT('',#71487);
#21672=VERTEX_POINT('',#71489);
#21673=VERTEX_POINT('',#71491);
#21674=VERTEX_POINT('',#71495);
#21675=VERTEX_POINT('',#71497);
#21676=VERTEX_POINT('',#71499);
#21677=VERTEX_POINT('',#71501);
#21678=VERTEX_POINT('',#71503);
#21679=VERTEX_POINT('',#71505);
#21680=VERTEX_POINT('',#71507);
#21681=VERTEX_POINT('',#71509);
#21682=VERTEX_POINT('',#71511);
#21683=VERTEX_POINT('',#71513);
#21684=VERTEX_POINT('',#71515);
#21685=VERTEX_POINT('',#71517);
#21686=VERTEX_POINT('',#71519);
#21687=VERTEX_POINT('',#71521);
#21688=VERTEX_POINT('',#71525);
#21689=VERTEX_POINT('',#71527);
#21690=VERTEX_POINT('',#71529);
#21691=VERTEX_POINT('',#71533);
#21692=VERTEX_POINT('',#71537);
#21693=VERTEX_POINT('',#71538);
#21694=VERTEX_POINT('',#71547);
#21695=VERTEX_POINT('',#71548);
#21696=VERTEX_POINT('',#71557);
#21697=VERTEX_POINT('',#71558);
#21698=VERTEX_POINT('',#71567);
#21699=VERTEX_POINT('',#71568);
#21700=VERTEX_POINT('',#71577);
#21701=VERTEX_POINT('',#71578);
#21702=VERTEX_POINT('',#71587);
#21703=VERTEX_POINT('',#71588);
#21704=VERTEX_POINT('',#71597);
#21705=VERTEX_POINT('',#71598);
#21706=VERTEX_POINT('',#71607);
#21707=VERTEX_POINT('',#71608);
#21708=VERTEX_POINT('',#71617);
#21709=VERTEX_POINT('',#71618);
#21710=VERTEX_POINT('',#71627);
#21711=VERTEX_POINT('',#71628);
#21712=VERTEX_POINT('',#71637);
#21713=VERTEX_POINT('',#71638);
#21714=VERTEX_POINT('',#71647);
#21715=VERTEX_POINT('',#71648);
#21716=VERTEX_POINT('',#71657);
#21717=VERTEX_POINT('',#71658);
#21718=VERTEX_POINT('',#71667);
#21719=VERTEX_POINT('',#71668);
#21720=VERTEX_POINT('',#71677);
#21721=VERTEX_POINT('',#71678);
#21722=VERTEX_POINT('',#71687);
#21723=VERTEX_POINT('',#71688);
#21724=VERTEX_POINT('',#71697);
#21725=VERTEX_POINT('',#71698);
#21726=VERTEX_POINT('',#71707);
#21727=VERTEX_POINT('',#71708);
#21728=VERTEX_POINT('',#71717);
#21729=VERTEX_POINT('',#71718);
#21730=VERTEX_POINT('',#71727);
#21731=VERTEX_POINT('',#71728);
#21732=VERTEX_POINT('',#71737);
#21733=VERTEX_POINT('',#71738);
#21734=VERTEX_POINT('',#71747);
#21735=VERTEX_POINT('',#71748);
#21736=VERTEX_POINT('',#71757);
#21737=VERTEX_POINT('',#71758);
#21738=VERTEX_POINT('',#71767);
#21739=VERTEX_POINT('',#71768);
#21740=VERTEX_POINT('',#71777);
#21741=VERTEX_POINT('',#71778);
#21742=VERTEX_POINT('',#71787);
#21743=VERTEX_POINT('',#71788);
#21744=VERTEX_POINT('',#71797);
#21745=VERTEX_POINT('',#71798);
#21746=VERTEX_POINT('',#71807);
#21747=VERTEX_POINT('',#71808);
#21748=VERTEX_POINT('',#71817);
#21749=VERTEX_POINT('',#71818);
#21750=VERTEX_POINT('',#71827);
#21751=VERTEX_POINT('',#71828);
#21752=VERTEX_POINT('',#71837);
#21753=VERTEX_POINT('',#71838);
#21754=VERTEX_POINT('',#71847);
#21755=VERTEX_POINT('',#71848);
#21756=VERTEX_POINT('',#71857);
#21757=VERTEX_POINT('',#71858);
#21758=VERTEX_POINT('',#71867);
#21759=VERTEX_POINT('',#71868);
#21760=VERTEX_POINT('',#71877);
#21761=VERTEX_POINT('',#71878);
#21762=VERTEX_POINT('',#71887);
#21763=VERTEX_POINT('',#71888);
#21764=VERTEX_POINT('',#71897);
#21765=VERTEX_POINT('',#71899);
#21766=VERTEX_POINT('',#71901);
#21767=VERTEX_POINT('',#71905);
#21768=VERTEX_POINT('',#71909);
#21769=VERTEX_POINT('',#71911);
#21770=VERTEX_POINT('',#71913);
#21771=VERTEX_POINT('',#71917);
#21772=VERTEX_POINT('',#71921);
#21773=VERTEX_POINT('',#71923);
#21774=VERTEX_POINT('',#71925);
#21775=VERTEX_POINT('',#71929);
#21776=VERTEX_POINT('',#71933);
#21777=VERTEX_POINT('',#71935);
#21778=VERTEX_POINT('',#71937);
#21779=VERTEX_POINT('',#71941);
#21780=VERTEX_POINT('',#71945);
#21781=VERTEX_POINT('',#71947);
#21782=VERTEX_POINT('',#71949);
#21783=VERTEX_POINT('',#71953);
#21784=VERTEX_POINT('',#71957);
#21785=VERTEX_POINT('',#71959);
#21786=VERTEX_POINT('',#71961);
#21787=VERTEX_POINT('',#71965);
#21788=VERTEX_POINT('',#71969);
#21789=VERTEX_POINT('',#71971);
#21790=VERTEX_POINT('',#71973);
#21791=VERTEX_POINT('',#71977);
#21792=VERTEX_POINT('',#71981);
#21793=VERTEX_POINT('',#71983);
#21794=VERTEX_POINT('',#71985);
#21795=VERTEX_POINT('',#71989);
#21796=VERTEX_POINT('',#71993);
#21797=VERTEX_POINT('',#71995);
#21798=VERTEX_POINT('',#71997);
#21799=VERTEX_POINT('',#72001);
#21800=VERTEX_POINT('',#72005);
#21801=VERTEX_POINT('',#72007);
#21802=VERTEX_POINT('',#72009);
#21803=VERTEX_POINT('',#72013);
#21804=VERTEX_POINT('',#72017);
#21805=VERTEX_POINT('',#72019);
#21806=VERTEX_POINT('',#72021);
#21807=VERTEX_POINT('',#72025);
#21808=VERTEX_POINT('',#72029);
#21809=VERTEX_POINT('',#72031);
#21810=VERTEX_POINT('',#72033);
#21811=VERTEX_POINT('',#72037);
#21812=VERTEX_POINT('',#72041);
#21813=VERTEX_POINT('',#72043);
#21814=VERTEX_POINT('',#72045);
#21815=VERTEX_POINT('',#72049);
#21816=VERTEX_POINT('',#72053);
#21817=VERTEX_POINT('',#72055);
#21818=VERTEX_POINT('',#72057);
#21819=VERTEX_POINT('',#72061);
#21820=VERTEX_POINT('',#72065);
#21821=VERTEX_POINT('',#72067);
#21822=VERTEX_POINT('',#72069);
#21823=VERTEX_POINT('',#72073);
#21824=VERTEX_POINT('',#72077);
#21825=VERTEX_POINT('',#72079);
#21826=VERTEX_POINT('',#72081);
#21827=VERTEX_POINT('',#72085);
#21828=VERTEX_POINT('',#72089);
#21829=VERTEX_POINT('',#72091);
#21830=VERTEX_POINT('',#72093);
#21831=VERTEX_POINT('',#72097);
#21832=VERTEX_POINT('',#72101);
#21833=VERTEX_POINT('',#72103);
#21834=VERTEX_POINT('',#72105);
#21835=VERTEX_POINT('',#72109);
#21836=VERTEX_POINT('',#72113);
#21837=VERTEX_POINT('',#72115);
#21838=VERTEX_POINT('',#72117);
#21839=VERTEX_POINT('',#72121);
#21840=VERTEX_POINT('',#72125);
#21841=VERTEX_POINT('',#72127);
#21842=VERTEX_POINT('',#72129);
#21843=VERTEX_POINT('',#72133);
#21844=VERTEX_POINT('',#72137);
#21845=VERTEX_POINT('',#72139);
#21846=VERTEX_POINT('',#72141);
#21847=VERTEX_POINT('',#72145);
#21848=VERTEX_POINT('',#72149);
#21849=VERTEX_POINT('',#72151);
#21850=VERTEX_POINT('',#72153);
#21851=VERTEX_POINT('',#72157);
#21852=VERTEX_POINT('',#72161);
#21853=VERTEX_POINT('',#72163);
#21854=VERTEX_POINT('',#72165);
#21855=VERTEX_POINT('',#72169);
#21856=VERTEX_POINT('',#72173);
#21857=VERTEX_POINT('',#72175);
#21858=VERTEX_POINT('',#72177);
#21859=VERTEX_POINT('',#72181);
#21860=VERTEX_POINT('',#72185);
#21861=VERTEX_POINT('',#72187);
#21862=VERTEX_POINT('',#72189);
#21863=VERTEX_POINT('',#72193);
#21864=VERTEX_POINT('',#72197);
#21865=VERTEX_POINT('',#72199);
#21866=VERTEX_POINT('',#72201);
#21867=VERTEX_POINT('',#72205);
#21868=VERTEX_POINT('',#72209);
#21869=VERTEX_POINT('',#72211);
#21870=VERTEX_POINT('',#72213);
#21871=VERTEX_POINT('',#72217);
#21872=VERTEX_POINT('',#72221);
#21873=VERTEX_POINT('',#72223);
#21874=VERTEX_POINT('',#72225);
#21875=VERTEX_POINT('',#72229);
#21876=VERTEX_POINT('',#72233);
#21877=VERTEX_POINT('',#72235);
#21878=VERTEX_POINT('',#72237);
#21879=VERTEX_POINT('',#72241);
#21880=VERTEX_POINT('',#72245);
#21881=VERTEX_POINT('',#72247);
#21882=VERTEX_POINT('',#72249);
#21883=VERTEX_POINT('',#72253);
#21884=VERTEX_POINT('',#72257);
#21885=VERTEX_POINT('',#72259);
#21886=VERTEX_POINT('',#72261);
#21887=VERTEX_POINT('',#72265);
#21888=VERTEX_POINT('',#72269);
#21889=VERTEX_POINT('',#72271);
#21890=VERTEX_POINT('',#72273);
#21891=VERTEX_POINT('',#72277);
#21892=VERTEX_POINT('',#72281);
#21893=VERTEX_POINT('',#72283);
#21894=VERTEX_POINT('',#72285);
#21895=VERTEX_POINT('',#72289);
#21896=VERTEX_POINT('',#72293);
#21897=VERTEX_POINT('',#72295);
#21898=VERTEX_POINT('',#72297);
#21899=VERTEX_POINT('',#72301);
#21900=VERTEX_POINT('',#72305);
#21901=VERTEX_POINT('',#72307);
#21902=VERTEX_POINT('',#72309);
#21903=VERTEX_POINT('',#72313);
#21904=VERTEX_POINT('',#72317);
#21905=VERTEX_POINT('',#72319);
#21906=VERTEX_POINT('',#72321);
#21907=VERTEX_POINT('',#72325);
#21908=VERTEX_POINT('',#72329);
#21909=VERTEX_POINT('',#72333);
#21910=VERTEX_POINT('',#72337);
#21911=VERTEX_POINT('',#72341);
#21912=VERTEX_POINT('',#72345);
#21913=VERTEX_POINT('',#72349);
#21914=VERTEX_POINT('',#72353);
#21915=VERTEX_POINT('',#72357);
#21916=VERTEX_POINT('',#72361);
#21917=VERTEX_POINT('',#72365);
#21918=VERTEX_POINT('',#72369);
#21919=VERTEX_POINT('',#72373);
#21920=VERTEX_POINT('',#72377);
#21921=VERTEX_POINT('',#72381);
#21922=VERTEX_POINT('',#72385);
#21923=VERTEX_POINT('',#72389);
#21924=VERTEX_POINT('',#72393);
#21925=VERTEX_POINT('',#72397);
#21926=VERTEX_POINT('',#72401);
#21927=VERTEX_POINT('',#72405);
#21928=VERTEX_POINT('',#72409);
#21929=VERTEX_POINT('',#72413);
#21930=VERTEX_POINT('',#72417);
#21931=VERTEX_POINT('',#72421);
#21932=VERTEX_POINT('',#72425);
#21933=VERTEX_POINT('',#72429);
#21934=VERTEX_POINT('',#72433);
#21935=VERTEX_POINT('',#72437);
#21936=VERTEX_POINT('',#72441);
#21937=VERTEX_POINT('',#72445);
#21938=VERTEX_POINT('',#72449);
#21939=VERTEX_POINT('',#72453);
#21940=VERTEX_POINT('',#72457);
#21941=VERTEX_POINT('',#72461);
#21942=VERTEX_POINT('',#72465);
#21943=VERTEX_POINT('',#72469);
#21944=VERTEX_POINT('',#72473);
#21945=VERTEX_POINT('',#72475);
#21946=VERTEX_POINT('',#72477);
#21947=VERTEX_POINT('',#72483);
#21948=VERTEX_POINT('',#72485);
#21949=VERTEX_POINT('',#72487);
#21950=VERTEX_POINT('',#72493);
#21951=VERTEX_POINT('',#72495);
#21952=VERTEX_POINT('',#72497);
#21953=VERTEX_POINT('',#72503);
#21954=VERTEX_POINT('',#72505);
#21955=VERTEX_POINT('',#72507);
#21956=VERTEX_POINT('',#72513);
#21957=VERTEX_POINT('',#72515);
#21958=VERTEX_POINT('',#72517);
#21959=VERTEX_POINT('',#72523);
#21960=VERTEX_POINT('',#72525);
#21961=VERTEX_POINT('',#72527);
#21962=VERTEX_POINT('',#72533);
#21963=VERTEX_POINT('',#72535);
#21964=VERTEX_POINT('',#72537);
#21965=VERTEX_POINT('',#72543);
#21966=VERTEX_POINT('',#72545);
#21967=VERTEX_POINT('',#72547);
#21968=VERTEX_POINT('',#72553);
#21969=VERTEX_POINT('',#72555);
#21970=VERTEX_POINT('',#72557);
#21971=VERTEX_POINT('',#72563);
#21972=VERTEX_POINT('',#72565);
#21973=VERTEX_POINT('',#72567);
#21974=VERTEX_POINT('',#72573);
#21975=VERTEX_POINT('',#72575);
#21976=VERTEX_POINT('',#72577);
#21977=VERTEX_POINT('',#72583);
#21978=VERTEX_POINT('',#72585);
#21979=VERTEX_POINT('',#72587);
#21980=VERTEX_POINT('',#72593);
#21981=VERTEX_POINT('',#72595);
#21982=VERTEX_POINT('',#72597);
#21983=VERTEX_POINT('',#72603);
#21984=VERTEX_POINT('',#72605);
#21985=VERTEX_POINT('',#72607);
#21986=VERTEX_POINT('',#72613);
#21987=VERTEX_POINT('',#72615);
#21988=VERTEX_POINT('',#72617);
#21989=VERTEX_POINT('',#72623);
#21990=VERTEX_POINT('',#72625);
#21991=VERTEX_POINT('',#72627);
#21992=VERTEX_POINT('',#72633);
#21993=VERTEX_POINT('',#72635);
#21994=VERTEX_POINT('',#72637);
#21995=VERTEX_POINT('',#72643);
#21996=VERTEX_POINT('',#72645);
#21997=VERTEX_POINT('',#72647);
#21998=VERTEX_POINT('',#72653);
#21999=VERTEX_POINT('',#72655);
#22000=VERTEX_POINT('',#72657);
#22001=VERTEX_POINT('',#72663);
#22002=VERTEX_POINT('',#72665);
#22003=VERTEX_POINT('',#72667);
#22004=VERTEX_POINT('',#72673);
#22005=VERTEX_POINT('',#72675);
#22006=VERTEX_POINT('',#72677);
#22007=VERTEX_POINT('',#72683);
#22008=VERTEX_POINT('',#72685);
#22009=VERTEX_POINT('',#72687);
#22010=VERTEX_POINT('',#72693);
#22011=VERTEX_POINT('',#72695);
#22012=VERTEX_POINT('',#72697);
#22013=VERTEX_POINT('',#72703);
#22014=VERTEX_POINT('',#72705);
#22015=VERTEX_POINT('',#72707);
#22016=VERTEX_POINT('',#72713);
#22017=VERTEX_POINT('',#72715);
#22018=VERTEX_POINT('',#72717);
#22019=VERTEX_POINT('',#72723);
#22020=VERTEX_POINT('',#72725);
#22021=VERTEX_POINT('',#72727);
#22022=VERTEX_POINT('',#72733);
#22023=VERTEX_POINT('',#72735);
#22024=VERTEX_POINT('',#72737);
#22025=VERTEX_POINT('',#72743);
#22026=VERTEX_POINT('',#72745);
#22027=VERTEX_POINT('',#72747);
#22028=VERTEX_POINT('',#72753);
#22029=VERTEX_POINT('',#72755);
#22030=VERTEX_POINT('',#72757);
#22031=VERTEX_POINT('',#72763);
#22032=VERTEX_POINT('',#72765);
#22033=VERTEX_POINT('',#72767);
#22034=VERTEX_POINT('',#72773);
#22035=VERTEX_POINT('',#72775);
#22036=VERTEX_POINT('',#72777);
#22037=VERTEX_POINT('',#72783);
#22038=VERTEX_POINT('',#72785);
#22039=VERTEX_POINT('',#72787);
#22040=VERTEX_POINT('',#72793);
#22041=VERTEX_POINT('',#72795);
#22042=VERTEX_POINT('',#72797);
#22043=VERTEX_POINT('',#72803);
#22044=VERTEX_POINT('',#72805);
#22045=VERTEX_POINT('',#72807);
#22046=VERTEX_POINT('',#72813);
#22047=VERTEX_POINT('',#72815);
#22048=VERTEX_POINT('',#72817);
#22049=VERTEX_POINT('',#72823);
#22050=VERTEX_POINT('',#72829);
#22051=VERTEX_POINT('',#72833);
#22052=VERTEX_POINT('',#72837);
#22053=VERTEX_POINT('',#72841);
#22054=VERTEX_POINT('',#72845);
#22055=VERTEX_POINT('',#72849);
#22056=VERTEX_POINT('',#72853);
#22057=VERTEX_POINT('',#72857);
#22058=VERTEX_POINT('',#72861);
#22059=VERTEX_POINT('',#72865);
#22060=VERTEX_POINT('',#72869);
#22061=VERTEX_POINT('',#72873);
#22062=VERTEX_POINT('',#72877);
#22063=VERTEX_POINT('',#72881);
#22064=VERTEX_POINT('',#72885);
#22065=VERTEX_POINT('',#72889);
#22066=VERTEX_POINT('',#72893);
#22067=VERTEX_POINT('',#72897);
#22068=VERTEX_POINT('',#72901);
#22069=VERTEX_POINT('',#72905);
#22070=VERTEX_POINT('',#72909);
#22071=VERTEX_POINT('',#72913);
#22072=VERTEX_POINT('',#72917);
#22073=VERTEX_POINT('',#72921);
#22074=VERTEX_POINT('',#72925);
#22075=VERTEX_POINT('',#72929);
#22076=VERTEX_POINT('',#72933);
#22077=VERTEX_POINT('',#72937);
#22078=VERTEX_POINT('',#72941);
#22079=VERTEX_POINT('',#72945);
#22080=VERTEX_POINT('',#72949);
#22081=VERTEX_POINT('',#72953);
#22082=VERTEX_POINT('',#72957);
#22083=VERTEX_POINT('',#72961);
#22084=VERTEX_POINT('',#72965);
#22085=VERTEX_POINT('',#72969);
#22086=VERTEX_POINT('',#72973);
#22087=VERTEX_POINT('',#72979);
#22088=VERTEX_POINT('',#72985);
#22089=VERTEX_POINT('',#72991);
#22090=VERTEX_POINT('',#72997);
#22091=VERTEX_POINT('',#73003);
#22092=VERTEX_POINT('',#73009);
#22093=VERTEX_POINT('',#73015);
#22094=VERTEX_POINT('',#73021);
#22095=VERTEX_POINT('',#73027);
#22096=VERTEX_POINT('',#73033);
#22097=VERTEX_POINT('',#73039);
#22098=VERTEX_POINT('',#73045);
#22099=VERTEX_POINT('',#73051);
#22100=VERTEX_POINT('',#73057);
#22101=VERTEX_POINT('',#73063);
#22102=VERTEX_POINT('',#73069);
#22103=VERTEX_POINT('',#73075);
#22104=VERTEX_POINT('',#73077);
#22105=VERTEX_POINT('',#73085);
#22106=VERTEX_POINT('',#73091);
#22107=VERTEX_POINT('',#73097);
#22108=VERTEX_POINT('',#73103);
#22109=VERTEX_POINT('',#73109);
#22110=VERTEX_POINT('',#73115);
#22111=VERTEX_POINT('',#73121);
#22112=VERTEX_POINT('',#73127);
#22113=VERTEX_POINT('',#73133);
#22114=VERTEX_POINT('',#73139);
#22115=VERTEX_POINT('',#73145);
#22116=VERTEX_POINT('',#73151);
#22117=VERTEX_POINT('',#73157);
#22118=VERTEX_POINT('',#73163);
#22119=VERTEX_POINT('',#73169);
#22120=VERTEX_POINT('',#73175);
#22121=VERTEX_POINT('',#73181);
#22122=VERTEX_POINT('',#73187);
#22123=VERTEX_POINT('',#73193);
#22124=VERTEX_POINT('',#73197);
#22125=VERTEX_POINT('',#73201);
#22126=VERTEX_POINT('',#73205);
#22127=VERTEX_POINT('',#73209);
#22128=VERTEX_POINT('',#73213);
#22129=VERTEX_POINT('',#73217);
#22130=VERTEX_POINT('',#73221);
#22131=VERTEX_POINT('',#73225);
#22132=VERTEX_POINT('',#73229);
#22133=VERTEX_POINT('',#73233);
#22134=VERTEX_POINT('',#73237);
#22135=VERTEX_POINT('',#73241);
#22136=VERTEX_POINT('',#73245);
#22137=VERTEX_POINT('',#73251);
#22138=VERTEX_POINT('',#73255);
#22139=VERTEX_POINT('',#73259);
#22140=VERTEX_POINT('',#73263);
#22141=VERTEX_POINT('',#73267);
#22142=VERTEX_POINT('',#73271);
#22143=VERTEX_POINT('',#73275);
#22144=VERTEX_POINT('',#73279);
#22145=VERTEX_POINT('',#73283);
#22146=VERTEX_POINT('',#73287);
#22147=VERTEX_POINT('',#73291);
#22148=VERTEX_POINT('',#73295);
#22149=VERTEX_POINT('',#73305);
#22150=VERTEX_POINT('',#73307);
#22151=VERTEX_POINT('',#73381);
#22152=VERTEX_POINT('',#73455);
#22153=VERTEX_POINT('',#73457);
#22154=VERTEX_POINT('',#73459);
#22155=VERTEX_POINT('',#73461);
#22156=VERTEX_POINT('',#73463);
#22157=VERTEX_POINT('',#73465);
#22158=VERTEX_POINT('',#73467);
#22159=VERTEX_POINT('',#73469);
#22160=VERTEX_POINT('',#73471);
#22161=VERTEX_POINT('',#73473);
#22162=VERTEX_POINT('',#73475);
#22163=VERTEX_POINT('',#73477);
#22164=VERTEX_POINT('',#73479);
#22165=VERTEX_POINT('',#73481);
#22166=VERTEX_POINT('',#73515);
#22167=VERTEX_POINT('',#73519);
#22168=VERTEX_POINT('',#73523);
#22169=VERTEX_POINT('',#73527);
#22170=VERTEX_POINT('',#73531);
#22171=VERTEX_POINT('',#73535);
#22172=VERTEX_POINT('',#73539);
#22173=VERTEX_POINT('',#73543);
#22174=VERTEX_POINT('',#73547);
#22175=VERTEX_POINT('',#73551);
#22176=VERTEX_POINT('',#73555);
#22177=VERTEX_POINT('',#73559);
#22178=VERTEX_POINT('',#73566);
#22179=VERTEX_POINT('',#73568);
#22180=VERTEX_POINT('',#73570);
#22181=VERTEX_POINT('',#73572);
#22182=VERTEX_POINT('',#73574);
#22183=VERTEX_POINT('',#73576);
#22184=VERTEX_POINT('',#73578);
#22185=VERTEX_POINT('',#73580);
#22186=VERTEX_POINT('',#73582);
#22187=VERTEX_POINT('',#73584);
#22188=VERTEX_POINT('',#73586);
#22189=VERTEX_POINT('',#73588);
#22190=VERTEX_POINT('',#73590);
#22191=VERTEX_POINT('',#73592);
#22192=VERTEX_POINT('',#73626);
#22193=VERTEX_POINT('',#73630);
#22194=VERTEX_POINT('',#73634);
#22195=VERTEX_POINT('',#73638);
#22196=VERTEX_POINT('',#73642);
#22197=VERTEX_POINT('',#73646);
#22198=VERTEX_POINT('',#73650);
#22199=VERTEX_POINT('',#73654);
#22200=VERTEX_POINT('',#73658);
#22201=VERTEX_POINT('',#73662);
#22202=VERTEX_POINT('',#73666);
#22203=VERTEX_POINT('',#73670);
#22204=VERTEX_POINT('',#73677);
#22205=VERTEX_POINT('',#73679);
#22206=VERTEX_POINT('',#73681);
#22207=VERTEX_POINT('',#73683);
#22208=VERTEX_POINT('',#73685);
#22209=VERTEX_POINT('',#73687);
#22210=VERTEX_POINT('',#73689);
#22211=VERTEX_POINT('',#73691);
#22212=VERTEX_POINT('',#73693);
#22213=VERTEX_POINT('',#73695);
#22214=VERTEX_POINT('',#73697);
#22215=VERTEX_POINT('',#73699);
#22216=VERTEX_POINT('',#73701);
#22217=VERTEX_POINT('',#73703);
#22218=VERTEX_POINT('',#73737);
#22219=VERTEX_POINT('',#73741);
#22220=VERTEX_POINT('',#73745);
#22221=VERTEX_POINT('',#73749);
#22222=VERTEX_POINT('',#73753);
#22223=VERTEX_POINT('',#73757);
#22224=VERTEX_POINT('',#73761);
#22225=VERTEX_POINT('',#73765);
#22226=VERTEX_POINT('',#73769);
#22227=VERTEX_POINT('',#73773);
#22228=VERTEX_POINT('',#73777);
#22229=VERTEX_POINT('',#73781);
#22230=VERTEX_POINT('',#73788);
#22231=VERTEX_POINT('',#73790);
#22232=VERTEX_POINT('',#73792);
#22233=VERTEX_POINT('',#73794);
#22234=VERTEX_POINT('',#73796);
#22235=VERTEX_POINT('',#73798);
#22236=VERTEX_POINT('',#73800);
#22237=VERTEX_POINT('',#73802);
#22238=VERTEX_POINT('',#73804);
#22239=VERTEX_POINT('',#73806);
#22240=VERTEX_POINT('',#73808);
#22241=VERTEX_POINT('',#73810);
#22242=VERTEX_POINT('',#73812);
#22243=VERTEX_POINT('',#73814);
#22244=VERTEX_POINT('',#73848);
#22245=VERTEX_POINT('',#73852);
#22246=VERTEX_POINT('',#73856);
#22247=VERTEX_POINT('',#73860);
#22248=VERTEX_POINT('',#73864);
#22249=VERTEX_POINT('',#73868);
#22250=VERTEX_POINT('',#73872);
#22251=VERTEX_POINT('',#73876);
#22252=VERTEX_POINT('',#73880);
#22253=VERTEX_POINT('',#73884);
#22254=VERTEX_POINT('',#73888);
#22255=VERTEX_POINT('',#73892);
#22256=VERTEX_POINT('',#73899);
#22257=VERTEX_POINT('',#73901);
#22258=VERTEX_POINT('',#73903);
#22259=VERTEX_POINT('',#73905);
#22260=VERTEX_POINT('',#73907);
#22261=VERTEX_POINT('',#73909);
#22262=VERTEX_POINT('',#73911);
#22263=VERTEX_POINT('',#73913);
#22264=VERTEX_POINT('',#73915);
#22265=VERTEX_POINT('',#73917);
#22266=VERTEX_POINT('',#73919);
#22267=VERTEX_POINT('',#73921);
#22268=VERTEX_POINT('',#73923);
#22269=VERTEX_POINT('',#73925);
#22270=VERTEX_POINT('',#73959);
#22271=VERTEX_POINT('',#73963);
#22272=VERTEX_POINT('',#73967);
#22273=VERTEX_POINT('',#73971);
#22274=VERTEX_POINT('',#73975);
#22275=VERTEX_POINT('',#73979);
#22276=VERTEX_POINT('',#73983);
#22277=VERTEX_POINT('',#73987);
#22278=VERTEX_POINT('',#73991);
#22279=VERTEX_POINT('',#73995);
#22280=VERTEX_POINT('',#73999);
#22281=VERTEX_POINT('',#74003);
#22282=VERTEX_POINT('',#74010);
#22283=VERTEX_POINT('',#74012);
#22284=VERTEX_POINT('',#74014);
#22285=VERTEX_POINT('',#74016);
#22286=VERTEX_POINT('',#74018);
#22287=VERTEX_POINT('',#74020);
#22288=VERTEX_POINT('',#74022);
#22289=VERTEX_POINT('',#74024);
#22290=VERTEX_POINT('',#74026);
#22291=VERTEX_POINT('',#74028);
#22292=VERTEX_POINT('',#74030);
#22293=VERTEX_POINT('',#74032);
#22294=VERTEX_POINT('',#74034);
#22295=VERTEX_POINT('',#74036);
#22296=VERTEX_POINT('',#74070);
#22297=VERTEX_POINT('',#74074);
#22298=VERTEX_POINT('',#74078);
#22299=VERTEX_POINT('',#74082);
#22300=VERTEX_POINT('',#74086);
#22301=VERTEX_POINT('',#74090);
#22302=VERTEX_POINT('',#74094);
#22303=VERTEX_POINT('',#74098);
#22304=VERTEX_POINT('',#74102);
#22305=VERTEX_POINT('',#74106);
#22306=VERTEX_POINT('',#74110);
#22307=VERTEX_POINT('',#74114);
#22308=VERTEX_POINT('',#74121);
#22309=VERTEX_POINT('',#74123);
#22310=VERTEX_POINT('',#74125);
#22311=VERTEX_POINT('',#74127);
#22312=VERTEX_POINT('',#74129);
#22313=VERTEX_POINT('',#74131);
#22314=VERTEX_POINT('',#74133);
#22315=VERTEX_POINT('',#74135);
#22316=VERTEX_POINT('',#74137);
#22317=VERTEX_POINT('',#74139);
#22318=VERTEX_POINT('',#74141);
#22319=VERTEX_POINT('',#74143);
#22320=VERTEX_POINT('',#74145);
#22321=VERTEX_POINT('',#74147);
#22322=VERTEX_POINT('',#74181);
#22323=VERTEX_POINT('',#74185);
#22324=VERTEX_POINT('',#74189);
#22325=VERTEX_POINT('',#74193);
#22326=VERTEX_POINT('',#74197);
#22327=VERTEX_POINT('',#74201);
#22328=VERTEX_POINT('',#74205);
#22329=VERTEX_POINT('',#74209);
#22330=VERTEX_POINT('',#74213);
#22331=VERTEX_POINT('',#74217);
#22332=VERTEX_POINT('',#74221);
#22333=VERTEX_POINT('',#74225);
#22334=VERTEX_POINT('',#74232);
#22335=VERTEX_POINT('',#74234);
#22336=VERTEX_POINT('',#74236);
#22337=VERTEX_POINT('',#74238);
#22338=VERTEX_POINT('',#74240);
#22339=VERTEX_POINT('',#74242);
#22340=VERTEX_POINT('',#74244);
#22341=VERTEX_POINT('',#74246);
#22342=VERTEX_POINT('',#74248);
#22343=VERTEX_POINT('',#74250);
#22344=VERTEX_POINT('',#74252);
#22345=VERTEX_POINT('',#74254);
#22346=VERTEX_POINT('',#74256);
#22347=VERTEX_POINT('',#74258);
#22348=VERTEX_POINT('',#74292);
#22349=VERTEX_POINT('',#74296);
#22350=VERTEX_POINT('',#74300);
#22351=VERTEX_POINT('',#74304);
#22352=VERTEX_POINT('',#74308);
#22353=VERTEX_POINT('',#74312);
#22354=VERTEX_POINT('',#74316);
#22355=VERTEX_POINT('',#74320);
#22356=VERTEX_POINT('',#74324);
#22357=VERTEX_POINT('',#74328);
#22358=VERTEX_POINT('',#74332);
#22359=VERTEX_POINT('',#74336);
#22360=VERTEX_POINT('',#74343);
#22361=VERTEX_POINT('',#74345);
#22362=VERTEX_POINT('',#74347);
#22363=VERTEX_POINT('',#74349);
#22364=VERTEX_POINT('',#74351);
#22365=VERTEX_POINT('',#74353);
#22366=VERTEX_POINT('',#74355);
#22367=VERTEX_POINT('',#74357);
#22368=VERTEX_POINT('',#74359);
#22369=VERTEX_POINT('',#74361);
#22370=VERTEX_POINT('',#74363);
#22371=VERTEX_POINT('',#74365);
#22372=VERTEX_POINT('',#74367);
#22373=VERTEX_POINT('',#74369);
#22374=VERTEX_POINT('',#74403);
#22375=VERTEX_POINT('',#74407);
#22376=VERTEX_POINT('',#74411);
#22377=VERTEX_POINT('',#74415);
#22378=VERTEX_POINT('',#74419);
#22379=VERTEX_POINT('',#74423);
#22380=VERTEX_POINT('',#74427);
#22381=VERTEX_POINT('',#74431);
#22382=VERTEX_POINT('',#74435);
#22383=VERTEX_POINT('',#74439);
#22384=VERTEX_POINT('',#74443);
#22385=VERTEX_POINT('',#74447);
#22386=VERTEX_POINT('',#74454);
#22387=VERTEX_POINT('',#74456);
#22388=VERTEX_POINT('',#74458);
#22389=VERTEX_POINT('',#74460);
#22390=VERTEX_POINT('',#74462);
#22391=VERTEX_POINT('',#74464);
#22392=VERTEX_POINT('',#74466);
#22393=VERTEX_POINT('',#74468);
#22394=VERTEX_POINT('',#74470);
#22395=VERTEX_POINT('',#74472);
#22396=VERTEX_POINT('',#74474);
#22397=VERTEX_POINT('',#74476);
#22398=VERTEX_POINT('',#74478);
#22399=VERTEX_POINT('',#74480);
#22400=VERTEX_POINT('',#74514);
#22401=VERTEX_POINT('',#74518);
#22402=VERTEX_POINT('',#74522);
#22403=VERTEX_POINT('',#74526);
#22404=VERTEX_POINT('',#74530);
#22405=VERTEX_POINT('',#74534);
#22406=VERTEX_POINT('',#74538);
#22407=VERTEX_POINT('',#74542);
#22408=VERTEX_POINT('',#74546);
#22409=VERTEX_POINT('',#74550);
#22410=VERTEX_POINT('',#74554);
#22411=VERTEX_POINT('',#74558);
#22412=VERTEX_POINT('',#74565);
#22413=VERTEX_POINT('',#74567);
#22414=VERTEX_POINT('',#74569);
#22415=VERTEX_POINT('',#74571);
#22416=VERTEX_POINT('',#74573);
#22417=VERTEX_POINT('',#74575);
#22418=VERTEX_POINT('',#74577);
#22419=VERTEX_POINT('',#74579);
#22420=VERTEX_POINT('',#74581);
#22421=VERTEX_POINT('',#74583);
#22422=VERTEX_POINT('',#74585);
#22423=VERTEX_POINT('',#74587);
#22424=VERTEX_POINT('',#74589);
#22425=VERTEX_POINT('',#74591);
#22426=VERTEX_POINT('',#74625);
#22427=VERTEX_POINT('',#74629);
#22428=VERTEX_POINT('',#74633);
#22429=VERTEX_POINT('',#74637);
#22430=VERTEX_POINT('',#74641);
#22431=VERTEX_POINT('',#74645);
#22432=VERTEX_POINT('',#74649);
#22433=VERTEX_POINT('',#74653);
#22434=VERTEX_POINT('',#74657);
#22435=VERTEX_POINT('',#74661);
#22436=VERTEX_POINT('',#74665);
#22437=VERTEX_POINT('',#74669);
#22438=VERTEX_POINT('',#74676);
#22439=VERTEX_POINT('',#74678);
#22440=VERTEX_POINT('',#74680);
#22441=VERTEX_POINT('',#74682);
#22442=VERTEX_POINT('',#74684);
#22443=VERTEX_POINT('',#74686);
#22444=VERTEX_POINT('',#74688);
#22445=VERTEX_POINT('',#74690);
#22446=VERTEX_POINT('',#74692);
#22447=VERTEX_POINT('',#74694);
#22448=VERTEX_POINT('',#74696);
#22449=VERTEX_POINT('',#74698);
#22450=VERTEX_POINT('',#74700);
#22451=VERTEX_POINT('',#74702);
#22452=VERTEX_POINT('',#74736);
#22453=VERTEX_POINT('',#74740);
#22454=VERTEX_POINT('',#74744);
#22455=VERTEX_POINT('',#74748);
#22456=VERTEX_POINT('',#74752);
#22457=VERTEX_POINT('',#74756);
#22458=VERTEX_POINT('',#74760);
#22459=VERTEX_POINT('',#74764);
#22460=VERTEX_POINT('',#74768);
#22461=VERTEX_POINT('',#74772);
#22462=VERTEX_POINT('',#74776);
#22463=VERTEX_POINT('',#74780);
#22464=VERTEX_POINT('',#74787);
#22465=VERTEX_POINT('',#74789);
#22466=VERTEX_POINT('',#74791);
#22467=VERTEX_POINT('',#74793);
#22468=VERTEX_POINT('',#74795);
#22469=VERTEX_POINT('',#74797);
#22470=VERTEX_POINT('',#74799);
#22471=VERTEX_POINT('',#74801);
#22472=VERTEX_POINT('',#74803);
#22473=VERTEX_POINT('',#74805);
#22474=VERTEX_POINT('',#74807);
#22475=VERTEX_POINT('',#74809);
#22476=VERTEX_POINT('',#74811);
#22477=VERTEX_POINT('',#74813);
#22478=VERTEX_POINT('',#74847);
#22479=VERTEX_POINT('',#74851);
#22480=VERTEX_POINT('',#74855);
#22481=VERTEX_POINT('',#74859);
#22482=VERTEX_POINT('',#74863);
#22483=VERTEX_POINT('',#74867);
#22484=VERTEX_POINT('',#74871);
#22485=VERTEX_POINT('',#74875);
#22486=VERTEX_POINT('',#74879);
#22487=VERTEX_POINT('',#74883);
#22488=VERTEX_POINT('',#74887);
#22489=VERTEX_POINT('',#74891);
#22490=VERTEX_POINT('',#74898);
#22491=VERTEX_POINT('',#74900);
#22492=VERTEX_POINT('',#74902);
#22493=VERTEX_POINT('',#74904);
#22494=VERTEX_POINT('',#74906);
#22495=VERTEX_POINT('',#74908);
#22496=VERTEX_POINT('',#74910);
#22497=VERTEX_POINT('',#74912);
#22498=VERTEX_POINT('',#74914);
#22499=VERTEX_POINT('',#74916);
#22500=VERTEX_POINT('',#74918);
#22501=VERTEX_POINT('',#74920);
#22502=VERTEX_POINT('',#74922);
#22503=VERTEX_POINT('',#74924);
#22504=VERTEX_POINT('',#74958);
#22505=VERTEX_POINT('',#74962);
#22506=VERTEX_POINT('',#74966);
#22507=VERTEX_POINT('',#74970);
#22508=VERTEX_POINT('',#74974);
#22509=VERTEX_POINT('',#74978);
#22510=VERTEX_POINT('',#74982);
#22511=VERTEX_POINT('',#74986);
#22512=VERTEX_POINT('',#74990);
#22513=VERTEX_POINT('',#74994);
#22514=VERTEX_POINT('',#74998);
#22515=VERTEX_POINT('',#75002);
#22516=VERTEX_POINT('',#75009);
#22517=VERTEX_POINT('',#75011);
#22518=VERTEX_POINT('',#75013);
#22519=VERTEX_POINT('',#75015);
#22520=VERTEX_POINT('',#75017);
#22521=VERTEX_POINT('',#75019);
#22522=VERTEX_POINT('',#75021);
#22523=VERTEX_POINT('',#75023);
#22524=VERTEX_POINT('',#75025);
#22525=VERTEX_POINT('',#75027);
#22526=VERTEX_POINT('',#75029);
#22527=VERTEX_POINT('',#75031);
#22528=VERTEX_POINT('',#75033);
#22529=VERTEX_POINT('',#75035);
#22530=VERTEX_POINT('',#75069);
#22531=VERTEX_POINT('',#75073);
#22532=VERTEX_POINT('',#75077);
#22533=VERTEX_POINT('',#75081);
#22534=VERTEX_POINT('',#75085);
#22535=VERTEX_POINT('',#75089);
#22536=VERTEX_POINT('',#75093);
#22537=VERTEX_POINT('',#75097);
#22538=VERTEX_POINT('',#75101);
#22539=VERTEX_POINT('',#75105);
#22540=VERTEX_POINT('',#75109);
#22541=VERTEX_POINT('',#75113);
#22542=VERTEX_POINT('',#75120);
#22543=VERTEX_POINT('',#75122);
#22544=VERTEX_POINT('',#75124);
#22545=VERTEX_POINT('',#75126);
#22546=VERTEX_POINT('',#75128);
#22547=VERTEX_POINT('',#75130);
#22548=VERTEX_POINT('',#75132);
#22549=VERTEX_POINT('',#75134);
#22550=VERTEX_POINT('',#75136);
#22551=VERTEX_POINT('',#75138);
#22552=VERTEX_POINT('',#75140);
#22553=VERTEX_POINT('',#75142);
#22554=VERTEX_POINT('',#75144);
#22555=VERTEX_POINT('',#75146);
#22556=VERTEX_POINT('',#75180);
#22557=VERTEX_POINT('',#75184);
#22558=VERTEX_POINT('',#75188);
#22559=VERTEX_POINT('',#75192);
#22560=VERTEX_POINT('',#75196);
#22561=VERTEX_POINT('',#75200);
#22562=VERTEX_POINT('',#75204);
#22563=VERTEX_POINT('',#75208);
#22564=VERTEX_POINT('',#75212);
#22565=VERTEX_POINT('',#75216);
#22566=VERTEX_POINT('',#75220);
#22567=VERTEX_POINT('',#75224);
#22568=VERTEX_POINT('',#75231);
#22569=VERTEX_POINT('',#75233);
#22570=VERTEX_POINT('',#75235);
#22571=VERTEX_POINT('',#75237);
#22572=VERTEX_POINT('',#75239);
#22573=VERTEX_POINT('',#75241);
#22574=VERTEX_POINT('',#75243);
#22575=VERTEX_POINT('',#75245);
#22576=VERTEX_POINT('',#75247);
#22577=VERTEX_POINT('',#75249);
#22578=VERTEX_POINT('',#75251);
#22579=VERTEX_POINT('',#75253);
#22580=VERTEX_POINT('',#75255);
#22581=VERTEX_POINT('',#75257);
#22582=VERTEX_POINT('',#75291);
#22583=VERTEX_POINT('',#75295);
#22584=VERTEX_POINT('',#75299);
#22585=VERTEX_POINT('',#75303);
#22586=VERTEX_POINT('',#75307);
#22587=VERTEX_POINT('',#75311);
#22588=VERTEX_POINT('',#75315);
#22589=VERTEX_POINT('',#75319);
#22590=VERTEX_POINT('',#75323);
#22591=VERTEX_POINT('',#75327);
#22592=VERTEX_POINT('',#75331);
#22593=VERTEX_POINT('',#75335);
#22594=VERTEX_POINT('',#75342);
#22595=VERTEX_POINT('',#75344);
#22596=VERTEX_POINT('',#75346);
#22597=VERTEX_POINT('',#75348);
#22598=VERTEX_POINT('',#75350);
#22599=VERTEX_POINT('',#75352);
#22600=VERTEX_POINT('',#75354);
#22601=VERTEX_POINT('',#75356);
#22602=VERTEX_POINT('',#75358);
#22603=VERTEX_POINT('',#75360);
#22604=VERTEX_POINT('',#75362);
#22605=VERTEX_POINT('',#75364);
#22606=VERTEX_POINT('',#75366);
#22607=VERTEX_POINT('',#75368);
#22608=VERTEX_POINT('',#75402);
#22609=VERTEX_POINT('',#75406);
#22610=VERTEX_POINT('',#75410);
#22611=VERTEX_POINT('',#75414);
#22612=VERTEX_POINT('',#75418);
#22613=VERTEX_POINT('',#75422);
#22614=VERTEX_POINT('',#75426);
#22615=VERTEX_POINT('',#75430);
#22616=VERTEX_POINT('',#75434);
#22617=VERTEX_POINT('',#75438);
#22618=VERTEX_POINT('',#75442);
#22619=VERTEX_POINT('',#75446);
#22620=VERTEX_POINT('',#75453);
#22621=VERTEX_POINT('',#75455);
#22622=VERTEX_POINT('',#75457);
#22623=VERTEX_POINT('',#75459);
#22624=VERTEX_POINT('',#75461);
#22625=VERTEX_POINT('',#75463);
#22626=VERTEX_POINT('',#75465);
#22627=VERTEX_POINT('',#75467);
#22628=VERTEX_POINT('',#75469);
#22629=VERTEX_POINT('',#75471);
#22630=VERTEX_POINT('',#75473);
#22631=VERTEX_POINT('',#75475);
#22632=VERTEX_POINT('',#75477);
#22633=VERTEX_POINT('',#75479);
#22634=VERTEX_POINT('',#75513);
#22635=VERTEX_POINT('',#75517);
#22636=VERTEX_POINT('',#75521);
#22637=VERTEX_POINT('',#75525);
#22638=VERTEX_POINT('',#75529);
#22639=VERTEX_POINT('',#75533);
#22640=VERTEX_POINT('',#75537);
#22641=VERTEX_POINT('',#75541);
#22642=VERTEX_POINT('',#75545);
#22643=VERTEX_POINT('',#75549);
#22644=VERTEX_POINT('',#75553);
#22645=VERTEX_POINT('',#75557);
#22646=VERTEX_POINT('',#75564);
#22647=VERTEX_POINT('',#75566);
#22648=VERTEX_POINT('',#75568);
#22649=VERTEX_POINT('',#75570);
#22650=VERTEX_POINT('',#75572);
#22651=VERTEX_POINT('',#75574);
#22652=VERTEX_POINT('',#75576);
#22653=VERTEX_POINT('',#75578);
#22654=VERTEX_POINT('',#75580);
#22655=VERTEX_POINT('',#75582);
#22656=VERTEX_POINT('',#75584);
#22657=VERTEX_POINT('',#75586);
#22658=VERTEX_POINT('',#75588);
#22659=VERTEX_POINT('',#75590);
#22660=VERTEX_POINT('',#75624);
#22661=VERTEX_POINT('',#75628);
#22662=VERTEX_POINT('',#75632);
#22663=VERTEX_POINT('',#75636);
#22664=VERTEX_POINT('',#75640);
#22665=VERTEX_POINT('',#75644);
#22666=VERTEX_POINT('',#75648);
#22667=VERTEX_POINT('',#75652);
#22668=VERTEX_POINT('',#75656);
#22669=VERTEX_POINT('',#75660);
#22670=VERTEX_POINT('',#75664);
#22671=VERTEX_POINT('',#75668);
#22672=VERTEX_POINT('',#75675);
#22673=VERTEX_POINT('',#75677);
#22674=VERTEX_POINT('',#75679);
#22675=VERTEX_POINT('',#75681);
#22676=VERTEX_POINT('',#75683);
#22677=VERTEX_POINT('',#75685);
#22678=VERTEX_POINT('',#75687);
#22679=VERTEX_POINT('',#75689);
#22680=VERTEX_POINT('',#75691);
#22681=VERTEX_POINT('',#75693);
#22682=VERTEX_POINT('',#75695);
#22683=VERTEX_POINT('',#75697);
#22684=VERTEX_POINT('',#75699);
#22685=VERTEX_POINT('',#75701);
#22686=VERTEX_POINT('',#75735);
#22687=VERTEX_POINT('',#75739);
#22688=VERTEX_POINT('',#75743);
#22689=VERTEX_POINT('',#75747);
#22690=VERTEX_POINT('',#75751);
#22691=VERTEX_POINT('',#75755);
#22692=VERTEX_POINT('',#75759);
#22693=VERTEX_POINT('',#75763);
#22694=VERTEX_POINT('',#75767);
#22695=VERTEX_POINT('',#75771);
#22696=VERTEX_POINT('',#75775);
#22697=VERTEX_POINT('',#75779);
#22698=VERTEX_POINT('',#75786);
#22699=VERTEX_POINT('',#75788);
#22700=VERTEX_POINT('',#75790);
#22701=VERTEX_POINT('',#75792);
#22702=VERTEX_POINT('',#75794);
#22703=VERTEX_POINT('',#75796);
#22704=VERTEX_POINT('',#75798);
#22705=VERTEX_POINT('',#75800);
#22706=VERTEX_POINT('',#75802);
#22707=VERTEX_POINT('',#75804);
#22708=VERTEX_POINT('',#75806);
#22709=VERTEX_POINT('',#75808);
#22710=VERTEX_POINT('',#75810);
#22711=VERTEX_POINT('',#75812);
#22712=VERTEX_POINT('',#75846);
#22713=VERTEX_POINT('',#75850);
#22714=VERTEX_POINT('',#75854);
#22715=VERTEX_POINT('',#75858);
#22716=VERTEX_POINT('',#75862);
#22717=VERTEX_POINT('',#75866);
#22718=VERTEX_POINT('',#75870);
#22719=VERTEX_POINT('',#75874);
#22720=VERTEX_POINT('',#75878);
#22721=VERTEX_POINT('',#75882);
#22722=VERTEX_POINT('',#75886);
#22723=VERTEX_POINT('',#75890);
#22724=VERTEX_POINT('',#75897);
#22725=VERTEX_POINT('',#75899);
#22726=VERTEX_POINT('',#75901);
#22727=VERTEX_POINT('',#75903);
#22728=VERTEX_POINT('',#75905);
#22729=VERTEX_POINT('',#75907);
#22730=VERTEX_POINT('',#75909);
#22731=VERTEX_POINT('',#75911);
#22732=VERTEX_POINT('',#75913);
#22733=VERTEX_POINT('',#75915);
#22734=VERTEX_POINT('',#75917);
#22735=VERTEX_POINT('',#75919);
#22736=VERTEX_POINT('',#75921);
#22737=VERTEX_POINT('',#75923);
#22738=VERTEX_POINT('',#75957);
#22739=VERTEX_POINT('',#75961);
#22740=VERTEX_POINT('',#75965);
#22741=VERTEX_POINT('',#75969);
#22742=VERTEX_POINT('',#75973);
#22743=VERTEX_POINT('',#75977);
#22744=VERTEX_POINT('',#75981);
#22745=VERTEX_POINT('',#75985);
#22746=VERTEX_POINT('',#75989);
#22747=VERTEX_POINT('',#75993);
#22748=VERTEX_POINT('',#75997);
#22749=VERTEX_POINT('',#76001);
#22750=VERTEX_POINT('',#76008);
#22751=VERTEX_POINT('',#76010);
#22752=VERTEX_POINT('',#76012);
#22753=VERTEX_POINT('',#76014);
#22754=VERTEX_POINT('',#76016);
#22755=VERTEX_POINT('',#76018);
#22756=VERTEX_POINT('',#76020);
#22757=VERTEX_POINT('',#76022);
#22758=VERTEX_POINT('',#76024);
#22759=VERTEX_POINT('',#76026);
#22760=VERTEX_POINT('',#76028);
#22761=VERTEX_POINT('',#76030);
#22762=VERTEX_POINT('',#76032);
#22763=VERTEX_POINT('',#76034);
#22764=VERTEX_POINT('',#76068);
#22765=VERTEX_POINT('',#76072);
#22766=VERTEX_POINT('',#76076);
#22767=VERTEX_POINT('',#76080);
#22768=VERTEX_POINT('',#76084);
#22769=VERTEX_POINT('',#76088);
#22770=VERTEX_POINT('',#76092);
#22771=VERTEX_POINT('',#76096);
#22772=VERTEX_POINT('',#76100);
#22773=VERTEX_POINT('',#76104);
#22774=VERTEX_POINT('',#76108);
#22775=VERTEX_POINT('',#76112);
#22776=VERTEX_POINT('',#76119);
#22777=VERTEX_POINT('',#76121);
#22778=VERTEX_POINT('',#76123);
#22779=VERTEX_POINT('',#76125);
#22780=VERTEX_POINT('',#76127);
#22781=VERTEX_POINT('',#76129);
#22782=VERTEX_POINT('',#76131);
#22783=VERTEX_POINT('',#76133);
#22784=VERTEX_POINT('',#76135);
#22785=VERTEX_POINT('',#76137);
#22786=VERTEX_POINT('',#76139);
#22787=VERTEX_POINT('',#76141);
#22788=VERTEX_POINT('',#76143);
#22789=VERTEX_POINT('',#76145);
#22790=VERTEX_POINT('',#76179);
#22791=VERTEX_POINT('',#76183);
#22792=VERTEX_POINT('',#76187);
#22793=VERTEX_POINT('',#76191);
#22794=VERTEX_POINT('',#76195);
#22795=VERTEX_POINT('',#76199);
#22796=VERTEX_POINT('',#76203);
#22797=VERTEX_POINT('',#76207);
#22798=VERTEX_POINT('',#76211);
#22799=VERTEX_POINT('',#76215);
#22800=VERTEX_POINT('',#76219);
#22801=VERTEX_POINT('',#76223);
#22802=VERTEX_POINT('',#76230);
#22803=VERTEX_POINT('',#76232);
#22804=VERTEX_POINT('',#76234);
#22805=VERTEX_POINT('',#76236);
#22806=VERTEX_POINT('',#76238);
#22807=VERTEX_POINT('',#76240);
#22808=VERTEX_POINT('',#76242);
#22809=VERTEX_POINT('',#76244);
#22810=VERTEX_POINT('',#76246);
#22811=VERTEX_POINT('',#76248);
#22812=VERTEX_POINT('',#76250);
#22813=VERTEX_POINT('',#76252);
#22814=VERTEX_POINT('',#76254);
#22815=VERTEX_POINT('',#76256);
#22816=VERTEX_POINT('',#76290);
#22817=VERTEX_POINT('',#76294);
#22818=VERTEX_POINT('',#76298);
#22819=VERTEX_POINT('',#76302);
#22820=VERTEX_POINT('',#76306);
#22821=VERTEX_POINT('',#76310);
#22822=VERTEX_POINT('',#76314);
#22823=VERTEX_POINT('',#76318);
#22824=VERTEX_POINT('',#76322);
#22825=VERTEX_POINT('',#76326);
#22826=VERTEX_POINT('',#76330);
#22827=VERTEX_POINT('',#76334);
#22828=VERTEX_POINT('',#76341);
#22829=VERTEX_POINT('',#76343);
#22830=VERTEX_POINT('',#76345);
#22831=VERTEX_POINT('',#76347);
#22832=VERTEX_POINT('',#76349);
#22833=VERTEX_POINT('',#76351);
#22834=VERTEX_POINT('',#76353);
#22835=VERTEX_POINT('',#76355);
#22836=VERTEX_POINT('',#76357);
#22837=VERTEX_POINT('',#76359);
#22838=VERTEX_POINT('',#76361);
#22839=VERTEX_POINT('',#76363);
#22840=VERTEX_POINT('',#76365);
#22841=VERTEX_POINT('',#76367);
#22842=VERTEX_POINT('',#76401);
#22843=VERTEX_POINT('',#76405);
#22844=VERTEX_POINT('',#76409);
#22845=VERTEX_POINT('',#76413);
#22846=VERTEX_POINT('',#76417);
#22847=VERTEX_POINT('',#76421);
#22848=VERTEX_POINT('',#76425);
#22849=VERTEX_POINT('',#76429);
#22850=VERTEX_POINT('',#76433);
#22851=VERTEX_POINT('',#76437);
#22852=VERTEX_POINT('',#76441);
#22853=VERTEX_POINT('',#76445);
#22854=VERTEX_POINT('',#76452);
#22855=VERTEX_POINT('',#76454);
#22856=VERTEX_POINT('',#76456);
#22857=VERTEX_POINT('',#76458);
#22858=VERTEX_POINT('',#76460);
#22859=VERTEX_POINT('',#76462);
#22860=VERTEX_POINT('',#76464);
#22861=VERTEX_POINT('',#76466);
#22862=VERTEX_POINT('',#76468);
#22863=VERTEX_POINT('',#76470);
#22864=VERTEX_POINT('',#76472);
#22865=VERTEX_POINT('',#76474);
#22866=VERTEX_POINT('',#76476);
#22867=VERTEX_POINT('',#76478);
#22868=VERTEX_POINT('',#76512);
#22869=VERTEX_POINT('',#76516);
#22870=VERTEX_POINT('',#76520);
#22871=VERTEX_POINT('',#76524);
#22872=VERTEX_POINT('',#76528);
#22873=VERTEX_POINT('',#76532);
#22874=VERTEX_POINT('',#76536);
#22875=VERTEX_POINT('',#76540);
#22876=VERTEX_POINT('',#76544);
#22877=VERTEX_POINT('',#76548);
#22878=VERTEX_POINT('',#76552);
#22879=VERTEX_POINT('',#76556);
#22880=VERTEX_POINT('',#76563);
#22881=VERTEX_POINT('',#76565);
#22882=VERTEX_POINT('',#76567);
#22883=VERTEX_POINT('',#76569);
#22884=VERTEX_POINT('',#76571);
#22885=VERTEX_POINT('',#76573);
#22886=VERTEX_POINT('',#76575);
#22887=VERTEX_POINT('',#76577);
#22888=VERTEX_POINT('',#76579);
#22889=VERTEX_POINT('',#76581);
#22890=VERTEX_POINT('',#76583);
#22891=VERTEX_POINT('',#76585);
#22892=VERTEX_POINT('',#76587);
#22893=VERTEX_POINT('',#76589);
#22894=VERTEX_POINT('',#76623);
#22895=VERTEX_POINT('',#76627);
#22896=VERTEX_POINT('',#76631);
#22897=VERTEX_POINT('',#76635);
#22898=VERTEX_POINT('',#76639);
#22899=VERTEX_POINT('',#76643);
#22900=VERTEX_POINT('',#76647);
#22901=VERTEX_POINT('',#76651);
#22902=VERTEX_POINT('',#76655);
#22903=VERTEX_POINT('',#76659);
#22904=VERTEX_POINT('',#76663);
#22905=VERTEX_POINT('',#76667);
#22906=VERTEX_POINT('',#76674);
#22907=VERTEX_POINT('',#76676);
#22908=VERTEX_POINT('',#76678);
#22909=VERTEX_POINT('',#76680);
#22910=VERTEX_POINT('',#76682);
#22911=VERTEX_POINT('',#76684);
#22912=VERTEX_POINT('',#76686);
#22913=VERTEX_POINT('',#76688);
#22914=VERTEX_POINT('',#76690);
#22915=VERTEX_POINT('',#76692);
#22916=VERTEX_POINT('',#76694);
#22917=VERTEX_POINT('',#76696);
#22918=VERTEX_POINT('',#76698);
#22919=VERTEX_POINT('',#76700);
#22920=VERTEX_POINT('',#76734);
#22921=VERTEX_POINT('',#76738);
#22922=VERTEX_POINT('',#76742);
#22923=VERTEX_POINT('',#76746);
#22924=VERTEX_POINT('',#76750);
#22925=VERTEX_POINT('',#76754);
#22926=VERTEX_POINT('',#76758);
#22927=VERTEX_POINT('',#76762);
#22928=VERTEX_POINT('',#76766);
#22929=VERTEX_POINT('',#76770);
#22930=VERTEX_POINT('',#76774);
#22931=VERTEX_POINT('',#76778);
#22932=VERTEX_POINT('',#76785);
#22933=VERTEX_POINT('',#76787);
#22934=VERTEX_POINT('',#76789);
#22935=VERTEX_POINT('',#76791);
#22936=VERTEX_POINT('',#76793);
#22937=VERTEX_POINT('',#76795);
#22938=VERTEX_POINT('',#76797);
#22939=VERTEX_POINT('',#76799);
#22940=VERTEX_POINT('',#76801);
#22941=VERTEX_POINT('',#76803);
#22942=VERTEX_POINT('',#76805);
#22943=VERTEX_POINT('',#76807);
#22944=VERTEX_POINT('',#76809);
#22945=VERTEX_POINT('',#76811);
#22946=VERTEX_POINT('',#76845);
#22947=VERTEX_POINT('',#76849);
#22948=VERTEX_POINT('',#76853);
#22949=VERTEX_POINT('',#76857);
#22950=VERTEX_POINT('',#76861);
#22951=VERTEX_POINT('',#76865);
#22952=VERTEX_POINT('',#76869);
#22953=VERTEX_POINT('',#76873);
#22954=VERTEX_POINT('',#76877);
#22955=VERTEX_POINT('',#76881);
#22956=VERTEX_POINT('',#76885);
#22957=VERTEX_POINT('',#76889);
#22958=VERTEX_POINT('',#76896);
#22959=VERTEX_POINT('',#76898);
#22960=VERTEX_POINT('',#76900);
#22961=VERTEX_POINT('',#76902);
#22962=VERTEX_POINT('',#76904);
#22963=VERTEX_POINT('',#76906);
#22964=VERTEX_POINT('',#76908);
#22965=VERTEX_POINT('',#76910);
#22966=VERTEX_POINT('',#76912);
#22967=VERTEX_POINT('',#76914);
#22968=VERTEX_POINT('',#76916);
#22969=VERTEX_POINT('',#76918);
#22970=VERTEX_POINT('',#76920);
#22971=VERTEX_POINT('',#76922);
#22972=VERTEX_POINT('',#76956);
#22973=VERTEX_POINT('',#76960);
#22974=VERTEX_POINT('',#76964);
#22975=VERTEX_POINT('',#76968);
#22976=VERTEX_POINT('',#76972);
#22977=VERTEX_POINT('',#76976);
#22978=VERTEX_POINT('',#76980);
#22979=VERTEX_POINT('',#76984);
#22980=VERTEX_POINT('',#76988);
#22981=VERTEX_POINT('',#76992);
#22982=VERTEX_POINT('',#76996);
#22983=VERTEX_POINT('',#77000);
#22984=VERTEX_POINT('',#77007);
#22985=VERTEX_POINT('',#77009);
#22986=VERTEX_POINT('',#77011);
#22987=VERTEX_POINT('',#77013);
#22988=VERTEX_POINT('',#77015);
#22989=VERTEX_POINT('',#77017);
#22990=VERTEX_POINT('',#77019);
#22991=VERTEX_POINT('',#77021);
#22992=VERTEX_POINT('',#77023);
#22993=VERTEX_POINT('',#77025);
#22994=VERTEX_POINT('',#77027);
#22995=VERTEX_POINT('',#77029);
#22996=VERTEX_POINT('',#77031);
#22997=VERTEX_POINT('',#77033);
#22998=VERTEX_POINT('',#77067);
#22999=VERTEX_POINT('',#77071);
#23000=VERTEX_POINT('',#77075);
#23001=VERTEX_POINT('',#77079);
#23002=VERTEX_POINT('',#77083);
#23003=VERTEX_POINT('',#77087);
#23004=VERTEX_POINT('',#77091);
#23005=VERTEX_POINT('',#77095);
#23006=VERTEX_POINT('',#77099);
#23007=VERTEX_POINT('',#77103);
#23008=VERTEX_POINT('',#77107);
#23009=VERTEX_POINT('',#77111);
#23010=VERTEX_POINT('',#77118);
#23011=VERTEX_POINT('',#77120);
#23012=VERTEX_POINT('',#77122);
#23013=VERTEX_POINT('',#77124);
#23014=VERTEX_POINT('',#77126);
#23015=VERTEX_POINT('',#77128);
#23016=VERTEX_POINT('',#77130);
#23017=VERTEX_POINT('',#77132);
#23018=VERTEX_POINT('',#77134);
#23019=VERTEX_POINT('',#77136);
#23020=VERTEX_POINT('',#77138);
#23021=VERTEX_POINT('',#77140);
#23022=VERTEX_POINT('',#77142);
#23023=VERTEX_POINT('',#77144);
#23024=VERTEX_POINT('',#77178);
#23025=VERTEX_POINT('',#77182);
#23026=VERTEX_POINT('',#77186);
#23027=VERTEX_POINT('',#77190);
#23028=VERTEX_POINT('',#77194);
#23029=VERTEX_POINT('',#77198);
#23030=VERTEX_POINT('',#77202);
#23031=VERTEX_POINT('',#77206);
#23032=VERTEX_POINT('',#77210);
#23033=VERTEX_POINT('',#77214);
#23034=VERTEX_POINT('',#77218);
#23035=VERTEX_POINT('',#77222);
#23036=VERTEX_POINT('',#77229);
#23037=VERTEX_POINT('',#77231);
#23038=VERTEX_POINT('',#77233);
#23039=VERTEX_POINT('',#77235);
#23040=VERTEX_POINT('',#77237);
#23041=VERTEX_POINT('',#77239);
#23042=VERTEX_POINT('',#77241);
#23043=VERTEX_POINT('',#77243);
#23044=VERTEX_POINT('',#77245);
#23045=VERTEX_POINT('',#77247);
#23046=VERTEX_POINT('',#77249);
#23047=VERTEX_POINT('',#77251);
#23048=VERTEX_POINT('',#77253);
#23049=VERTEX_POINT('',#77255);
#23050=VERTEX_POINT('',#77259);
#23051=VERTEX_POINT('',#77263);
#23052=VERTEX_POINT('',#77267);
#23053=VERTEX_POINT('',#77271);
#23054=VERTEX_POINT('',#77275);
#23055=VERTEX_POINT('',#77279);
#23056=VERTEX_POINT('',#77283);
#23057=VERTEX_POINT('',#77287);
#23058=VERTEX_POINT('',#77291);
#23059=VERTEX_POINT('',#77295);
#23060=VERTEX_POINT('',#77299);
#23061=VERTEX_POINT('',#77303);
#23062=VERTEX_POINT('',#77307);
#23063=VERTEX_POINT('',#77344);
#23064=VERTEX_POINT('',#77348);
#23065=VERTEX_POINT('',#77350);
#23066=VERTEX_POINT('',#77352);
#23067=VERTEX_POINT('',#77356);
#23068=VERTEX_POINT('',#77358);
#23069=VERTEX_POINT('',#77363);
#23070=VERTEX_POINT('',#77365);
#23071=VERTEX_POINT('',#77369);
#23072=VERTEX_POINT('',#77373);
#23073=VERTEX_POINT('',#77374);
#23074=VERTEX_POINT('',#77376);
#23075=VERTEX_POINT('',#77381);
#23076=VERTEX_POINT('',#77383);
#23077=VERTEX_POINT('',#77387);
#23078=VERTEX_POINT('',#77390);
#23079=VERTEX_POINT('',#77394);
#23080=VERTEX_POINT('',#77398);
#23081=VERTEX_POINT('',#77401);
#23082=VERTEX_POINT('',#77405);
#23083=VERTEX_POINT('',#77411);
#23084=VERTEX_POINT('',#77418);
#23085=VERTEX_POINT('',#77419);
#23086=VERTEX_POINT('',#77423);
#23087=VERTEX_POINT('',#77425);
#23088=VERTEX_POINT('',#77427);
#23089=VERTEX_POINT('',#77429);
#23090=VERTEX_POINT('',#77435);
#23091=VERTEX_POINT('',#77436);
#23092=VERTEX_POINT('',#77440);
#23093=VERTEX_POINT('',#77442);
#23094=VERTEX_POINT('',#77446);
#23095=VERTEX_POINT('',#77448);
#23096=VERTEX_POINT('',#77455);
#23097=VERTEX_POINT('',#77457);
#23098=VERTEX_POINT('',#77461);
#23099=VERTEX_POINT('',#77463);
#23100=VERTEX_POINT('',#77467);
#23101=VERTEX_POINT('',#77469);
#23102=VERTEX_POINT('',#77473);
#23103=VERTEX_POINT('',#77477);
#23104=VERTEX_POINT('',#77481);
#23105=VERTEX_POINT('',#77483);
#23106=VERTEX_POINT('',#77487);
#23107=VERTEX_POINT('',#77491);
#23108=VERTEX_POINT('',#77495);
#23109=VERTEX_POINT('',#77497);
#23110=VERTEX_POINT('',#77501);
#23111=VERTEX_POINT('',#77505);
#23112=VERTEX_POINT('',#77509);
#23113=VERTEX_POINT('',#77511);
#23114=VERTEX_POINT('',#77515);
#23115=VERTEX_POINT('',#77519);
#23116=VERTEX_POINT('',#77523);
#23117=VERTEX_POINT('',#77525);
#23118=VERTEX_POINT('',#77529);
#23119=VERTEX_POINT('',#77533);
#23120=VERTEX_POINT('',#77537);
#23121=VERTEX_POINT('',#77539);
#23122=VERTEX_POINT('',#77543);
#23123=VERTEX_POINT('',#77547);
#23124=VERTEX_POINT('',#77551);
#23125=VERTEX_POINT('',#77553);
#23126=VERTEX_POINT('',#77557);
#23127=VERTEX_POINT('',#77561);
#23128=VERTEX_POINT('',#77565);
#23129=VERTEX_POINT('',#77567);
#23130=VERTEX_POINT('',#77571);
#23131=VERTEX_POINT('',#77575);
#23132=VERTEX_POINT('',#77579);
#23133=VERTEX_POINT('',#77581);
#23134=VERTEX_POINT('',#77585);
#23135=VERTEX_POINT('',#77589);
#23136=VERTEX_POINT('',#77593);
#23137=VERTEX_POINT('',#77595);
#23138=VERTEX_POINT('',#77599);
#23139=VERTEX_POINT('',#77603);
#23140=VERTEX_POINT('',#77607);
#23141=VERTEX_POINT('',#77609);
#23142=VERTEX_POINT('',#77613);
#23143=VERTEX_POINT('',#77617);
#23144=VERTEX_POINT('',#77623);
#23145=VERTEX_POINT('',#77625);
#23146=VERTEX_POINT('',#77627);
#23147=VERTEX_POINT('',#77629);
#23148=VERTEX_POINT('',#77631);
#23149=VERTEX_POINT('',#77633);
#23150=VERTEX_POINT('',#77635);
#23151=VERTEX_POINT('',#77637);
#23152=VERTEX_POINT('',#77640);
#23153=VERTEX_POINT('',#77643);
#23154=VERTEX_POINT('',#77645);
#23155=VERTEX_POINT('',#77649);
#23156=VERTEX_POINT('',#77653);
#23157=VERTEX_POINT('',#77657);
#23158=VERTEX_POINT('',#77659);
#23159=VERTEX_POINT('',#77663);
#23160=VERTEX_POINT('',#77667);
#23161=VERTEX_POINT('',#77671);
#23162=VERTEX_POINT('',#77673);
#23163=VERTEX_POINT('',#77677);
#23164=VERTEX_POINT('',#77681);
#23165=VERTEX_POINT('',#77685);
#23166=VERTEX_POINT('',#77687);
#23167=VERTEX_POINT('',#77691);
#23168=VERTEX_POINT('',#77695);
#23169=VERTEX_POINT('',#77699);
#23170=VERTEX_POINT('',#77701);
#23171=VERTEX_POINT('',#77705);
#23172=VERTEX_POINT('',#77709);
#23173=VERTEX_POINT('',#77713);
#23174=VERTEX_POINT('',#77715);
#23175=VERTEX_POINT('',#77719);
#23176=VERTEX_POINT('',#77723);
#23177=VERTEX_POINT('',#77727);
#23178=VERTEX_POINT('',#77729);
#23179=VERTEX_POINT('',#77733);
#23180=VERTEX_POINT('',#77737);
#23181=VERTEX_POINT('',#77741);
#23182=VERTEX_POINT('',#77743);
#23183=VERTEX_POINT('',#77747);
#23184=VERTEX_POINT('',#77751);
#23185=VERTEX_POINT('',#77755);
#23186=VERTEX_POINT('',#77757);
#23187=VERTEX_POINT('',#77761);
#23188=VERTEX_POINT('',#77765);
#23189=VERTEX_POINT('',#77769);
#23190=VERTEX_POINT('',#77771);
#23191=VERTEX_POINT('',#77775);
#23192=VERTEX_POINT('',#77779);
#23193=VERTEX_POINT('',#77783);
#23194=VERTEX_POINT('',#77785);
#23195=VERTEX_POINT('',#77789);
#23196=VERTEX_POINT('',#77793);
#23197=VERTEX_POINT('',#77797);
#23198=VERTEX_POINT('',#77803);
#23199=VERTEX_POINT('',#77807);
#23200=VERTEX_POINT('',#77809);
#23201=VERTEX_POINT('',#77813);
#23202=VERTEX_POINT('',#77817);
#23203=VERTEX_POINT('',#77821);
#23204=VERTEX_POINT('',#77823);
#23205=VERTEX_POINT('',#77827);
#23206=VERTEX_POINT('',#77831);
#23207=VERTEX_POINT('',#77835);
#23208=VERTEX_POINT('',#77837);
#23209=VERTEX_POINT('',#77841);
#23210=VERTEX_POINT('',#77845);
#23211=VERTEX_POINT('',#77849);
#23212=VERTEX_POINT('',#77851);
#23213=VERTEX_POINT('',#77855);
#23214=VERTEX_POINT('',#77859);
#23215=VERTEX_POINT('',#77863);
#23216=VERTEX_POINT('',#77865);
#23217=VERTEX_POINT('',#77869);
#23218=VERTEX_POINT('',#77873);
#23219=VERTEX_POINT('',#77877);
#23220=VERTEX_POINT('',#77879);
#23221=VERTEX_POINT('',#77883);
#23222=VERTEX_POINT('',#77887);
#23223=VERTEX_POINT('',#77891);
#23224=VERTEX_POINT('',#77893);
#23225=VERTEX_POINT('',#77897);
#23226=VERTEX_POINT('',#77901);
#23227=VERTEX_POINT('',#77905);
#23228=VERTEX_POINT('',#77907);
#23229=VERTEX_POINT('',#77911);
#23230=VERTEX_POINT('',#77915);
#23231=VERTEX_POINT('',#77919);
#23232=VERTEX_POINT('',#77921);
#23233=VERTEX_POINT('',#77925);
#23234=VERTEX_POINT('',#77929);
#23235=VERTEX_POINT('',#77933);
#23236=VERTEX_POINT('',#77935);
#23237=VERTEX_POINT('',#77939);
#23238=VERTEX_POINT('',#77943);
#23239=VERTEX_POINT('',#77947);
#23240=VERTEX_POINT('',#77949);
#23241=VERTEX_POINT('',#77953);
#23242=VERTEX_POINT('',#77961);
#23243=VERTEX_POINT('',#77966);
#23244=VERTEX_POINT('',#77967);
#23245=VERTEX_POINT('',#77971);
#23246=VERTEX_POINT('',#77976);
#23247=VERTEX_POINT('',#77982);
#23248=VERTEX_POINT('',#77984);
#23249=VERTEX_POINT('',#77988);
#23250=VERTEX_POINT('',#77990);
#23251=VERTEX_POINT('',#77994);
#23252=VERTEX_POINT('',#77998);
#23253=VERTEX_POINT('',#78002);
#23254=VERTEX_POINT('',#78004);
#23255=VERTEX_POINT('',#78008);
#23256=VERTEX_POINT('',#78012);
#23257=VERTEX_POINT('',#78016);
#23258=VERTEX_POINT('',#78018);
#23259=VERTEX_POINT('',#78022);
#23260=VERTEX_POINT('',#78026);
#23261=VERTEX_POINT('',#78030);
#23262=VERTEX_POINT('',#78032);
#23263=VERTEX_POINT('',#78036);
#23264=VERTEX_POINT('',#78040);
#23265=VERTEX_POINT('',#78044);
#23266=VERTEX_POINT('',#78046);
#23267=VERTEX_POINT('',#78050);
#23268=VERTEX_POINT('',#78054);
#23269=VERTEX_POINT('',#78058);
#23270=VERTEX_POINT('',#78060);
#23271=VERTEX_POINT('',#78064);
#23272=VERTEX_POINT('',#78068);
#23273=VERTEX_POINT('',#78072);
#23274=VERTEX_POINT('',#78074);
#23275=VERTEX_POINT('',#78078);
#23276=VERTEX_POINT('',#78082);
#23277=VERTEX_POINT('',#78086);
#23278=VERTEX_POINT('',#78088);
#23279=VERTEX_POINT('',#78092);
#23280=VERTEX_POINT('',#78096);
#23281=VERTEX_POINT('',#78100);
#23282=VERTEX_POINT('',#78102);
#23283=VERTEX_POINT('',#78106);
#23284=VERTEX_POINT('',#78110);
#23285=VERTEX_POINT('',#78114);
#23286=VERTEX_POINT('',#78116);
#23287=VERTEX_POINT('',#78120);
#23288=VERTEX_POINT('',#78124);
#23289=VERTEX_POINT('',#78128);
#23290=VERTEX_POINT('',#78130);
#23291=VERTEX_POINT('',#78134);
#23292=VERTEX_POINT('',#78138);
#23293=VERTEX_POINT('',#78144);
#23294=VERTEX_POINT('',#78148);
#23295=VERTEX_POINT('',#78152);
#23296=VERTEX_POINT('',#78156);
#23297=VERTEX_POINT('',#78158);
#23298=VERTEX_POINT('',#78162);
#23299=VERTEX_POINT('',#78166);
#23300=VERTEX_POINT('',#78170);
#23301=VERTEX_POINT('',#78172);
#23302=VERTEX_POINT('',#78176);
#23303=VERTEX_POINT('',#78180);
#23304=VERTEX_POINT('',#78184);
#23305=VERTEX_POINT('',#78186);
#23306=VERTEX_POINT('',#78190);
#23307=VERTEX_POINT('',#78194);
#23308=VERTEX_POINT('',#78198);
#23309=VERTEX_POINT('',#78200);
#23310=VERTEX_POINT('',#78204);
#23311=VERTEX_POINT('',#78208);
#23312=VERTEX_POINT('',#78212);
#23313=VERTEX_POINT('',#78214);
#23314=VERTEX_POINT('',#78218);
#23315=VERTEX_POINT('',#78222);
#23316=VERTEX_POINT('',#78226);
#23317=VERTEX_POINT('',#78228);
#23318=VERTEX_POINT('',#78232);
#23319=VERTEX_POINT('',#78236);
#23320=VERTEX_POINT('',#78240);
#23321=VERTEX_POINT('',#78242);
#23322=VERTEX_POINT('',#78246);
#23323=VERTEX_POINT('',#78250);
#23324=VERTEX_POINT('',#78254);
#23325=VERTEX_POINT('',#78256);
#23326=VERTEX_POINT('',#78260);
#23327=VERTEX_POINT('',#78264);
#23328=VERTEX_POINT('',#78268);
#23329=VERTEX_POINT('',#78270);
#23330=VERTEX_POINT('',#78274);
#23331=VERTEX_POINT('',#78278);
#23332=VERTEX_POINT('',#78282);
#23333=VERTEX_POINT('',#78284);
#23334=VERTEX_POINT('',#78288);
#23335=VERTEX_POINT('',#78292);
#23336=VERTEX_POINT('',#78296);
#23337=VERTEX_POINT('',#78298);
#23338=VERTEX_POINT('',#78306);
#23339=VERTEX_POINT('',#78308);
#23340=VERTEX_POINT('',#78312);
#23341=VERTEX_POINT('',#78316);
#23342=VERTEX_POINT('',#78320);
#23343=VERTEX_POINT('',#78322);
#23344=VERTEX_POINT('',#78326);
#23345=VERTEX_POINT('',#78330);
#23346=VERTEX_POINT('',#78334);
#23347=VERTEX_POINT('',#78336);
#23348=VERTEX_POINT('',#78340);
#23349=VERTEX_POINT('',#78344);
#23350=VERTEX_POINT('',#78348);
#23351=VERTEX_POINT('',#78350);
#23352=VERTEX_POINT('',#78354);
#23353=VERTEX_POINT('',#78358);
#23354=VERTEX_POINT('',#78362);
#23355=VERTEX_POINT('',#78364);
#23356=VERTEX_POINT('',#78368);
#23357=VERTEX_POINT('',#78372);
#23358=VERTEX_POINT('',#78376);
#23359=VERTEX_POINT('',#78378);
#23360=VERTEX_POINT('',#78382);
#23361=VERTEX_POINT('',#78386);
#23362=VERTEX_POINT('',#78390);
#23363=VERTEX_POINT('',#78392);
#23364=VERTEX_POINT('',#78396);
#23365=VERTEX_POINT('',#78400);
#23366=VERTEX_POINT('',#78404);
#23367=VERTEX_POINT('',#78406);
#23368=VERTEX_POINT('',#78410);
#23369=VERTEX_POINT('',#78414);
#23370=VERTEX_POINT('',#78418);
#23371=VERTEX_POINT('',#78420);
#23372=VERTEX_POINT('',#78424);
#23373=VERTEX_POINT('',#78428);
#23374=VERTEX_POINT('',#78432);
#23375=VERTEX_POINT('',#78434);
#23376=VERTEX_POINT('',#78438);
#23377=VERTEX_POINT('',#78442);
#23378=VERTEX_POINT('',#78446);
#23379=VERTEX_POINT('',#78448);
#23380=VERTEX_POINT('',#78452);
#23381=VERTEX_POINT('',#78456);
#23382=VERTEX_POINT('',#78460);
#23383=VERTEX_POINT('',#78466);
#23384=VERTEX_POINT('',#78472);
#23385=VERTEX_POINT('',#78480);
#23386=VERTEX_POINT('',#78481);
#23387=VERTEX_POINT('',#78485);
#23388=VERTEX_POINT('',#78489);
#23389=VERTEX_POINT('',#78495);
#23390=VERTEX_POINT('',#78496);
#23391=VERTEX_POINT('',#78500);
#23392=VERTEX_POINT('',#78504);
#23393=VERTEX_POINT('',#78510);
#23394=VERTEX_POINT('',#78511);
#23395=VERTEX_POINT('',#78515);
#23396=VERTEX_POINT('',#78519);
#23397=VERTEX_POINT('',#78525);
#23398=VERTEX_POINT('',#78526);
#23399=VERTEX_POINT('',#78530);
#23400=VERTEX_POINT('',#78534);
#23401=VERTEX_POINT('',#78540);
#23402=VERTEX_POINT('',#78541);
#23403=VERTEX_POINT('',#78545);
#23404=VERTEX_POINT('',#78549);
#23405=VERTEX_POINT('',#78555);
#23406=VERTEX_POINT('',#78556);
#23407=VERTEX_POINT('',#78560);
#23408=VERTEX_POINT('',#78564);
#23409=VERTEX_POINT('',#78570);
#23410=VERTEX_POINT('',#78571);
#23411=VERTEX_POINT('',#78575);
#23412=VERTEX_POINT('',#78579);
#23413=VERTEX_POINT('',#78585);
#23414=VERTEX_POINT('',#78586);
#23415=VERTEX_POINT('',#78590);
#23416=VERTEX_POINT('',#78594);
#23417=VERTEX_POINT('',#78600);
#23418=VERTEX_POINT('',#78601);
#23419=VERTEX_POINT('',#78605);
#23420=VERTEX_POINT('',#78609);
#23421=VERTEX_POINT('',#78615);
#23422=VERTEX_POINT('',#78616);
#23423=VERTEX_POINT('',#78620);
#23424=VERTEX_POINT('',#78624);
#23425=VERTEX_POINT('',#78630);
#23426=VERTEX_POINT('',#78631);
#23427=VERTEX_POINT('',#78635);
#23428=VERTEX_POINT('',#78639);
#23429=VERTEX_POINT('',#78645);
#23430=VERTEX_POINT('',#78646);
#23431=VERTEX_POINT('',#78650);
#23432=VERTEX_POINT('',#78654);
#23433=VERTEX_POINT('',#78660);
#23434=VERTEX_POINT('',#78661);
#23435=VERTEX_POINT('',#78665);
#23436=VERTEX_POINT('',#78669);
#23437=VERTEX_POINT('',#78675);
#23438=VERTEX_POINT('',#78676);
#23439=VERTEX_POINT('',#78680);
#23440=VERTEX_POINT('',#78684);
#23441=VERTEX_POINT('',#78690);
#23442=VERTEX_POINT('',#78691);
#23443=VERTEX_POINT('',#78695);
#23444=VERTEX_POINT('',#78699);
#23445=VERTEX_POINT('',#78705);
#23446=VERTEX_POINT('',#78706);
#23447=VERTEX_POINT('',#78710);
#23448=VERTEX_POINT('',#78714);
#23449=VERTEX_POINT('',#78720);
#23450=VERTEX_POINT('',#78721);
#23451=VERTEX_POINT('',#78725);
#23452=VERTEX_POINT('',#78729);
#23453=VERTEX_POINT('',#78735);
#23454=VERTEX_POINT('',#78736);
#23455=VERTEX_POINT('',#78740);
#23456=VERTEX_POINT('',#78744);
#23457=VERTEX_POINT('',#78750);
#23458=VERTEX_POINT('',#78751);
#23459=VERTEX_POINT('',#78755);
#23460=VERTEX_POINT('',#78759);
#23461=VERTEX_POINT('',#78765);
#23462=VERTEX_POINT('',#78766);
#23463=VERTEX_POINT('',#78770);
#23464=VERTEX_POINT('',#78774);
#23465=VERTEX_POINT('',#78780);
#23466=VERTEX_POINT('',#78781);
#23467=VERTEX_POINT('',#78785);
#23468=VERTEX_POINT('',#78789);
#23469=VERTEX_POINT('',#78795);
#23470=VERTEX_POINT('',#78796);
#23471=VERTEX_POINT('',#78800);
#23472=VERTEX_POINT('',#78804);
#23473=VERTEX_POINT('',#78810);
#23474=VERTEX_POINT('',#78811);
#23475=VERTEX_POINT('',#78815);
#23476=VERTEX_POINT('',#78819);
#23477=VERTEX_POINT('',#78825);
#23478=VERTEX_POINT('',#78826);
#23479=VERTEX_POINT('',#78830);
#23480=VERTEX_POINT('',#78834);
#23481=VERTEX_POINT('',#78840);
#23482=VERTEX_POINT('',#78841);
#23483=VERTEX_POINT('',#78845);
#23484=VERTEX_POINT('',#78849);
#23485=VERTEX_POINT('',#78855);
#23486=VERTEX_POINT('',#78856);
#23487=VERTEX_POINT('',#78860);
#23488=VERTEX_POINT('',#78864);
#23489=VERTEX_POINT('',#78870);
#23490=VERTEX_POINT('',#78871);
#23491=VERTEX_POINT('',#78875);
#23492=VERTEX_POINT('',#78879);
#23493=VERTEX_POINT('',#78885);
#23494=VERTEX_POINT('',#78886);
#23495=VERTEX_POINT('',#78890);
#23496=VERTEX_POINT('',#78894);
#23497=VERTEX_POINT('',#78900);
#23498=VERTEX_POINT('',#78901);
#23499=VERTEX_POINT('',#78905);
#23500=VERTEX_POINT('',#78909);
#23501=VERTEX_POINT('',#78915);
#23502=VERTEX_POINT('',#78916);
#23503=VERTEX_POINT('',#78920);
#23504=VERTEX_POINT('',#78924);
#23505=VERTEX_POINT('',#78930);
#23506=VERTEX_POINT('',#78931);
#23507=VERTEX_POINT('',#78935);
#23508=VERTEX_POINT('',#78939);
#23509=VERTEX_POINT('',#78945);
#23510=VERTEX_POINT('',#78946);
#23511=VERTEX_POINT('',#78950);
#23512=VERTEX_POINT('',#78954);
#23513=VERTEX_POINT('',#78960);
#23514=VERTEX_POINT('',#78961);
#23515=VERTEX_POINT('',#78965);
#23516=VERTEX_POINT('',#78969);
#23517=VERTEX_POINT('',#78975);
#23518=VERTEX_POINT('',#78977);
#23519=VERTEX_POINT('',#78981);
#23520=VERTEX_POINT('',#78985);
#23521=VERTEX_POINT('',#78989);
#23522=VERTEX_POINT('',#78995);
#23523=VERTEX_POINT('',#78997);
#23524=VERTEX_POINT('',#79001);
#23525=VERTEX_POINT('',#79005);
#23526=VERTEX_POINT('',#79009);
#23527=VERTEX_POINT('',#79015);
#23528=VERTEX_POINT('',#79017);
#23529=VERTEX_POINT('',#79021);
#23530=VERTEX_POINT('',#79025);
#23531=VERTEX_POINT('',#79029);
#23532=VERTEX_POINT('',#79035);
#23533=VERTEX_POINT('',#79037);
#23534=VERTEX_POINT('',#79041);
#23535=VERTEX_POINT('',#79045);
#23536=VERTEX_POINT('',#79049);
#23537=VERTEX_POINT('',#79055);
#23538=VERTEX_POINT('',#79057);
#23539=VERTEX_POINT('',#79061);
#23540=VERTEX_POINT('',#79065);
#23541=VERTEX_POINT('',#79069);
#23542=VERTEX_POINT('',#79075);
#23543=VERTEX_POINT('',#79077);
#23544=VERTEX_POINT('',#79081);
#23545=VERTEX_POINT('',#79085);
#23546=VERTEX_POINT('',#79089);
#23547=VERTEX_POINT('',#79095);
#23548=VERTEX_POINT('',#79097);
#23549=VERTEX_POINT('',#79101);
#23550=VERTEX_POINT('',#79105);
#23551=VERTEX_POINT('',#79109);
#23552=VERTEX_POINT('',#79115);
#23553=VERTEX_POINT('',#79117);
#23554=VERTEX_POINT('',#79121);
#23555=VERTEX_POINT('',#79125);
#23556=VERTEX_POINT('',#79129);
#23557=VERTEX_POINT('',#79135);
#23558=VERTEX_POINT('',#79137);
#23559=VERTEX_POINT('',#79141);
#23560=VERTEX_POINT('',#79145);
#23561=VERTEX_POINT('',#79149);
#23562=VERTEX_POINT('',#79155);
#23563=VERTEX_POINT('',#79157);
#23564=VERTEX_POINT('',#79161);
#23565=VERTEX_POINT('',#79165);
#23566=VERTEX_POINT('',#79169);
#23567=VERTEX_POINT('',#79175);
#23568=VERTEX_POINT('',#79177);
#23569=VERTEX_POINT('',#79181);
#23570=VERTEX_POINT('',#79185);
#23571=VERTEX_POINT('',#79189);
#23572=VERTEX_POINT('',#79195);
#23573=VERTEX_POINT('',#79197);
#23574=VERTEX_POINT('',#79201);
#23575=VERTEX_POINT('',#79205);
#23576=VERTEX_POINT('',#79209);
#23577=VERTEX_POINT('',#79215);
#23578=VERTEX_POINT('',#79217);
#23579=VERTEX_POINT('',#79221);
#23580=VERTEX_POINT('',#79225);
#23581=VERTEX_POINT('',#79229);
#23582=VERTEX_POINT('',#79235);
#23583=VERTEX_POINT('',#79237);
#23584=VERTEX_POINT('',#79241);
#23585=VERTEX_POINT('',#79245);
#23586=VERTEX_POINT('',#79249);
#23587=VERTEX_POINT('',#79255);
#23588=VERTEX_POINT('',#79257);
#23589=VERTEX_POINT('',#79261);
#23590=VERTEX_POINT('',#79265);
#23591=VERTEX_POINT('',#79269);
#23592=VERTEX_POINT('',#79275);
#23593=VERTEX_POINT('',#79277);
#23594=VERTEX_POINT('',#79281);
#23595=VERTEX_POINT('',#79285);
#23596=VERTEX_POINT('',#79289);
#23597=VERTEX_POINT('',#79295);
#23598=VERTEX_POINT('',#79297);
#23599=VERTEX_POINT('',#79301);
#23600=VERTEX_POINT('',#79305);
#23601=VERTEX_POINT('',#79309);
#23602=VERTEX_POINT('',#79315);
#23603=VERTEX_POINT('',#79317);
#23604=VERTEX_POINT('',#79321);
#23605=VERTEX_POINT('',#79325);
#23606=VERTEX_POINT('',#79329);
#23607=VERTEX_POINT('',#79335);
#23608=VERTEX_POINT('',#79337);
#23609=VERTEX_POINT('',#79341);
#23610=VERTEX_POINT('',#79345);
#23611=VERTEX_POINT('',#79349);
#23612=VERTEX_POINT('',#79355);
#23613=VERTEX_POINT('',#79357);
#23614=VERTEX_POINT('',#79361);
#23615=VERTEX_POINT('',#79365);
#23616=VERTEX_POINT('',#79369);
#23617=VERTEX_POINT('',#79375);
#23618=VERTEX_POINT('',#79377);
#23619=VERTEX_POINT('',#79381);
#23620=VERTEX_POINT('',#79385);
#23621=VERTEX_POINT('',#79389);
#23622=VERTEX_POINT('',#79395);
#23623=VERTEX_POINT('',#79397);
#23624=VERTEX_POINT('',#79401);
#23625=VERTEX_POINT('',#79405);
#23626=VERTEX_POINT('',#79409);
#23627=VERTEX_POINT('',#79415);
#23628=VERTEX_POINT('',#79417);
#23629=VERTEX_POINT('',#79421);
#23630=VERTEX_POINT('',#79425);
#23631=VERTEX_POINT('',#79429);
#23632=VERTEX_POINT('',#79435);
#23633=VERTEX_POINT('',#79437);
#23634=VERTEX_POINT('',#79441);
#23635=VERTEX_POINT('',#79445);
#23636=VERTEX_POINT('',#79449);
#23637=VERTEX_POINT('',#79455);
#23638=VERTEX_POINT('',#79457);
#23639=VERTEX_POINT('',#79461);
#23640=VERTEX_POINT('',#79465);
#23641=VERTEX_POINT('',#79469);
#23642=VERTEX_POINT('',#79475);
#23643=VERTEX_POINT('',#79477);
#23644=VERTEX_POINT('',#79481);
#23645=VERTEX_POINT('',#79485);
#23646=VERTEX_POINT('',#79489);
#23647=VERTEX_POINT('',#79495);
#23648=VERTEX_POINT('',#79497);
#23649=VERTEX_POINT('',#79501);
#23650=VERTEX_POINT('',#79505);
#23651=VERTEX_POINT('',#79509);
#23652=VERTEX_POINT('',#79515);
#23653=VERTEX_POINT('',#79517);
#23654=VERTEX_POINT('',#79521);
#23655=VERTEX_POINT('',#79525);
#23656=VERTEX_POINT('',#79529);
#23657=VERTEX_POINT('',#79535);
#23658=VERTEX_POINT('',#79537);
#23659=VERTEX_POINT('',#79541);
#23660=VERTEX_POINT('',#79545);
#23661=VERTEX_POINT('',#79549);
#23662=VERTEX_POINT('',#79555);
#23663=VERTEX_POINT('',#79557);
#23664=VERTEX_POINT('',#79561);
#23665=VERTEX_POINT('',#79565);
#23666=VERTEX_POINT('',#79569);
#23667=VERTEX_POINT('',#79575);
#23668=VERTEX_POINT('',#79577);
#23669=VERTEX_POINT('',#79581);
#23670=VERTEX_POINT('',#79585);
#23671=VERTEX_POINT('',#79589);
#23672=VERTEX_POINT('',#79595);
#23673=VERTEX_POINT('',#79597);
#23674=VERTEX_POINT('',#79601);
#23675=VERTEX_POINT('',#79605);
#23676=VERTEX_POINT('',#79609);
#23677=VERTEX_POINT('',#79615);
#23678=VERTEX_POINT('',#79617);
#23679=VERTEX_POINT('',#79621);
#23680=VERTEX_POINT('',#79625);
#23681=VERTEX_POINT('',#79629);
#23682=VERTEX_POINT('',#79635);
#23683=VERTEX_POINT('',#79641);
#23684=VERTEX_POINT('',#79647);
#23685=VERTEX_POINT('',#79653);
#23686=VERTEX_POINT('',#79659);
#23687=VERTEX_POINT('',#79665);
#23688=VERTEX_POINT('',#79671);
#23689=VERTEX_POINT('',#79677);
#23690=VERTEX_POINT('',#79683);
#23691=VERTEX_POINT('',#79689);
#23692=VERTEX_POINT('',#79695);
#23693=VERTEX_POINT('',#79701);
#23694=VERTEX_POINT('',#79707);
#23695=VERTEX_POINT('',#79713);
#23696=VERTEX_POINT('',#79719);
#23697=VERTEX_POINT('',#79725);
#23698=VERTEX_POINT('',#79731);
#23699=VERTEX_POINT('',#79737);
#23700=VERTEX_POINT('',#79743);
#23701=VERTEX_POINT('',#79749);
#23702=VERTEX_POINT('',#79755);
#23703=VERTEX_POINT('',#79761);
#23704=VERTEX_POINT('',#79767);
#23705=VERTEX_POINT('',#79773);
#23706=VERTEX_POINT('',#79779);
#23707=VERTEX_POINT('',#79785);
#23708=VERTEX_POINT('',#79791);
#23709=VERTEX_POINT('',#79797);
#23710=VERTEX_POINT('',#79803);
#23711=VERTEX_POINT('',#79809);
#23712=VERTEX_POINT('',#79815);
#23713=VERTEX_POINT('',#79821);
#23714=VERTEX_POINT('',#79827);
#23715=VERTEX_POINT('',#79833);
#23716=VERTEX_POINT('',#79837);
#23717=VERTEX_POINT('',#79841);
#23718=VERTEX_POINT('',#79845);
#23719=VERTEX_POINT('',#79849);
#23720=VERTEX_POINT('',#79853);
#23721=VERTEX_POINT('',#79857);
#23722=VERTEX_POINT('',#79861);
#23723=VERTEX_POINT('',#79865);
#23724=VERTEX_POINT('',#79869);
#23725=VERTEX_POINT('',#79873);
#23726=VERTEX_POINT('',#79877);
#23727=VERTEX_POINT('',#79881);
#23728=VERTEX_POINT('',#79885);
#23729=VERTEX_POINT('',#79889);
#23730=VERTEX_POINT('',#79893);
#23731=VERTEX_POINT('',#79897);
#23732=VERTEX_POINT('',#79901);
#23733=VERTEX_POINT('',#79905);
#23734=VERTEX_POINT('',#79909);
#23735=VERTEX_POINT('',#79913);
#23736=VERTEX_POINT('',#79916);
#23737=VERTEX_POINT('',#79920);
#23738=VERTEX_POINT('',#79924);
#23739=VERTEX_POINT('',#79928);
#23740=VERTEX_POINT('',#79932);
#23741=VERTEX_POINT('',#79936);
#23742=VERTEX_POINT('',#79940);
#23743=VERTEX_POINT('',#79944);
#23744=VERTEX_POINT('',#79948);
#23745=VERTEX_POINT('',#79952);
#23746=VERTEX_POINT('',#79956);
#23747=VERTEX_POINT('',#79960);
#23748=VERTEX_POINT('',#79964);
#23749=VERTEX_POINT('',#79968);
#23750=VERTEX_POINT('',#79972);
#23751=VERTEX_POINT('',#79976);
#23752=VERTEX_POINT('',#79980);
#23753=VERTEX_POINT('',#79984);
#23754=VERTEX_POINT('',#79988);
#23755=VERTEX_POINT('',#79992);
#23756=VERTEX_POINT('',#79996);
#23757=VERTEX_POINT('',#80000);
#23758=VERTEX_POINT('',#80003);
#23759=VERTEX_POINT('',#80007);
#23760=VERTEX_POINT('',#80011);
#23761=VERTEX_POINT('',#80015);
#23762=VERTEX_POINT('',#80019);
#23763=VERTEX_POINT('',#80023);
#23764=VERTEX_POINT('',#80027);
#23765=VERTEX_POINT('',#80031);
#23766=VERTEX_POINT('',#80035);
#23767=VERTEX_POINT('',#80039);
#23768=VERTEX_POINT('',#80043);
#23769=VERTEX_POINT('',#80047);
#23770=VERTEX_POINT('',#80051);
#23771=VERTEX_POINT('',#80055);
#23772=VERTEX_POINT('',#80059);
#23773=VERTEX_POINT('',#80063);
#23774=VERTEX_POINT('',#80067);
#23775=VERTEX_POINT('',#80071);
#23776=VERTEX_POINT('',#80075);
#23777=VERTEX_POINT('',#80079);
#23778=VERTEX_POINT('',#80083);
#23779=VERTEX_POINT('',#80087);
#23780=VERTEX_POINT('',#80090);
#23781=VERTEX_POINT('',#80325);
#23782=VERTEX_POINT('',#80326);
#23783=VERTEX_POINT('',#80328);
#23784=VERTEX_POINT('',#80333);
#23785=VERTEX_POINT('',#80336);
#23786=VERTEX_POINT('',#80340);
#23787=VERTEX_POINT('',#80342);
#23788=VERTEX_POINT('',#80344);
#23789=VERTEX_POINT('',#80348);
#23790=VERTEX_POINT('',#80353);
#23791=VERTEX_POINT('',#80355);
#23792=VERTEX_POINT('',#80359);
#23793=VERTEX_POINT('',#80363);
#23794=VERTEX_POINT('',#80364);
#23795=VERTEX_POINT('',#80369);
#23796=VERTEX_POINT('',#80373);
#23797=VERTEX_POINT('',#80375);
#23798=VERTEX_POINT('',#80379);
#23799=VERTEX_POINT('',#80385);
#23800=VERTEX_POINT('',#80391);
#23801=VERTEX_POINT('',#80393);
#23802=VERTEX_POINT('',#80397);
#23803=VERTEX_POINT('',#80399);
#23804=VERTEX_POINT('',#80401);
#23805=VERTEX_POINT('',#80403);
#23806=VERTEX_POINT('',#80405);
#23807=VERTEX_POINT('',#80407);
#23808=VERTEX_POINT('',#80409);
#23809=VERTEX_POINT('',#80412);
#23810=VERTEX_POINT('',#80416);
#23811=VERTEX_POINT('',#80420);
#23812=VERTEX_POINT('',#80424);
#23813=VERTEX_POINT('',#80426);
#23814=VERTEX_POINT('',#80430);
#23815=VERTEX_POINT('',#80432);
#23816=VERTEX_POINT('',#80436);
#23817=VERTEX_POINT('',#80438);
#23818=VERTEX_POINT('',#80442);
#23819=VERTEX_POINT('',#80444);
#23820=VERTEX_POINT('',#80448);
#23821=VERTEX_POINT('',#80453);
#23822=VERTEX_POINT('',#80458);
#23823=VERTEX_POINT('',#80463);
#23824=VERTEX_POINT('',#80468);
#23825=VERTEX_POINT('',#80469);
#23826=VERTEX_POINT('',#80473);
#23827=VERTEX_POINT('',#80477);
#23828=VERTEX_POINT('',#80481);
#23829=VERTEX_POINT('',#80483);
#23830=VERTEX_POINT('',#80487);
#23831=VERTEX_POINT('',#80491);
#23832=VERTEX_POINT('',#80494);
#23833=VERTEX_POINT('',#80498);
#23834=VERTEX_POINT('',#80502);
#23835=VERTEX_POINT('',#80505);
#23836=VERTEX_POINT('',#80509);
#23837=VERTEX_POINT('',#80515);
#23838=VERTEX_POINT('',#80518);
#23839=VERTEX_POINT('',#80522);
#23840=VERTEX_POINT('',#80528);
#23841=VERTEX_POINT('',#80529);
#23842=VERTEX_POINT('',#80531);
#23843=VERTEX_POINT('',#80533);
#23844=VERTEX_POINT('',#80537);
#23845=VERTEX_POINT('',#80539);
#23846=VERTEX_POINT('',#80543);
#23847=VERTEX_POINT('',#80545);
#23848=VERTEX_POINT('',#80549);
#23849=VERTEX_POINT('',#80551);
#23850=VERTEX_POINT('',#80555);
#23851=VERTEX_POINT('',#80557);
#23852=VERTEX_POINT('',#80561);
#23853=VERTEX_POINT('',#80563);
#23854=VERTEX_POINT('',#80567);
#23855=VERTEX_POINT('',#80569);
#23856=VERTEX_POINT('',#80573);
#23857=VERTEX_POINT('',#80575);
#23858=VERTEX_POINT('',#80579);
#23859=VERTEX_POINT('',#80581);
#23860=VERTEX_POINT('',#80585);
#23861=VERTEX_POINT('',#80587);
#23862=VERTEX_POINT('',#80591);
#23863=VERTEX_POINT('',#80593);
#23864=VERTEX_POINT('',#80601);
#23865=VERTEX_POINT('',#80602);
#23866=VERTEX_POINT('',#80604);
#23867=VERTEX_POINT('',#80606);
#23868=VERTEX_POINT('',#80610);
#23869=VERTEX_POINT('',#80612);
#23870=VERTEX_POINT('',#80616);
#23871=VERTEX_POINT('',#80618);
#23872=VERTEX_POINT('',#80631);
#23873=VERTEX_POINT('',#80632);
#23874=VERTEX_POINT('',#80636);
#23875=VERTEX_POINT('',#80638);
#23876=VERTEX_POINT('',#80649);
#23877=VERTEX_POINT('',#80653);
#23878=VERTEX_POINT('',#80664);
#23879=VERTEX_POINT('',#80668);
#23880=VERTEX_POINT('',#80679);
#23881=VERTEX_POINT('',#80683);
#23882=VERTEX_POINT('',#80694);
#23883=VERTEX_POINT('',#80698);
#23884=VERTEX_POINT('',#80709);
#23885=VERTEX_POINT('',#80713);
#23886=VERTEX_POINT('',#80724);
#23887=VERTEX_POINT('',#80728);
#23888=VERTEX_POINT('',#80739);
#23889=VERTEX_POINT('',#80743);
#23890=VERTEX_POINT('',#80754);
#23891=VERTEX_POINT('',#80758);
#23892=VERTEX_POINT('',#80769);
#23893=VERTEX_POINT('',#80773);
#23894=VERTEX_POINT('',#80784);
#23895=VERTEX_POINT('',#80788);
#23896=VERTEX_POINT('',#80799);
#23897=VERTEX_POINT('',#80803);
#23898=VERTEX_POINT('',#80814);
#23899=VERTEX_POINT('',#80818);
#23900=VERTEX_POINT('',#80824);
#23901=VERTEX_POINT('',#80826);
#23902=VERTEX_POINT('',#80835);
#23903=VERTEX_POINT('',#80839);
#23904=VERTEX_POINT('',#80850);
#23905=VERTEX_POINT('',#80854);
#23906=VERTEX_POINT('',#80865);
#23907=VERTEX_POINT('',#80869);
#23908=VERTEX_POINT('',#80880);
#23909=VERTEX_POINT('',#80884);
#23910=VERTEX_POINT('',#80895);
#23911=VERTEX_POINT('',#80899);
#23912=VERTEX_POINT('',#80910);
#23913=VERTEX_POINT('',#80914);
#23914=VERTEX_POINT('',#80925);
#23915=VERTEX_POINT('',#80929);
#23916=VERTEX_POINT('',#80940);
#23917=VERTEX_POINT('',#80944);
#23918=VERTEX_POINT('',#80955);
#23919=VERTEX_POINT('',#80959);
#23920=VERTEX_POINT('',#80970);
#23921=VERTEX_POINT('',#80974);
#23922=VERTEX_POINT('',#80985);
#23923=VERTEX_POINT('',#80989);
#23924=VERTEX_POINT('',#81000);
#23925=VERTEX_POINT('',#81004);
#23926=VERTEX_POINT('',#81015);
#23927=VERTEX_POINT('',#81019);
#23928=VERTEX_POINT('',#81030);
#23929=VERTEX_POINT('',#81034);
#23930=VERTEX_POINT('',#81045);
#23931=VERTEX_POINT('',#81049);
#23932=VERTEX_POINT('',#81060);
#23933=VERTEX_POINT('',#81064);
#23934=VERTEX_POINT('',#81075);
#23935=VERTEX_POINT('',#81079);
#23936=VERTEX_POINT('',#81090);
#23937=VERTEX_POINT('',#81094);
#23938=VERTEX_POINT('',#81100);
#23939=VERTEX_POINT('',#81102);
#23940=VERTEX_POINT('',#81111);
#23941=VERTEX_POINT('',#81115);
#23942=VERTEX_POINT('',#81139);
#23943=VERTEX_POINT('',#81140);
#23944=VERTEX_POINT('',#81144);
#23945=VERTEX_POINT('',#81146);
#23946=VERTEX_POINT('',#81157);
#23947=VERTEX_POINT('',#81161);
#23948=VERTEX_POINT('',#81172);
#23949=VERTEX_POINT('',#81176);
#23950=VERTEX_POINT('',#81187);
#23951=VERTEX_POINT('',#81191);
#23952=VERTEX_POINT('',#81202);
#23953=VERTEX_POINT('',#81206);
#23954=VERTEX_POINT('',#81217);
#23955=VERTEX_POINT('',#81221);
#23956=VERTEX_POINT('',#81232);
#23957=VERTEX_POINT('',#81236);
#23958=VERTEX_POINT('',#81247);
#23959=VERTEX_POINT('',#81251);
#23960=VERTEX_POINT('',#81257);
#23961=VERTEX_POINT('',#81259);
#23962=VERTEX_POINT('',#81268);
#23963=VERTEX_POINT('',#81272);
#23964=VERTEX_POINT('',#81283);
#23965=VERTEX_POINT('',#81287);
#23966=VERTEX_POINT('',#81298);
#23967=VERTEX_POINT('',#81302);
#23968=VERTEX_POINT('',#81313);
#23969=VERTEX_POINT('',#81317);
#23970=VERTEX_POINT('',#81328);
#23971=VERTEX_POINT('',#81332);
#23972=VERTEX_POINT('',#81343);
#23973=VERTEX_POINT('',#81347);
#23974=VERTEX_POINT('',#81358);
#23975=VERTEX_POINT('',#81362);
#23976=VERTEX_POINT('',#81373);
#23977=VERTEX_POINT('',#81377);
#23978=VERTEX_POINT('',#81388);
#23979=VERTEX_POINT('',#81392);
#23980=VERTEX_POINT('',#81403);
#23981=VERTEX_POINT('',#81407);
#23982=VERTEX_POINT('',#81413);
#23983=VERTEX_POINT('',#81415);
#23984=VERTEX_POINT('',#81424);
#23985=VERTEX_POINT('',#81428);
#23986=VERTEX_POINT('',#81447);
#23987=VERTEX_POINT('',#81448);
#23988=VERTEX_POINT('',#81450);
#23989=VERTEX_POINT('',#81452);
#23990=VERTEX_POINT('',#81456);
#23991=VERTEX_POINT('',#81458);
#23992=VERTEX_POINT('',#81462);
#23993=VERTEX_POINT('',#81464);
#23994=VERTEX_POINT('',#81468);
#23995=VERTEX_POINT('',#81470);
#23996=VERTEX_POINT('',#81474);
#23997=VERTEX_POINT('',#81476);
#23998=VERTEX_POINT('',#81484);
#23999=VERTEX_POINT('',#81485);
#24000=VERTEX_POINT('',#81487);
#24001=VERTEX_POINT('',#81489);
#24002=VERTEX_POINT('',#81493);
#24003=VERTEX_POINT('',#81495);
#24004=VERTEX_POINT('',#81499);
#24005=VERTEX_POINT('',#81501);
#24006=VERTEX_POINT('',#81505);
#24007=VERTEX_POINT('',#81507);
#24008=VERTEX_POINT('',#81511);
#24009=VERTEX_POINT('',#81513);
#24010=VERTEX_POINT('',#81517);
#24011=VERTEX_POINT('',#81519);
#24012=VERTEX_POINT('',#81523);
#24013=VERTEX_POINT('',#81525);
#24014=VERTEX_POINT('',#81538);
#24015=VERTEX_POINT('',#81539);
#24016=VERTEX_POINT('',#81543);
#24017=VERTEX_POINT('',#81545);
#24018=VERTEX_POINT('',#81556);
#24019=VERTEX_POINT('',#81560);
#24020=VERTEX_POINT('',#81571);
#24021=VERTEX_POINT('',#81575);
#24022=VERTEX_POINT('',#81586);
#24023=VERTEX_POINT('',#81590);
#24024=VERTEX_POINT('',#81596);
#24025=VERTEX_POINT('',#81598);
#24026=VERTEX_POINT('',#81602);
#24027=VERTEX_POINT('',#81604);
#24028=VERTEX_POINT('',#81608);
#24029=VERTEX_POINT('',#81610);
#24030=VERTEX_POINT('',#81619);
#24031=VERTEX_POINT('',#81623);
#24032=VERTEX_POINT('',#81634);
#24033=VERTEX_POINT('',#81638);
#24034=VERTEX_POINT('',#81649);
#24035=VERTEX_POINT('',#81653);
#24036=VERTEX_POINT('',#81664);
#24037=VERTEX_POINT('',#81668);
#24038=VERTEX_POINT('',#81679);
#24039=VERTEX_POINT('',#81683);
#24040=VERTEX_POINT('',#81694);
#24041=VERTEX_POINT('',#81698);
#24042=VERTEX_POINT('',#81704);
#24043=VERTEX_POINT('',#81706);
#24044=VERTEX_POINT('',#81710);
#24045=VERTEX_POINT('',#81712);
#24046=VERTEX_POINT('',#81716);
#24047=VERTEX_POINT('',#81718);
#24048=VERTEX_POINT('',#81735);
#24049=VERTEX_POINT('',#81736);
#24050=VERTEX_POINT('',#81738);
#24051=VERTEX_POINT('',#81740);
#24052=VERTEX_POINT('',#81749);
#24053=VERTEX_POINT('',#81753);
#24054=VERTEX_POINT('',#81764);
#24055=VERTEX_POINT('',#81768);
#24056=VERTEX_POINT('',#81779);
#24057=VERTEX_POINT('',#81783);
#24058=VERTEX_POINT('',#81794);
#24059=VERTEX_POINT('',#81798);
#24060=VERTEX_POINT('',#81804);
#24061=VERTEX_POINT('',#81806);
#24062=VERTEX_POINT('',#81810);
#24063=VERTEX_POINT('',#81812);
#24064=VERTEX_POINT('',#81816);
#24065=VERTEX_POINT('',#81818);
#24066=VERTEX_POINT('',#81827);
#24067=VERTEX_POINT('',#81831);
#24068=VERTEX_POINT('',#81842);
#24069=VERTEX_POINT('',#81846);
#24070=VERTEX_POINT('',#81857);
#24071=VERTEX_POINT('',#81861);
#24072=VERTEX_POINT('',#81872);
#24073=VERTEX_POINT('',#81876);
#24074=VERTEX_POINT('',#81887);
#24075=VERTEX_POINT('',#81891);
#24076=VERTEX_POINT('',#81902);
#24077=VERTEX_POINT('',#81906);
#24078=VERTEX_POINT('',#81917);
#24079=VERTEX_POINT('',#81921);
#24080=VERTEX_POINT('',#81927);
#24081=VERTEX_POINT('',#81929);
#24082=VERTEX_POINT('',#81933);
#24083=VERTEX_POINT('',#81935);
#24084=VERTEX_POINT('',#81939);
#24085=VERTEX_POINT('',#81941);
#24086=VERTEX_POINT('',#81949);
#24087=VERTEX_POINT('',#81950);
#24088=VERTEX_POINT('',#81952);
#24089=VERTEX_POINT('',#81954);
#24090=VERTEX_POINT('',#81958);
#24091=VERTEX_POINT('',#81960);
#24092=VERTEX_POINT('',#81964);
#24093=VERTEX_POINT('',#81966);
#24094=VERTEX_POINT('',#81970);
#24095=VERTEX_POINT('',#81972);
#24096=VERTEX_POINT('',#81976);
#24097=VERTEX_POINT('',#81978);
#24098=VERTEX_POINT('',#81982);
#24099=VERTEX_POINT('',#81984);
#24100=VERTEX_POINT('',#81988);
#24101=VERTEX_POINT('',#81990);
#24102=VERTEX_POINT('',#82003);
#24103=VERTEX_POINT('',#82004);
#24104=VERTEX_POINT('',#82008);
#24105=VERTEX_POINT('',#82010);
#24106=VERTEX_POINT('',#82021);
#24107=VERTEX_POINT('',#82025);
#24108=VERTEX_POINT('',#82031);
#24109=VERTEX_POINT('',#82033);
#24110=VERTEX_POINT('',#82042);
#24111=VERTEX_POINT('',#82046);
#24112=VERTEX_POINT('',#82057);
#24113=VERTEX_POINT('',#82061);
#24114=VERTEX_POINT('',#82067);
#24115=VERTEX_POINT('',#82069);
#24116=VERTEX_POINT('',#82073);
#24117=VERTEX_POINT('',#82075);
#24118=VERTEX_POINT('',#82079);
#24119=VERTEX_POINT('',#82081);
#24120=VERTEX_POINT('',#82094);
#24121=VERTEX_POINT('',#82095);
#24122=VERTEX_POINT('',#82099);
#24123=VERTEX_POINT('',#82101);
#24124=VERTEX_POINT('',#82112);
#24125=VERTEX_POINT('',#82116);
#24126=VERTEX_POINT('',#82127);
#24127=VERTEX_POINT('',#82131);
#24128=VERTEX_POINT('',#82142);
#24129=VERTEX_POINT('',#82146);
#24130=VERTEX_POINT('',#82157);
#24131=VERTEX_POINT('',#82161);
#24132=VERTEX_POINT('',#82172);
#24133=VERTEX_POINT('',#82176);
#24134=VERTEX_POINT('',#82187);
#24135=VERTEX_POINT('',#82191);
#24136=VERTEX_POINT('',#82202);
#24137=VERTEX_POINT('',#82206);
#24138=VERTEX_POINT('',#82217);
#24139=VERTEX_POINT('',#82221);
#24140=VERTEX_POINT('',#82232);
#24141=VERTEX_POINT('',#82236);
#24142=VERTEX_POINT('',#82247);
#24143=VERTEX_POINT('',#82251);
#24144=VERTEX_POINT('',#82275);
#24145=VERTEX_POINT('',#82276);
#24146=VERTEX_POINT('',#82280);
#24147=VERTEX_POINT('',#82282);
#24148=VERTEX_POINT('',#82293);
#24149=VERTEX_POINT('',#82297);
#24150=VERTEX_POINT('',#82303);
#24151=VERTEX_POINT('',#82305);
#24152=VERTEX_POINT('',#82314);
#24153=VERTEX_POINT('',#82318);
#24154=VERTEX_POINT('',#82329);
#24155=VERTEX_POINT('',#82333);
#24156=VERTEX_POINT('',#82339);
#24157=VERTEX_POINT('',#82341);
#24158=VERTEX_POINT('',#82345);
#24159=VERTEX_POINT('',#82347);
#24160=VERTEX_POINT('',#82351);
#24161=VERTEX_POINT('',#82353);
#24162=VERTEX_POINT('',#82361);
#24163=VERTEX_POINT('',#82362);
#24164=VERTEX_POINT('',#82364);
#24165=VERTEX_POINT('',#82366);
#24166=VERTEX_POINT('',#82370);
#24167=VERTEX_POINT('',#82372);
#24168=VERTEX_POINT('',#82376);
#24169=VERTEX_POINT('',#82378);
#24170=VERTEX_POINT('',#82391);
#24171=VERTEX_POINT('',#82392);
#24172=VERTEX_POINT('',#82396);
#24173=VERTEX_POINT('',#82398);
#24174=VERTEX_POINT('',#82409);
#24175=VERTEX_POINT('',#82413);
#24176=VERTEX_POINT('',#82424);
#24177=VERTEX_POINT('',#82428);
#24178=VERTEX_POINT('',#82439);
#24179=VERTEX_POINT('',#82443);
#24180=VERTEX_POINT('',#82454);
#24181=VERTEX_POINT('',#82458);
#24182=VERTEX_POINT('',#82464);
#24183=VERTEX_POINT('',#82466);
#24184=VERTEX_POINT('',#82470);
#24185=VERTEX_POINT('',#82472);
#24186=VERTEX_POINT('',#82476);
#24187=VERTEX_POINT('',#82478);
#24188=VERTEX_POINT('',#82482);
#24189=VERTEX_POINT('',#82484);
#24190=VERTEX_POINT('',#82488);
#24191=VERTEX_POINT('',#82490);
#24192=VERTEX_POINT('',#82494);
#24193=VERTEX_POINT('',#82496);
#24194=VERTEX_POINT('',#82505);
#24195=VERTEX_POINT('',#82509);
#24196=VERTEX_POINT('',#82520);
#24197=VERTEX_POINT('',#82524);
#24198=VERTEX_POINT('',#82535);
#24199=VERTEX_POINT('',#82539);
#24200=VERTEX_POINT('',#82550);
#24201=VERTEX_POINT('',#82554);
#24202=VERTEX_POINT('',#82565);
#24203=VERTEX_POINT('',#82569);
#24204=VERTEX_POINT('',#82580);
#24205=VERTEX_POINT('',#82584);
#24206=VERTEX_POINT('',#82595);
#24207=VERTEX_POINT('',#82599);
#24208=VERTEX_POINT('',#82610);
#24209=VERTEX_POINT('',#82614);
#24210=VERTEX_POINT('',#82620);
#24211=VERTEX_POINT('',#82622);
#24212=VERTEX_POINT('',#82631);
#24213=VERTEX_POINT('',#82635);
#24214=VERTEX_POINT('',#82659);
#24215=VERTEX_POINT('',#82660);
#24216=VERTEX_POINT('',#82664);
#24217=VERTEX_POINT('',#82666);
#24218=VERTEX_POINT('',#82677);
#24219=VERTEX_POINT('',#82681);
#24220=VERTEX_POINT('',#82692);
#24221=VERTEX_POINT('',#82696);
#24222=VERTEX_POINT('',#82707);
#24223=VERTEX_POINT('',#82711);
#24224=VERTEX_POINT('',#82722);
#24225=VERTEX_POINT('',#82726);
#24226=VERTEX_POINT('',#82737);
#24227=VERTEX_POINT('',#82741);
#24228=VERTEX_POINT('',#82752);
#24229=VERTEX_POINT('',#82756);
#24230=VERTEX_POINT('',#82767);
#24231=VERTEX_POINT('',#82771);
#24232=VERTEX_POINT('',#82782);
#24233=VERTEX_POINT('',#82786);
#24234=VERTEX_POINT('',#82797);
#24235=VERTEX_POINT('',#82801);
#24236=VERTEX_POINT('',#82825);
#24237=VERTEX_POINT('',#82826);
#24238=VERTEX_POINT('',#82830);
#24239=VERTEX_POINT('',#82832);
#24240=VERTEX_POINT('',#82843);
#24241=VERTEX_POINT('',#82847);
#24242=VERTEX_POINT('',#82858);
#24243=VERTEX_POINT('',#82862);
#24244=VERTEX_POINT('',#82873);
#24245=VERTEX_POINT('',#82877);
#24246=VERTEX_POINT('',#82888);
#24247=VERTEX_POINT('',#82892);
#24248=VERTEX_POINT('',#82903);
#24249=VERTEX_POINT('',#82907);
#24250=VERTEX_POINT('',#82918);
#24251=VERTEX_POINT('',#82922);
#24252=VERTEX_POINT('',#82933);
#24253=VERTEX_POINT('',#82937);
#24254=VERTEX_POINT('',#82948);
#24255=VERTEX_POINT('',#82952);
#24256=VERTEX_POINT('',#82963);
#24257=VERTEX_POINT('',#82967);
#24258=VERTEX_POINT('',#82978);
#24259=VERTEX_POINT('',#82982);
#24260=VERTEX_POINT('',#82988);
#24261=VERTEX_POINT('',#82990);
#24262=VERTEX_POINT('',#82999);
#24263=VERTEX_POINT('',#83003);
#24264=VERTEX_POINT('',#83014);
#24265=VERTEX_POINT('',#83018);
#24266=VERTEX_POINT('',#83037);
#24267=VERTEX_POINT('',#83038);
#24268=VERTEX_POINT('',#83040);
#24269=VERTEX_POINT('',#83042);
#24270=VERTEX_POINT('',#83046);
#24271=VERTEX_POINT('',#83048);
#24272=VERTEX_POINT('',#83052);
#24273=VERTEX_POINT('',#83054);
#24274=VERTEX_POINT('',#83058);
#24275=VERTEX_POINT('',#83060);
#24276=VERTEX_POINT('',#83064);
#24277=VERTEX_POINT('',#83066);
#24278=VERTEX_POINT('',#83070);
#24279=VERTEX_POINT('',#83072);
#24280=VERTEX_POINT('',#83076);
#24281=VERTEX_POINT('',#83078);
#24282=VERTEX_POINT('',#83082);
#24283=VERTEX_POINT('',#83084);
#24284=VERTEX_POINT('',#83088);
#24285=VERTEX_POINT('',#83090);
#24286=VERTEX_POINT('',#83094);
#24287=VERTEX_POINT('',#83096);
#24288=VERTEX_POINT('',#83100);
#24289=VERTEX_POINT('',#83102);
#24290=VERTEX_POINT('',#83110);
#24291=VERTEX_POINT('',#83111);
#24292=VERTEX_POINT('',#83113);
#24293=VERTEX_POINT('',#83115);
#24294=VERTEX_POINT('',#83119);
#24295=VERTEX_POINT('',#83121);
#24296=VERTEX_POINT('',#83125);
#24297=VERTEX_POINT('',#83127);
#24298=VERTEX_POINT('',#83140);
#24299=VERTEX_POINT('',#83141);
#24300=VERTEX_POINT('',#83145);
#24301=VERTEX_POINT('',#83147);
#24302=VERTEX_POINT('',#83158);
#24303=VERTEX_POINT('',#83162);
#24304=VERTEX_POINT('',#83173);
#24305=VERTEX_POINT('',#83177);
#24306=VERTEX_POINT('',#83188);
#24307=VERTEX_POINT('',#83192);
#24308=VERTEX_POINT('',#83203);
#24309=VERTEX_POINT('',#83207);
#24310=VERTEX_POINT('',#83218);
#24311=VERTEX_POINT('',#83222);
#24312=VERTEX_POINT('',#83233);
#24313=VERTEX_POINT('',#83237);
#24314=VERTEX_POINT('',#83248);
#24315=VERTEX_POINT('',#83252);
#24316=VERTEX_POINT('',#83263);
#24317=VERTEX_POINT('',#83267);
#24318=VERTEX_POINT('',#83278);
#24319=VERTEX_POINT('',#83282);
#24320=VERTEX_POINT('',#83301);
#24321=VERTEX_POINT('',#83302);
#24322=VERTEX_POINT('',#83304);
#24323=VERTEX_POINT('',#83306);
#24324=VERTEX_POINT('',#83310);
#24325=VERTEX_POINT('',#83312);
#24326=VERTEX_POINT('',#83316);
#24327=VERTEX_POINT('',#83318);
#24328=VERTEX_POINT('',#83322);
#24329=VERTEX_POINT('',#83324);
#24330=VERTEX_POINT('',#83328);
#24331=VERTEX_POINT('',#83330);
#24332=VERTEX_POINT('',#83334);
#24333=VERTEX_POINT('',#83336);
#24334=VERTEX_POINT('',#83340);
#24335=VERTEX_POINT('',#83342);
#24336=VERTEX_POINT('',#83346);
#24337=VERTEX_POINT('',#83348);
#24338=VERTEX_POINT('',#83352);
#24339=VERTEX_POINT('',#83354);
#24340=VERTEX_POINT('',#83358);
#24341=VERTEX_POINT('',#83360);
#24342=VERTEX_POINT('',#83364);
#24343=VERTEX_POINT('',#83366);
#24344=VERTEX_POINT('',#83374);
#24345=VERTEX_POINT('',#83375);
#24346=VERTEX_POINT('',#83377);
#24347=VERTEX_POINT('',#83379);
#24348=VERTEX_POINT('',#83383);
#24349=VERTEX_POINT('',#83385);
#24350=VERTEX_POINT('',#83389);
#24351=VERTEX_POINT('',#83391);
#24352=VERTEX_POINT('',#83395);
#24353=VERTEX_POINT('',#83397);
#24354=VERTEX_POINT('',#83401);
#24355=VERTEX_POINT('',#83403);
#24356=VERTEX_POINT('',#83416);
#24357=VERTEX_POINT('',#83417);
#24358=VERTEX_POINT('',#83421);
#24359=VERTEX_POINT('',#83423);
#24360=VERTEX_POINT('',#83434);
#24361=VERTEX_POINT('',#83438);
#24362=VERTEX_POINT('',#83449);
#24363=VERTEX_POINT('',#83453);
#24364=VERTEX_POINT('',#83464);
#24365=VERTEX_POINT('',#83468);
#24366=VERTEX_POINT('',#83479);
#24367=VERTEX_POINT('',#83483);
#24368=VERTEX_POINT('',#83494);
#24369=VERTEX_POINT('',#83498);
#24370=VERTEX_POINT('',#83509);
#24371=VERTEX_POINT('',#83513);
#24372=VERTEX_POINT('',#83524);
#24373=VERTEX_POINT('',#83528);
#24374=VERTEX_POINT('',#83534);
#24375=VERTEX_POINT('',#83536);
#24376=VERTEX_POINT('',#83540);
#24377=VERTEX_POINT('',#83542);
#24378=VERTEX_POINT('',#83546);
#24379=VERTEX_POINT('',#83548);
#24380=VERTEX_POINT('',#83565);
#24381=VERTEX_POINT('',#83566);
#24382=VERTEX_POINT('',#83568);
#24383=VERTEX_POINT('',#83570);
#24384=VERTEX_POINT('',#83579);
#24385=VERTEX_POINT('',#83583);
#24386=VERTEX_POINT('',#83594);
#24387=VERTEX_POINT('',#83598);
#24388=VERTEX_POINT('',#83609);
#24389=VERTEX_POINT('',#83613);
#24390=VERTEX_POINT('',#83624);
#24391=VERTEX_POINT('',#83628);
#24392=VERTEX_POINT('',#83634);
#24393=VERTEX_POINT('',#83636);
#24394=VERTEX_POINT('',#83640);
#24395=VERTEX_POINT('',#83642);
#24396=VERTEX_POINT('',#83646);
#24397=VERTEX_POINT('',#83648);
#24398=VERTEX_POINT('',#83657);
#24399=VERTEX_POINT('',#83661);
#24400=VERTEX_POINT('',#83672);
#24401=VERTEX_POINT('',#83676);
#24402=VERTEX_POINT('',#83687);
#24403=VERTEX_POINT('',#83691);
#24404=VERTEX_POINT('',#83702);
#24405=VERTEX_POINT('',#83706);
#24406=VERTEX_POINT('',#83717);
#24407=VERTEX_POINT('',#83721);
#24408=VERTEX_POINT('',#83732);
#24409=VERTEX_POINT('',#83736);
#24410=VERTEX_POINT('',#83747);
#24411=VERTEX_POINT('',#83751);
#24412=VERTEX_POINT('',#83757);
#24413=VERTEX_POINT('',#83759);
#24414=VERTEX_POINT('',#83763);
#24415=VERTEX_POINT('',#83765);
#24416=VERTEX_POINT('',#83769);
#24417=VERTEX_POINT('',#83771);
#24418=VERTEX_POINT('',#83779);
#24419=VERTEX_POINT('',#83780);
#24420=VERTEX_POINT('',#83782);
#24421=VERTEX_POINT('',#83784);
#24422=VERTEX_POINT('',#83788);
#24423=VERTEX_POINT('',#83790);
#24424=VERTEX_POINT('',#83794);
#24425=VERTEX_POINT('',#83796);
#24426=VERTEX_POINT('',#83804);
#24427=VERTEX_POINT('',#83806);
#24428=VERTEX_POINT('',#83810);
#24429=VERTEX_POINT('',#83814);
#24430=VERTEX_POINT('',#83815);
#24431=VERTEX_POINT('',#83817);
#24432=VERTEX_POINT('',#83819);
#24433=VERTEX_POINT('',#83821);
#24434=VERTEX_POINT('',#83823);
#24435=VERTEX_POINT('',#83825);
#24436=VERTEX_POINT('',#83827);
#24437=VERTEX_POINT('',#83830);
#24438=VERTEX_POINT('',#83832);
#24439=VERTEX_POINT('',#83834);
#24440=VERTEX_POINT('',#83836);
#24441=VERTEX_POINT('',#83838);
#24442=VERTEX_POINT('',#83840);
#24443=VERTEX_POINT('',#83842);
#24444=VERTEX_POINT('',#83844);
#24445=VERTEX_POINT('',#83846);
#24446=VERTEX_POINT('',#83848);
#24447=VERTEX_POINT('',#83851);
#24448=VERTEX_POINT('',#83855);
#24449=VERTEX_POINT('',#83856);
#24450=VERTEX_POINT('',#83858);
#24451=VERTEX_POINT('',#83860);
#24452=VERTEX_POINT('',#83862);
#24453=VERTEX_POINT('',#83864);
#24454=VERTEX_POINT('',#83866);
#24455=VERTEX_POINT('',#83868);
#24456=VERTEX_POINT('',#83871);
#24457=VERTEX_POINT('',#83873);
#24458=VERTEX_POINT('',#83875);
#24459=VERTEX_POINT('',#83878);
#24460=VERTEX_POINT('',#83882);
#24461=VERTEX_POINT('',#83888);
#24462=VERTEX_POINT('',#83892);
#24463=VERTEX_POINT('',#83898);
#24464=VERTEX_POINT('',#83902);
#24465=VERTEX_POINT('',#83908);
#24466=VERTEX_POINT('',#83910);
#24467=VERTEX_POINT('',#83915);
#24468=VERTEX_POINT('',#83917);
#24469=VERTEX_POINT('',#83922);
#24470=VERTEX_POINT('',#83924);
#24471=VERTEX_POINT('',#83927);
#24472=VERTEX_POINT('',#83933);
#24473=VERTEX_POINT('',#83935);
#24474=VERTEX_POINT('',#83938);
#24475=VERTEX_POINT('',#83944);
#24476=VERTEX_POINT('',#83946);
#24477=VERTEX_POINT('',#83949);
#24478=VERTEX_POINT('',#83955);
#24479=VERTEX_POINT('',#83957);
#24480=VERTEX_POINT('',#83960);
#24481=VERTEX_POINT('',#83966);
#24482=VERTEX_POINT('',#83971);
#24483=VERTEX_POINT('',#83973);
#24484=VERTEX_POINT('',#83977);
#24485=VERTEX_POINT('',#83981);
#24486=VERTEX_POINT('',#83985);
#24487=VERTEX_POINT('',#83989);
#24488=VERTEX_POINT('',#83993);
#24489=VERTEX_POINT('',#83997);
#24490=VERTEX_POINT('',#84003);
#24491=VERTEX_POINT('',#84005);
#24492=VERTEX_POINT('',#84009);
#24493=VERTEX_POINT('',#84013);
#24494=VERTEX_POINT('',#84017);
#24495=VERTEX_POINT('',#84030);
#24496=VERTEX_POINT('',#84034);
#24497=VERTEX_POINT('',#84038);
#24498=VERTEX_POINT('',#84052);
#24499=VERTEX_POINT('',#84054);
#24500=VERTEX_POINT('',#84058);
#24501=VERTEX_POINT('',#84062);
#24502=VERTEX_POINT('',#84065);
#24503=VERTEX_POINT('',#84069);
#24504=VERTEX_POINT('',#84073);
#24505=VERTEX_POINT('',#84077);
#24506=VERTEX_POINT('',#84083);
#24507=VERTEX_POINT('',#84084);
#24508=VERTEX_POINT('',#84086);
#24509=VERTEX_POINT('',#84097);
#24510=VERTEX_POINT('',#84110);
#24511=VERTEX_POINT('',#84111);
#24512=VERTEX_POINT('',#84158);
#24513=VERTEX_POINT('',#84159);
#24514=VERTEX_POINT('',#84206);
#24515=VERTEX_POINT('',#84207);
#24516=VERTEX_POINT('',#84260);
#24517=VERTEX_POINT('',#84261);
#24518=VERTEX_POINT('',#84308);
#24519=VERTEX_POINT('',#84309);
#24520=VERTEX_POINT('',#84356);
#24521=VERTEX_POINT('',#84357);
#24522=VERTEX_POINT('',#84410);
#24523=VERTEX_POINT('',#84411);
#24524=VERTEX_POINT('',#84458);
#24525=VERTEX_POINT('',#84459);
#24526=VERTEX_POINT('',#84506);
#24527=VERTEX_POINT('',#84507);
#24528=VERTEX_POINT('',#84560);
#24529=VERTEX_POINT('',#84561);
#24530=VERTEX_POINT('',#84608);
#24531=VERTEX_POINT('',#84609);
#24532=VERTEX_POINT('',#84656);
#24533=VERTEX_POINT('',#84657);
#24534=VERTEX_POINT('',#84710);
#24535=VERTEX_POINT('',#84711);
#24536=VERTEX_POINT('',#84758);
#24537=VERTEX_POINT('',#84759);
#24538=VERTEX_POINT('',#84806);
#24539=VERTEX_POINT('',#84807);
#24540=VERTEX_POINT('',#84860);
#24541=VERTEX_POINT('',#84861);
#24542=VERTEX_POINT('',#84863);
#24543=VERTEX_POINT('',#84870);
#24544=VERTEX_POINT('',#84871);
#24545=VERTEX_POINT('',#84884);
#24546=VERTEX_POINT('',#84897);
#24547=VERTEX_POINT('',#84898);
#24548=VERTEX_POINT('',#84922);
#24549=VERTEX_POINT('',#84923);
#24550=VERTEX_POINT('',#84946);
#24551=VERTEX_POINT('',#84947);
#24552=VERTEX_POINT('',#84971);
#24553=VERTEX_POINT('',#84972);
#24554=VERTEX_POINT('',#84996);
#24555=VERTEX_POINT('',#84997);
#24556=VERTEX_POINT('',#85020);
#24557=VERTEX_POINT('',#85021);
#24558=VERTEX_POINT('',#85045);
#24559=VERTEX_POINT('',#85046);
#24560=VERTEX_POINT('',#85070);
#24561=VERTEX_POINT('',#85071);
#24562=VERTEX_POINT('',#85094);
#24563=VERTEX_POINT('',#85095);
#24564=VERTEX_POINT('',#85119);
#24565=VERTEX_POINT('',#85120);
#24566=VERTEX_POINT('',#85144);
#24567=VERTEX_POINT('',#85145);
#24568=VERTEX_POINT('',#85168);
#24569=VERTEX_POINT('',#85169);
#24570=VERTEX_POINT('',#85193);
#24571=VERTEX_POINT('',#85194);
#24572=VERTEX_POINT('',#85218);
#24573=VERTEX_POINT('',#85219);
#24574=VERTEX_POINT('',#85242);
#24575=VERTEX_POINT('',#85349);
#24576=VERTEX_POINT('',#85351);
#24577=VERTEX_POINT('',#85900);
#24578=VERTEX_POINT('',#86017);
#24579=VERTEX_POINT('',#86020);
#24580=VERTEX_POINT('',#86580);
#24581=VERTEX_POINT('',#86586);
#24582=VERTEX_POINT('',#86589);
#24583=VERTEX_POINT('',#86590);
#24584=VERTEX_POINT('',#86592);
#24585=VERTEX_POINT('',#86594);
#24586=VERTEX_POINT('',#86598);
#24587=VERTEX_POINT('',#86602);
#24588=VERTEX_POINT('',#86608);
#24589=VERTEX_POINT('',#86609);
#24590=VERTEX_POINT('',#86611);
#24591=VERTEX_POINT('',#86613);
#24592=VERTEX_POINT('',#86617);
#24593=VERTEX_POINT('',#86621);
#24594=VERTEX_POINT('',#86627);
#24595=VERTEX_POINT('',#86628);
#24596=VERTEX_POINT('',#86630);
#24597=VERTEX_POINT('',#86632);
#24598=VERTEX_POINT('',#86636);
#24599=VERTEX_POINT('',#86640);
#24600=VERTEX_POINT('',#86646);
#24601=VERTEX_POINT('',#86647);
#24602=VERTEX_POINT('',#86649);
#24603=VERTEX_POINT('',#86651);
#24604=VERTEX_POINT('',#86655);
#24605=VERTEX_POINT('',#86659);
#24606=VERTEX_POINT('',#86665);
#24607=VERTEX_POINT('',#86666);
#24608=VERTEX_POINT('',#86668);
#24609=VERTEX_POINT('',#86670);
#24610=VERTEX_POINT('',#86674);
#24611=VERTEX_POINT('',#86678);
#24612=VERTEX_POINT('',#86684);
#24613=VERTEX_POINT('',#86685);
#24614=VERTEX_POINT('',#86687);
#24615=VERTEX_POINT('',#86689);
#24616=VERTEX_POINT('',#86693);
#24617=VERTEX_POINT('',#86697);
#24618=VERTEX_POINT('',#86703);
#24619=VERTEX_POINT('',#86704);
#24620=VERTEX_POINT('',#86706);
#24621=VERTEX_POINT('',#86708);
#24622=VERTEX_POINT('',#86712);
#24623=VERTEX_POINT('',#86716);
#24624=VERTEX_POINT('',#86722);
#24625=VERTEX_POINT('',#86723);
#24626=VERTEX_POINT('',#86725);
#24627=VERTEX_POINT('',#86727);
#24628=VERTEX_POINT('',#86731);
#24629=VERTEX_POINT('',#86735);
#24630=VERTEX_POINT('',#86741);
#24631=VERTEX_POINT('',#86742);
#24632=VERTEX_POINT('',#86744);
#24633=VERTEX_POINT('',#86746);
#24634=VERTEX_POINT('',#86750);
#24635=VERTEX_POINT('',#86754);
#24636=VERTEX_POINT('',#86760);
#24637=VERTEX_POINT('',#86761);
#24638=VERTEX_POINT('',#86763);
#24639=VERTEX_POINT('',#86765);
#24640=VERTEX_POINT('',#86769);
#24641=VERTEX_POINT('',#86773);
#24642=VERTEX_POINT('',#86779);
#24643=VERTEX_POINT('',#86780);
#24644=VERTEX_POINT('',#86782);
#24645=VERTEX_POINT('',#86784);
#24646=VERTEX_POINT('',#86788);
#24647=VERTEX_POINT('',#86792);
#24648=VERTEX_POINT('',#86798);
#24649=VERTEX_POINT('',#86799);
#24650=VERTEX_POINT('',#86801);
#24651=VERTEX_POINT('',#86803);
#24652=VERTEX_POINT('',#86807);
#24653=VERTEX_POINT('',#86811);
#24654=VERTEX_POINT('',#86817);
#24655=VERTEX_POINT('',#86818);
#24656=VERTEX_POINT('',#86820);
#24657=VERTEX_POINT('',#86822);
#24658=VERTEX_POINT('',#86826);
#24659=VERTEX_POINT('',#86830);
#24660=VERTEX_POINT('',#86836);
#24661=VERTEX_POINT('',#86837);
#24662=VERTEX_POINT('',#86839);
#24663=VERTEX_POINT('',#86841);
#24664=VERTEX_POINT('',#86845);
#24665=VERTEX_POINT('',#86849);
#24666=VERTEX_POINT('',#86855);
#24667=VERTEX_POINT('',#86856);
#24668=VERTEX_POINT('',#86858);
#24669=VERTEX_POINT('',#86860);
#24670=VERTEX_POINT('',#86864);
#24671=VERTEX_POINT('',#86868);
#24672=VERTEX_POINT('',#86874);
#24673=VERTEX_POINT('',#86875);
#24674=VERTEX_POINT('',#86877);
#24675=VERTEX_POINT('',#86879);
#24676=VERTEX_POINT('',#86883);
#24677=VERTEX_POINT('',#86887);
#24678=VERTEX_POINT('',#86893);
#24679=VERTEX_POINT('',#86894);
#24680=VERTEX_POINT('',#86896);
#24681=VERTEX_POINT('',#86898);
#24682=VERTEX_POINT('',#86902);
#24683=VERTEX_POINT('',#86906);
#24684=VERTEX_POINT('',#86912);
#24685=VERTEX_POINT('',#86913);
#24686=VERTEX_POINT('',#86915);
#24687=VERTEX_POINT('',#86917);
#24688=VERTEX_POINT('',#86921);
#24689=VERTEX_POINT('',#86923);
#24690=VERTEX_POINT('',#86927);
#24691=VERTEX_POINT('',#86931);
#24692=VERTEX_POINT('',#86935);
#24693=VERTEX_POINT('',#86936);
#24694=VERTEX_POINT('',#86938);
#24695=VERTEX_POINT('',#86940);
#24696=VERTEX_POINT('',#86944);
#24697=VERTEX_POINT('',#86948);
#24698=VERTEX_POINT('',#86954);
#24699=VERTEX_POINT('',#86955);
#24700=VERTEX_POINT('',#86957);
#24701=VERTEX_POINT('',#86959);
#24702=VERTEX_POINT('',#86963);
#24703=VERTEX_POINT('',#86967);
#24704=VERTEX_POINT('',#86973);
#24705=VERTEX_POINT('',#86974);
#24706=VERTEX_POINT('',#86976);
#24707=VERTEX_POINT('',#86978);
#24708=VERTEX_POINT('',#86982);
#24709=VERTEX_POINT('',#86986);
#24710=VERTEX_POINT('',#86992);
#24711=VERTEX_POINT('',#86993);
#24712=VERTEX_POINT('',#86995);
#24713=VERTEX_POINT('',#86997);
#24714=VERTEX_POINT('',#87001);
#24715=VERTEX_POINT('',#87005);
#24716=VERTEX_POINT('',#87011);
#24717=VERTEX_POINT('',#87012);
#24718=VERTEX_POINT('',#87014);
#24719=VERTEX_POINT('',#87016);
#24720=VERTEX_POINT('',#87020);
#24721=VERTEX_POINT('',#87024);
#24722=VERTEX_POINT('',#87030);
#24723=VERTEX_POINT('',#87031);
#24724=VERTEX_POINT('',#87033);
#24725=VERTEX_POINT('',#87035);
#24726=VERTEX_POINT('',#87039);
#24727=VERTEX_POINT('',#87043);
#24728=VERTEX_POINT('',#87049);
#24729=VERTEX_POINT('',#87050);
#24730=VERTEX_POINT('',#87052);
#24731=VERTEX_POINT('',#87054);
#24732=VERTEX_POINT('',#87058);
#24733=VERTEX_POINT('',#87062);
#24734=VERTEX_POINT('',#87068);
#24735=VERTEX_POINT('',#87069);
#24736=VERTEX_POINT('',#87071);
#24737=VERTEX_POINT('',#87073);
#24738=VERTEX_POINT('',#87077);
#24739=VERTEX_POINT('',#87081);
#24740=VERTEX_POINT('',#87087);
#24741=VERTEX_POINT('',#87088);
#24742=VERTEX_POINT('',#87090);
#24743=VERTEX_POINT('',#87092);
#24744=VERTEX_POINT('',#87096);
#24745=VERTEX_POINT('',#87100);
#24746=VERTEX_POINT('',#87106);
#24747=VERTEX_POINT('',#87107);
#24748=VERTEX_POINT('',#87109);
#24749=VERTEX_POINT('',#87111);
#24750=VERTEX_POINT('',#87115);
#24751=VERTEX_POINT('',#87119);
#24752=VERTEX_POINT('',#87125);
#24753=VERTEX_POINT('',#87126);
#24754=VERTEX_POINT('',#87128);
#24755=VERTEX_POINT('',#87130);
#24756=VERTEX_POINT('',#87134);
#24757=VERTEX_POINT('',#87138);
#24758=VERTEX_POINT('',#87144);
#24759=VERTEX_POINT('',#87145);
#24760=VERTEX_POINT('',#87147);
#24761=VERTEX_POINT('',#87149);
#24762=VERTEX_POINT('',#87153);
#24763=VERTEX_POINT('',#87157);
#24764=VERTEX_POINT('',#87163);
#24765=VERTEX_POINT('',#87164);
#24766=VERTEX_POINT('',#87166);
#24767=VERTEX_POINT('',#87168);
#24768=VERTEX_POINT('',#87172);
#24769=VERTEX_POINT('',#87176);
#24770=VERTEX_POINT('',#87182);
#24771=VERTEX_POINT('',#87183);
#24772=VERTEX_POINT('',#87185);
#24773=VERTEX_POINT('',#87187);
#24774=VERTEX_POINT('',#87191);
#24775=VERTEX_POINT('',#87195);
#24776=VERTEX_POINT('',#87201);
#24777=VERTEX_POINT('',#87202);
#24778=VERTEX_POINT('',#87204);
#24779=VERTEX_POINT('',#87206);
#24780=VERTEX_POINT('',#87210);
#24781=VERTEX_POINT('',#87214);
#24782=VERTEX_POINT('',#87220);
#24783=VERTEX_POINT('',#87221);
#24784=VERTEX_POINT('',#87223);
#24785=VERTEX_POINT('',#87225);
#24786=VERTEX_POINT('',#87229);
#24787=VERTEX_POINT('',#87233);
#24788=VERTEX_POINT('',#87239);
#24789=VERTEX_POINT('',#87240);
#24790=VERTEX_POINT('',#87242);
#24791=VERTEX_POINT('',#87244);
#24792=VERTEX_POINT('',#87248);
#24793=VERTEX_POINT('',#87252);
#24794=VERTEX_POINT('',#87258);
#24795=VERTEX_POINT('',#87259);
#24796=VERTEX_POINT('',#87261);
#24797=VERTEX_POINT('',#87265);
#24798=VERTEX_POINT('',#87267);
#24799=VERTEX_POINT('',#87271);
#24800=VERTEX_POINT('',#87277);
#24801=VERTEX_POINT('',#87278);
#24802=VERTEX_POINT('',#87282);
#24803=VERTEX_POINT('',#87283);
#24804=VERTEX_POINT('',#87285);
#24805=VERTEX_POINT('',#87287);
#24806=VERTEX_POINT('',#87291);
#24807=VERTEX_POINT('',#87293);
#24808=VERTEX_POINT('',#87297);
#24809=VERTEX_POINT('',#87299);
#24810=VERTEX_POINT('',#87303);
#24811=VERTEX_POINT('',#87305);
#24812=VERTEX_POINT('',#87309);
#24813=VERTEX_POINT('',#87311);
#24814=VERTEX_POINT('',#87319);
#24815=VERTEX_POINT('',#87362);
#24816=VERTEX_POINT('',#87368);
#24817=VERTEX_POINT('',#87370);
#24818=VERTEX_POINT('',#87374);
#24819=VERTEX_POINT('',#87378);
#24820=VERTEX_POINT('',#87382);
#24821=VERTEX_POINT('',#87385);
#24822=VERTEX_POINT('',#87389);
#24823=VERTEX_POINT('',#87393);
#24824=VERTEX_POINT('',#87399);
#24825=VERTEX_POINT('',#87400);
#24826=VERTEX_POINT('',#87402);
#24827=VERTEX_POINT('',#87404);
#24828=VERTEX_POINT('',#87408);
#24829=VERTEX_POINT('',#87409);
#24830=VERTEX_POINT('',#87411);
#24831=VERTEX_POINT('',#87413);
#24832=VERTEX_POINT('',#87417);
#24833=VERTEX_POINT('',#87421);
#24834=VERTEX_POINT('',#87423);
#24835=VERTEX_POINT('',#87427);
#24836=VERTEX_POINT('',#87429);
#24837=VERTEX_POINT('',#87433);
#24838=VERTEX_POINT('',#87439);
#24839=VERTEX_POINT('',#87440);
#24840=VERTEX_POINT('',#87444);
#24841=VERTEX_POINT('',#87446);
#24842=VERTEX_POINT('',#87450);
#24843=VERTEX_POINT('',#87455);
#24844=VERTEX_POINT('',#87478);
#24845=VERTEX_POINT('',#87479);
#24846=VERTEX_POINT('',#87481);
#24847=VERTEX_POINT('',#87492);
#24848=VERTEX_POINT('',#87502);
#24849=VERTEX_POINT('',#87503);
#24850=VERTEX_POINT('',#87550);
#24851=VERTEX_POINT('',#87551);
#24852=VERTEX_POINT('',#87598);
#24853=VERTEX_POINT('',#87599);
#24854=VERTEX_POINT('',#87652);
#24855=VERTEX_POINT('',#87653);
#24856=VERTEX_POINT('',#87700);
#24857=VERTEX_POINT('',#87701);
#24858=VERTEX_POINT('',#87748);
#24859=VERTEX_POINT('',#87749);
#24860=VERTEX_POINT('',#87796);
#24861=VERTEX_POINT('',#87797);
#24862=VERTEX_POINT('',#87850);
#24863=VERTEX_POINT('',#87851);
#24864=VERTEX_POINT('',#87898);
#24865=VERTEX_POINT('',#87899);
#24866=VERTEX_POINT('',#87946);
#24867=VERTEX_POINT('',#87947);
#24868=VERTEX_POINT('',#88000);
#24869=VERTEX_POINT('',#88001);
#24870=VERTEX_POINT('',#88048);
#24871=VERTEX_POINT('',#88049);
#24872=VERTEX_POINT('',#88096);
#24873=VERTEX_POINT('',#88097);
#24874=VERTEX_POINT('',#88150);
#24875=VERTEX_POINT('',#88151);
#24876=VERTEX_POINT('',#88198);
#24877=VERTEX_POINT('',#88199);
#24878=VERTEX_POINT('',#88201);
#24879=VERTEX_POINT('',#88245);
#24880=VERTEX_POINT('',#88246);
#24881=VERTEX_POINT('',#88248);
#24882=VERTEX_POINT('',#88256);
#24883=VERTEX_POINT('',#88265);
#24884=VERTEX_POINT('',#88266);
#24885=VERTEX_POINT('',#88289);
#24886=VERTEX_POINT('',#88290);
#24887=VERTEX_POINT('',#88314);
#24888=VERTEX_POINT('',#88315);
#24889=VERTEX_POINT('',#88339);
#24890=VERTEX_POINT('',#88340);
#24891=VERTEX_POINT('',#88363);
#24892=VERTEX_POINT('',#88364);
#24893=VERTEX_POINT('',#88388);
#24894=VERTEX_POINT('',#88389);
#24895=VERTEX_POINT('',#88413);
#24896=VERTEX_POINT('',#88414);
#24897=VERTEX_POINT('',#88437);
#24898=VERTEX_POINT('',#88438);
#24899=VERTEX_POINT('',#88462);
#24900=VERTEX_POINT('',#88463);
#24901=VERTEX_POINT('',#88487);
#24902=VERTEX_POINT('',#88488);
#24903=VERTEX_POINT('',#88511);
#24904=VERTEX_POINT('',#88512);
#24905=VERTEX_POINT('',#88535);
#24906=VERTEX_POINT('',#88536);
#24907=VERTEX_POINT('',#88560);
#24908=VERTEX_POINT('',#88561);
#24909=VERTEX_POINT('',#88585);
#24910=VERTEX_POINT('',#88586);
#24911=VERTEX_POINT('',#88700);
#24912=VERTEX_POINT('',#88702);
#24913=VERTEX_POINT('',#89206);
#24914=VERTEX_POINT('',#89308);
#24915=VERTEX_POINT('',#89311);
#24916=VERTEX_POINT('',#89822);
#24917=VERTEX_POINT('',#89827);
#24918=VERTEX_POINT('',#89830);
#24919=VERTEX_POINT('',#89831);
#24920=VERTEX_POINT('',#89833);
#24921=VERTEX_POINT('',#89835);
#24922=VERTEX_POINT('',#89839);
#24923=VERTEX_POINT('',#89843);
#24924=VERTEX_POINT('',#89849);
#24925=VERTEX_POINT('',#89850);
#24926=VERTEX_POINT('',#89852);
#24927=VERTEX_POINT('',#89854);
#24928=VERTEX_POINT('',#89858);
#24929=VERTEX_POINT('',#89862);
#24930=VERTEX_POINT('',#89868);
#24931=VERTEX_POINT('',#89869);
#24932=VERTEX_POINT('',#89871);
#24933=VERTEX_POINT('',#89873);
#24934=VERTEX_POINT('',#89877);
#24935=VERTEX_POINT('',#89881);
#24936=VERTEX_POINT('',#89887);
#24937=VERTEX_POINT('',#89888);
#24938=VERTEX_POINT('',#89890);
#24939=VERTEX_POINT('',#89892);
#24940=VERTEX_POINT('',#89896);
#24941=VERTEX_POINT('',#89900);
#24942=VERTEX_POINT('',#89906);
#24943=VERTEX_POINT('',#89907);
#24944=VERTEX_POINT('',#89909);
#24945=VERTEX_POINT('',#89911);
#24946=VERTEX_POINT('',#89915);
#24947=VERTEX_POINT('',#89919);
#24948=VERTEX_POINT('',#89925);
#24949=VERTEX_POINT('',#89926);
#24950=VERTEX_POINT('',#89928);
#24951=VERTEX_POINT('',#89930);
#24952=VERTEX_POINT('',#89934);
#24953=VERTEX_POINT('',#89938);
#24954=VERTEX_POINT('',#89944);
#24955=VERTEX_POINT('',#89945);
#24956=VERTEX_POINT('',#89947);
#24957=VERTEX_POINT('',#89949);
#24958=VERTEX_POINT('',#89953);
#24959=VERTEX_POINT('',#89957);
#24960=VERTEX_POINT('',#89963);
#24961=VERTEX_POINT('',#89964);
#24962=VERTEX_POINT('',#89966);
#24963=VERTEX_POINT('',#89968);
#24964=VERTEX_POINT('',#89972);
#24965=VERTEX_POINT('',#89976);
#24966=VERTEX_POINT('',#89982);
#24967=VERTEX_POINT('',#89983);
#24968=VERTEX_POINT('',#89985);
#24969=VERTEX_POINT('',#89987);
#24970=VERTEX_POINT('',#89991);
#24971=VERTEX_POINT('',#89995);
#24972=VERTEX_POINT('',#90001);
#24973=VERTEX_POINT('',#90002);
#24974=VERTEX_POINT('',#90004);
#24975=VERTEX_POINT('',#90006);
#24976=VERTEX_POINT('',#90010);
#24977=VERTEX_POINT('',#90014);
#24978=VERTEX_POINT('',#90020);
#24979=VERTEX_POINT('',#90021);
#24980=VERTEX_POINT('',#90023);
#24981=VERTEX_POINT('',#90025);
#24982=VERTEX_POINT('',#90029);
#24983=VERTEX_POINT('',#90033);
#24984=VERTEX_POINT('',#90039);
#24985=VERTEX_POINT('',#90040);
#24986=VERTEX_POINT('',#90042);
#24987=VERTEX_POINT('',#90044);
#24988=VERTEX_POINT('',#90048);
#24989=VERTEX_POINT('',#90052);
#24990=VERTEX_POINT('',#90058);
#24991=VERTEX_POINT('',#90059);
#24992=VERTEX_POINT('',#90061);
#24993=VERTEX_POINT('',#90063);
#24994=VERTEX_POINT('',#90067);
#24995=VERTEX_POINT('',#90071);
#24996=VERTEX_POINT('',#90077);
#24997=VERTEX_POINT('',#90078);
#24998=VERTEX_POINT('',#90080);
#24999=VERTEX_POINT('',#90082);
#25000=VERTEX_POINT('',#90086);
#25001=VERTEX_POINT('',#90090);
#25002=VERTEX_POINT('',#90096);
#25003=VERTEX_POINT('',#90097);
#25004=VERTEX_POINT('',#90099);
#25005=VERTEX_POINT('',#90101);
#25006=VERTEX_POINT('',#90105);
#25007=VERTEX_POINT('',#90109);
#25008=VERTEX_POINT('',#90115);
#25009=VERTEX_POINT('',#90116);
#25010=VERTEX_POINT('',#90118);
#25011=VERTEX_POINT('',#90120);
#25012=VERTEX_POINT('',#90124);
#25013=VERTEX_POINT('',#90128);
#25014=VERTEX_POINT('',#90134);
#25015=VERTEX_POINT('',#90135);
#25016=VERTEX_POINT('',#90137);
#25017=VERTEX_POINT('',#90139);
#25018=VERTEX_POINT('',#90143);
#25019=VERTEX_POINT('',#90147);
#25020=VERTEX_POINT('',#90153);
#25021=VERTEX_POINT('',#90154);
#25022=VERTEX_POINT('',#90156);
#25023=VERTEX_POINT('',#90158);
#25024=VERTEX_POINT('',#90162);
#25025=VERTEX_POINT('',#90164);
#25026=VERTEX_POINT('',#90168);
#25027=VERTEX_POINT('',#90172);
#25028=VERTEX_POINT('',#90176);
#25029=VERTEX_POINT('',#90177);
#25030=VERTEX_POINT('',#90179);
#25031=VERTEX_POINT('',#90181);
#25032=VERTEX_POINT('',#90185);
#25033=VERTEX_POINT('',#90189);
#25034=VERTEX_POINT('',#90195);
#25035=VERTEX_POINT('',#90196);
#25036=VERTEX_POINT('',#90198);
#25037=VERTEX_POINT('',#90200);
#25038=VERTEX_POINT('',#90204);
#25039=VERTEX_POINT('',#90208);
#25040=VERTEX_POINT('',#90214);
#25041=VERTEX_POINT('',#90215);
#25042=VERTEX_POINT('',#90217);
#25043=VERTEX_POINT('',#90219);
#25044=VERTEX_POINT('',#90223);
#25045=VERTEX_POINT('',#90227);
#25046=VERTEX_POINT('',#90233);
#25047=VERTEX_POINT('',#90234);
#25048=VERTEX_POINT('',#90236);
#25049=VERTEX_POINT('',#90238);
#25050=VERTEX_POINT('',#90242);
#25051=VERTEX_POINT('',#90246);
#25052=VERTEX_POINT('',#90252);
#25053=VERTEX_POINT('',#90253);
#25054=VERTEX_POINT('',#90255);
#25055=VERTEX_POINT('',#90257);
#25056=VERTEX_POINT('',#90261);
#25057=VERTEX_POINT('',#90265);
#25058=VERTEX_POINT('',#90271);
#25059=VERTEX_POINT('',#90272);
#25060=VERTEX_POINT('',#90274);
#25061=VERTEX_POINT('',#90276);
#25062=VERTEX_POINT('',#90280);
#25063=VERTEX_POINT('',#90284);
#25064=VERTEX_POINT('',#90290);
#25065=VERTEX_POINT('',#90291);
#25066=VERTEX_POINT('',#90293);
#25067=VERTEX_POINT('',#90295);
#25068=VERTEX_POINT('',#90299);
#25069=VERTEX_POINT('',#90303);
#25070=VERTEX_POINT('',#90309);
#25071=VERTEX_POINT('',#90310);
#25072=VERTEX_POINT('',#90312);
#25073=VERTEX_POINT('',#90314);
#25074=VERTEX_POINT('',#90318);
#25075=VERTEX_POINT('',#90322);
#25076=VERTEX_POINT('',#90328);
#25077=VERTEX_POINT('',#90329);
#25078=VERTEX_POINT('',#90331);
#25079=VERTEX_POINT('',#90333);
#25080=VERTEX_POINT('',#90337);
#25081=VERTEX_POINT('',#90341);
#25082=VERTEX_POINT('',#90347);
#25083=VERTEX_POINT('',#90348);
#25084=VERTEX_POINT('',#90350);
#25085=VERTEX_POINT('',#90352);
#25086=VERTEX_POINT('',#90356);
#25087=VERTEX_POINT('',#90360);
#25088=VERTEX_POINT('',#90366);
#25089=VERTEX_POINT('',#90367);
#25090=VERTEX_POINT('',#90369);
#25091=VERTEX_POINT('',#90371);
#25092=VERTEX_POINT('',#90375);
#25093=VERTEX_POINT('',#90379);
#25094=VERTEX_POINT('',#90385);
#25095=VERTEX_POINT('',#90386);
#25096=VERTEX_POINT('',#90388);
#25097=VERTEX_POINT('',#90390);
#25098=VERTEX_POINT('',#90394);
#25099=VERTEX_POINT('',#90398);
#25100=VERTEX_POINT('',#90404);
#25101=VERTEX_POINT('',#90405);
#25102=VERTEX_POINT('',#90407);
#25103=VERTEX_POINT('',#90409);
#25104=VERTEX_POINT('',#90413);
#25105=VERTEX_POINT('',#90417);
#25106=VERTEX_POINT('',#90423);
#25107=VERTEX_POINT('',#90424);
#25108=VERTEX_POINT('',#90426);
#25109=VERTEX_POINT('',#90428);
#25110=VERTEX_POINT('',#90432);
#25111=VERTEX_POINT('',#90436);
#25112=VERTEX_POINT('',#90442);
#25113=VERTEX_POINT('',#90443);
#25114=VERTEX_POINT('',#90445);
#25115=VERTEX_POINT('',#90447);
#25116=VERTEX_POINT('',#90451);
#25117=VERTEX_POINT('',#90455);
#25118=VERTEX_POINT('',#90461);
#25119=VERTEX_POINT('',#90462);
#25120=VERTEX_POINT('',#90464);
#25121=VERTEX_POINT('',#90466);
#25122=VERTEX_POINT('',#90470);
#25123=VERTEX_POINT('',#90474);
#25124=VERTEX_POINT('',#90480);
#25125=VERTEX_POINT('',#90481);
#25126=VERTEX_POINT('',#90483);
#25127=VERTEX_POINT('',#90485);
#25128=VERTEX_POINT('',#90489);
#25129=VERTEX_POINT('',#90493);
#25130=VERTEX_POINT('',#90499);
#25131=VERTEX_POINT('',#90500);
#25132=VERTEX_POINT('',#90502);
#25133=VERTEX_POINT('',#90506);
#25134=VERTEX_POINT('',#90508);
#25135=VERTEX_POINT('',#90512);
#25136=VERTEX_POINT('',#90518);
#25137=VERTEX_POINT('',#90519);
#25138=VERTEX_POINT('',#90523);
#25139=VERTEX_POINT('',#90524);
#25140=VERTEX_POINT('',#90526);
#25141=VERTEX_POINT('',#90528);
#25142=VERTEX_POINT('',#90532);
#25143=VERTEX_POINT('',#90534);
#25144=VERTEX_POINT('',#90538);
#25145=VERTEX_POINT('',#90540);
#25146=VERTEX_POINT('',#90544);
#25147=VERTEX_POINT('',#90546);
#25148=VERTEX_POINT('',#90550);
#25149=VERTEX_POINT('',#90552);
#25150=VERTEX_POINT('',#90560);
#25151=VERTEX_POINT('',#90603);
#25152=VERTEX_POINT('',#90609);
#25153=VERTEX_POINT('',#90611);
#25154=VERTEX_POINT('',#90613);
#25155=VERTEX_POINT('',#90617);
#25156=VERTEX_POINT('',#90622);
#25157=VERTEX_POINT('',#90625);
#25158=VERTEX_POINT('',#90632);
#25159=VERTEX_POINT('',#90633);
#25160=VERTEX_POINT('',#90635);
#25161=VERTEX_POINT('',#90646);
#25162=VERTEX_POINT('',#90656);
#25163=VERTEX_POINT('',#90657);
#25164=VERTEX_POINT('',#90704);
#25165=VERTEX_POINT('',#90705);
#25166=VERTEX_POINT('',#90752);
#25167=VERTEX_POINT('',#90753);
#25168=VERTEX_POINT('',#90806);
#25169=VERTEX_POINT('',#90807);
#25170=VERTEX_POINT('',#90854);
#25171=VERTEX_POINT('',#90855);
#25172=VERTEX_POINT('',#90902);
#25173=VERTEX_POINT('',#90903);
#25174=VERTEX_POINT('',#90956);
#25175=VERTEX_POINT('',#90957);
#25176=VERTEX_POINT('',#91004);
#25177=VERTEX_POINT('',#91005);
#25178=VERTEX_POINT('',#91052);
#25179=VERTEX_POINT('',#91053);
#25180=VERTEX_POINT('',#91100);
#25181=VERTEX_POINT('',#91101);
#25182=VERTEX_POINT('',#91154);
#25183=VERTEX_POINT('',#91155);
#25184=VERTEX_POINT('',#91202);
#25185=VERTEX_POINT('',#91203);
#25186=VERTEX_POINT('',#91250);
#25187=VERTEX_POINT('',#91251);
#25188=VERTEX_POINT('',#91304);
#25189=VERTEX_POINT('',#91305);
#25190=VERTEX_POINT('',#91352);
#25191=VERTEX_POINT('',#91353);
#25192=VERTEX_POINT('',#91400);
#25193=VERTEX_POINT('',#91401);
#25194=VERTEX_POINT('',#91454);
#25195=VERTEX_POINT('',#91455);
#25196=VERTEX_POINT('',#91502);
#25197=VERTEX_POINT('',#91503);
#25198=VERTEX_POINT('',#91550);
#25199=VERTEX_POINT('',#91551);
#25200=VERTEX_POINT('',#91604);
#25201=VERTEX_POINT('',#91605);
#25202=VERTEX_POINT('',#91652);
#25203=VERTEX_POINT('',#91653);
#25204=VERTEX_POINT('',#91700);
#25205=VERTEX_POINT('',#91701);
#25206=VERTEX_POINT('',#91754);
#25207=VERTEX_POINT('',#91755);
#25208=VERTEX_POINT('',#91757);
#25209=VERTEX_POINT('',#91764);
#25210=VERTEX_POINT('',#91772);
#25211=VERTEX_POINT('',#91773);
#25212=VERTEX_POINT('',#91797);
#25213=VERTEX_POINT('',#91798);
#25214=VERTEX_POINT('',#91822);
#25215=VERTEX_POINT('',#91823);
#25216=VERTEX_POINT('',#91846);
#25217=VERTEX_POINT('',#91847);
#25218=VERTEX_POINT('',#91871);
#25219=VERTEX_POINT('',#91872);
#25220=VERTEX_POINT('',#91896);
#25221=VERTEX_POINT('',#91897);
#25222=VERTEX_POINT('',#91920);
#25223=VERTEX_POINT('',#91921);
#25224=VERTEX_POINT('',#91945);
#25225=VERTEX_POINT('',#91946);
#25226=VERTEX_POINT('',#91970);
#25227=VERTEX_POINT('',#91971);
#25228=VERTEX_POINT('',#91994);
#25229=VERTEX_POINT('',#91995);
#25230=VERTEX_POINT('',#92019);
#25231=VERTEX_POINT('',#92020);
#25232=VERTEX_POINT('',#92044);
#25233=VERTEX_POINT('',#92045);
#25234=VERTEX_POINT('',#92068);
#25235=VERTEX_POINT('',#92069);
#25236=VERTEX_POINT('',#92093);
#25237=VERTEX_POINT('',#92094);
#25238=VERTEX_POINT('',#92118);
#25239=VERTEX_POINT('',#92119);
#25240=VERTEX_POINT('',#92142);
#25241=VERTEX_POINT('',#92143);
#25242=VERTEX_POINT('',#92166);
#25243=VERTEX_POINT('',#92167);
#25244=VERTEX_POINT('',#92191);
#25245=VERTEX_POINT('',#92192);
#25246=VERTEX_POINT('',#92216);
#25247=VERTEX_POINT('',#92217);
#25248=VERTEX_POINT('',#92240);
#25249=VERTEX_POINT('',#92241);
#25250=VERTEX_POINT('',#92265);
#25251=VERTEX_POINT('',#92266);
#25252=VERTEX_POINT('',#92290);
#25253=VERTEX_POINT('',#92291);
#25254=VERTEX_POINT('',#92314);
#25255=VERTEX_POINT('',#92412);
#25256=VERTEX_POINT('',#92414);
#25257=VERTEX_POINT('',#93136);
#25258=VERTEX_POINT('',#93244);
#25259=VERTEX_POINT('',#93247);
#25260=VERTEX_POINT('',#93976);
#25261=VERTEX_POINT('',#93982);
#25262=VERTEX_POINT('',#93985);
#25263=VERTEX_POINT('',#93986);
#25264=VERTEX_POINT('',#93990);
#25265=VERTEX_POINT('',#93994);
#25266=VERTEX_POINT('',#93998);
#25267=VERTEX_POINT('',#94002);
#25268=VERTEX_POINT('',#94006);
#25269=VERTEX_POINT('',#94013);
#25270=VERTEX_POINT('',#94015);
#25271=VERTEX_POINT('',#94019);
#25272=VERTEX_POINT('',#94023);
#25273=VERTEX_POINT('',#94027);
#25274=VERTEX_POINT('',#94031);
#25275=VERTEX_POINT('',#94036);
#25276=VERTEX_POINT('',#94040);
#25277=VERTEX_POINT('',#94049);
#25278=VERTEX_POINT('',#94051);
#25279=VERTEX_POINT('',#94055);
#25280=VERTEX_POINT('',#94059);
#25281=VERTEX_POINT('',#94063);
#25282=VERTEX_POINT('',#94066);
#25283=VERTEX_POINT('',#94070);
#25284=VERTEX_POINT('',#94074);
#25285=VERTEX_POINT('',#94080);
#25286=VERTEX_POINT('',#94081);
#25287=VERTEX_POINT('',#94083);
#25288=VERTEX_POINT('',#94085);
#25289=VERTEX_POINT('',#94089);
#25290=VERTEX_POINT('',#94090);
#25291=VERTEX_POINT('',#94094);
#25292=VERTEX_POINT('',#94096);
#25293=VERTEX_POINT('',#94100);
#25294=VERTEX_POINT('',#94102);
#25295=VERTEX_POINT('',#94106);
#25296=VERTEX_POINT('',#94108);
#25297=VERTEX_POINT('',#94114);
#25298=VERTEX_POINT('',#94115);
#25299=VERTEX_POINT('',#94119);
#25300=VERTEX_POINT('',#94121);
#25301=VERTEX_POINT('',#94125);
#25302=VERTEX_POINT('',#94130);
#25303=VERTEX_POINT('',#94153);
#25304=VERTEX_POINT('',#94155);
#25305=VERTEX_POINT('',#94159);
#25306=VERTEX_POINT('',#94163);
#25307=VERTEX_POINT('',#94167);
#25308=VERTEX_POINT('',#94169);
#25309=VERTEX_POINT('',#94171);
#25310=VERTEX_POINT('',#94175);
#25311=VERTEX_POINT('',#94179);
#25312=VERTEX_POINT('',#94183);
#25313=VERTEX_POINT('',#94187);
#25314=VERTEX_POINT('',#94195);
#25315=VERTEX_POINT('',#94197);
#25316=VERTEX_POINT('',#94203);
#25317=VERTEX_POINT('',#94209);
#25318=VERTEX_POINT('',#94215);
#25319=VERTEX_POINT('',#94219);
#25320=VERTEX_POINT('',#94223);
#25321=EDGE_CURVE('',#20324,#20325,#19574,.T.);
#25322=EDGE_CURVE('',#20326,#20324,#18698,.T.);
#25323=EDGE_CURVE('',#20327,#20326,#18699,.T.);
#25324=EDGE_CURVE('',#20325,#20327,#18700,.T.);
#25325=EDGE_CURVE('',#20328,#20329,#19575,.T.);
#25326=EDGE_CURVE('',#20330,#20328,#18701,.T.);
#25327=EDGE_CURVE('',#20331,#20330,#18702,.T.);
#25328=EDGE_CURVE('',#20329,#20331,#18703,.T.);
#25329=EDGE_CURVE('',#20332,#20333,#19576,.T.);
#25330=EDGE_CURVE('',#20334,#20332,#18704,.T.);
#25331=EDGE_CURVE('',#20335,#20334,#18705,.T.);
#25332=EDGE_CURVE('',#20333,#20335,#18706,.T.);
#25333=EDGE_CURVE('',#20336,#20337,#19577,.T.);
#25334=EDGE_CURVE('',#20338,#20336,#18707,.T.);
#25335=EDGE_CURVE('',#20339,#20338,#18708,.T.);
#25336=EDGE_CURVE('',#20337,#20339,#18709,.T.);
#25337=EDGE_CURVE('',#20340,#20341,#19578,.T.);
#25338=EDGE_CURVE('',#20342,#20340,#18710,.T.);
#25339=EDGE_CURVE('',#20343,#20342,#18711,.T.);
#25340=EDGE_CURVE('',#20341,#20343,#18712,.T.);
#25341=EDGE_CURVE('',#20344,#20345,#19579,.T.);
#25342=EDGE_CURVE('',#20346,#20344,#18713,.T.);
#25343=EDGE_CURVE('',#20347,#20346,#18714,.T.);
#25344=EDGE_CURVE('',#20345,#20347,#18715,.T.);
#25345=EDGE_CURVE('',#20348,#20349,#19580,.T.);
#25346=EDGE_CURVE('',#20350,#20348,#18716,.T.);
#25347=EDGE_CURVE('',#20351,#20350,#18717,.T.);
#25348=EDGE_CURVE('',#20349,#20351,#18718,.T.);
#25349=EDGE_CURVE('',#20352,#20353,#19581,.T.);
#25350=EDGE_CURVE('',#20354,#20352,#18719,.T.);
#25351=EDGE_CURVE('',#20355,#20354,#18720,.T.);
#25352=EDGE_CURVE('',#20353,#20355,#18721,.T.);
#25353=EDGE_CURVE('',#20356,#20357,#19582,.T.);
#25354=EDGE_CURVE('',#20358,#20356,#18722,.T.);
#25355=EDGE_CURVE('',#20359,#20358,#18723,.T.);
#25356=EDGE_CURVE('',#20357,#20359,#18724,.T.);
#25357=EDGE_CURVE('',#20360,#20361,#19583,.T.);
#25358=EDGE_CURVE('',#20362,#20360,#18725,.T.);
#25359=EDGE_CURVE('',#20363,#20362,#18726,.T.);
#25360=EDGE_CURVE('',#20361,#20363,#18727,.T.);
#25361=EDGE_CURVE('',#20364,#20365,#19584,.T.);
#25362=EDGE_CURVE('',#20366,#20364,#18728,.T.);
#25363=EDGE_CURVE('',#20367,#20366,#18729,.T.);
#25364=EDGE_CURVE('',#20365,#20367,#18730,.T.);
#25365=EDGE_CURVE('',#20368,#20369,#19585,.T.);
#25366=EDGE_CURVE('',#20370,#20368,#18731,.T.);
#25367=EDGE_CURVE('',#20371,#20370,#18732,.T.);
#25368=EDGE_CURVE('',#20369,#20371,#18733,.T.);
#25369=EDGE_CURVE('',#20372,#20373,#19586,.T.);
#25370=EDGE_CURVE('',#20374,#20372,#18734,.T.);
#25371=EDGE_CURVE('',#20375,#20374,#18735,.T.);
#25372=EDGE_CURVE('',#20373,#20375,#18736,.T.);
#25373=EDGE_CURVE('',#20376,#20377,#19587,.T.);
#25374=EDGE_CURVE('',#20378,#20376,#18737,.T.);
#25375=EDGE_CURVE('',#20379,#20378,#18738,.T.);
#25376=EDGE_CURVE('',#20377,#20379,#18739,.T.);
#25377=EDGE_CURVE('',#20380,#20381,#19588,.T.);
#25378=EDGE_CURVE('',#20382,#20380,#18740,.T.);
#25379=EDGE_CURVE('',#20383,#20382,#18741,.T.);
#25380=EDGE_CURVE('',#20381,#20383,#18742,.T.);
#25381=EDGE_CURVE('',#20384,#20385,#19589,.T.);
#25382=EDGE_CURVE('',#20386,#20384,#18743,.T.);
#25383=EDGE_CURVE('',#20387,#20386,#18744,.T.);
#25384=EDGE_CURVE('',#20385,#20387,#18745,.T.);
#25385=EDGE_CURVE('',#20388,#20389,#19590,.T.);
#25386=EDGE_CURVE('',#20390,#20388,#18746,.T.);
#25387=EDGE_CURVE('',#20391,#20390,#18747,.T.);
#25388=EDGE_CURVE('',#20389,#20391,#18748,.T.);
#25389=EDGE_CURVE('',#20392,#20393,#19591,.T.);
#25390=EDGE_CURVE('',#20394,#20392,#18749,.T.);
#25391=EDGE_CURVE('',#20395,#20394,#18750,.T.);
#25392=EDGE_CURVE('',#20393,#20395,#18751,.T.);
#25393=EDGE_CURVE('',#20396,#20397,#19592,.T.);
#25394=EDGE_CURVE('',#20398,#20396,#18752,.T.);
#25395=EDGE_CURVE('',#20399,#20398,#18753,.T.);
#25396=EDGE_CURVE('',#20397,#20399,#18754,.T.);
#25397=EDGE_CURVE('',#20400,#20401,#19593,.T.);
#25398=EDGE_CURVE('',#20402,#20400,#18755,.T.);
#25399=EDGE_CURVE('',#20403,#20402,#18756,.T.);
#25400=EDGE_CURVE('',#20401,#20403,#18757,.T.);
#25401=EDGE_CURVE('',#20404,#20405,#19594,.T.);
#25402=EDGE_CURVE('',#20406,#20404,#18758,.T.);
#25403=EDGE_CURVE('',#20407,#20406,#18759,.T.);
#25404=EDGE_CURVE('',#20405,#20407,#18760,.T.);
#25405=EDGE_CURVE('',#20408,#20409,#19595,.T.);
#25406=EDGE_CURVE('',#20410,#20408,#18761,.T.);
#25407=EDGE_CURVE('',#20411,#20410,#18762,.T.);
#25408=EDGE_CURVE('',#20409,#20411,#18763,.T.);
#25409=EDGE_CURVE('',#20412,#20413,#19596,.T.);
#25410=EDGE_CURVE('',#20414,#20412,#18764,.T.);
#25411=EDGE_CURVE('',#20415,#20414,#18765,.T.);
#25412=EDGE_CURVE('',#20413,#20415,#18766,.T.);
#25413=EDGE_CURVE('',#20416,#20417,#19597,.T.);
#25414=EDGE_CURVE('',#20418,#20416,#18767,.T.);
#25415=EDGE_CURVE('',#20419,#20418,#18768,.T.);
#25416=EDGE_CURVE('',#20417,#20419,#18769,.T.);
#25417=EDGE_CURVE('',#20420,#20421,#19598,.T.);
#25418=EDGE_CURVE('',#20422,#20420,#18770,.T.);
#25419=EDGE_CURVE('',#20423,#20422,#18771,.T.);
#25420=EDGE_CURVE('',#20421,#20423,#18772,.T.);
#25421=EDGE_CURVE('',#20424,#20425,#19599,.T.);
#25422=EDGE_CURVE('',#20426,#20424,#18773,.T.);
#25423=EDGE_CURVE('',#20427,#20426,#18774,.T.);
#25424=EDGE_CURVE('',#20425,#20427,#18775,.T.);
#25425=EDGE_CURVE('',#20428,#20429,#19600,.T.);
#25426=EDGE_CURVE('',#20430,#20428,#18776,.T.);
#25427=EDGE_CURVE('',#20431,#20430,#18777,.T.);
#25428=EDGE_CURVE('',#20429,#20431,#18778,.T.);
#25429=EDGE_CURVE('',#20432,#20433,#19601,.T.);
#25430=EDGE_CURVE('',#20434,#20432,#18779,.T.);
#25431=EDGE_CURVE('',#20435,#20434,#18780,.T.);
#25432=EDGE_CURVE('',#20433,#20435,#18781,.T.);
#25433=EDGE_CURVE('',#20436,#20437,#19602,.T.);
#25434=EDGE_CURVE('',#20438,#20436,#18782,.T.);
#25435=EDGE_CURVE('',#20439,#20438,#18783,.T.);
#25436=EDGE_CURVE('',#20437,#20439,#18784,.T.);
#25437=EDGE_CURVE('',#20440,#20441,#19603,.T.);
#25438=EDGE_CURVE('',#20442,#20440,#18785,.T.);
#25439=EDGE_CURVE('',#20443,#20442,#18786,.T.);
#25440=EDGE_CURVE('',#20441,#20443,#18787,.T.);
#25441=EDGE_CURVE('',#20444,#20445,#19604,.T.);
#25442=EDGE_CURVE('',#20446,#20444,#18788,.T.);
#25443=EDGE_CURVE('',#20447,#20446,#18789,.T.);
#25444=EDGE_CURVE('',#20445,#20447,#18790,.T.);
#25445=EDGE_CURVE('',#20448,#20449,#19605,.T.);
#25446=EDGE_CURVE('',#20450,#20448,#18791,.T.);
#25447=EDGE_CURVE('',#20451,#20450,#18792,.T.);
#25448=EDGE_CURVE('',#20449,#20451,#18793,.T.);
#25449=EDGE_CURVE('',#20452,#20453,#19606,.T.);
#25450=EDGE_CURVE('',#20454,#20452,#18794,.T.);
#25451=EDGE_CURVE('',#20455,#20454,#18795,.T.);
#25452=EDGE_CURVE('',#20453,#20455,#18796,.T.);
#25453=EDGE_CURVE('',#20456,#20457,#19607,.T.);
#25454=EDGE_CURVE('',#20458,#20456,#18797,.T.);
#25455=EDGE_CURVE('',#20459,#20458,#18798,.T.);
#25456=EDGE_CURVE('',#20457,#20459,#18799,.T.);
#25457=EDGE_CURVE('',#20460,#20461,#19608,.T.);
#25458=EDGE_CURVE('',#20462,#20460,#18800,.T.);
#25459=EDGE_CURVE('',#20463,#20462,#18801,.T.);
#25460=EDGE_CURVE('',#20461,#20463,#18802,.T.);
#25461=EDGE_CURVE('',#20464,#20465,#19609,.T.);
#25462=EDGE_CURVE('',#20466,#20464,#18803,.T.);
#25463=EDGE_CURVE('',#20467,#20466,#18804,.T.);
#25464=EDGE_CURVE('',#20465,#20467,#18805,.T.);
#25465=EDGE_CURVE('',#20468,#20466,#2160,.T.);
#25466=EDGE_CURVE('',#20469,#20468,#2161,.T.);
#25467=EDGE_CURVE('',#20470,#20469,#2162,.T.);
#25468=EDGE_CURVE('',#20471,#20470,#2163,.T.);
#25469=EDGE_CURVE('',#20472,#20471,#2164,.T.);
#25470=EDGE_CURVE('',#20473,#20472,#2165,.T.);
#25471=EDGE_CURVE('',#20474,#20473,#2166,.T.);
#25472=EDGE_CURVE('',#20475,#20474,#2167,.T.);
#25473=EDGE_CURVE('',#20476,#20475,#2168,.T.);
#25474=EDGE_CURVE('',#20477,#20476,#2169,.T.);
#25475=EDGE_CURVE('',#20478,#20477,#2170,.T.);
#25476=EDGE_CURVE('',#20479,#20478,#2171,.T.);
#25477=EDGE_CURVE('',#20480,#20479,#2172,.T.);
#25478=EDGE_CURVE('',#20481,#20480,#2173,.T.);
#25479=EDGE_CURVE('',#20482,#20481,#2174,.T.);
#25480=EDGE_CURVE('',#20482,#20483,#18806,.T.);
#25481=EDGE_CURVE('',#20484,#20483,#2175,.T.);
#25482=EDGE_CURVE('',#20485,#20484,#2176,.T.);
#25483=EDGE_CURVE('',#20486,#20485,#2177,.T.);
#25484=EDGE_CURVE('',#20487,#20486,#2178,.T.);
#25485=EDGE_CURVE('',#20488,#20487,#2179,.T.);
#25486=EDGE_CURVE('',#20489,#20488,#2180,.T.);
#25487=EDGE_CURVE('',#20490,#20489,#2181,.T.);
#25488=EDGE_CURVE('',#20491,#20490,#2182,.T.);
#25489=EDGE_CURVE('',#20492,#20491,#2183,.T.);
#25490=EDGE_CURVE('',#20493,#20492,#2184,.T.);
#25491=EDGE_CURVE('',#20494,#20493,#2185,.T.);
#25492=EDGE_CURVE('',#20495,#20494,#2186,.T.);
#25493=EDGE_CURVE('',#20496,#20495,#2187,.T.);
#25494=EDGE_CURVE('',#20497,#20496,#2188,.T.);
#25495=EDGE_CURVE('',#20467,#20497,#2189,.T.);
#25496=EDGE_CURVE('',#20464,#20498,#2190,.T.);
#25497=EDGE_CURVE('',#20498,#20499,#2191,.T.);
#25498=EDGE_CURVE('',#20500,#20499,#18807,.T.);
#25499=EDGE_CURVE('',#20501,#20500,#1288,.T.);
#25500=EDGE_CURVE('',#20468,#20501,#2192,.T.);
#25501=EDGE_CURVE('',#20502,#20462,#2193,.T.);
#25502=EDGE_CURVE('',#20503,#20502,#2194,.T.);
#25503=EDGE_CURVE('',#20504,#20503,#2195,.T.);
#25504=EDGE_CURVE('',#20505,#20504,#2196,.T.);
#25505=EDGE_CURVE('',#20506,#20505,#2197,.T.);
#25506=EDGE_CURVE('',#20507,#20506,#2198,.T.);
#25507=EDGE_CURVE('',#20508,#20507,#2199,.T.);
#25508=EDGE_CURVE('',#20509,#20508,#2200,.T.);
#25509=EDGE_CURVE('',#20510,#20509,#2201,.T.);
#25510=EDGE_CURVE('',#20511,#20510,#2202,.T.);
#25511=EDGE_CURVE('',#20512,#20511,#2203,.T.);
#25512=EDGE_CURVE('',#20513,#20512,#2204,.T.);
#25513=EDGE_CURVE('',#20514,#20513,#2205,.T.);
#25514=EDGE_CURVE('',#20515,#20514,#2206,.T.);
#25515=EDGE_CURVE('',#20516,#20515,#2207,.T.);
#25516=EDGE_CURVE('',#20516,#20517,#18808,.T.);
#25517=EDGE_CURVE('',#20518,#20517,#2208,.T.);
#25518=EDGE_CURVE('',#20519,#20518,#2209,.T.);
#25519=EDGE_CURVE('',#20520,#20519,#2210,.T.);
#25520=EDGE_CURVE('',#20521,#20520,#2211,.T.);
#25521=EDGE_CURVE('',#20522,#20521,#2212,.T.);
#25522=EDGE_CURVE('',#20523,#20522,#2213,.T.);
#25523=EDGE_CURVE('',#20524,#20523,#2214,.T.);
#25524=EDGE_CURVE('',#20525,#20524,#2215,.T.);
#25525=EDGE_CURVE('',#20526,#20525,#2216,.T.);
#25526=EDGE_CURVE('',#20527,#20526,#2217,.T.);
#25527=EDGE_CURVE('',#20528,#20527,#2218,.T.);
#25528=EDGE_CURVE('',#20529,#20528,#2219,.T.);
#25529=EDGE_CURVE('',#20530,#20529,#2220,.T.);
#25530=EDGE_CURVE('',#20531,#20530,#2221,.T.);
#25531=EDGE_CURVE('',#20463,#20531,#2222,.T.);
#25532=EDGE_CURVE('',#20460,#20532,#2223,.T.);
#25533=EDGE_CURVE('',#20532,#20533,#2224,.T.);
#25534=EDGE_CURVE('',#20534,#20533,#18809,.T.);
#25535=EDGE_CURVE('',#20535,#20534,#1289,.T.);
#25536=EDGE_CURVE('',#20502,#20535,#2225,.T.);
#25537=EDGE_CURVE('',#20536,#20458,#2226,.T.);
#25538=EDGE_CURVE('',#20537,#20536,#2227,.T.);
#25539=EDGE_CURVE('',#20538,#20537,#2228,.T.);
#25540=EDGE_CURVE('',#20539,#20538,#2229,.T.);
#25541=EDGE_CURVE('',#20540,#20539,#2230,.T.);
#25542=EDGE_CURVE('',#20541,#20540,#2231,.T.);
#25543=EDGE_CURVE('',#20542,#20541,#2232,.T.);
#25544=EDGE_CURVE('',#20543,#20542,#2233,.T.);
#25545=EDGE_CURVE('',#20544,#20543,#2234,.T.);
#25546=EDGE_CURVE('',#20545,#20544,#2235,.T.);
#25547=EDGE_CURVE('',#20546,#20545,#2236,.T.);
#25548=EDGE_CURVE('',#20547,#20546,#2237,.T.);
#25549=EDGE_CURVE('',#20548,#20547,#2238,.T.);
#25550=EDGE_CURVE('',#20549,#20548,#2239,.T.);
#25551=EDGE_CURVE('',#20550,#20549,#2240,.T.);
#25552=EDGE_CURVE('',#20550,#20551,#18810,.T.);
#25553=EDGE_CURVE('',#20552,#20551,#2241,.T.);
#25554=EDGE_CURVE('',#20553,#20552,#2242,.T.);
#25555=EDGE_CURVE('',#20554,#20553,#2243,.T.);
#25556=EDGE_CURVE('',#20555,#20554,#2244,.T.);
#25557=EDGE_CURVE('',#20556,#20555,#2245,.T.);
#25558=EDGE_CURVE('',#20557,#20556,#2246,.T.);
#25559=EDGE_CURVE('',#20558,#20557,#2247,.T.);
#25560=EDGE_CURVE('',#20559,#20558,#2248,.T.);
#25561=EDGE_CURVE('',#20560,#20559,#2249,.T.);
#25562=EDGE_CURVE('',#20561,#20560,#2250,.T.);
#25563=EDGE_CURVE('',#20562,#20561,#2251,.T.);
#25564=EDGE_CURVE('',#20563,#20562,#2252,.T.);
#25565=EDGE_CURVE('',#20564,#20563,#2253,.T.);
#25566=EDGE_CURVE('',#20565,#20564,#2254,.T.);
#25567=EDGE_CURVE('',#20459,#20565,#2255,.T.);
#25568=EDGE_CURVE('',#20456,#20566,#2256,.T.);
#25569=EDGE_CURVE('',#20566,#20567,#2257,.T.);
#25570=EDGE_CURVE('',#20568,#20567,#18811,.T.);
#25571=EDGE_CURVE('',#20569,#20568,#1290,.T.);
#25572=EDGE_CURVE('',#20536,#20569,#2258,.T.);
#25573=EDGE_CURVE('',#20570,#20454,#2259,.T.);
#25574=EDGE_CURVE('',#20571,#20570,#2260,.T.);
#25575=EDGE_CURVE('',#20572,#20571,#2261,.T.);
#25576=EDGE_CURVE('',#20573,#20572,#2262,.T.);
#25577=EDGE_CURVE('',#20574,#20573,#2263,.T.);
#25578=EDGE_CURVE('',#20575,#20574,#2264,.T.);
#25579=EDGE_CURVE('',#20576,#20575,#2265,.T.);
#25580=EDGE_CURVE('',#20577,#20576,#2266,.T.);
#25581=EDGE_CURVE('',#20578,#20577,#2267,.T.);
#25582=EDGE_CURVE('',#20579,#20578,#2268,.T.);
#25583=EDGE_CURVE('',#20580,#20579,#2269,.T.);
#25584=EDGE_CURVE('',#20581,#20580,#2270,.T.);
#25585=EDGE_CURVE('',#20582,#20581,#2271,.T.);
#25586=EDGE_CURVE('',#20583,#20582,#2272,.T.);
#25587=EDGE_CURVE('',#20584,#20583,#2273,.T.);
#25588=EDGE_CURVE('',#20584,#20585,#18812,.T.);
#25589=EDGE_CURVE('',#20586,#20585,#2274,.T.);
#25590=EDGE_CURVE('',#20587,#20586,#2275,.T.);
#25591=EDGE_CURVE('',#20588,#20587,#2276,.T.);
#25592=EDGE_CURVE('',#20589,#20588,#2277,.T.);
#25593=EDGE_CURVE('',#20590,#20589,#2278,.T.);
#25594=EDGE_CURVE('',#20591,#20590,#2279,.T.);
#25595=EDGE_CURVE('',#20592,#20591,#2280,.T.);
#25596=EDGE_CURVE('',#20593,#20592,#2281,.T.);
#25597=EDGE_CURVE('',#20594,#20593,#2282,.T.);
#25598=EDGE_CURVE('',#20595,#20594,#2283,.T.);
#25599=EDGE_CURVE('',#20596,#20595,#2284,.T.);
#25600=EDGE_CURVE('',#20597,#20596,#2285,.T.);
#25601=EDGE_CURVE('',#20598,#20597,#2286,.T.);
#25602=EDGE_CURVE('',#20599,#20598,#2287,.T.);
#25603=EDGE_CURVE('',#20455,#20599,#2288,.T.);
#25604=EDGE_CURVE('',#20452,#20600,#2289,.T.);
#25605=EDGE_CURVE('',#20600,#20601,#2290,.T.);
#25606=EDGE_CURVE('',#20602,#20601,#18813,.T.);
#25607=EDGE_CURVE('',#20603,#20602,#1291,.T.);
#25608=EDGE_CURVE('',#20570,#20603,#2291,.T.);
#25609=EDGE_CURVE('',#20604,#20450,#2292,.T.);
#25610=EDGE_CURVE('',#20605,#20604,#2293,.T.);
#25611=EDGE_CURVE('',#20606,#20605,#2294,.T.);
#25612=EDGE_CURVE('',#20607,#20606,#2295,.T.);
#25613=EDGE_CURVE('',#20608,#20607,#2296,.T.);
#25614=EDGE_CURVE('',#20609,#20608,#2297,.T.);
#25615=EDGE_CURVE('',#20610,#20609,#2298,.T.);
#25616=EDGE_CURVE('',#20611,#20610,#2299,.T.);
#25617=EDGE_CURVE('',#20612,#20611,#2300,.T.);
#25618=EDGE_CURVE('',#20613,#20612,#2301,.T.);
#25619=EDGE_CURVE('',#20614,#20613,#2302,.T.);
#25620=EDGE_CURVE('',#20615,#20614,#2303,.T.);
#25621=EDGE_CURVE('',#20616,#20615,#2304,.T.);
#25622=EDGE_CURVE('',#20617,#20616,#2305,.T.);
#25623=EDGE_CURVE('',#20618,#20617,#2306,.T.);
#25624=EDGE_CURVE('',#20618,#20619,#18814,.T.);
#25625=EDGE_CURVE('',#20620,#20619,#2307,.T.);
#25626=EDGE_CURVE('',#20621,#20620,#2308,.T.);
#25627=EDGE_CURVE('',#20622,#20621,#2309,.T.);
#25628=EDGE_CURVE('',#20623,#20622,#2310,.T.);
#25629=EDGE_CURVE('',#20624,#20623,#2311,.T.);
#25630=EDGE_CURVE('',#20625,#20624,#2312,.T.);
#25631=EDGE_CURVE('',#20626,#20625,#2313,.T.);
#25632=EDGE_CURVE('',#20627,#20626,#2314,.T.);
#25633=EDGE_CURVE('',#20628,#20627,#2315,.T.);
#25634=EDGE_CURVE('',#20629,#20628,#2316,.T.);
#25635=EDGE_CURVE('',#20630,#20629,#2317,.T.);
#25636=EDGE_CURVE('',#20631,#20630,#2318,.T.);
#25637=EDGE_CURVE('',#20632,#20631,#2319,.T.);
#25638=EDGE_CURVE('',#20633,#20632,#2320,.T.);
#25639=EDGE_CURVE('',#20451,#20633,#2321,.T.);
#25640=EDGE_CURVE('',#20448,#20634,#2322,.T.);
#25641=EDGE_CURVE('',#20634,#20635,#2323,.T.);
#25642=EDGE_CURVE('',#20636,#20635,#18815,.T.);
#25643=EDGE_CURVE('',#20637,#20636,#1292,.T.);
#25644=EDGE_CURVE('',#20604,#20637,#2324,.T.);
#25645=EDGE_CURVE('',#20638,#20446,#2325,.T.);
#25646=EDGE_CURVE('',#20639,#20638,#2326,.T.);
#25647=EDGE_CURVE('',#20640,#20639,#2327,.T.);
#25648=EDGE_CURVE('',#20641,#20640,#2328,.T.);
#25649=EDGE_CURVE('',#20642,#20641,#2329,.T.);
#25650=EDGE_CURVE('',#20643,#20642,#2330,.T.);
#25651=EDGE_CURVE('',#20644,#20643,#2331,.T.);
#25652=EDGE_CURVE('',#20645,#20644,#2332,.T.);
#25653=EDGE_CURVE('',#20646,#20645,#2333,.T.);
#25654=EDGE_CURVE('',#20647,#20646,#2334,.T.);
#25655=EDGE_CURVE('',#20648,#20647,#2335,.T.);
#25656=EDGE_CURVE('',#20649,#20648,#2336,.T.);
#25657=EDGE_CURVE('',#20650,#20649,#2337,.T.);
#25658=EDGE_CURVE('',#20651,#20650,#2338,.T.);
#25659=EDGE_CURVE('',#20652,#20651,#2339,.T.);
#25660=EDGE_CURVE('',#20652,#20653,#18816,.T.);
#25661=EDGE_CURVE('',#20654,#20653,#2340,.T.);
#25662=EDGE_CURVE('',#20655,#20654,#2341,.T.);
#25663=EDGE_CURVE('',#20656,#20655,#2342,.T.);
#25664=EDGE_CURVE('',#20657,#20656,#2343,.T.);
#25665=EDGE_CURVE('',#20658,#20657,#2344,.T.);
#25666=EDGE_CURVE('',#20659,#20658,#2345,.T.);
#25667=EDGE_CURVE('',#20660,#20659,#2346,.T.);
#25668=EDGE_CURVE('',#20661,#20660,#2347,.T.);
#25669=EDGE_CURVE('',#20662,#20661,#2348,.T.);
#25670=EDGE_CURVE('',#20663,#20662,#2349,.T.);
#25671=EDGE_CURVE('',#20664,#20663,#2350,.T.);
#25672=EDGE_CURVE('',#20665,#20664,#2351,.T.);
#25673=EDGE_CURVE('',#20666,#20665,#2352,.T.);
#25674=EDGE_CURVE('',#20667,#20666,#2353,.T.);
#25675=EDGE_CURVE('',#20447,#20667,#2354,.T.);
#25676=EDGE_CURVE('',#20444,#20668,#2355,.T.);
#25677=EDGE_CURVE('',#20668,#20669,#2356,.T.);
#25678=EDGE_CURVE('',#20670,#20669,#18817,.T.);
#25679=EDGE_CURVE('',#20671,#20670,#1293,.T.);
#25680=EDGE_CURVE('',#20638,#20671,#2357,.T.);
#25681=EDGE_CURVE('',#20672,#20442,#2358,.T.);
#25682=EDGE_CURVE('',#20673,#20672,#2359,.T.);
#25683=EDGE_CURVE('',#20674,#20673,#2360,.T.);
#25684=EDGE_CURVE('',#20675,#20674,#2361,.T.);
#25685=EDGE_CURVE('',#20676,#20675,#2362,.T.);
#25686=EDGE_CURVE('',#20677,#20676,#2363,.T.);
#25687=EDGE_CURVE('',#20678,#20677,#2364,.T.);
#25688=EDGE_CURVE('',#20679,#20678,#2365,.T.);
#25689=EDGE_CURVE('',#20680,#20679,#2366,.T.);
#25690=EDGE_CURVE('',#20681,#20680,#2367,.T.);
#25691=EDGE_CURVE('',#20682,#20681,#2368,.T.);
#25692=EDGE_CURVE('',#20683,#20682,#2369,.T.);
#25693=EDGE_CURVE('',#20684,#20683,#2370,.T.);
#25694=EDGE_CURVE('',#20685,#20684,#2371,.T.);
#25695=EDGE_CURVE('',#20686,#20685,#2372,.T.);
#25696=EDGE_CURVE('',#20686,#20687,#18818,.T.);
#25697=EDGE_CURVE('',#20688,#20687,#2373,.T.);
#25698=EDGE_CURVE('',#20689,#20688,#2374,.T.);
#25699=EDGE_CURVE('',#20690,#20689,#2375,.T.);
#25700=EDGE_CURVE('',#20691,#20690,#2376,.T.);
#25701=EDGE_CURVE('',#20692,#20691,#2377,.T.);
#25702=EDGE_CURVE('',#20693,#20692,#2378,.T.);
#25703=EDGE_CURVE('',#20694,#20693,#2379,.T.);
#25704=EDGE_CURVE('',#20695,#20694,#2380,.T.);
#25705=EDGE_CURVE('',#20696,#20695,#2381,.T.);
#25706=EDGE_CURVE('',#20697,#20696,#2382,.T.);
#25707=EDGE_CURVE('',#20698,#20697,#2383,.T.);
#25708=EDGE_CURVE('',#20699,#20698,#2384,.T.);
#25709=EDGE_CURVE('',#20700,#20699,#2385,.T.);
#25710=EDGE_CURVE('',#20701,#20700,#2386,.T.);
#25711=EDGE_CURVE('',#20443,#20701,#2387,.T.);
#25712=EDGE_CURVE('',#20440,#20702,#2388,.T.);
#25713=EDGE_CURVE('',#20702,#20703,#2389,.T.);
#25714=EDGE_CURVE('',#20704,#20703,#18819,.T.);
#25715=EDGE_CURVE('',#20705,#20704,#1294,.T.);
#25716=EDGE_CURVE('',#20672,#20705,#2390,.T.);
#25717=EDGE_CURVE('',#20706,#20438,#2391,.T.);
#25718=EDGE_CURVE('',#20707,#20706,#2392,.T.);
#25719=EDGE_CURVE('',#20708,#20707,#2393,.T.);
#25720=EDGE_CURVE('',#20709,#20708,#2394,.T.);
#25721=EDGE_CURVE('',#20710,#20709,#2395,.T.);
#25722=EDGE_CURVE('',#20711,#20710,#2396,.T.);
#25723=EDGE_CURVE('',#20712,#20711,#2397,.T.);
#25724=EDGE_CURVE('',#20713,#20712,#2398,.T.);
#25725=EDGE_CURVE('',#20714,#20713,#2399,.T.);
#25726=EDGE_CURVE('',#20715,#20714,#2400,.T.);
#25727=EDGE_CURVE('',#20716,#20715,#2401,.T.);
#25728=EDGE_CURVE('',#20717,#20716,#2402,.T.);
#25729=EDGE_CURVE('',#20718,#20717,#2403,.T.);
#25730=EDGE_CURVE('',#20719,#20718,#2404,.T.);
#25731=EDGE_CURVE('',#20720,#20719,#2405,.T.);
#25732=EDGE_CURVE('',#20720,#20721,#18820,.T.);
#25733=EDGE_CURVE('',#20722,#20721,#2406,.T.);
#25734=EDGE_CURVE('',#20723,#20722,#2407,.T.);
#25735=EDGE_CURVE('',#20724,#20723,#2408,.T.);
#25736=EDGE_CURVE('',#20725,#20724,#2409,.T.);
#25737=EDGE_CURVE('',#20726,#20725,#2410,.T.);
#25738=EDGE_CURVE('',#20727,#20726,#2411,.T.);
#25739=EDGE_CURVE('',#20728,#20727,#2412,.T.);
#25740=EDGE_CURVE('',#20729,#20728,#2413,.T.);
#25741=EDGE_CURVE('',#20730,#20729,#2414,.T.);
#25742=EDGE_CURVE('',#20731,#20730,#2415,.T.);
#25743=EDGE_CURVE('',#20732,#20731,#2416,.T.);
#25744=EDGE_CURVE('',#20733,#20732,#2417,.T.);
#25745=EDGE_CURVE('',#20734,#20733,#2418,.T.);
#25746=EDGE_CURVE('',#20735,#20734,#2419,.T.);
#25747=EDGE_CURVE('',#20439,#20735,#2420,.T.);
#25748=EDGE_CURVE('',#20436,#20736,#2421,.T.);
#25749=EDGE_CURVE('',#20736,#20737,#2422,.T.);
#25750=EDGE_CURVE('',#20738,#20737,#18821,.T.);
#25751=EDGE_CURVE('',#20739,#20738,#1295,.T.);
#25752=EDGE_CURVE('',#20706,#20739,#2423,.T.);
#25753=EDGE_CURVE('',#20740,#20434,#2424,.T.);
#25754=EDGE_CURVE('',#20741,#20740,#2425,.T.);
#25755=EDGE_CURVE('',#20742,#20741,#2426,.T.);
#25756=EDGE_CURVE('',#20743,#20742,#2427,.T.);
#25757=EDGE_CURVE('',#20744,#20743,#2428,.T.);
#25758=EDGE_CURVE('',#20745,#20744,#2429,.T.);
#25759=EDGE_CURVE('',#20746,#20745,#2430,.T.);
#25760=EDGE_CURVE('',#20747,#20746,#2431,.T.);
#25761=EDGE_CURVE('',#20748,#20747,#2432,.T.);
#25762=EDGE_CURVE('',#20749,#20748,#2433,.T.);
#25763=EDGE_CURVE('',#20750,#20749,#2434,.T.);
#25764=EDGE_CURVE('',#20751,#20750,#2435,.T.);
#25765=EDGE_CURVE('',#20752,#20751,#2436,.T.);
#25766=EDGE_CURVE('',#20753,#20752,#2437,.T.);
#25767=EDGE_CURVE('',#20754,#20753,#2438,.T.);
#25768=EDGE_CURVE('',#20754,#20755,#18822,.T.);
#25769=EDGE_CURVE('',#20756,#20755,#2439,.T.);
#25770=EDGE_CURVE('',#20757,#20756,#2440,.T.);
#25771=EDGE_CURVE('',#20758,#20757,#2441,.T.);
#25772=EDGE_CURVE('',#20759,#20758,#2442,.T.);
#25773=EDGE_CURVE('',#20760,#20759,#2443,.T.);
#25774=EDGE_CURVE('',#20761,#20760,#2444,.T.);
#25775=EDGE_CURVE('',#20762,#20761,#2445,.T.);
#25776=EDGE_CURVE('',#20763,#20762,#2446,.T.);
#25777=EDGE_CURVE('',#20764,#20763,#2447,.T.);
#25778=EDGE_CURVE('',#20765,#20764,#2448,.T.);
#25779=EDGE_CURVE('',#20766,#20765,#2449,.T.);
#25780=EDGE_CURVE('',#20767,#20766,#2450,.T.);
#25781=EDGE_CURVE('',#20768,#20767,#2451,.T.);
#25782=EDGE_CURVE('',#20769,#20768,#2452,.T.);
#25783=EDGE_CURVE('',#20435,#20769,#2453,.T.);
#25784=EDGE_CURVE('',#20432,#20770,#2454,.T.);
#25785=EDGE_CURVE('',#20770,#20771,#2455,.T.);
#25786=EDGE_CURVE('',#20772,#20771,#18823,.T.);
#25787=EDGE_CURVE('',#20773,#20772,#1296,.T.);
#25788=EDGE_CURVE('',#20740,#20773,#2456,.T.);
#25789=EDGE_CURVE('',#20774,#20430,#2457,.T.);
#25790=EDGE_CURVE('',#20775,#20774,#2458,.T.);
#25791=EDGE_CURVE('',#20776,#20775,#2459,.T.);
#25792=EDGE_CURVE('',#20777,#20776,#2460,.T.);
#25793=EDGE_CURVE('',#20778,#20777,#2461,.T.);
#25794=EDGE_CURVE('',#20779,#20778,#2462,.T.);
#25795=EDGE_CURVE('',#20780,#20779,#2463,.T.);
#25796=EDGE_CURVE('',#20781,#20780,#2464,.T.);
#25797=EDGE_CURVE('',#20782,#20781,#2465,.T.);
#25798=EDGE_CURVE('',#20783,#20782,#2466,.T.);
#25799=EDGE_CURVE('',#20784,#20783,#2467,.T.);
#25800=EDGE_CURVE('',#20785,#20784,#2468,.T.);
#25801=EDGE_CURVE('',#20786,#20785,#2469,.T.);
#25802=EDGE_CURVE('',#20787,#20786,#2470,.T.);
#25803=EDGE_CURVE('',#20788,#20787,#2471,.T.);
#25804=EDGE_CURVE('',#20788,#20789,#18824,.T.);
#25805=EDGE_CURVE('',#20790,#20789,#2472,.T.);
#25806=EDGE_CURVE('',#20791,#20790,#2473,.T.);
#25807=EDGE_CURVE('',#20792,#20791,#2474,.T.);
#25808=EDGE_CURVE('',#20793,#20792,#2475,.T.);
#25809=EDGE_CURVE('',#20794,#20793,#2476,.T.);
#25810=EDGE_CURVE('',#20795,#20794,#2477,.T.);
#25811=EDGE_CURVE('',#20796,#20795,#2478,.T.);
#25812=EDGE_CURVE('',#20797,#20796,#2479,.T.);
#25813=EDGE_CURVE('',#20798,#20797,#2480,.T.);
#25814=EDGE_CURVE('',#20799,#20798,#2481,.T.);
#25815=EDGE_CURVE('',#20800,#20799,#2482,.T.);
#25816=EDGE_CURVE('',#20801,#20800,#2483,.T.);
#25817=EDGE_CURVE('',#20802,#20801,#2484,.T.);
#25818=EDGE_CURVE('',#20803,#20802,#2485,.T.);
#25819=EDGE_CURVE('',#20431,#20803,#2486,.T.);
#25820=EDGE_CURVE('',#20428,#20804,#2487,.T.);
#25821=EDGE_CURVE('',#20804,#20805,#2488,.T.);
#25822=EDGE_CURVE('',#20806,#20805,#18825,.T.);
#25823=EDGE_CURVE('',#20807,#20806,#1297,.T.);
#25824=EDGE_CURVE('',#20774,#20807,#2489,.T.);
#25825=EDGE_CURVE('',#20808,#20426,#2490,.T.);
#25826=EDGE_CURVE('',#20809,#20808,#2491,.T.);
#25827=EDGE_CURVE('',#20810,#20809,#2492,.T.);
#25828=EDGE_CURVE('',#20811,#20810,#2493,.T.);
#25829=EDGE_CURVE('',#20812,#20811,#2494,.T.);
#25830=EDGE_CURVE('',#20813,#20812,#2495,.T.);
#25831=EDGE_CURVE('',#20814,#20813,#2496,.T.);
#25832=EDGE_CURVE('',#20815,#20814,#2497,.T.);
#25833=EDGE_CURVE('',#20816,#20815,#2498,.T.);
#25834=EDGE_CURVE('',#20817,#20816,#2499,.T.);
#25835=EDGE_CURVE('',#20818,#20817,#2500,.T.);
#25836=EDGE_CURVE('',#20819,#20818,#2501,.T.);
#25837=EDGE_CURVE('',#20820,#20819,#2502,.T.);
#25838=EDGE_CURVE('',#20821,#20820,#2503,.T.);
#25839=EDGE_CURVE('',#20822,#20821,#2504,.T.);
#25840=EDGE_CURVE('',#20822,#20823,#18826,.T.);
#25841=EDGE_CURVE('',#20824,#20823,#2505,.T.);
#25842=EDGE_CURVE('',#20825,#20824,#2506,.T.);
#25843=EDGE_CURVE('',#20826,#20825,#2507,.T.);
#25844=EDGE_CURVE('',#20827,#20826,#2508,.T.);
#25845=EDGE_CURVE('',#20828,#20827,#2509,.T.);
#25846=EDGE_CURVE('',#20829,#20828,#2510,.T.);
#25847=EDGE_CURVE('',#20830,#20829,#2511,.T.);
#25848=EDGE_CURVE('',#20831,#20830,#2512,.T.);
#25849=EDGE_CURVE('',#20832,#20831,#2513,.T.);
#25850=EDGE_CURVE('',#20833,#20832,#2514,.T.);
#25851=EDGE_CURVE('',#20834,#20833,#2515,.T.);
#25852=EDGE_CURVE('',#20835,#20834,#2516,.T.);
#25853=EDGE_CURVE('',#20836,#20835,#2517,.T.);
#25854=EDGE_CURVE('',#20837,#20836,#2518,.T.);
#25855=EDGE_CURVE('',#20427,#20837,#2519,.T.);
#25856=EDGE_CURVE('',#20424,#20838,#2520,.T.);
#25857=EDGE_CURVE('',#20838,#20839,#2521,.T.);
#25858=EDGE_CURVE('',#20840,#20839,#18827,.T.);
#25859=EDGE_CURVE('',#20841,#20840,#1298,.T.);
#25860=EDGE_CURVE('',#20808,#20841,#2522,.T.);
#25861=EDGE_CURVE('',#20842,#20422,#2523,.T.);
#25862=EDGE_CURVE('',#20843,#20842,#2524,.T.);
#25863=EDGE_CURVE('',#20844,#20843,#2525,.T.);
#25864=EDGE_CURVE('',#20845,#20844,#2526,.T.);
#25865=EDGE_CURVE('',#20846,#20845,#2527,.T.);
#25866=EDGE_CURVE('',#20847,#20846,#2528,.T.);
#25867=EDGE_CURVE('',#20848,#20847,#2529,.T.);
#25868=EDGE_CURVE('',#20849,#20848,#2530,.T.);
#25869=EDGE_CURVE('',#20850,#20849,#2531,.T.);
#25870=EDGE_CURVE('',#20851,#20850,#2532,.T.);
#25871=EDGE_CURVE('',#20852,#20851,#2533,.T.);
#25872=EDGE_CURVE('',#20853,#20852,#2534,.T.);
#25873=EDGE_CURVE('',#20854,#20853,#2535,.T.);
#25874=EDGE_CURVE('',#20855,#20854,#2536,.T.);
#25875=EDGE_CURVE('',#20856,#20855,#2537,.T.);
#25876=EDGE_CURVE('',#20856,#20857,#18828,.T.);
#25877=EDGE_CURVE('',#20858,#20857,#2538,.T.);
#25878=EDGE_CURVE('',#20859,#20858,#2539,.T.);
#25879=EDGE_CURVE('',#20860,#20859,#2540,.T.);
#25880=EDGE_CURVE('',#20861,#20860,#2541,.T.);
#25881=EDGE_CURVE('',#20862,#20861,#2542,.T.);
#25882=EDGE_CURVE('',#20863,#20862,#2543,.T.);
#25883=EDGE_CURVE('',#20864,#20863,#2544,.T.);
#25884=EDGE_CURVE('',#20865,#20864,#2545,.T.);
#25885=EDGE_CURVE('',#20866,#20865,#2546,.T.);
#25886=EDGE_CURVE('',#20867,#20866,#2547,.T.);
#25887=EDGE_CURVE('',#20868,#20867,#2548,.T.);
#25888=EDGE_CURVE('',#20869,#20868,#2549,.T.);
#25889=EDGE_CURVE('',#20870,#20869,#2550,.T.);
#25890=EDGE_CURVE('',#20871,#20870,#2551,.T.);
#25891=EDGE_CURVE('',#20423,#20871,#2552,.T.);
#25892=EDGE_CURVE('',#20420,#20872,#2553,.T.);
#25893=EDGE_CURVE('',#20872,#20873,#2554,.T.);
#25894=EDGE_CURVE('',#20874,#20873,#18829,.T.);
#25895=EDGE_CURVE('',#20875,#20874,#1299,.T.);
#25896=EDGE_CURVE('',#20842,#20875,#2555,.T.);
#25897=EDGE_CURVE('',#20876,#20418,#2556,.T.);
#25898=EDGE_CURVE('',#20877,#20876,#2557,.T.);
#25899=EDGE_CURVE('',#20878,#20877,#2558,.T.);
#25900=EDGE_CURVE('',#20879,#20878,#2559,.T.);
#25901=EDGE_CURVE('',#20880,#20879,#2560,.T.);
#25902=EDGE_CURVE('',#20881,#20880,#2561,.T.);
#25903=EDGE_CURVE('',#20882,#20881,#2562,.T.);
#25904=EDGE_CURVE('',#20883,#20882,#2563,.T.);
#25905=EDGE_CURVE('',#20884,#20883,#2564,.T.);
#25906=EDGE_CURVE('',#20885,#20884,#2565,.T.);
#25907=EDGE_CURVE('',#20886,#20885,#2566,.T.);
#25908=EDGE_CURVE('',#20887,#20886,#2567,.T.);
#25909=EDGE_CURVE('',#20888,#20887,#2568,.T.);
#25910=EDGE_CURVE('',#20889,#20888,#2569,.T.);
#25911=EDGE_CURVE('',#20890,#20889,#2570,.T.);
#25912=EDGE_CURVE('',#20890,#20891,#18830,.T.);
#25913=EDGE_CURVE('',#20892,#20891,#2571,.T.);
#25914=EDGE_CURVE('',#20893,#20892,#2572,.T.);
#25915=EDGE_CURVE('',#20894,#20893,#2573,.T.);
#25916=EDGE_CURVE('',#20895,#20894,#2574,.T.);
#25917=EDGE_CURVE('',#20896,#20895,#2575,.T.);
#25918=EDGE_CURVE('',#20897,#20896,#2576,.T.);
#25919=EDGE_CURVE('',#20898,#20897,#2577,.T.);
#25920=EDGE_CURVE('',#20899,#20898,#2578,.T.);
#25921=EDGE_CURVE('',#20900,#20899,#2579,.T.);
#25922=EDGE_CURVE('',#20901,#20900,#2580,.T.);
#25923=EDGE_CURVE('',#20902,#20901,#2581,.T.);
#25924=EDGE_CURVE('',#20903,#20902,#2582,.T.);
#25925=EDGE_CURVE('',#20904,#20903,#2583,.T.);
#25926=EDGE_CURVE('',#20905,#20904,#2584,.T.);
#25927=EDGE_CURVE('',#20419,#20905,#2585,.T.);
#25928=EDGE_CURVE('',#20416,#20906,#2586,.T.);
#25929=EDGE_CURVE('',#20906,#20907,#2587,.T.);
#25930=EDGE_CURVE('',#20908,#20907,#18831,.T.);
#25931=EDGE_CURVE('',#20909,#20908,#1300,.T.);
#25932=EDGE_CURVE('',#20876,#20909,#2588,.T.);
#25933=EDGE_CURVE('',#20910,#20414,#2589,.T.);
#25934=EDGE_CURVE('',#20911,#20910,#2590,.T.);
#25935=EDGE_CURVE('',#20912,#20911,#2591,.T.);
#25936=EDGE_CURVE('',#20913,#20912,#2592,.T.);
#25937=EDGE_CURVE('',#20914,#20913,#2593,.T.);
#25938=EDGE_CURVE('',#20915,#20914,#2594,.T.);
#25939=EDGE_CURVE('',#20916,#20915,#2595,.T.);
#25940=EDGE_CURVE('',#20917,#20916,#2596,.T.);
#25941=EDGE_CURVE('',#20918,#20917,#2597,.T.);
#25942=EDGE_CURVE('',#20919,#20918,#2598,.T.);
#25943=EDGE_CURVE('',#20920,#20919,#2599,.T.);
#25944=EDGE_CURVE('',#20921,#20920,#2600,.T.);
#25945=EDGE_CURVE('',#20922,#20921,#2601,.T.);
#25946=EDGE_CURVE('',#20923,#20922,#2602,.T.);
#25947=EDGE_CURVE('',#20924,#20923,#2603,.T.);
#25948=EDGE_CURVE('',#20924,#20925,#18832,.T.);
#25949=EDGE_CURVE('',#20926,#20925,#2604,.T.);
#25950=EDGE_CURVE('',#20927,#20926,#2605,.T.);
#25951=EDGE_CURVE('',#20928,#20927,#2606,.T.);
#25952=EDGE_CURVE('',#20929,#20928,#2607,.T.);
#25953=EDGE_CURVE('',#20930,#20929,#2608,.T.);
#25954=EDGE_CURVE('',#20931,#20930,#2609,.T.);
#25955=EDGE_CURVE('',#20932,#20931,#2610,.T.);
#25956=EDGE_CURVE('',#20933,#20932,#2611,.T.);
#25957=EDGE_CURVE('',#20934,#20933,#2612,.T.);
#25958=EDGE_CURVE('',#20935,#20934,#2613,.T.);
#25959=EDGE_CURVE('',#20936,#20935,#2614,.T.);
#25960=EDGE_CURVE('',#20937,#20936,#2615,.T.);
#25961=EDGE_CURVE('',#20938,#20937,#2616,.T.);
#25962=EDGE_CURVE('',#20939,#20938,#2617,.T.);
#25963=EDGE_CURVE('',#20415,#20939,#2618,.T.);
#25964=EDGE_CURVE('',#20412,#20940,#2619,.T.);
#25965=EDGE_CURVE('',#20940,#20941,#2620,.T.);
#25966=EDGE_CURVE('',#20942,#20941,#18833,.T.);
#25967=EDGE_CURVE('',#20943,#20942,#1301,.T.);
#25968=EDGE_CURVE('',#20910,#20943,#2621,.T.);
#25969=EDGE_CURVE('',#20944,#20410,#2622,.T.);
#25970=EDGE_CURVE('',#20945,#20944,#2623,.T.);
#25971=EDGE_CURVE('',#20946,#20945,#2624,.T.);
#25972=EDGE_CURVE('',#20947,#20946,#2625,.T.);
#25973=EDGE_CURVE('',#20948,#20947,#2626,.T.);
#25974=EDGE_CURVE('',#20949,#20948,#2627,.T.);
#25975=EDGE_CURVE('',#20950,#20949,#2628,.T.);
#25976=EDGE_CURVE('',#20951,#20950,#2629,.T.);
#25977=EDGE_CURVE('',#20952,#20951,#2630,.T.);
#25978=EDGE_CURVE('',#20953,#20952,#2631,.T.);
#25979=EDGE_CURVE('',#20954,#20953,#2632,.T.);
#25980=EDGE_CURVE('',#20955,#20954,#2633,.T.);
#25981=EDGE_CURVE('',#20956,#20955,#2634,.T.);
#25982=EDGE_CURVE('',#20957,#20956,#2635,.T.);
#25983=EDGE_CURVE('',#20958,#20957,#2636,.T.);
#25984=EDGE_CURVE('',#20958,#20959,#18834,.T.);
#25985=EDGE_CURVE('',#20960,#20959,#2637,.T.);
#25986=EDGE_CURVE('',#20961,#20960,#2638,.T.);
#25987=EDGE_CURVE('',#20962,#20961,#2639,.T.);
#25988=EDGE_CURVE('',#20963,#20962,#2640,.T.);
#25989=EDGE_CURVE('',#20964,#20963,#2641,.T.);
#25990=EDGE_CURVE('',#20965,#20964,#2642,.T.);
#25991=EDGE_CURVE('',#20966,#20965,#2643,.T.);
#25992=EDGE_CURVE('',#20967,#20966,#2644,.T.);
#25993=EDGE_CURVE('',#20968,#20967,#2645,.T.);
#25994=EDGE_CURVE('',#20969,#20968,#2646,.T.);
#25995=EDGE_CURVE('',#20970,#20969,#2647,.T.);
#25996=EDGE_CURVE('',#20971,#20970,#2648,.T.);
#25997=EDGE_CURVE('',#20972,#20971,#2649,.T.);
#25998=EDGE_CURVE('',#20973,#20972,#2650,.T.);
#25999=EDGE_CURVE('',#20411,#20973,#2651,.T.);
#26000=EDGE_CURVE('',#20408,#20974,#2652,.T.);
#26001=EDGE_CURVE('',#20974,#20975,#2653,.T.);
#26002=EDGE_CURVE('',#20976,#20975,#18835,.T.);
#26003=EDGE_CURVE('',#20977,#20976,#1302,.T.);
#26004=EDGE_CURVE('',#20944,#20977,#2654,.T.);
#26005=EDGE_CURVE('',#20978,#20406,#2655,.T.);
#26006=EDGE_CURVE('',#20979,#20978,#2656,.T.);
#26007=EDGE_CURVE('',#20980,#20979,#2657,.T.);
#26008=EDGE_CURVE('',#20981,#20980,#2658,.T.);
#26009=EDGE_CURVE('',#20982,#20981,#2659,.T.);
#26010=EDGE_CURVE('',#20983,#20982,#2660,.T.);
#26011=EDGE_CURVE('',#20984,#20983,#2661,.T.);
#26012=EDGE_CURVE('',#20985,#20984,#2662,.T.);
#26013=EDGE_CURVE('',#20986,#20985,#2663,.T.);
#26014=EDGE_CURVE('',#20987,#20986,#2664,.T.);
#26015=EDGE_CURVE('',#20988,#20987,#2665,.T.);
#26016=EDGE_CURVE('',#20989,#20988,#2666,.T.);
#26017=EDGE_CURVE('',#20990,#20989,#2667,.T.);
#26018=EDGE_CURVE('',#20991,#20990,#2668,.T.);
#26019=EDGE_CURVE('',#20992,#20991,#2669,.T.);
#26020=EDGE_CURVE('',#20992,#20993,#18836,.T.);
#26021=EDGE_CURVE('',#20994,#20993,#2670,.T.);
#26022=EDGE_CURVE('',#20995,#20994,#2671,.T.);
#26023=EDGE_CURVE('',#20996,#20995,#2672,.T.);
#26024=EDGE_CURVE('',#20997,#20996,#2673,.T.);
#26025=EDGE_CURVE('',#20998,#20997,#2674,.T.);
#26026=EDGE_CURVE('',#20999,#20998,#2675,.T.);
#26027=EDGE_CURVE('',#21000,#20999,#2676,.T.);
#26028=EDGE_CURVE('',#21001,#21000,#2677,.T.);
#26029=EDGE_CURVE('',#21002,#21001,#2678,.T.);
#26030=EDGE_CURVE('',#21003,#21002,#2679,.T.);
#26031=EDGE_CURVE('',#21004,#21003,#2680,.T.);
#26032=EDGE_CURVE('',#21005,#21004,#2681,.T.);
#26033=EDGE_CURVE('',#21006,#21005,#2682,.T.);
#26034=EDGE_CURVE('',#21007,#21006,#2683,.T.);
#26035=EDGE_CURVE('',#20407,#21007,#2684,.T.);
#26036=EDGE_CURVE('',#20404,#21008,#2685,.T.);
#26037=EDGE_CURVE('',#21008,#21009,#2686,.T.);
#26038=EDGE_CURVE('',#21010,#21009,#18837,.T.);
#26039=EDGE_CURVE('',#21011,#21010,#1303,.T.);
#26040=EDGE_CURVE('',#20978,#21011,#2687,.T.);
#26041=EDGE_CURVE('',#21012,#20402,#2688,.T.);
#26042=EDGE_CURVE('',#21013,#21012,#2689,.T.);
#26043=EDGE_CURVE('',#21014,#21013,#2690,.T.);
#26044=EDGE_CURVE('',#21015,#21014,#2691,.T.);
#26045=EDGE_CURVE('',#21016,#21015,#2692,.T.);
#26046=EDGE_CURVE('',#21017,#21016,#2693,.T.);
#26047=EDGE_CURVE('',#21018,#21017,#2694,.T.);
#26048=EDGE_CURVE('',#21019,#21018,#2695,.T.);
#26049=EDGE_CURVE('',#21020,#21019,#2696,.T.);
#26050=EDGE_CURVE('',#21021,#21020,#2697,.T.);
#26051=EDGE_CURVE('',#21022,#21021,#2698,.T.);
#26052=EDGE_CURVE('',#21023,#21022,#2699,.T.);
#26053=EDGE_CURVE('',#21024,#21023,#2700,.T.);
#26054=EDGE_CURVE('',#21025,#21024,#2701,.T.);
#26055=EDGE_CURVE('',#21026,#21025,#2702,.T.);
#26056=EDGE_CURVE('',#21026,#21027,#18838,.T.);
#26057=EDGE_CURVE('',#21028,#21027,#2703,.T.);
#26058=EDGE_CURVE('',#21029,#21028,#2704,.T.);
#26059=EDGE_CURVE('',#21030,#21029,#2705,.T.);
#26060=EDGE_CURVE('',#21031,#21030,#2706,.T.);
#26061=EDGE_CURVE('',#21032,#21031,#2707,.T.);
#26062=EDGE_CURVE('',#21033,#21032,#2708,.T.);
#26063=EDGE_CURVE('',#21034,#21033,#2709,.T.);
#26064=EDGE_CURVE('',#21035,#21034,#2710,.T.);
#26065=EDGE_CURVE('',#21036,#21035,#2711,.T.);
#26066=EDGE_CURVE('',#21037,#21036,#2712,.T.);
#26067=EDGE_CURVE('',#21038,#21037,#2713,.T.);
#26068=EDGE_CURVE('',#21039,#21038,#2714,.T.);
#26069=EDGE_CURVE('',#21040,#21039,#2715,.T.);
#26070=EDGE_CURVE('',#21041,#21040,#2716,.T.);
#26071=EDGE_CURVE('',#20403,#21041,#2717,.T.);
#26072=EDGE_CURVE('',#20400,#21042,#2718,.T.);
#26073=EDGE_CURVE('',#21042,#21043,#2719,.T.);
#26074=EDGE_CURVE('',#21044,#21043,#18839,.T.);
#26075=EDGE_CURVE('',#21045,#21044,#1304,.T.);
#26076=EDGE_CURVE('',#21012,#21045,#2720,.T.);
#26077=EDGE_CURVE('',#21046,#20398,#2721,.T.);
#26078=EDGE_CURVE('',#21047,#21046,#2722,.T.);
#26079=EDGE_CURVE('',#21048,#21047,#2723,.T.);
#26080=EDGE_CURVE('',#21049,#21048,#2724,.T.);
#26081=EDGE_CURVE('',#21050,#21049,#2725,.T.);
#26082=EDGE_CURVE('',#21051,#21050,#2726,.T.);
#26083=EDGE_CURVE('',#21052,#21051,#2727,.T.);
#26084=EDGE_CURVE('',#21053,#21052,#2728,.T.);
#26085=EDGE_CURVE('',#21054,#21053,#2729,.T.);
#26086=EDGE_CURVE('',#21055,#21054,#2730,.T.);
#26087=EDGE_CURVE('',#21056,#21055,#2731,.T.);
#26088=EDGE_CURVE('',#21057,#21056,#2732,.T.);
#26089=EDGE_CURVE('',#21058,#21057,#2733,.T.);
#26090=EDGE_CURVE('',#21059,#21058,#2734,.T.);
#26091=EDGE_CURVE('',#21060,#21059,#2735,.T.);
#26092=EDGE_CURVE('',#21060,#21061,#18840,.T.);
#26093=EDGE_CURVE('',#21062,#21061,#2736,.T.);
#26094=EDGE_CURVE('',#21063,#21062,#2737,.T.);
#26095=EDGE_CURVE('',#21064,#21063,#2738,.T.);
#26096=EDGE_CURVE('',#21065,#21064,#2739,.T.);
#26097=EDGE_CURVE('',#21066,#21065,#2740,.T.);
#26098=EDGE_CURVE('',#21067,#21066,#2741,.T.);
#26099=EDGE_CURVE('',#21068,#21067,#2742,.T.);
#26100=EDGE_CURVE('',#21069,#21068,#2743,.T.);
#26101=EDGE_CURVE('',#21070,#21069,#2744,.T.);
#26102=EDGE_CURVE('',#21071,#21070,#2745,.T.);
#26103=EDGE_CURVE('',#21072,#21071,#2746,.T.);
#26104=EDGE_CURVE('',#21073,#21072,#2747,.T.);
#26105=EDGE_CURVE('',#21074,#21073,#2748,.T.);
#26106=EDGE_CURVE('',#21075,#21074,#2749,.T.);
#26107=EDGE_CURVE('',#20399,#21075,#2750,.T.);
#26108=EDGE_CURVE('',#20396,#21076,#2751,.T.);
#26109=EDGE_CURVE('',#21076,#21077,#2752,.T.);
#26110=EDGE_CURVE('',#21078,#21077,#18841,.T.);
#26111=EDGE_CURVE('',#21079,#21078,#1305,.T.);
#26112=EDGE_CURVE('',#21046,#21079,#2753,.T.);
#26113=EDGE_CURVE('',#21080,#20394,#2754,.T.);
#26114=EDGE_CURVE('',#21081,#21080,#2755,.T.);
#26115=EDGE_CURVE('',#21082,#21081,#2756,.T.);
#26116=EDGE_CURVE('',#21083,#21082,#2757,.T.);
#26117=EDGE_CURVE('',#21084,#21083,#2758,.T.);
#26118=EDGE_CURVE('',#21085,#21084,#2759,.T.);
#26119=EDGE_CURVE('',#21086,#21085,#2760,.T.);
#26120=EDGE_CURVE('',#21087,#21086,#2761,.T.);
#26121=EDGE_CURVE('',#21088,#21087,#2762,.T.);
#26122=EDGE_CURVE('',#21089,#21088,#2763,.T.);
#26123=EDGE_CURVE('',#21090,#21089,#2764,.T.);
#26124=EDGE_CURVE('',#21091,#21090,#2765,.T.);
#26125=EDGE_CURVE('',#21092,#21091,#2766,.T.);
#26126=EDGE_CURVE('',#21093,#21092,#2767,.T.);
#26127=EDGE_CURVE('',#21094,#21093,#2768,.T.);
#26128=EDGE_CURVE('',#21094,#21095,#18842,.T.);
#26129=EDGE_CURVE('',#21096,#21095,#2769,.T.);
#26130=EDGE_CURVE('',#21097,#21096,#2770,.T.);
#26131=EDGE_CURVE('',#21098,#21097,#2771,.T.);
#26132=EDGE_CURVE('',#21099,#21098,#2772,.T.);
#26133=EDGE_CURVE('',#21100,#21099,#2773,.T.);
#26134=EDGE_CURVE('',#21101,#21100,#2774,.T.);
#26135=EDGE_CURVE('',#21102,#21101,#2775,.T.);
#26136=EDGE_CURVE('',#21103,#21102,#2776,.T.);
#26137=EDGE_CURVE('',#21104,#21103,#2777,.T.);
#26138=EDGE_CURVE('',#21105,#21104,#2778,.T.);
#26139=EDGE_CURVE('',#21106,#21105,#2779,.T.);
#26140=EDGE_CURVE('',#21107,#21106,#2780,.T.);
#26141=EDGE_CURVE('',#21108,#21107,#2781,.T.);
#26142=EDGE_CURVE('',#21109,#21108,#2782,.T.);
#26143=EDGE_CURVE('',#20395,#21109,#2783,.T.);
#26144=EDGE_CURVE('',#20392,#21110,#2784,.T.);
#26145=EDGE_CURVE('',#21110,#21111,#2785,.T.);
#26146=EDGE_CURVE('',#21112,#21111,#18843,.T.);
#26147=EDGE_CURVE('',#21113,#21112,#1306,.T.);
#26148=EDGE_CURVE('',#21080,#21113,#2786,.T.);
#26149=EDGE_CURVE('',#21114,#20390,#2787,.T.);
#26150=EDGE_CURVE('',#21115,#21114,#2788,.T.);
#26151=EDGE_CURVE('',#21116,#21115,#2789,.T.);
#26152=EDGE_CURVE('',#21117,#21116,#2790,.T.);
#26153=EDGE_CURVE('',#21118,#21117,#2791,.T.);
#26154=EDGE_CURVE('',#21119,#21118,#2792,.T.);
#26155=EDGE_CURVE('',#21120,#21119,#2793,.T.);
#26156=EDGE_CURVE('',#21121,#21120,#2794,.T.);
#26157=EDGE_CURVE('',#21122,#21121,#2795,.T.);
#26158=EDGE_CURVE('',#21123,#21122,#2796,.T.);
#26159=EDGE_CURVE('',#21124,#21123,#2797,.T.);
#26160=EDGE_CURVE('',#21125,#21124,#2798,.T.);
#26161=EDGE_CURVE('',#21126,#21125,#2799,.T.);
#26162=EDGE_CURVE('',#21127,#21126,#2800,.T.);
#26163=EDGE_CURVE('',#21128,#21127,#2801,.T.);
#26164=EDGE_CURVE('',#21128,#21129,#18844,.T.);
#26165=EDGE_CURVE('',#21130,#21129,#2802,.T.);
#26166=EDGE_CURVE('',#21131,#21130,#2803,.T.);
#26167=EDGE_CURVE('',#21132,#21131,#2804,.T.);
#26168=EDGE_CURVE('',#21133,#21132,#2805,.T.);
#26169=EDGE_CURVE('',#21134,#21133,#2806,.T.);
#26170=EDGE_CURVE('',#21135,#21134,#2807,.T.);
#26171=EDGE_CURVE('',#21136,#21135,#2808,.T.);
#26172=EDGE_CURVE('',#21137,#21136,#2809,.T.);
#26173=EDGE_CURVE('',#21138,#21137,#2810,.T.);
#26174=EDGE_CURVE('',#21139,#21138,#2811,.T.);
#26175=EDGE_CURVE('',#21140,#21139,#2812,.T.);
#26176=EDGE_CURVE('',#21141,#21140,#2813,.T.);
#26177=EDGE_CURVE('',#21142,#21141,#2814,.T.);
#26178=EDGE_CURVE('',#21143,#21142,#2815,.T.);
#26179=EDGE_CURVE('',#20391,#21143,#2816,.T.);
#26180=EDGE_CURVE('',#20388,#21144,#2817,.T.);
#26181=EDGE_CURVE('',#21144,#21145,#2818,.T.);
#26182=EDGE_CURVE('',#21146,#21145,#18845,.T.);
#26183=EDGE_CURVE('',#21147,#21146,#1307,.T.);
#26184=EDGE_CURVE('',#21114,#21147,#2819,.T.);
#26185=EDGE_CURVE('',#21148,#20386,#2820,.T.);
#26186=EDGE_CURVE('',#21149,#21148,#2821,.T.);
#26187=EDGE_CURVE('',#21150,#21149,#2822,.T.);
#26188=EDGE_CURVE('',#21151,#21150,#2823,.T.);
#26189=EDGE_CURVE('',#21152,#21151,#2824,.T.);
#26190=EDGE_CURVE('',#21153,#21152,#2825,.T.);
#26191=EDGE_CURVE('',#21154,#21153,#2826,.T.);
#26192=EDGE_CURVE('',#21155,#21154,#2827,.T.);
#26193=EDGE_CURVE('',#21156,#21155,#2828,.T.);
#26194=EDGE_CURVE('',#21157,#21156,#2829,.T.);
#26195=EDGE_CURVE('',#21158,#21157,#2830,.T.);
#26196=EDGE_CURVE('',#21159,#21158,#2831,.T.);
#26197=EDGE_CURVE('',#21160,#21159,#2832,.T.);
#26198=EDGE_CURVE('',#21161,#21160,#2833,.T.);
#26199=EDGE_CURVE('',#21162,#21161,#2834,.T.);
#26200=EDGE_CURVE('',#21162,#21163,#18846,.T.);
#26201=EDGE_CURVE('',#21164,#21163,#2835,.T.);
#26202=EDGE_CURVE('',#21165,#21164,#2836,.T.);
#26203=EDGE_CURVE('',#21166,#21165,#2837,.T.);
#26204=EDGE_CURVE('',#21167,#21166,#2838,.T.);
#26205=EDGE_CURVE('',#21168,#21167,#2839,.T.);
#26206=EDGE_CURVE('',#21169,#21168,#2840,.T.);
#26207=EDGE_CURVE('',#21170,#21169,#2841,.T.);
#26208=EDGE_CURVE('',#21171,#21170,#2842,.T.);
#26209=EDGE_CURVE('',#21172,#21171,#2843,.T.);
#26210=EDGE_CURVE('',#21173,#21172,#2844,.T.);
#26211=EDGE_CURVE('',#21174,#21173,#2845,.T.);
#26212=EDGE_CURVE('',#21175,#21174,#2846,.T.);
#26213=EDGE_CURVE('',#21176,#21175,#2847,.T.);
#26214=EDGE_CURVE('',#21177,#21176,#2848,.T.);
#26215=EDGE_CURVE('',#20387,#21177,#2849,.T.);
#26216=EDGE_CURVE('',#20384,#21178,#2850,.T.);
#26217=EDGE_CURVE('',#21178,#21179,#2851,.T.);
#26218=EDGE_CURVE('',#21180,#21179,#18847,.T.);
#26219=EDGE_CURVE('',#21181,#21180,#1308,.T.);
#26220=EDGE_CURVE('',#21148,#21181,#2852,.T.);
#26221=EDGE_CURVE('',#21182,#20382,#2853,.T.);
#26222=EDGE_CURVE('',#21183,#21182,#2854,.T.);
#26223=EDGE_CURVE('',#21184,#21183,#2855,.T.);
#26224=EDGE_CURVE('',#21185,#21184,#2856,.T.);
#26225=EDGE_CURVE('',#21186,#21185,#2857,.T.);
#26226=EDGE_CURVE('',#21187,#21186,#2858,.T.);
#26227=EDGE_CURVE('',#21188,#21187,#2859,.T.);
#26228=EDGE_CURVE('',#21189,#21188,#2860,.T.);
#26229=EDGE_CURVE('',#21190,#21189,#2861,.T.);
#26230=EDGE_CURVE('',#21191,#21190,#2862,.T.);
#26231=EDGE_CURVE('',#21192,#21191,#2863,.T.);
#26232=EDGE_CURVE('',#21193,#21192,#2864,.T.);
#26233=EDGE_CURVE('',#21194,#21193,#2865,.T.);
#26234=EDGE_CURVE('',#21195,#21194,#2866,.T.);
#26235=EDGE_CURVE('',#21196,#21195,#2867,.T.);
#26236=EDGE_CURVE('',#21196,#21197,#18848,.T.);
#26237=EDGE_CURVE('',#21198,#21197,#2868,.T.);
#26238=EDGE_CURVE('',#21199,#21198,#2869,.T.);
#26239=EDGE_CURVE('',#21200,#21199,#2870,.T.);
#26240=EDGE_CURVE('',#21201,#21200,#2871,.T.);
#26241=EDGE_CURVE('',#21202,#21201,#2872,.T.);
#26242=EDGE_CURVE('',#21203,#21202,#2873,.T.);
#26243=EDGE_CURVE('',#21204,#21203,#2874,.T.);
#26244=EDGE_CURVE('',#21205,#21204,#2875,.T.);
#26245=EDGE_CURVE('',#21206,#21205,#2876,.T.);
#26246=EDGE_CURVE('',#21207,#21206,#2877,.T.);
#26247=EDGE_CURVE('',#21208,#21207,#2878,.T.);
#26248=EDGE_CURVE('',#21209,#21208,#2879,.T.);
#26249=EDGE_CURVE('',#21210,#21209,#2880,.T.);
#26250=EDGE_CURVE('',#21211,#21210,#2881,.T.);
#26251=EDGE_CURVE('',#20383,#21211,#2882,.T.);
#26252=EDGE_CURVE('',#20380,#21212,#2883,.T.);
#26253=EDGE_CURVE('',#21212,#21213,#2884,.T.);
#26254=EDGE_CURVE('',#21214,#21213,#18849,.T.);
#26255=EDGE_CURVE('',#21215,#21214,#1309,.T.);
#26256=EDGE_CURVE('',#21182,#21215,#2885,.T.);
#26257=EDGE_CURVE('',#21216,#20378,#2886,.T.);
#26258=EDGE_CURVE('',#21217,#21216,#2887,.T.);
#26259=EDGE_CURVE('',#21218,#21217,#2888,.T.);
#26260=EDGE_CURVE('',#21219,#21218,#2889,.T.);
#26261=EDGE_CURVE('',#21220,#21219,#2890,.T.);
#26262=EDGE_CURVE('',#21221,#21220,#2891,.T.);
#26263=EDGE_CURVE('',#21222,#21221,#2892,.T.);
#26264=EDGE_CURVE('',#21223,#21222,#2893,.T.);
#26265=EDGE_CURVE('',#21224,#21223,#2894,.T.);
#26266=EDGE_CURVE('',#21225,#21224,#2895,.T.);
#26267=EDGE_CURVE('',#21226,#21225,#2896,.T.);
#26268=EDGE_CURVE('',#21227,#21226,#2897,.T.);
#26269=EDGE_CURVE('',#21228,#21227,#2898,.T.);
#26270=EDGE_CURVE('',#21229,#21228,#2899,.T.);
#26271=EDGE_CURVE('',#21230,#21229,#2900,.T.);
#26272=EDGE_CURVE('',#21230,#21231,#18850,.T.);
#26273=EDGE_CURVE('',#21232,#21231,#2901,.T.);
#26274=EDGE_CURVE('',#21233,#21232,#2902,.T.);
#26275=EDGE_CURVE('',#21234,#21233,#2903,.T.);
#26276=EDGE_CURVE('',#21235,#21234,#2904,.T.);
#26277=EDGE_CURVE('',#21236,#21235,#2905,.T.);
#26278=EDGE_CURVE('',#21237,#21236,#2906,.T.);
#26279=EDGE_CURVE('',#21238,#21237,#2907,.T.);
#26280=EDGE_CURVE('',#21239,#21238,#2908,.T.);
#26281=EDGE_CURVE('',#21240,#21239,#2909,.T.);
#26282=EDGE_CURVE('',#21241,#21240,#2910,.T.);
#26283=EDGE_CURVE('',#21242,#21241,#2911,.T.);
#26284=EDGE_CURVE('',#21243,#21242,#2912,.T.);
#26285=EDGE_CURVE('',#21244,#21243,#2913,.T.);
#26286=EDGE_CURVE('',#21245,#21244,#2914,.T.);
#26287=EDGE_CURVE('',#20379,#21245,#2915,.T.);
#26288=EDGE_CURVE('',#20376,#21246,#2916,.T.);
#26289=EDGE_CURVE('',#21246,#21247,#2917,.T.);
#26290=EDGE_CURVE('',#21248,#21247,#18851,.T.);
#26291=EDGE_CURVE('',#21249,#21248,#1310,.T.);
#26292=EDGE_CURVE('',#21216,#21249,#2918,.T.);
#26293=EDGE_CURVE('',#21250,#20374,#2919,.T.);
#26294=EDGE_CURVE('',#21251,#21250,#2920,.T.);
#26295=EDGE_CURVE('',#21252,#21251,#2921,.T.);
#26296=EDGE_CURVE('',#21253,#21252,#2922,.T.);
#26297=EDGE_CURVE('',#21254,#21253,#2923,.T.);
#26298=EDGE_CURVE('',#21255,#21254,#2924,.T.);
#26299=EDGE_CURVE('',#21256,#21255,#2925,.T.);
#26300=EDGE_CURVE('',#21257,#21256,#2926,.T.);
#26301=EDGE_CURVE('',#21258,#21257,#2927,.T.);
#26302=EDGE_CURVE('',#21259,#21258,#2928,.T.);
#26303=EDGE_CURVE('',#21260,#21259,#2929,.T.);
#26304=EDGE_CURVE('',#21261,#21260,#2930,.T.);
#26305=EDGE_CURVE('',#21262,#21261,#2931,.T.);
#26306=EDGE_CURVE('',#21263,#21262,#2932,.T.);
#26307=EDGE_CURVE('',#21264,#21263,#2933,.T.);
#26308=EDGE_CURVE('',#21264,#21265,#18852,.T.);
#26309=EDGE_CURVE('',#21266,#21265,#2934,.T.);
#26310=EDGE_CURVE('',#21267,#21266,#2935,.T.);
#26311=EDGE_CURVE('',#21268,#21267,#2936,.T.);
#26312=EDGE_CURVE('',#21269,#21268,#2937,.T.);
#26313=EDGE_CURVE('',#21270,#21269,#2938,.T.);
#26314=EDGE_CURVE('',#21271,#21270,#2939,.T.);
#26315=EDGE_CURVE('',#21272,#21271,#2940,.T.);
#26316=EDGE_CURVE('',#21273,#21272,#2941,.T.);
#26317=EDGE_CURVE('',#21274,#21273,#2942,.T.);
#26318=EDGE_CURVE('',#21275,#21274,#2943,.T.);
#26319=EDGE_CURVE('',#21276,#21275,#2944,.T.);
#26320=EDGE_CURVE('',#21277,#21276,#2945,.T.);
#26321=EDGE_CURVE('',#21278,#21277,#2946,.T.);
#26322=EDGE_CURVE('',#21279,#21278,#2947,.T.);
#26323=EDGE_CURVE('',#20375,#21279,#2948,.T.);
#26324=EDGE_CURVE('',#20372,#21280,#2949,.T.);
#26325=EDGE_CURVE('',#21280,#21281,#2950,.T.);
#26326=EDGE_CURVE('',#21282,#21281,#18853,.T.);
#26327=EDGE_CURVE('',#21283,#21282,#1311,.T.);
#26328=EDGE_CURVE('',#21250,#21283,#2951,.T.);
#26329=EDGE_CURVE('',#21284,#20370,#2952,.T.);
#26330=EDGE_CURVE('',#21285,#21284,#2953,.T.);
#26331=EDGE_CURVE('',#21286,#21285,#2954,.T.);
#26332=EDGE_CURVE('',#21287,#21286,#2955,.T.);
#26333=EDGE_CURVE('',#21288,#21287,#2956,.T.);
#26334=EDGE_CURVE('',#21289,#21288,#2957,.T.);
#26335=EDGE_CURVE('',#21290,#21289,#2958,.T.);
#26336=EDGE_CURVE('',#21291,#21290,#2959,.T.);
#26337=EDGE_CURVE('',#21292,#21291,#2960,.T.);
#26338=EDGE_CURVE('',#21293,#21292,#2961,.T.);
#26339=EDGE_CURVE('',#21294,#21293,#2962,.T.);
#26340=EDGE_CURVE('',#21295,#21294,#2963,.T.);
#26341=EDGE_CURVE('',#21296,#21295,#2964,.T.);
#26342=EDGE_CURVE('',#21297,#21296,#2965,.T.);
#26343=EDGE_CURVE('',#21298,#21297,#2966,.T.);
#26344=EDGE_CURVE('',#21298,#21299,#18854,.T.);
#26345=EDGE_CURVE('',#21300,#21299,#2967,.T.);
#26346=EDGE_CURVE('',#21301,#21300,#2968,.T.);
#26347=EDGE_CURVE('',#21302,#21301,#2969,.T.);
#26348=EDGE_CURVE('',#21303,#21302,#2970,.T.);
#26349=EDGE_CURVE('',#21304,#21303,#2971,.T.);
#26350=EDGE_CURVE('',#21305,#21304,#2972,.T.);
#26351=EDGE_CURVE('',#21306,#21305,#2973,.T.);
#26352=EDGE_CURVE('',#21307,#21306,#2974,.T.);
#26353=EDGE_CURVE('',#21308,#21307,#2975,.T.);
#26354=EDGE_CURVE('',#21309,#21308,#2976,.T.);
#26355=EDGE_CURVE('',#21310,#21309,#2977,.T.);
#26356=EDGE_CURVE('',#21311,#21310,#2978,.T.);
#26357=EDGE_CURVE('',#21312,#21311,#2979,.T.);
#26358=EDGE_CURVE('',#21313,#21312,#2980,.T.);
#26359=EDGE_CURVE('',#20371,#21313,#2981,.T.);
#26360=EDGE_CURVE('',#20368,#21314,#2982,.T.);
#26361=EDGE_CURVE('',#21314,#21315,#2983,.T.);
#26362=EDGE_CURVE('',#21316,#21315,#18855,.T.);
#26363=EDGE_CURVE('',#21317,#21316,#1312,.T.);
#26364=EDGE_CURVE('',#21284,#21317,#2984,.T.);
#26365=EDGE_CURVE('',#21318,#20366,#2985,.T.);
#26366=EDGE_CURVE('',#21319,#21318,#2986,.T.);
#26367=EDGE_CURVE('',#21320,#21319,#2987,.T.);
#26368=EDGE_CURVE('',#21321,#21320,#2988,.T.);
#26369=EDGE_CURVE('',#21322,#21321,#2989,.T.);
#26370=EDGE_CURVE('',#21323,#21322,#2990,.T.);
#26371=EDGE_CURVE('',#21324,#21323,#2991,.T.);
#26372=EDGE_CURVE('',#21325,#21324,#2992,.T.);
#26373=EDGE_CURVE('',#21326,#21325,#2993,.T.);
#26374=EDGE_CURVE('',#21327,#21326,#2994,.T.);
#26375=EDGE_CURVE('',#21328,#21327,#2995,.T.);
#26376=EDGE_CURVE('',#21329,#21328,#2996,.T.);
#26377=EDGE_CURVE('',#21330,#21329,#2997,.T.);
#26378=EDGE_CURVE('',#21331,#21330,#2998,.T.);
#26379=EDGE_CURVE('',#21332,#21331,#2999,.T.);
#26380=EDGE_CURVE('',#21332,#21333,#18856,.T.);
#26381=EDGE_CURVE('',#21334,#21333,#3000,.T.);
#26382=EDGE_CURVE('',#21335,#21334,#3001,.T.);
#26383=EDGE_CURVE('',#21336,#21335,#3002,.T.);
#26384=EDGE_CURVE('',#21337,#21336,#3003,.T.);
#26385=EDGE_CURVE('',#21338,#21337,#3004,.T.);
#26386=EDGE_CURVE('',#21339,#21338,#3005,.T.);
#26387=EDGE_CURVE('',#21340,#21339,#3006,.T.);
#26388=EDGE_CURVE('',#21341,#21340,#3007,.T.);
#26389=EDGE_CURVE('',#21342,#21341,#3008,.T.);
#26390=EDGE_CURVE('',#21343,#21342,#3009,.T.);
#26391=EDGE_CURVE('',#21344,#21343,#3010,.T.);
#26392=EDGE_CURVE('',#21345,#21344,#3011,.T.);
#26393=EDGE_CURVE('',#21346,#21345,#3012,.T.);
#26394=EDGE_CURVE('',#21347,#21346,#3013,.T.);
#26395=EDGE_CURVE('',#20367,#21347,#3014,.T.);
#26396=EDGE_CURVE('',#20364,#21348,#3015,.T.);
#26397=EDGE_CURVE('',#21348,#21349,#3016,.T.);
#26398=EDGE_CURVE('',#21350,#21349,#18857,.T.);
#26399=EDGE_CURVE('',#21351,#21350,#1313,.T.);
#26400=EDGE_CURVE('',#21318,#21351,#3017,.T.);
#26401=EDGE_CURVE('',#21352,#20362,#3018,.T.);
#26402=EDGE_CURVE('',#21353,#21352,#3019,.T.);
#26403=EDGE_CURVE('',#21354,#21353,#3020,.T.);
#26404=EDGE_CURVE('',#21355,#21354,#3021,.T.);
#26405=EDGE_CURVE('',#21356,#21355,#3022,.T.);
#26406=EDGE_CURVE('',#21357,#21356,#3023,.T.);
#26407=EDGE_CURVE('',#21358,#21357,#3024,.T.);
#26408=EDGE_CURVE('',#21359,#21358,#3025,.T.);
#26409=EDGE_CURVE('',#21360,#21359,#3026,.T.);
#26410=EDGE_CURVE('',#21361,#21360,#3027,.T.);
#26411=EDGE_CURVE('',#21362,#21361,#3028,.T.);
#26412=EDGE_CURVE('',#21363,#21362,#3029,.T.);
#26413=EDGE_CURVE('',#21364,#21363,#3030,.T.);
#26414=EDGE_CURVE('',#21365,#21364,#3031,.T.);
#26415=EDGE_CURVE('',#21366,#21365,#3032,.T.);
#26416=EDGE_CURVE('',#21366,#21367,#18858,.T.);
#26417=EDGE_CURVE('',#21368,#21367,#3033,.T.);
#26418=EDGE_CURVE('',#21369,#21368,#3034,.T.);
#26419=EDGE_CURVE('',#21370,#21369,#3035,.T.);
#26420=EDGE_CURVE('',#21371,#21370,#3036,.T.);
#26421=EDGE_CURVE('',#21372,#21371,#3037,.T.);
#26422=EDGE_CURVE('',#21373,#21372,#3038,.T.);
#26423=EDGE_CURVE('',#21374,#21373,#3039,.T.);
#26424=EDGE_CURVE('',#21375,#21374,#3040,.T.);
#26425=EDGE_CURVE('',#21376,#21375,#3041,.T.);
#26426=EDGE_CURVE('',#21377,#21376,#3042,.T.);
#26427=EDGE_CURVE('',#21378,#21377,#3043,.T.);
#26428=EDGE_CURVE('',#21379,#21378,#3044,.T.);
#26429=EDGE_CURVE('',#21380,#21379,#3045,.T.);
#26430=EDGE_CURVE('',#21381,#21380,#3046,.T.);
#26431=EDGE_CURVE('',#20363,#21381,#3047,.T.);
#26432=EDGE_CURVE('',#20360,#21382,#3048,.T.);
#26433=EDGE_CURVE('',#21382,#21383,#3049,.T.);
#26434=EDGE_CURVE('',#21384,#21383,#18859,.T.);
#26435=EDGE_CURVE('',#21385,#21384,#1314,.T.);
#26436=EDGE_CURVE('',#21352,#21385,#3050,.T.);
#26437=EDGE_CURVE('',#21386,#20358,#3051,.T.);
#26438=EDGE_CURVE('',#21387,#21386,#3052,.T.);
#26439=EDGE_CURVE('',#21388,#21387,#3053,.T.);
#26440=EDGE_CURVE('',#21389,#21388,#3054,.T.);
#26441=EDGE_CURVE('',#21390,#21389,#3055,.T.);
#26442=EDGE_CURVE('',#21391,#21390,#3056,.T.);
#26443=EDGE_CURVE('',#21392,#21391,#3057,.T.);
#26444=EDGE_CURVE('',#21393,#21392,#3058,.T.);
#26445=EDGE_CURVE('',#21394,#21393,#3059,.T.);
#26446=EDGE_CURVE('',#21395,#21394,#3060,.T.);
#26447=EDGE_CURVE('',#21396,#21395,#3061,.T.);
#26448=EDGE_CURVE('',#21397,#21396,#3062,.T.);
#26449=EDGE_CURVE('',#21398,#21397,#3063,.T.);
#26450=EDGE_CURVE('',#21399,#21398,#3064,.T.);
#26451=EDGE_CURVE('',#21400,#21399,#3065,.T.);
#26452=EDGE_CURVE('',#21400,#21401,#18860,.T.);
#26453=EDGE_CURVE('',#21402,#21401,#3066,.T.);
#26454=EDGE_CURVE('',#21403,#21402,#3067,.T.);
#26455=EDGE_CURVE('',#21404,#21403,#3068,.T.);
#26456=EDGE_CURVE('',#21405,#21404,#3069,.T.);
#26457=EDGE_CURVE('',#21406,#21405,#3070,.T.);
#26458=EDGE_CURVE('',#21407,#21406,#3071,.T.);
#26459=EDGE_CURVE('',#21408,#21407,#3072,.T.);
#26460=EDGE_CURVE('',#21409,#21408,#3073,.T.);
#26461=EDGE_CURVE('',#21410,#21409,#3074,.T.);
#26462=EDGE_CURVE('',#21411,#21410,#3075,.T.);
#26463=EDGE_CURVE('',#21412,#21411,#3076,.T.);
#26464=EDGE_CURVE('',#21413,#21412,#3077,.T.);
#26465=EDGE_CURVE('',#21414,#21413,#3078,.T.);
#26466=EDGE_CURVE('',#21415,#21414,#3079,.T.);
#26467=EDGE_CURVE('',#20359,#21415,#3080,.T.);
#26468=EDGE_CURVE('',#20356,#21416,#3081,.T.);
#26469=EDGE_CURVE('',#21416,#21417,#3082,.T.);
#26470=EDGE_CURVE('',#21418,#21417,#18861,.T.);
#26471=EDGE_CURVE('',#21419,#21418,#1315,.T.);
#26472=EDGE_CURVE('',#21386,#21419,#3083,.T.);
#26473=EDGE_CURVE('',#21420,#20354,#3084,.T.);
#26474=EDGE_CURVE('',#21421,#21420,#3085,.T.);
#26475=EDGE_CURVE('',#21422,#21421,#3086,.T.);
#26476=EDGE_CURVE('',#21423,#21422,#3087,.T.);
#26477=EDGE_CURVE('',#21424,#21423,#3088,.T.);
#26478=EDGE_CURVE('',#21425,#21424,#3089,.T.);
#26479=EDGE_CURVE('',#21426,#21425,#3090,.T.);
#26480=EDGE_CURVE('',#21427,#21426,#3091,.T.);
#26481=EDGE_CURVE('',#21428,#21427,#3092,.T.);
#26482=EDGE_CURVE('',#21429,#21428,#3093,.T.);
#26483=EDGE_CURVE('',#21430,#21429,#3094,.T.);
#26484=EDGE_CURVE('',#21431,#21430,#3095,.T.);
#26485=EDGE_CURVE('',#21432,#21431,#3096,.T.);
#26486=EDGE_CURVE('',#21433,#21432,#3097,.T.);
#26487=EDGE_CURVE('',#21434,#21433,#3098,.T.);
#26488=EDGE_CURVE('',#21434,#21435,#18862,.T.);
#26489=EDGE_CURVE('',#21436,#21435,#3099,.T.);
#26490=EDGE_CURVE('',#21437,#21436,#3100,.T.);
#26491=EDGE_CURVE('',#21438,#21437,#3101,.T.);
#26492=EDGE_CURVE('',#21439,#21438,#3102,.T.);
#26493=EDGE_CURVE('',#21440,#21439,#3103,.T.);
#26494=EDGE_CURVE('',#21441,#21440,#3104,.T.);
#26495=EDGE_CURVE('',#21442,#21441,#3105,.T.);
#26496=EDGE_CURVE('',#21443,#21442,#3106,.T.);
#26497=EDGE_CURVE('',#21444,#21443,#3107,.T.);
#26498=EDGE_CURVE('',#21445,#21444,#3108,.T.);
#26499=EDGE_CURVE('',#21446,#21445,#3109,.T.);
#26500=EDGE_CURVE('',#21447,#21446,#3110,.T.);
#26501=EDGE_CURVE('',#21448,#21447,#3111,.T.);
#26502=EDGE_CURVE('',#21449,#21448,#3112,.T.);
#26503=EDGE_CURVE('',#20355,#21449,#3113,.T.);
#26504=EDGE_CURVE('',#20352,#21450,#3114,.T.);
#26505=EDGE_CURVE('',#21450,#21451,#3115,.T.);
#26506=EDGE_CURVE('',#21452,#21451,#18863,.T.);
#26507=EDGE_CURVE('',#21453,#21452,#1316,.T.);
#26508=EDGE_CURVE('',#21420,#21453,#3116,.T.);
#26509=EDGE_CURVE('',#21454,#20350,#3117,.T.);
#26510=EDGE_CURVE('',#21455,#21454,#3118,.T.);
#26511=EDGE_CURVE('',#21456,#21455,#3119,.T.);
#26512=EDGE_CURVE('',#21457,#21456,#3120,.T.);
#26513=EDGE_CURVE('',#21458,#21457,#3121,.T.);
#26514=EDGE_CURVE('',#21459,#21458,#3122,.T.);
#26515=EDGE_CURVE('',#21460,#21459,#3123,.T.);
#26516=EDGE_CURVE('',#21461,#21460,#3124,.T.);
#26517=EDGE_CURVE('',#21462,#21461,#3125,.T.);
#26518=EDGE_CURVE('',#21463,#21462,#3126,.T.);
#26519=EDGE_CURVE('',#21464,#21463,#3127,.T.);
#26520=EDGE_CURVE('',#21465,#21464,#3128,.T.);
#26521=EDGE_CURVE('',#21466,#21465,#3129,.T.);
#26522=EDGE_CURVE('',#21467,#21466,#3130,.T.);
#26523=EDGE_CURVE('',#21468,#21467,#3131,.T.);
#26524=EDGE_CURVE('',#21468,#21469,#18864,.T.);
#26525=EDGE_CURVE('',#21470,#21469,#3132,.T.);
#26526=EDGE_CURVE('',#21471,#21470,#3133,.T.);
#26527=EDGE_CURVE('',#21472,#21471,#3134,.T.);
#26528=EDGE_CURVE('',#21473,#21472,#3135,.T.);
#26529=EDGE_CURVE('',#21474,#21473,#3136,.T.);
#26530=EDGE_CURVE('',#21475,#21474,#3137,.T.);
#26531=EDGE_CURVE('',#21476,#21475,#3138,.T.);
#26532=EDGE_CURVE('',#21477,#21476,#3139,.T.);
#26533=EDGE_CURVE('',#21478,#21477,#3140,.T.);
#26534=EDGE_CURVE('',#21479,#21478,#3141,.T.);
#26535=EDGE_CURVE('',#21480,#21479,#3142,.T.);
#26536=EDGE_CURVE('',#21481,#21480,#3143,.T.);
#26537=EDGE_CURVE('',#21482,#21481,#3144,.T.);
#26538=EDGE_CURVE('',#21483,#21482,#3145,.T.);
#26539=EDGE_CURVE('',#20351,#21483,#3146,.T.);
#26540=EDGE_CURVE('',#20348,#21484,#3147,.T.);
#26541=EDGE_CURVE('',#21484,#21485,#3148,.T.);
#26542=EDGE_CURVE('',#21486,#21485,#18865,.T.);
#26543=EDGE_CURVE('',#21487,#21486,#1317,.T.);
#26544=EDGE_CURVE('',#21454,#21487,#3149,.T.);
#26545=EDGE_CURVE('',#21488,#20346,#3150,.T.);
#26546=EDGE_CURVE('',#21489,#21488,#3151,.T.);
#26547=EDGE_CURVE('',#21490,#21489,#3152,.T.);
#26548=EDGE_CURVE('',#21491,#21490,#3153,.T.);
#26549=EDGE_CURVE('',#21492,#21491,#3154,.T.);
#26550=EDGE_CURVE('',#21493,#21492,#3155,.T.);
#26551=EDGE_CURVE('',#21494,#21493,#3156,.T.);
#26552=EDGE_CURVE('',#21495,#21494,#3157,.T.);
#26553=EDGE_CURVE('',#21496,#21495,#3158,.T.);
#26554=EDGE_CURVE('',#21497,#21496,#3159,.T.);
#26555=EDGE_CURVE('',#21498,#21497,#3160,.T.);
#26556=EDGE_CURVE('',#21499,#21498,#3161,.T.);
#26557=EDGE_CURVE('',#21500,#21499,#3162,.T.);
#26558=EDGE_CURVE('',#21501,#21500,#3163,.T.);
#26559=EDGE_CURVE('',#21502,#21501,#3164,.T.);
#26560=EDGE_CURVE('',#21502,#21503,#18866,.T.);
#26561=EDGE_CURVE('',#21504,#21503,#3165,.T.);
#26562=EDGE_CURVE('',#21505,#21504,#3166,.T.);
#26563=EDGE_CURVE('',#21506,#21505,#3167,.T.);
#26564=EDGE_CURVE('',#21507,#21506,#3168,.T.);
#26565=EDGE_CURVE('',#21508,#21507,#3169,.T.);
#26566=EDGE_CURVE('',#21509,#21508,#3170,.T.);
#26567=EDGE_CURVE('',#21510,#21509,#3171,.T.);
#26568=EDGE_CURVE('',#21511,#21510,#3172,.T.);
#26569=EDGE_CURVE('',#21512,#21511,#3173,.T.);
#26570=EDGE_CURVE('',#21513,#21512,#3174,.T.);
#26571=EDGE_CURVE('',#21514,#21513,#3175,.T.);
#26572=EDGE_CURVE('',#21515,#21514,#3176,.T.);
#26573=EDGE_CURVE('',#21516,#21515,#3177,.T.);
#26574=EDGE_CURVE('',#21517,#21516,#3178,.T.);
#26575=EDGE_CURVE('',#20347,#21517,#3179,.T.);
#26576=EDGE_CURVE('',#20344,#21518,#3180,.T.);
#26577=EDGE_CURVE('',#21518,#21519,#3181,.T.);
#26578=EDGE_CURVE('',#21520,#21519,#18867,.T.);
#26579=EDGE_CURVE('',#21521,#21520,#1318,.T.);
#26580=EDGE_CURVE('',#21488,#21521,#3182,.T.);
#26581=EDGE_CURVE('',#21522,#20342,#3183,.T.);
#26582=EDGE_CURVE('',#21523,#21522,#3184,.T.);
#26583=EDGE_CURVE('',#21524,#21523,#3185,.T.);
#26584=EDGE_CURVE('',#21525,#21524,#3186,.T.);
#26585=EDGE_CURVE('',#21526,#21525,#3187,.T.);
#26586=EDGE_CURVE('',#21527,#21526,#3188,.T.);
#26587=EDGE_CURVE('',#21528,#21527,#3189,.T.);
#26588=EDGE_CURVE('',#21529,#21528,#3190,.T.);
#26589=EDGE_CURVE('',#21530,#21529,#3191,.T.);
#26590=EDGE_CURVE('',#21531,#21530,#3192,.T.);
#26591=EDGE_CURVE('',#21532,#21531,#3193,.T.);
#26592=EDGE_CURVE('',#21533,#21532,#3194,.T.);
#26593=EDGE_CURVE('',#21534,#21533,#3195,.T.);
#26594=EDGE_CURVE('',#21535,#21534,#3196,.T.);
#26595=EDGE_CURVE('',#21536,#21535,#3197,.T.);
#26596=EDGE_CURVE('',#21536,#21537,#18868,.T.);
#26597=EDGE_CURVE('',#21538,#21537,#3198,.T.);
#26598=EDGE_CURVE('',#21539,#21538,#3199,.T.);
#26599=EDGE_CURVE('',#21540,#21539,#3200,.T.);
#26600=EDGE_CURVE('',#21541,#21540,#3201,.T.);
#26601=EDGE_CURVE('',#21542,#21541,#3202,.T.);
#26602=EDGE_CURVE('',#21543,#21542,#3203,.T.);
#26603=EDGE_CURVE('',#21544,#21543,#3204,.T.);
#26604=EDGE_CURVE('',#21545,#21544,#3205,.T.);
#26605=EDGE_CURVE('',#21546,#21545,#3206,.T.);
#26606=EDGE_CURVE('',#21547,#21546,#3207,.T.);
#26607=EDGE_CURVE('',#21548,#21547,#3208,.T.);
#26608=EDGE_CURVE('',#21549,#21548,#3209,.T.);
#26609=EDGE_CURVE('',#21550,#21549,#3210,.T.);
#26610=EDGE_CURVE('',#21551,#21550,#3211,.T.);
#26611=EDGE_CURVE('',#20343,#21551,#3212,.T.);
#26612=EDGE_CURVE('',#20340,#21552,#3213,.T.);
#26613=EDGE_CURVE('',#21552,#21553,#3214,.T.);
#26614=EDGE_CURVE('',#21554,#21553,#18869,.T.);
#26615=EDGE_CURVE('',#21555,#21554,#1319,.T.);
#26616=EDGE_CURVE('',#21522,#21555,#3215,.T.);
#26617=EDGE_CURVE('',#21556,#20338,#3216,.T.);
#26618=EDGE_CURVE('',#21557,#21556,#3217,.T.);
#26619=EDGE_CURVE('',#21558,#21557,#3218,.T.);
#26620=EDGE_CURVE('',#21559,#21558,#3219,.T.);
#26621=EDGE_CURVE('',#21560,#21559,#3220,.T.);
#26622=EDGE_CURVE('',#21561,#21560,#3221,.T.);
#26623=EDGE_CURVE('',#21562,#21561,#3222,.T.);
#26624=EDGE_CURVE('',#21563,#21562,#3223,.T.);
#26625=EDGE_CURVE('',#21564,#21563,#3224,.T.);
#26626=EDGE_CURVE('',#21565,#21564,#3225,.T.);
#26627=EDGE_CURVE('',#21566,#21565,#3226,.T.);
#26628=EDGE_CURVE('',#21567,#21566,#3227,.T.);
#26629=EDGE_CURVE('',#21568,#21567,#3228,.T.);
#26630=EDGE_CURVE('',#21569,#21568,#3229,.T.);
#26631=EDGE_CURVE('',#21570,#21569,#3230,.T.);
#26632=EDGE_CURVE('',#21570,#21571,#18870,.T.);
#26633=EDGE_CURVE('',#21572,#21571,#3231,.T.);
#26634=EDGE_CURVE('',#21573,#21572,#3232,.T.);
#26635=EDGE_CURVE('',#21574,#21573,#3233,.T.);
#26636=EDGE_CURVE('',#21575,#21574,#3234,.T.);
#26637=EDGE_CURVE('',#21576,#21575,#3235,.T.);
#26638=EDGE_CURVE('',#21577,#21576,#3236,.T.);
#26639=EDGE_CURVE('',#21578,#21577,#3237,.T.);
#26640=EDGE_CURVE('',#21579,#21578,#3238,.T.);
#26641=EDGE_CURVE('',#21580,#21579,#3239,.T.);
#26642=EDGE_CURVE('',#21581,#21580,#3240,.T.);
#26643=EDGE_CURVE('',#21582,#21581,#3241,.T.);
#26644=EDGE_CURVE('',#21583,#21582,#3242,.T.);
#26645=EDGE_CURVE('',#21584,#21583,#3243,.T.);
#26646=EDGE_CURVE('',#21585,#21584,#3244,.T.);
#26647=EDGE_CURVE('',#20339,#21585,#3245,.T.);
#26648=EDGE_CURVE('',#20336,#21586,#3246,.T.);
#26649=EDGE_CURVE('',#21586,#21587,#3247,.T.);
#26650=EDGE_CURVE('',#21588,#21587,#18871,.T.);
#26651=EDGE_CURVE('',#21589,#21588,#1320,.T.);
#26652=EDGE_CURVE('',#21556,#21589,#3248,.T.);
#26653=EDGE_CURVE('',#21590,#20334,#3249,.T.);
#26654=EDGE_CURVE('',#21591,#21590,#3250,.T.);
#26655=EDGE_CURVE('',#21592,#21591,#3251,.T.);
#26656=EDGE_CURVE('',#21593,#21592,#3252,.T.);
#26657=EDGE_CURVE('',#21594,#21593,#3253,.T.);
#26658=EDGE_CURVE('',#21595,#21594,#3254,.T.);
#26659=EDGE_CURVE('',#21596,#21595,#3255,.T.);
#26660=EDGE_CURVE('',#21597,#21596,#3256,.T.);
#26661=EDGE_CURVE('',#21598,#21597,#3257,.T.);
#26662=EDGE_CURVE('',#21599,#21598,#3258,.T.);
#26663=EDGE_CURVE('',#21600,#21599,#3259,.T.);
#26664=EDGE_CURVE('',#21601,#21600,#3260,.T.);
#26665=EDGE_CURVE('',#21602,#21601,#3261,.T.);
#26666=EDGE_CURVE('',#21603,#21602,#3262,.T.);
#26667=EDGE_CURVE('',#21604,#21603,#3263,.T.);
#26668=EDGE_CURVE('',#21604,#21605,#18872,.T.);
#26669=EDGE_CURVE('',#21606,#21605,#3264,.T.);
#26670=EDGE_CURVE('',#21607,#21606,#3265,.T.);
#26671=EDGE_CURVE('',#21608,#21607,#3266,.T.);
#26672=EDGE_CURVE('',#21609,#21608,#3267,.T.);
#26673=EDGE_CURVE('',#21610,#21609,#3268,.T.);
#26674=EDGE_CURVE('',#21611,#21610,#3269,.T.);
#26675=EDGE_CURVE('',#21612,#21611,#3270,.T.);
#26676=EDGE_CURVE('',#21613,#21612,#3271,.T.);
#26677=EDGE_CURVE('',#21614,#21613,#3272,.T.);
#26678=EDGE_CURVE('',#21615,#21614,#3273,.T.);
#26679=EDGE_CURVE('',#21616,#21615,#3274,.T.);
#26680=EDGE_CURVE('',#21617,#21616,#3275,.T.);
#26681=EDGE_CURVE('',#21618,#21617,#3276,.T.);
#26682=EDGE_CURVE('',#21619,#21618,#3277,.T.);
#26683=EDGE_CURVE('',#20335,#21619,#3278,.T.);
#26684=EDGE_CURVE('',#20332,#21620,#3279,.T.);
#26685=EDGE_CURVE('',#21620,#21621,#3280,.T.);
#26686=EDGE_CURVE('',#21622,#21621,#18873,.T.);
#26687=EDGE_CURVE('',#21623,#21622,#1321,.T.);
#26688=EDGE_CURVE('',#21590,#21623,#3281,.T.);
#26689=EDGE_CURVE('',#21624,#20330,#3282,.T.);
#26690=EDGE_CURVE('',#21625,#21624,#3283,.T.);
#26691=EDGE_CURVE('',#21626,#21625,#3284,.T.);
#26692=EDGE_CURVE('',#21627,#21626,#3285,.T.);
#26693=EDGE_CURVE('',#21628,#21627,#3286,.T.);
#26694=EDGE_CURVE('',#21629,#21628,#3287,.T.);
#26695=EDGE_CURVE('',#21630,#21629,#3288,.T.);
#26696=EDGE_CURVE('',#21631,#21630,#3289,.T.);
#26697=EDGE_CURVE('',#21632,#21631,#3290,.T.);
#26698=EDGE_CURVE('',#21633,#21632,#3291,.T.);
#26699=EDGE_CURVE('',#21634,#21633,#3292,.T.);
#26700=EDGE_CURVE('',#21635,#21634,#3293,.T.);
#26701=EDGE_CURVE('',#21636,#21635,#3294,.T.);
#26702=EDGE_CURVE('',#21637,#21636,#3295,.T.);
#26703=EDGE_CURVE('',#21638,#21637,#3296,.T.);
#26704=EDGE_CURVE('',#21638,#21639,#18874,.T.);
#26705=EDGE_CURVE('',#21640,#21639,#3297,.T.);
#26706=EDGE_CURVE('',#21641,#21640,#3298,.T.);
#26707=EDGE_CURVE('',#21642,#21641,#3299,.T.);
#26708=EDGE_CURVE('',#21643,#21642,#3300,.T.);
#26709=EDGE_CURVE('',#21644,#21643,#3301,.T.);
#26710=EDGE_CURVE('',#21645,#21644,#3302,.T.);
#26711=EDGE_CURVE('',#21646,#21645,#3303,.T.);
#26712=EDGE_CURVE('',#21647,#21646,#3304,.T.);
#26713=EDGE_CURVE('',#21648,#21647,#3305,.T.);
#26714=EDGE_CURVE('',#21649,#21648,#3306,.T.);
#26715=EDGE_CURVE('',#21650,#21649,#3307,.T.);
#26716=EDGE_CURVE('',#21651,#21650,#3308,.T.);
#26717=EDGE_CURVE('',#21652,#21651,#3309,.T.);
#26718=EDGE_CURVE('',#21653,#21652,#3310,.T.);
#26719=EDGE_CURVE('',#20331,#21653,#3311,.T.);
#26720=EDGE_CURVE('',#20328,#21654,#3312,.T.);
#26721=EDGE_CURVE('',#21654,#21655,#3313,.T.);
#26722=EDGE_CURVE('',#21656,#21655,#18875,.T.);
#26723=EDGE_CURVE('',#21657,#21656,#1322,.T.);
#26724=EDGE_CURVE('',#21624,#21657,#3314,.T.);
#26725=EDGE_CURVE('',#21658,#20326,#3315,.T.);
#26726=EDGE_CURVE('',#21659,#21658,#3316,.T.);
#26727=EDGE_CURVE('',#21660,#21659,#3317,.T.);
#26728=EDGE_CURVE('',#21661,#21660,#3318,.T.);
#26729=EDGE_CURVE('',#21662,#21661,#3319,.T.);
#26730=EDGE_CURVE('',#21663,#21662,#3320,.T.);
#26731=EDGE_CURVE('',#21664,#21663,#3321,.T.);
#26732=EDGE_CURVE('',#21665,#21664,#3322,.T.);
#26733=EDGE_CURVE('',#21666,#21665,#3323,.T.);
#26734=EDGE_CURVE('',#21667,#21666,#3324,.T.);
#26735=EDGE_CURVE('',#21668,#21667,#3325,.T.);
#26736=EDGE_CURVE('',#21669,#21668,#3326,.T.);
#26737=EDGE_CURVE('',#21670,#21669,#3327,.T.);
#26738=EDGE_CURVE('',#21671,#21670,#3328,.T.);
#26739=EDGE_CURVE('',#21672,#21671,#3329,.T.);
#26740=EDGE_CURVE('',#21672,#21673,#18876,.T.);
#26741=EDGE_CURVE('',#21674,#21673,#3330,.T.);
#26742=EDGE_CURVE('',#21675,#21674,#3331,.T.);
#26743=EDGE_CURVE('',#21676,#21675,#3332,.T.);
#26744=EDGE_CURVE('',#21677,#21676,#3333,.T.);
#26745=EDGE_CURVE('',#21678,#21677,#3334,.T.);
#26746=EDGE_CURVE('',#21679,#21678,#3335,.T.);
#26747=EDGE_CURVE('',#21680,#21679,#3336,.T.);
#26748=EDGE_CURVE('',#21681,#21680,#3337,.T.);
#26749=EDGE_CURVE('',#21682,#21681,#3338,.T.);
#26750=EDGE_CURVE('',#21683,#21682,#3339,.T.);
#26751=EDGE_CURVE('',#21684,#21683,#3340,.T.);
#26752=EDGE_CURVE('',#21685,#21684,#3341,.T.);
#26753=EDGE_CURVE('',#21686,#21685,#3342,.T.);
#26754=EDGE_CURVE('',#21687,#21686,#3343,.T.);
#26755=EDGE_CURVE('',#20327,#21687,#3344,.T.);
#26756=EDGE_CURVE('',#20324,#21688,#3345,.T.);
#26757=EDGE_CURVE('',#21688,#21689,#3346,.T.);
#26758=EDGE_CURVE('',#21690,#21689,#18877,.T.);
#26759=EDGE_CURVE('',#21691,#21690,#1323,.T.);
#26760=EDGE_CURVE('',#21658,#21691,#3347,.T.);
#26761=EDGE_CURVE('',#21692,#21693,#19610,.T.);
#26762=EDGE_CURVE('',#21673,#21692,#18878,.T.);
#26763=EDGE_CURVE('',#21693,#21672,#18879,.T.);
#26764=EDGE_CURVE('',#21694,#21695,#19611,.T.);
#26765=EDGE_CURVE('',#21639,#21694,#18880,.T.);
#26766=EDGE_CURVE('',#21695,#21638,#18881,.T.);
#26767=EDGE_CURVE('',#21696,#21697,#19612,.T.);
#26768=EDGE_CURVE('',#21605,#21696,#18882,.T.);
#26769=EDGE_CURVE('',#21697,#21604,#18883,.T.);
#26770=EDGE_CURVE('',#21698,#21699,#19613,.T.);
#26771=EDGE_CURVE('',#21571,#21698,#18884,.T.);
#26772=EDGE_CURVE('',#21699,#21570,#18885,.T.);
#26773=EDGE_CURVE('',#21700,#21701,#19614,.T.);
#26774=EDGE_CURVE('',#21537,#21700,#18886,.T.);
#26775=EDGE_CURVE('',#21701,#21536,#18887,.T.);
#26776=EDGE_CURVE('',#21702,#21703,#19615,.T.);
#26777=EDGE_CURVE('',#21503,#21702,#18888,.T.);
#26778=EDGE_CURVE('',#21703,#21502,#18889,.T.);
#26779=EDGE_CURVE('',#21704,#21705,#19616,.T.);
#26780=EDGE_CURVE('',#21469,#21704,#18890,.T.);
#26781=EDGE_CURVE('',#21705,#21468,#18891,.T.);
#26782=EDGE_CURVE('',#21706,#21707,#19617,.T.);
#26783=EDGE_CURVE('',#21435,#21706,#18892,.T.);
#26784=EDGE_CURVE('',#21707,#21434,#18893,.T.);
#26785=EDGE_CURVE('',#21708,#21709,#19618,.T.);
#26786=EDGE_CURVE('',#21401,#21708,#18894,.T.);
#26787=EDGE_CURVE('',#21709,#21400,#18895,.T.);
#26788=EDGE_CURVE('',#21710,#21711,#19619,.T.);
#26789=EDGE_CURVE('',#21367,#21710,#18896,.T.);
#26790=EDGE_CURVE('',#21711,#21366,#18897,.T.);
#26791=EDGE_CURVE('',#21712,#21713,#19620,.T.);
#26792=EDGE_CURVE('',#21333,#21712,#18898,.T.);
#26793=EDGE_CURVE('',#21713,#21332,#18899,.T.);
#26794=EDGE_CURVE('',#21714,#21715,#19621,.T.);
#26795=EDGE_CURVE('',#21299,#21714,#18900,.T.);
#26796=EDGE_CURVE('',#21715,#21298,#18901,.T.);
#26797=EDGE_CURVE('',#21716,#21717,#19622,.T.);
#26798=EDGE_CURVE('',#21265,#21716,#18902,.T.);
#26799=EDGE_CURVE('',#21717,#21264,#18903,.T.);
#26800=EDGE_CURVE('',#21718,#21719,#19623,.T.);
#26801=EDGE_CURVE('',#21231,#21718,#18904,.T.);
#26802=EDGE_CURVE('',#21719,#21230,#18905,.T.);
#26803=EDGE_CURVE('',#21720,#21721,#19624,.T.);
#26804=EDGE_CURVE('',#21197,#21720,#18906,.T.);
#26805=EDGE_CURVE('',#21721,#21196,#18907,.T.);
#26806=EDGE_CURVE('',#21722,#21723,#19625,.T.);
#26807=EDGE_CURVE('',#21163,#21722,#18908,.T.);
#26808=EDGE_CURVE('',#21723,#21162,#18909,.T.);
#26809=EDGE_CURVE('',#21724,#21725,#19626,.T.);
#26810=EDGE_CURVE('',#21129,#21724,#18910,.T.);
#26811=EDGE_CURVE('',#21725,#21128,#18911,.T.);
#26812=EDGE_CURVE('',#21726,#21727,#19627,.T.);
#26813=EDGE_CURVE('',#21095,#21726,#18912,.T.);
#26814=EDGE_CURVE('',#21727,#21094,#18913,.T.);
#26815=EDGE_CURVE('',#21728,#21729,#19628,.T.);
#26816=EDGE_CURVE('',#21061,#21728,#18914,.T.);
#26817=EDGE_CURVE('',#21729,#21060,#18915,.T.);
#26818=EDGE_CURVE('',#21730,#21731,#19629,.T.);
#26819=EDGE_CURVE('',#21027,#21730,#18916,.T.);
#26820=EDGE_CURVE('',#21731,#21026,#18917,.T.);
#26821=EDGE_CURVE('',#21732,#21733,#19630,.T.);
#26822=EDGE_CURVE('',#20993,#21732,#18918,.T.);
#26823=EDGE_CURVE('',#21733,#20992,#18919,.T.);
#26824=EDGE_CURVE('',#21734,#21735,#19631,.T.);
#26825=EDGE_CURVE('',#20959,#21734,#18920,.T.);
#26826=EDGE_CURVE('',#21735,#20958,#18921,.T.);
#26827=EDGE_CURVE('',#21736,#21737,#19632,.T.);
#26828=EDGE_CURVE('',#20925,#21736,#18922,.T.);
#26829=EDGE_CURVE('',#21737,#20924,#18923,.T.);
#26830=EDGE_CURVE('',#21738,#21739,#19633,.T.);
#26831=EDGE_CURVE('',#20891,#21738,#18924,.T.);
#26832=EDGE_CURVE('',#21739,#20890,#18925,.T.);
#26833=EDGE_CURVE('',#21740,#21741,#19634,.T.);
#26834=EDGE_CURVE('',#20857,#21740,#18926,.T.);
#26835=EDGE_CURVE('',#21741,#20856,#18927,.T.);
#26836=EDGE_CURVE('',#21742,#21743,#19635,.T.);
#26837=EDGE_CURVE('',#20823,#21742,#18928,.T.);
#26838=EDGE_CURVE('',#21743,#20822,#18929,.T.);
#26839=EDGE_CURVE('',#21744,#21745,#19636,.T.);
#26840=EDGE_CURVE('',#20789,#21744,#18930,.T.);
#26841=EDGE_CURVE('',#21745,#20788,#18931,.T.);
#26842=EDGE_CURVE('',#21746,#21747,#19637,.T.);
#26843=EDGE_CURVE('',#20755,#21746,#18932,.T.);
#26844=EDGE_CURVE('',#21747,#20754,#18933,.T.);
#26845=EDGE_CURVE('',#21748,#21749,#19638,.T.);
#26846=EDGE_CURVE('',#20721,#21748,#18934,.T.);
#26847=EDGE_CURVE('',#21749,#20720,#18935,.T.);
#26848=EDGE_CURVE('',#21750,#21751,#19639,.T.);
#26849=EDGE_CURVE('',#20687,#21750,#18936,.T.);
#26850=EDGE_CURVE('',#21751,#20686,#18937,.T.);
#26851=EDGE_CURVE('',#21752,#21753,#19640,.T.);
#26852=EDGE_CURVE('',#20653,#21752,#18938,.T.);
#26853=EDGE_CURVE('',#21753,#20652,#18939,.T.);
#26854=EDGE_CURVE('',#21754,#21755,#19641,.T.);
#26855=EDGE_CURVE('',#20619,#21754,#18940,.T.);
#26856=EDGE_CURVE('',#21755,#20618,#18941,.T.);
#26857=EDGE_CURVE('',#21756,#21757,#19642,.T.);
#26858=EDGE_CURVE('',#20585,#21756,#18942,.T.);
#26859=EDGE_CURVE('',#21757,#20584,#18943,.T.);
#26860=EDGE_CURVE('',#21758,#21759,#19643,.T.);
#26861=EDGE_CURVE('',#20551,#21758,#18944,.T.);
#26862=EDGE_CURVE('',#21759,#20550,#18945,.T.);
#26863=EDGE_CURVE('',#21760,#21761,#19644,.T.);
#26864=EDGE_CURVE('',#20517,#21760,#18946,.T.);
#26865=EDGE_CURVE('',#21761,#20516,#18947,.T.);
#26866=EDGE_CURVE('',#21762,#21763,#19645,.T.);
#26867=EDGE_CURVE('',#20483,#21762,#18948,.T.);
#26868=EDGE_CURVE('',#21763,#20482,#18949,.T.);
#26869=EDGE_CURVE('',#21762,#21764,#3348,.T.);
#26870=EDGE_CURVE('',#21764,#21765,#3349,.T.);
#26871=EDGE_CURVE('',#21766,#21765,#18950,.T.);
#26872=EDGE_CURVE('',#21767,#21766,#1324,.T.);
#26873=EDGE_CURVE('',#20484,#21767,#3350,.T.);
#26874=EDGE_CURVE('',#21760,#21768,#3351,.T.);
#26875=EDGE_CURVE('',#21768,#21769,#3352,.T.);
#26876=EDGE_CURVE('',#21770,#21769,#18951,.T.);
#26877=EDGE_CURVE('',#21771,#21770,#1325,.T.);
#26878=EDGE_CURVE('',#20518,#21771,#3353,.T.);
#26879=EDGE_CURVE('',#21758,#21772,#3354,.T.);
#26880=EDGE_CURVE('',#21772,#21773,#3355,.T.);
#26881=EDGE_CURVE('',#21774,#21773,#18952,.T.);
#26882=EDGE_CURVE('',#21775,#21774,#1326,.T.);
#26883=EDGE_CURVE('',#20552,#21775,#3356,.T.);
#26884=EDGE_CURVE('',#21756,#21776,#3357,.T.);
#26885=EDGE_CURVE('',#21776,#21777,#3358,.T.);
#26886=EDGE_CURVE('',#21778,#21777,#18953,.T.);
#26887=EDGE_CURVE('',#21779,#21778,#1327,.T.);
#26888=EDGE_CURVE('',#20586,#21779,#3359,.T.);
#26889=EDGE_CURVE('',#21754,#21780,#3360,.T.);
#26890=EDGE_CURVE('',#21780,#21781,#3361,.T.);
#26891=EDGE_CURVE('',#21782,#21781,#18954,.T.);
#26892=EDGE_CURVE('',#21783,#21782,#1328,.T.);
#26893=EDGE_CURVE('',#20620,#21783,#3362,.T.);
#26894=EDGE_CURVE('',#21752,#21784,#3363,.T.);
#26895=EDGE_CURVE('',#21784,#21785,#3364,.T.);
#26896=EDGE_CURVE('',#21786,#21785,#18955,.T.);
#26897=EDGE_CURVE('',#21787,#21786,#1329,.T.);
#26898=EDGE_CURVE('',#20654,#21787,#3365,.T.);
#26899=EDGE_CURVE('',#21750,#21788,#3366,.T.);
#26900=EDGE_CURVE('',#21788,#21789,#3367,.T.);
#26901=EDGE_CURVE('',#21790,#21789,#18956,.T.);
#26902=EDGE_CURVE('',#21791,#21790,#1330,.T.);
#26903=EDGE_CURVE('',#20688,#21791,#3368,.T.);
#26904=EDGE_CURVE('',#21748,#21792,#3369,.T.);
#26905=EDGE_CURVE('',#21792,#21793,#3370,.T.);
#26906=EDGE_CURVE('',#21794,#21793,#18957,.T.);
#26907=EDGE_CURVE('',#21795,#21794,#1331,.T.);
#26908=EDGE_CURVE('',#20722,#21795,#3371,.T.);
#26909=EDGE_CURVE('',#21746,#21796,#3372,.T.);
#26910=EDGE_CURVE('',#21796,#21797,#3373,.T.);
#26911=EDGE_CURVE('',#21798,#21797,#18958,.T.);
#26912=EDGE_CURVE('',#21799,#21798,#1332,.T.);
#26913=EDGE_CURVE('',#20756,#21799,#3374,.T.);
#26914=EDGE_CURVE('',#21744,#21800,#3375,.T.);
#26915=EDGE_CURVE('',#21800,#21801,#3376,.T.);
#26916=EDGE_CURVE('',#21802,#21801,#18959,.T.);
#26917=EDGE_CURVE('',#21803,#21802,#1333,.T.);
#26918=EDGE_CURVE('',#20790,#21803,#3377,.T.);
#26919=EDGE_CURVE('',#21742,#21804,#3378,.T.);
#26920=EDGE_CURVE('',#21804,#21805,#3379,.T.);
#26921=EDGE_CURVE('',#21806,#21805,#18960,.T.);
#26922=EDGE_CURVE('',#21807,#21806,#1334,.T.);
#26923=EDGE_CURVE('',#20824,#21807,#3380,.T.);
#26924=EDGE_CURVE('',#21740,#21808,#3381,.T.);
#26925=EDGE_CURVE('',#21808,#21809,#3382,.T.);
#26926=EDGE_CURVE('',#21810,#21809,#18961,.T.);
#26927=EDGE_CURVE('',#21811,#21810,#1335,.T.);
#26928=EDGE_CURVE('',#20858,#21811,#3383,.T.);
#26929=EDGE_CURVE('',#21738,#21812,#3384,.T.);
#26930=EDGE_CURVE('',#21812,#21813,#3385,.T.);
#26931=EDGE_CURVE('',#21814,#21813,#18962,.T.);
#26932=EDGE_CURVE('',#21815,#21814,#1336,.T.);
#26933=EDGE_CURVE('',#20892,#21815,#3386,.T.);
#26934=EDGE_CURVE('',#21736,#21816,#3387,.T.);
#26935=EDGE_CURVE('',#21816,#21817,#3388,.T.);
#26936=EDGE_CURVE('',#21818,#21817,#18963,.T.);
#26937=EDGE_CURVE('',#21819,#21818,#1337,.T.);
#26938=EDGE_CURVE('',#20926,#21819,#3389,.T.);
#26939=EDGE_CURVE('',#21734,#21820,#3390,.T.);
#26940=EDGE_CURVE('',#21820,#21821,#3391,.T.);
#26941=EDGE_CURVE('',#21822,#21821,#18964,.T.);
#26942=EDGE_CURVE('',#21823,#21822,#1338,.T.);
#26943=EDGE_CURVE('',#20960,#21823,#3392,.T.);
#26944=EDGE_CURVE('',#21732,#21824,#3393,.T.);
#26945=EDGE_CURVE('',#21824,#21825,#3394,.T.);
#26946=EDGE_CURVE('',#21826,#21825,#18965,.T.);
#26947=EDGE_CURVE('',#21827,#21826,#1339,.T.);
#26948=EDGE_CURVE('',#20994,#21827,#3395,.T.);
#26949=EDGE_CURVE('',#21730,#21828,#3396,.T.);
#26950=EDGE_CURVE('',#21828,#21829,#3397,.T.);
#26951=EDGE_CURVE('',#21830,#21829,#18966,.T.);
#26952=EDGE_CURVE('',#21831,#21830,#1340,.T.);
#26953=EDGE_CURVE('',#21028,#21831,#3398,.T.);
#26954=EDGE_CURVE('',#21728,#21832,#3399,.T.);
#26955=EDGE_CURVE('',#21832,#21833,#3400,.T.);
#26956=EDGE_CURVE('',#21834,#21833,#18967,.T.);
#26957=EDGE_CURVE('',#21835,#21834,#1341,.T.);
#26958=EDGE_CURVE('',#21062,#21835,#3401,.T.);
#26959=EDGE_CURVE('',#21726,#21836,#3402,.T.);
#26960=EDGE_CURVE('',#21836,#21837,#3403,.T.);
#26961=EDGE_CURVE('',#21838,#21837,#18968,.T.);
#26962=EDGE_CURVE('',#21839,#21838,#1342,.T.);
#26963=EDGE_CURVE('',#21096,#21839,#3404,.T.);
#26964=EDGE_CURVE('',#21724,#21840,#3405,.T.);
#26965=EDGE_CURVE('',#21840,#21841,#3406,.T.);
#26966=EDGE_CURVE('',#21842,#21841,#18969,.T.);
#26967=EDGE_CURVE('',#21843,#21842,#1343,.T.);
#26968=EDGE_CURVE('',#21130,#21843,#3407,.T.);
#26969=EDGE_CURVE('',#21722,#21844,#3408,.T.);
#26970=EDGE_CURVE('',#21844,#21845,#3409,.T.);
#26971=EDGE_CURVE('',#21846,#21845,#18970,.T.);
#26972=EDGE_CURVE('',#21847,#21846,#1344,.T.);
#26973=EDGE_CURVE('',#21164,#21847,#3410,.T.);
#26974=EDGE_CURVE('',#21720,#21848,#3411,.T.);
#26975=EDGE_CURVE('',#21848,#21849,#3412,.T.);
#26976=EDGE_CURVE('',#21850,#21849,#18971,.T.);
#26977=EDGE_CURVE('',#21851,#21850,#1345,.T.);
#26978=EDGE_CURVE('',#21198,#21851,#3413,.T.);
#26979=EDGE_CURVE('',#21718,#21852,#3414,.T.);
#26980=EDGE_CURVE('',#21852,#21853,#3415,.T.);
#26981=EDGE_CURVE('',#21854,#21853,#18972,.T.);
#26982=EDGE_CURVE('',#21855,#21854,#1346,.T.);
#26983=EDGE_CURVE('',#21232,#21855,#3416,.T.);
#26984=EDGE_CURVE('',#21716,#21856,#3417,.T.);
#26985=EDGE_CURVE('',#21856,#21857,#3418,.T.);
#26986=EDGE_CURVE('',#21858,#21857,#18973,.T.);
#26987=EDGE_CURVE('',#21859,#21858,#1347,.T.);
#26988=EDGE_CURVE('',#21266,#21859,#3419,.T.);
#26989=EDGE_CURVE('',#21714,#21860,#3420,.T.);
#26990=EDGE_CURVE('',#21860,#21861,#3421,.T.);
#26991=EDGE_CURVE('',#21862,#21861,#18974,.T.);
#26992=EDGE_CURVE('',#21863,#21862,#1348,.T.);
#26993=EDGE_CURVE('',#21300,#21863,#3422,.T.);
#26994=EDGE_CURVE('',#21712,#21864,#3423,.T.);
#26995=EDGE_CURVE('',#21864,#21865,#3424,.T.);
#26996=EDGE_CURVE('',#21866,#21865,#18975,.T.);
#26997=EDGE_CURVE('',#21867,#21866,#1349,.T.);
#26998=EDGE_CURVE('',#21334,#21867,#3425,.T.);
#26999=EDGE_CURVE('',#21710,#21868,#3426,.T.);
#27000=EDGE_CURVE('',#21868,#21869,#3427,.T.);
#27001=EDGE_CURVE('',#21870,#21869,#18976,.T.);
#27002=EDGE_CURVE('',#21871,#21870,#1350,.T.);
#27003=EDGE_CURVE('',#21368,#21871,#3428,.T.);
#27004=EDGE_CURVE('',#21708,#21872,#3429,.T.);
#27005=EDGE_CURVE('',#21872,#21873,#3430,.T.);
#27006=EDGE_CURVE('',#21874,#21873,#18977,.T.);
#27007=EDGE_CURVE('',#21875,#21874,#1351,.T.);
#27008=EDGE_CURVE('',#21402,#21875,#3431,.T.);
#27009=EDGE_CURVE('',#21706,#21876,#3432,.T.);
#27010=EDGE_CURVE('',#21876,#21877,#3433,.T.);
#27011=EDGE_CURVE('',#21878,#21877,#18978,.T.);
#27012=EDGE_CURVE('',#21879,#21878,#1352,.T.);
#27013=EDGE_CURVE('',#21436,#21879,#3434,.T.);
#27014=EDGE_CURVE('',#21704,#21880,#3435,.T.);
#27015=EDGE_CURVE('',#21880,#21881,#3436,.T.);
#27016=EDGE_CURVE('',#21882,#21881,#18979,.T.);
#27017=EDGE_CURVE('',#21883,#21882,#1353,.T.);
#27018=EDGE_CURVE('',#21470,#21883,#3437,.T.);
#27019=EDGE_CURVE('',#21702,#21884,#3438,.T.);
#27020=EDGE_CURVE('',#21884,#21885,#3439,.T.);
#27021=EDGE_CURVE('',#21886,#21885,#18980,.T.);
#27022=EDGE_CURVE('',#21887,#21886,#1354,.T.);
#27023=EDGE_CURVE('',#21504,#21887,#3440,.T.);
#27024=EDGE_CURVE('',#21700,#21888,#3441,.T.);
#27025=EDGE_CURVE('',#21888,#21889,#3442,.T.);
#27026=EDGE_CURVE('',#21890,#21889,#18981,.T.);
#27027=EDGE_CURVE('',#21891,#21890,#1355,.T.);
#27028=EDGE_CURVE('',#21538,#21891,#3443,.T.);
#27029=EDGE_CURVE('',#21698,#21892,#3444,.T.);
#27030=EDGE_CURVE('',#21892,#21893,#3445,.T.);
#27031=EDGE_CURVE('',#21894,#21893,#18982,.T.);
#27032=EDGE_CURVE('',#21895,#21894,#1356,.T.);
#27033=EDGE_CURVE('',#21572,#21895,#3446,.T.);
#27034=EDGE_CURVE('',#21696,#21896,#3447,.T.);
#27035=EDGE_CURVE('',#21896,#21897,#3448,.T.);
#27036=EDGE_CURVE('',#21898,#21897,#18983,.T.);
#27037=EDGE_CURVE('',#21899,#21898,#1357,.T.);
#27038=EDGE_CURVE('',#21606,#21899,#3449,.T.);
#27039=EDGE_CURVE('',#21694,#21900,#3450,.T.);
#27040=EDGE_CURVE('',#21900,#21901,#3451,.T.);
#27041=EDGE_CURVE('',#21902,#21901,#18984,.T.);
#27042=EDGE_CURVE('',#21903,#21902,#1358,.T.);
#27043=EDGE_CURVE('',#21640,#21903,#3452,.T.);
#27044=EDGE_CURVE('',#21692,#21904,#3453,.T.);
#27045=EDGE_CURVE('',#21904,#21905,#3454,.T.);
#27046=EDGE_CURVE('',#21906,#21905,#18985,.T.);
#27047=EDGE_CURVE('',#21907,#21906,#1359,.T.);
#27048=EDGE_CURVE('',#21674,#21907,#3455,.T.);
#27049=EDGE_CURVE('',#21908,#20465,#3456,.T.);
#27050=EDGE_CURVE('',#20498,#21908,#3457,.T.);
#27051=EDGE_CURVE('',#21909,#20461,#3458,.T.);
#27052=EDGE_CURVE('',#20532,#21909,#3459,.T.);
#27053=EDGE_CURVE('',#21910,#20457,#3460,.T.);
#27054=EDGE_CURVE('',#20566,#21910,#3461,.T.);
#27055=EDGE_CURVE('',#21911,#20453,#3462,.T.);
#27056=EDGE_CURVE('',#20600,#21911,#3463,.T.);
#27057=EDGE_CURVE('',#21912,#20449,#3464,.T.);
#27058=EDGE_CURVE('',#20634,#21912,#3465,.T.);
#27059=EDGE_CURVE('',#21913,#20445,#3466,.T.);
#27060=EDGE_CURVE('',#20668,#21913,#3467,.T.);
#27061=EDGE_CURVE('',#21914,#20441,#3468,.T.);
#27062=EDGE_CURVE('',#20702,#21914,#3469,.T.);
#27063=EDGE_CURVE('',#21915,#20437,#3470,.T.);
#27064=EDGE_CURVE('',#20736,#21915,#3471,.T.);
#27065=EDGE_CURVE('',#21916,#20433,#3472,.T.);
#27066=EDGE_CURVE('',#20770,#21916,#3473,.T.);
#27067=EDGE_CURVE('',#21917,#20429,#3474,.T.);
#27068=EDGE_CURVE('',#20804,#21917,#3475,.T.);
#27069=EDGE_CURVE('',#21918,#20425,#3476,.T.);
#27070=EDGE_CURVE('',#20838,#21918,#3477,.T.);
#27071=EDGE_CURVE('',#21919,#20421,#3478,.T.);
#27072=EDGE_CURVE('',#20872,#21919,#3479,.T.);
#27073=EDGE_CURVE('',#21920,#20417,#3480,.T.);
#27074=EDGE_CURVE('',#20906,#21920,#3481,.T.);
#27075=EDGE_CURVE('',#21921,#20413,#3482,.T.);
#27076=EDGE_CURVE('',#20940,#21921,#3483,.T.);
#27077=EDGE_CURVE('',#21922,#20409,#3484,.T.);
#27078=EDGE_CURVE('',#20974,#21922,#3485,.T.);
#27079=EDGE_CURVE('',#21923,#20405,#3486,.T.);
#27080=EDGE_CURVE('',#21008,#21923,#3487,.T.);
#27081=EDGE_CURVE('',#21924,#20401,#3488,.T.);
#27082=EDGE_CURVE('',#21042,#21924,#3489,.T.);
#27083=EDGE_CURVE('',#21925,#20397,#3490,.T.);
#27084=EDGE_CURVE('',#21076,#21925,#3491,.T.);
#27085=EDGE_CURVE('',#21926,#20393,#3492,.T.);
#27086=EDGE_CURVE('',#21110,#21926,#3493,.T.);
#27087=EDGE_CURVE('',#21927,#20389,#3494,.T.);
#27088=EDGE_CURVE('',#21144,#21927,#3495,.T.);
#27089=EDGE_CURVE('',#21928,#20385,#3496,.T.);
#27090=EDGE_CURVE('',#21178,#21928,#3497,.T.);
#27091=EDGE_CURVE('',#21929,#20381,#3498,.T.);
#27092=EDGE_CURVE('',#21212,#21929,#3499,.T.);
#27093=EDGE_CURVE('',#21930,#20377,#3500,.T.);
#27094=EDGE_CURVE('',#21246,#21930,#3501,.T.);
#27095=EDGE_CURVE('',#21931,#20373,#3502,.T.);
#27096=EDGE_CURVE('',#21280,#21931,#3503,.T.);
#27097=EDGE_CURVE('',#21932,#20369,#3504,.T.);
#27098=EDGE_CURVE('',#21314,#21932,#3505,.T.);
#27099=EDGE_CURVE('',#21933,#20365,#3506,.T.);
#27100=EDGE_CURVE('',#21348,#21933,#3507,.T.);
#27101=EDGE_CURVE('',#21934,#20361,#3508,.T.);
#27102=EDGE_CURVE('',#21382,#21934,#3509,.T.);
#27103=EDGE_CURVE('',#21935,#20357,#3510,.T.);
#27104=EDGE_CURVE('',#21416,#21935,#3511,.T.);
#27105=EDGE_CURVE('',#21936,#20353,#3512,.T.);
#27106=EDGE_CURVE('',#21450,#21936,#3513,.T.);
#27107=EDGE_CURVE('',#21937,#20349,#3514,.T.);
#27108=EDGE_CURVE('',#21484,#21937,#3515,.T.);
#27109=EDGE_CURVE('',#21938,#20345,#3516,.T.);
#27110=EDGE_CURVE('',#21518,#21938,#3517,.T.);
#27111=EDGE_CURVE('',#21939,#20341,#3518,.T.);
#27112=EDGE_CURVE('',#21552,#21939,#3519,.T.);
#27113=EDGE_CURVE('',#21940,#20337,#3520,.T.);
#27114=EDGE_CURVE('',#21586,#21940,#3521,.T.);
#27115=EDGE_CURVE('',#21941,#20333,#3522,.T.);
#27116=EDGE_CURVE('',#21620,#21941,#3523,.T.);
#27117=EDGE_CURVE('',#21942,#20329,#3524,.T.);
#27118=EDGE_CURVE('',#21654,#21942,#3525,.T.);
#27119=EDGE_CURVE('',#21943,#20325,#3526,.T.);
#27120=EDGE_CURVE('',#21688,#21943,#3527,.T.);
#27121=EDGE_CURVE('',#21687,#21944,#3528,.T.);
#27122=EDGE_CURVE('',#21945,#21944,#1360,.T.);
#27123=EDGE_CURVE('',#21946,#21945,#18986,.T.);
#27124=EDGE_CURVE('',#21946,#21943,#3529,.T.);
#27125=EDGE_CURVE('',#21653,#21947,#3530,.T.);
#27126=EDGE_CURVE('',#21948,#21947,#1361,.T.);
#27127=EDGE_CURVE('',#21949,#21948,#18987,.T.);
#27128=EDGE_CURVE('',#21949,#21942,#3531,.T.);
#27129=EDGE_CURVE('',#21619,#21950,#3532,.T.);
#27130=EDGE_CURVE('',#21951,#21950,#1362,.T.);
#27131=EDGE_CURVE('',#21952,#21951,#18988,.T.);
#27132=EDGE_CURVE('',#21952,#21941,#3533,.T.);
#27133=EDGE_CURVE('',#21585,#21953,#3534,.T.);
#27134=EDGE_CURVE('',#21954,#21953,#1363,.T.);
#27135=EDGE_CURVE('',#21955,#21954,#18989,.T.);
#27136=EDGE_CURVE('',#21955,#21940,#3535,.T.);
#27137=EDGE_CURVE('',#21551,#21956,#3536,.T.);
#27138=EDGE_CURVE('',#21957,#21956,#1364,.T.);
#27139=EDGE_CURVE('',#21958,#21957,#18990,.T.);
#27140=EDGE_CURVE('',#21958,#21939,#3537,.T.);
#27141=EDGE_CURVE('',#21517,#21959,#3538,.T.);
#27142=EDGE_CURVE('',#21960,#21959,#1365,.T.);
#27143=EDGE_CURVE('',#21961,#21960,#18991,.T.);
#27144=EDGE_CURVE('',#21961,#21938,#3539,.T.);
#27145=EDGE_CURVE('',#21483,#21962,#3540,.T.);
#27146=EDGE_CURVE('',#21963,#21962,#1366,.T.);
#27147=EDGE_CURVE('',#21964,#21963,#18992,.T.);
#27148=EDGE_CURVE('',#21964,#21937,#3541,.T.);
#27149=EDGE_CURVE('',#21449,#21965,#3542,.T.);
#27150=EDGE_CURVE('',#21966,#21965,#1367,.T.);
#27151=EDGE_CURVE('',#21967,#21966,#18993,.T.);
#27152=EDGE_CURVE('',#21967,#21936,#3543,.T.);
#27153=EDGE_CURVE('',#21415,#21968,#3544,.T.);
#27154=EDGE_CURVE('',#21969,#21968,#1368,.T.);
#27155=EDGE_CURVE('',#21970,#21969,#18994,.T.);
#27156=EDGE_CURVE('',#21970,#21935,#3545,.T.);
#27157=EDGE_CURVE('',#21381,#21971,#3546,.T.);
#27158=EDGE_CURVE('',#21972,#21971,#1369,.T.);
#27159=EDGE_CURVE('',#21973,#21972,#18995,.T.);
#27160=EDGE_CURVE('',#21973,#21934,#3547,.T.);
#27161=EDGE_CURVE('',#21347,#21974,#3548,.T.);
#27162=EDGE_CURVE('',#21975,#21974,#1370,.T.);
#27163=EDGE_CURVE('',#21976,#21975,#18996,.T.);
#27164=EDGE_CURVE('',#21976,#21933,#3549,.T.);
#27165=EDGE_CURVE('',#21313,#21977,#3550,.T.);
#27166=EDGE_CURVE('',#21978,#21977,#1371,.T.);
#27167=EDGE_CURVE('',#21979,#21978,#18997,.T.);
#27168=EDGE_CURVE('',#21979,#21932,#3551,.T.);
#27169=EDGE_CURVE('',#21279,#21980,#3552,.T.);
#27170=EDGE_CURVE('',#21981,#21980,#1372,.T.);
#27171=EDGE_CURVE('',#21982,#21981,#18998,.T.);
#27172=EDGE_CURVE('',#21982,#21931,#3553,.T.);
#27173=EDGE_CURVE('',#21245,#21983,#3554,.T.);
#27174=EDGE_CURVE('',#21984,#21983,#1373,.T.);
#27175=EDGE_CURVE('',#21985,#21984,#18999,.T.);
#27176=EDGE_CURVE('',#21985,#21930,#3555,.T.);
#27177=EDGE_CURVE('',#21211,#21986,#3556,.T.);
#27178=EDGE_CURVE('',#21987,#21986,#1374,.T.);
#27179=EDGE_CURVE('',#21988,#21987,#19000,.T.);
#27180=EDGE_CURVE('',#21988,#21929,#3557,.T.);
#27181=EDGE_CURVE('',#21177,#21989,#3558,.T.);
#27182=EDGE_CURVE('',#21990,#21989,#1375,.T.);
#27183=EDGE_CURVE('',#21991,#21990,#19001,.T.);
#27184=EDGE_CURVE('',#21991,#21928,#3559,.T.);
#27185=EDGE_CURVE('',#21143,#21992,#3560,.T.);
#27186=EDGE_CURVE('',#21993,#21992,#1376,.T.);
#27187=EDGE_CURVE('',#21994,#21993,#19002,.T.);
#27188=EDGE_CURVE('',#21994,#21927,#3561,.T.);
#27189=EDGE_CURVE('',#21109,#21995,#3562,.T.);
#27190=EDGE_CURVE('',#21996,#21995,#1377,.T.);
#27191=EDGE_CURVE('',#21997,#21996,#19003,.T.);
#27192=EDGE_CURVE('',#21997,#21926,#3563,.T.);
#27193=EDGE_CURVE('',#21075,#21998,#3564,.T.);
#27194=EDGE_CURVE('',#21999,#21998,#1378,.T.);
#27195=EDGE_CURVE('',#22000,#21999,#19004,.T.);
#27196=EDGE_CURVE('',#22000,#21925,#3565,.T.);
#27197=EDGE_CURVE('',#21041,#22001,#3566,.T.);
#27198=EDGE_CURVE('',#22002,#22001,#1379,.T.);
#27199=EDGE_CURVE('',#22003,#22002,#19005,.T.);
#27200=EDGE_CURVE('',#22003,#21924,#3567,.T.);
#27201=EDGE_CURVE('',#21007,#22004,#3568,.T.);
#27202=EDGE_CURVE('',#22005,#22004,#1380,.T.);
#27203=EDGE_CURVE('',#22006,#22005,#19006,.T.);
#27204=EDGE_CURVE('',#22006,#21923,#3569,.T.);
#27205=EDGE_CURVE('',#20973,#22007,#3570,.T.);
#27206=EDGE_CURVE('',#22008,#22007,#1381,.T.);
#27207=EDGE_CURVE('',#22009,#22008,#19007,.T.);
#27208=EDGE_CURVE('',#22009,#21922,#3571,.T.);
#27209=EDGE_CURVE('',#20939,#22010,#3572,.T.);
#27210=EDGE_CURVE('',#22011,#22010,#1382,.T.);
#27211=EDGE_CURVE('',#22012,#22011,#19008,.T.);
#27212=EDGE_CURVE('',#22012,#21921,#3573,.T.);
#27213=EDGE_CURVE('',#20905,#22013,#3574,.T.);
#27214=EDGE_CURVE('',#22014,#22013,#1383,.T.);
#27215=EDGE_CURVE('',#22015,#22014,#19009,.T.);
#27216=EDGE_CURVE('',#22015,#21920,#3575,.T.);
#27217=EDGE_CURVE('',#20871,#22016,#3576,.T.);
#27218=EDGE_CURVE('',#22017,#22016,#1384,.T.);
#27219=EDGE_CURVE('',#22018,#22017,#19010,.T.);
#27220=EDGE_CURVE('',#22018,#21919,#3577,.T.);
#27221=EDGE_CURVE('',#20837,#22019,#3578,.T.);
#27222=EDGE_CURVE('',#22020,#22019,#1385,.T.);
#27223=EDGE_CURVE('',#22021,#22020,#19011,.T.);
#27224=EDGE_CURVE('',#22021,#21918,#3579,.T.);
#27225=EDGE_CURVE('',#20803,#22022,#3580,.T.);
#27226=EDGE_CURVE('',#22023,#22022,#1386,.T.);
#27227=EDGE_CURVE('',#22024,#22023,#19012,.T.);
#27228=EDGE_CURVE('',#22024,#21917,#3581,.T.);
#27229=EDGE_CURVE('',#20769,#22025,#3582,.T.);
#27230=EDGE_CURVE('',#22026,#22025,#1387,.T.);
#27231=EDGE_CURVE('',#22027,#22026,#19013,.T.);
#27232=EDGE_CURVE('',#22027,#21916,#3583,.T.);
#27233=EDGE_CURVE('',#20735,#22028,#3584,.T.);
#27234=EDGE_CURVE('',#22029,#22028,#1388,.T.);
#27235=EDGE_CURVE('',#22030,#22029,#19014,.T.);
#27236=EDGE_CURVE('',#22030,#21915,#3585,.T.);
#27237=EDGE_CURVE('',#20701,#22031,#3586,.T.);
#27238=EDGE_CURVE('',#22032,#22031,#1389,.T.);
#27239=EDGE_CURVE('',#22033,#22032,#19015,.T.);
#27240=EDGE_CURVE('',#22033,#21914,#3587,.T.);
#27241=EDGE_CURVE('',#20667,#22034,#3588,.T.);
#27242=EDGE_CURVE('',#22035,#22034,#1390,.T.);
#27243=EDGE_CURVE('',#22036,#22035,#19016,.T.);
#27244=EDGE_CURVE('',#22036,#21913,#3589,.T.);
#27245=EDGE_CURVE('',#20633,#22037,#3590,.T.);
#27246=EDGE_CURVE('',#22038,#22037,#1391,.T.);
#27247=EDGE_CURVE('',#22039,#22038,#19017,.T.);
#27248=EDGE_CURVE('',#22039,#21912,#3591,.T.);
#27249=EDGE_CURVE('',#20599,#22040,#3592,.T.);
#27250=EDGE_CURVE('',#22041,#22040,#1392,.T.);
#27251=EDGE_CURVE('',#22042,#22041,#19018,.T.);
#27252=EDGE_CURVE('',#22042,#21911,#3593,.T.);
#27253=EDGE_CURVE('',#20565,#22043,#3594,.T.);
#27254=EDGE_CURVE('',#22044,#22043,#1393,.T.);
#27255=EDGE_CURVE('',#22045,#22044,#19019,.T.);
#27256=EDGE_CURVE('',#22045,#21910,#3595,.T.);
#27257=EDGE_CURVE('',#20531,#22046,#3596,.T.);
#27258=EDGE_CURVE('',#22047,#22046,#1394,.T.);
#27259=EDGE_CURVE('',#22048,#22047,#19020,.T.);
#27260=EDGE_CURVE('',#22048,#21909,#3597,.T.);
#27261=EDGE_CURVE('',#22049,#21908,#3598,.T.);
#27262=EDGE_CURVE('',#20499,#22049,#19021,.T.);
#27263=EDGE_CURVE('',#22050,#21763,#3599,.T.);
#27264=EDGE_CURVE('',#21764,#22050,#3600,.T.);
#27265=EDGE_CURVE('',#22051,#21761,#3601,.T.);
#27266=EDGE_CURVE('',#21768,#22051,#3602,.T.);
#27267=EDGE_CURVE('',#22052,#21759,#3603,.T.);
#27268=EDGE_CURVE('',#21772,#22052,#3604,.T.);
#27269=EDGE_CURVE('',#22053,#21757,#3605,.T.);
#27270=EDGE_CURVE('',#21776,#22053,#3606,.T.);
#27271=EDGE_CURVE('',#22054,#21755,#3607,.T.);
#27272=EDGE_CURVE('',#21780,#22054,#3608,.T.);
#27273=EDGE_CURVE('',#22055,#21753,#3609,.T.);
#27274=EDGE_CURVE('',#21784,#22055,#3610,.T.);
#27275=EDGE_CURVE('',#22056,#21751,#3611,.T.);
#27276=EDGE_CURVE('',#21788,#22056,#3612,.T.);
#27277=EDGE_CURVE('',#22057,#21749,#3613,.T.);
#27278=EDGE_CURVE('',#21792,#22057,#3614,.T.);
#27279=EDGE_CURVE('',#22058,#21747,#3615,.T.);
#27280=EDGE_CURVE('',#21796,#22058,#3616,.T.);
#27281=EDGE_CURVE('',#22059,#21745,#3617,.T.);
#27282=EDGE_CURVE('',#21800,#22059,#3618,.T.);
#27283=EDGE_CURVE('',#22060,#21743,#3619,.T.);
#27284=EDGE_CURVE('',#21804,#22060,#3620,.T.);
#27285=EDGE_CURVE('',#22061,#21741,#3621,.T.);
#27286=EDGE_CURVE('',#21808,#22061,#3622,.T.);
#27287=EDGE_CURVE('',#22062,#21739,#3623,.T.);
#27288=EDGE_CURVE('',#21812,#22062,#3624,.T.);
#27289=EDGE_CURVE('',#22063,#21737,#3625,.T.);
#27290=EDGE_CURVE('',#21816,#22063,#3626,.T.);
#27291=EDGE_CURVE('',#22064,#21735,#3627,.T.);
#27292=EDGE_CURVE('',#21820,#22064,#3628,.T.);
#27293=EDGE_CURVE('',#22065,#21733,#3629,.T.);
#27294=EDGE_CURVE('',#21824,#22065,#3630,.T.);
#27295=EDGE_CURVE('',#22066,#21731,#3631,.T.);
#27296=EDGE_CURVE('',#21828,#22066,#3632,.T.);
#27297=EDGE_CURVE('',#22067,#21729,#3633,.T.);
#27298=EDGE_CURVE('',#21832,#22067,#3634,.T.);
#27299=EDGE_CURVE('',#22068,#21727,#3635,.T.);
#27300=EDGE_CURVE('',#21836,#22068,#3636,.T.);
#27301=EDGE_CURVE('',#22069,#21725,#3637,.T.);
#27302=EDGE_CURVE('',#21840,#22069,#3638,.T.);
#27303=EDGE_CURVE('',#22070,#21723,#3639,.T.);
#27304=EDGE_CURVE('',#21844,#22070,#3640,.T.);
#27305=EDGE_CURVE('',#22071,#21721,#3641,.T.);
#27306=EDGE_CURVE('',#21848,#22071,#3642,.T.);
#27307=EDGE_CURVE('',#22072,#21719,#3643,.T.);
#27308=EDGE_CURVE('',#21852,#22072,#3644,.T.);
#27309=EDGE_CURVE('',#22073,#21717,#3645,.T.);
#27310=EDGE_CURVE('',#21856,#22073,#3646,.T.);
#27311=EDGE_CURVE('',#22074,#21715,#3647,.T.);
#27312=EDGE_CURVE('',#21860,#22074,#3648,.T.);
#27313=EDGE_CURVE('',#22075,#21713,#3649,.T.);
#27314=EDGE_CURVE('',#21864,#22075,#3650,.T.);
#27315=EDGE_CURVE('',#22076,#21711,#3651,.T.);
#27316=EDGE_CURVE('',#21868,#22076,#3652,.T.);
#27317=EDGE_CURVE('',#22077,#21709,#3653,.T.);
#27318=EDGE_CURVE('',#21872,#22077,#3654,.T.);
#27319=EDGE_CURVE('',#22078,#21707,#3655,.T.);
#27320=EDGE_CURVE('',#21876,#22078,#3656,.T.);
#27321=EDGE_CURVE('',#22079,#21705,#3657,.T.);
#27322=EDGE_CURVE('',#21880,#22079,#3658,.T.);
#27323=EDGE_CURVE('',#22080,#21703,#3659,.T.);
#27324=EDGE_CURVE('',#21884,#22080,#3660,.T.);
#27325=EDGE_CURVE('',#22081,#21701,#3661,.T.);
#27326=EDGE_CURVE('',#21888,#22081,#3662,.T.);
#27327=EDGE_CURVE('',#22082,#21699,#3663,.T.);
#27328=EDGE_CURVE('',#21892,#22082,#3664,.T.);
#27329=EDGE_CURVE('',#22083,#21697,#3665,.T.);
#27330=EDGE_CURVE('',#21896,#22083,#3666,.T.);
#27331=EDGE_CURVE('',#22084,#21695,#3667,.T.);
#27332=EDGE_CURVE('',#21900,#22084,#3668,.T.);
#27333=EDGE_CURVE('',#22085,#21693,#3669,.T.);
#27334=EDGE_CURVE('',#21904,#22085,#3670,.T.);
#27335=EDGE_CURVE('',#22086,#22085,#3671,.T.);
#27336=EDGE_CURVE('',#21905,#22086,#19022,.T.);
#27337=EDGE_CURVE('',#22087,#22084,#3672,.T.);
#27338=EDGE_CURVE('',#21901,#22087,#19023,.T.);
#27339=EDGE_CURVE('',#22088,#22083,#3673,.T.);
#27340=EDGE_CURVE('',#21897,#22088,#19024,.T.);
#27341=EDGE_CURVE('',#22089,#22082,#3674,.T.);
#27342=EDGE_CURVE('',#21893,#22089,#19025,.T.);
#27343=EDGE_CURVE('',#22090,#22081,#3675,.T.);
#27344=EDGE_CURVE('',#21889,#22090,#19026,.T.);
#27345=EDGE_CURVE('',#22091,#22080,#3676,.T.);
#27346=EDGE_CURVE('',#21885,#22091,#19027,.T.);
#27347=EDGE_CURVE('',#22092,#22079,#3677,.T.);
#27348=EDGE_CURVE('',#21881,#22092,#19028,.T.);
#27349=EDGE_CURVE('',#22093,#22078,#3678,.T.);
#27350=EDGE_CURVE('',#21877,#22093,#19029,.T.);
#27351=EDGE_CURVE('',#22094,#22077,#3679,.T.);
#27352=EDGE_CURVE('',#21873,#22094,#19030,.T.);
#27353=EDGE_CURVE('',#22095,#22076,#3680,.T.);
#27354=EDGE_CURVE('',#21869,#22095,#19031,.T.);
#27355=EDGE_CURVE('',#22096,#22075,#3681,.T.);
#27356=EDGE_CURVE('',#21865,#22096,#19032,.T.);
#27357=EDGE_CURVE('',#22097,#22074,#3682,.T.);
#27358=EDGE_CURVE('',#21861,#22097,#19033,.T.);
#27359=EDGE_CURVE('',#22098,#22073,#3683,.T.);
#27360=EDGE_CURVE('',#21857,#22098,#19034,.T.);
#27361=EDGE_CURVE('',#22099,#22072,#3684,.T.);
#27362=EDGE_CURVE('',#21853,#22099,#19035,.T.);
#27363=EDGE_CURVE('',#22100,#22071,#3685,.T.);
#27364=EDGE_CURVE('',#21849,#22100,#19036,.T.);
#27365=EDGE_CURVE('',#22101,#22070,#3686,.T.);
#27366=EDGE_CURVE('',#21845,#22101,#19037,.T.);
#27367=EDGE_CURVE('',#22102,#22069,#3687,.T.);
#27368=EDGE_CURVE('',#21841,#22102,#19038,.T.);
#27369=EDGE_CURVE('',#22103,#22068,#3688,.T.);
#27370=EDGE_CURVE('',#22104,#22103,#19039,.T.);
#27371=EDGE_CURVE('',#21837,#22104,#19040,.T.);
#27372=EDGE_CURVE('',#22105,#22067,#3689,.T.);
#27373=EDGE_CURVE('',#21833,#22105,#19041,.T.);
#27374=EDGE_CURVE('',#22106,#22066,#3690,.T.);
#27375=EDGE_CURVE('',#21829,#22106,#19042,.T.);
#27376=EDGE_CURVE('',#22107,#22065,#3691,.T.);
#27377=EDGE_CURVE('',#21825,#22107,#19043,.T.);
#27378=EDGE_CURVE('',#22108,#22064,#3692,.T.);
#27379=EDGE_CURVE('',#21821,#22108,#19044,.T.);
#27380=EDGE_CURVE('',#22109,#22063,#3693,.T.);
#27381=EDGE_CURVE('',#21817,#22109,#19045,.T.);
#27382=EDGE_CURVE('',#22110,#22062,#3694,.T.);
#27383=EDGE_CURVE('',#21813,#22110,#19046,.T.);
#27384=EDGE_CURVE('',#22111,#22061,#3695,.T.);
#27385=EDGE_CURVE('',#21809,#22111,#19047,.T.);
#27386=EDGE_CURVE('',#22112,#22060,#3696,.T.);
#27387=EDGE_CURVE('',#21805,#22112,#19048,.T.);
#27388=EDGE_CURVE('',#22113,#22059,#3697,.T.);
#27389=EDGE_CURVE('',#21801,#22113,#19049,.T.);
#27390=EDGE_CURVE('',#22114,#22058,#3698,.T.);
#27391=EDGE_CURVE('',#21797,#22114,#19050,.T.);
#27392=EDGE_CURVE('',#22115,#22057,#3699,.T.);
#27393=EDGE_CURVE('',#21793,#22115,#19051,.T.);
#27394=EDGE_CURVE('',#22116,#22056,#3700,.T.);
#27395=EDGE_CURVE('',#21789,#22116,#19052,.T.);
#27396=EDGE_CURVE('',#22117,#22055,#3701,.T.);
#27397=EDGE_CURVE('',#21785,#22117,#19053,.T.);
#27398=EDGE_CURVE('',#22118,#22054,#3702,.T.);
#27399=EDGE_CURVE('',#21781,#22118,#19054,.T.);
#27400=EDGE_CURVE('',#22119,#22053,#3703,.T.);
#27401=EDGE_CURVE('',#21777,#22119,#19055,.T.);
#27402=EDGE_CURVE('',#22120,#22052,#3704,.T.);
#27403=EDGE_CURVE('',#21773,#22120,#19056,.T.);
#27404=EDGE_CURVE('',#22121,#22051,#3705,.T.);
#27405=EDGE_CURVE('',#21769,#22121,#19057,.T.);
#27406=EDGE_CURVE('',#22122,#22050,#3706,.T.);
#27407=EDGE_CURVE('',#21765,#22122,#19058,.T.);
#27408=EDGE_CURVE('',#22123,#21691,#3707,.T.);
#27409=EDGE_CURVE('',#21659,#22123,#3708,.T.);
#27410=EDGE_CURVE('',#22124,#22123,#1395,.T.);
#27411=EDGE_CURVE('',#21660,#22124,#3709,.T.);
#27412=EDGE_CURVE('',#22125,#22124,#1396,.T.);
#27413=EDGE_CURVE('',#21661,#22125,#3710,.T.);
#27414=EDGE_CURVE('',#22126,#22125,#1397,.T.);
#27415=EDGE_CURVE('',#21662,#22126,#3711,.T.);
#27416=EDGE_CURVE('',#22127,#22126,#1398,.T.);
#27417=EDGE_CURVE('',#21663,#22127,#3712,.T.);
#27418=EDGE_CURVE('',#22128,#22127,#1399,.T.);
#27419=EDGE_CURVE('',#21664,#22128,#3713,.T.);
#27420=EDGE_CURVE('',#22129,#22128,#3714,.T.);
#27421=EDGE_CURVE('',#21665,#22129,#3715,.T.);
#27422=EDGE_CURVE('',#22130,#22129,#1400,.T.);
#27423=EDGE_CURVE('',#21666,#22130,#3716,.T.);
#27424=EDGE_CURVE('',#22131,#22130,#1401,.T.);
#27425=EDGE_CURVE('',#21667,#22131,#3717,.T.);
#27426=EDGE_CURVE('',#22132,#22131,#1402,.T.);
#27427=EDGE_CURVE('',#21668,#22132,#3718,.T.);
#27428=EDGE_CURVE('',#22133,#22132,#1403,.T.);
#27429=EDGE_CURVE('',#21669,#22133,#3719,.T.);
#27430=EDGE_CURVE('',#22134,#22133,#1404,.T.);
#27431=EDGE_CURVE('',#21670,#22134,#3720,.T.);
#27432=EDGE_CURVE('',#22135,#22134,#3721,.T.);
#27433=EDGE_CURVE('',#21671,#22135,#3722,.T.);
#27434=EDGE_CURVE('',#22136,#22135,#1405,.T.);
#27435=EDGE_CURVE('',#22086,#22136,#19059,.T.);
#27436=EDGE_CURVE('',#22137,#21907,#3723,.T.);
#27437=EDGE_CURVE('',#21675,#22137,#3724,.T.);
#27438=EDGE_CURVE('',#22138,#22137,#1406,.T.);
#27439=EDGE_CURVE('',#21676,#22138,#3725,.T.);
#27440=EDGE_CURVE('',#22139,#22138,#1407,.T.);
#27441=EDGE_CURVE('',#21677,#22139,#3726,.T.);
#27442=EDGE_CURVE('',#22140,#22139,#1408,.T.);
#27443=EDGE_CURVE('',#21678,#22140,#3727,.T.);
#27444=EDGE_CURVE('',#22141,#22140,#1409,.T.);
#27445=EDGE_CURVE('',#21679,#22141,#3728,.T.);
#27446=EDGE_CURVE('',#22142,#22141,#1410,.T.);
#27447=EDGE_CURVE('',#21680,#22142,#3729,.T.);
#27448=EDGE_CURVE('',#22143,#22142,#3730,.T.);
#27449=EDGE_CURVE('',#21681,#22143,#3731,.T.);
#27450=EDGE_CURVE('',#22144,#22143,#1411,.T.);
#27451=EDGE_CURVE('',#21682,#22144,#3732,.T.);
#27452=EDGE_CURVE('',#22145,#22144,#1412,.T.);
#27453=EDGE_CURVE('',#21683,#22145,#3733,.T.);
#27454=EDGE_CURVE('',#22146,#22145,#1413,.T.);
#27455=EDGE_CURVE('',#21684,#22146,#3734,.T.);
#27456=EDGE_CURVE('',#22147,#22146,#1414,.T.);
#27457=EDGE_CURVE('',#21685,#22147,#3735,.T.);
#27458=EDGE_CURVE('',#22148,#22147,#1415,.T.);
#27459=EDGE_CURVE('',#21686,#22148,#3736,.T.);
#27460=EDGE_CURVE('',#21944,#22148,#3737,.T.);
#27461=EDGE_CURVE('',#21689,#21946,#19060,.T.);
#27462=EDGE_CURVE('',#22149,#22149,#19646,.T.);
#27463=EDGE_CURVE('',#22149,#22150,#3738,.T.);
#27464=EDGE_CURVE('',#22150,#21997,#19061,.T.);
#27465=EDGE_CURVE('',#21078,#21996,#19647,.T.);
#27466=EDGE_CURVE('',#21077,#22000,#19062,.T.);
#27467=EDGE_CURVE('',#21044,#21999,#19648,.T.);
#27468=EDGE_CURVE('',#21043,#22003,#19063,.T.);
#27469=EDGE_CURVE('',#21010,#22002,#19649,.T.);
#27470=EDGE_CURVE('',#21009,#22006,#19064,.T.);
#27471=EDGE_CURVE('',#20976,#22005,#19650,.T.);
#27472=EDGE_CURVE('',#20975,#22009,#19065,.T.);
#27473=EDGE_CURVE('',#20942,#22008,#19651,.T.);
#27474=EDGE_CURVE('',#20941,#22012,#19066,.T.);
#27475=EDGE_CURVE('',#20908,#22011,#19652,.T.);
#27476=EDGE_CURVE('',#20907,#22015,#19067,.T.);
#27477=EDGE_CURVE('',#20874,#22014,#19653,.T.);
#27478=EDGE_CURVE('',#20873,#22018,#19068,.T.);
#27479=EDGE_CURVE('',#20840,#22017,#19654,.T.);
#27480=EDGE_CURVE('',#20839,#22021,#19069,.T.);
#27481=EDGE_CURVE('',#20806,#22020,#19655,.T.);
#27482=EDGE_CURVE('',#20805,#22024,#19070,.T.);
#27483=EDGE_CURVE('',#20772,#22023,#19656,.T.);
#27484=EDGE_CURVE('',#20771,#22027,#19071,.T.);
#27485=EDGE_CURVE('',#20738,#22026,#19657,.T.);
#27486=EDGE_CURVE('',#20737,#22030,#19072,.T.);
#27487=EDGE_CURVE('',#20704,#22029,#19658,.T.);
#27488=EDGE_CURVE('',#20703,#22033,#19073,.T.);
#27489=EDGE_CURVE('',#20670,#22032,#19659,.T.);
#27490=EDGE_CURVE('',#20669,#22036,#19074,.T.);
#27491=EDGE_CURVE('',#20636,#22035,#19660,.T.);
#27492=EDGE_CURVE('',#20635,#22039,#19075,.T.);
#27493=EDGE_CURVE('',#20602,#22038,#19661,.T.);
#27494=EDGE_CURVE('',#20601,#22042,#19076,.T.);
#27495=EDGE_CURVE('',#20568,#22041,#19662,.T.);
#27496=EDGE_CURVE('',#20567,#22045,#19077,.T.);
#27497=EDGE_CURVE('',#20534,#22044,#19663,.T.);
#27498=EDGE_CURVE('',#20533,#22048,#19078,.T.);
#27499=EDGE_CURVE('',#20500,#22047,#19664,.T.);
#27500=EDGE_CURVE('',#22049,#22151,#19079,.T.);
#27501=EDGE_CURVE('',#21690,#22151,#19665,.T.);
#27502=EDGE_CURVE('',#21656,#21945,#19666,.T.);
#27503=EDGE_CURVE('',#21655,#21949,#19080,.T.);
#27504=EDGE_CURVE('',#21622,#21948,#19667,.T.);
#27505=EDGE_CURVE('',#21621,#21952,#19081,.T.);
#27506=EDGE_CURVE('',#21588,#21951,#19668,.T.);
#27507=EDGE_CURVE('',#21587,#21955,#19082,.T.);
#27508=EDGE_CURVE('',#21554,#21954,#19669,.T.);
#27509=EDGE_CURVE('',#21553,#21958,#19083,.T.);
#27510=EDGE_CURVE('',#21520,#21957,#19670,.T.);
#27511=EDGE_CURVE('',#21519,#21961,#19084,.T.);
#27512=EDGE_CURVE('',#21486,#21960,#19671,.T.);
#27513=EDGE_CURVE('',#21485,#21964,#19085,.T.);
#27514=EDGE_CURVE('',#21452,#21963,#19672,.T.);
#27515=EDGE_CURVE('',#21451,#21967,#19086,.T.);
#27516=EDGE_CURVE('',#21418,#21966,#19673,.T.);
#27517=EDGE_CURVE('',#21417,#21970,#19087,.T.);
#27518=EDGE_CURVE('',#21384,#21969,#19674,.T.);
#27519=EDGE_CURVE('',#21383,#21973,#19088,.T.);
#27520=EDGE_CURVE('',#21350,#21972,#19675,.T.);
#27521=EDGE_CURVE('',#21349,#21976,#19089,.T.);
#27522=EDGE_CURVE('',#21316,#21975,#19676,.T.);
#27523=EDGE_CURVE('',#21315,#21979,#19090,.T.);
#27524=EDGE_CURVE('',#21282,#21978,#19677,.T.);
#27525=EDGE_CURVE('',#21281,#21982,#19091,.T.);
#27526=EDGE_CURVE('',#21248,#21981,#19678,.T.);
#27527=EDGE_CURVE('',#21247,#21985,#19092,.T.);
#27528=EDGE_CURVE('',#21214,#21984,#19679,.T.);
#27529=EDGE_CURVE('',#21213,#21988,#19093,.T.);
#27530=EDGE_CURVE('',#21180,#21987,#19680,.T.);
#27531=EDGE_CURVE('',#21179,#21991,#19094,.T.);
#27532=EDGE_CURVE('',#21146,#21990,#19681,.T.);
#27533=EDGE_CURVE('',#21145,#21994,#19095,.T.);
#27534=EDGE_CURVE('',#21112,#21993,#19682,.T.);
#27535=EDGE_CURVE('',#21111,#22150,#19096,.T.);
#27536=EDGE_CURVE('',#22152,#21906,#19683,.T.);
#27537=EDGE_CURVE('',#22152,#22153,#1416,.T.);
#27538=EDGE_CURVE('',#22153,#22154,#3739,.T.);
#27539=EDGE_CURVE('',#22154,#22155,#1417,.T.);
#27540=EDGE_CURVE('',#22155,#22156,#1418,.T.);
#27541=EDGE_CURVE('',#22156,#22157,#1419,.T.);
#27542=EDGE_CURVE('',#22157,#22158,#1420,.T.);
#27543=EDGE_CURVE('',#22158,#22159,#1421,.T.);
#27544=EDGE_CURVE('',#22159,#22160,#3740,.T.);
#27545=EDGE_CURVE('',#22160,#22161,#1422,.T.);
#27546=EDGE_CURVE('',#22161,#22162,#1423,.T.);
#27547=EDGE_CURVE('',#22162,#22163,#1424,.T.);
#27548=EDGE_CURVE('',#22163,#22164,#1425,.T.);
#27549=EDGE_CURVE('',#22164,#22165,#1426,.T.);
#27550=EDGE_CURVE('',#22165,#21657,#3741,.T.);
#27551=EDGE_CURVE('',#21625,#22165,#3742,.T.);
#27552=EDGE_CURVE('',#21626,#22164,#3743,.T.);
#27553=EDGE_CURVE('',#21627,#22163,#3744,.T.);
#27554=EDGE_CURVE('',#21628,#22162,#3745,.T.);
#27555=EDGE_CURVE('',#21629,#22161,#3746,.T.);
#27556=EDGE_CURVE('',#21630,#22160,#3747,.T.);
#27557=EDGE_CURVE('',#21631,#22159,#3748,.T.);
#27558=EDGE_CURVE('',#21632,#22158,#3749,.T.);
#27559=EDGE_CURVE('',#21633,#22157,#3750,.T.);
#27560=EDGE_CURVE('',#21634,#22156,#3751,.T.);
#27561=EDGE_CURVE('',#21635,#22155,#3752,.T.);
#27562=EDGE_CURVE('',#21636,#22154,#3753,.T.);
#27563=EDGE_CURVE('',#21637,#22153,#3754,.T.);
#27564=EDGE_CURVE('',#22087,#22152,#19097,.T.);
#27565=EDGE_CURVE('',#22166,#21903,#3755,.T.);
#27566=EDGE_CURVE('',#21641,#22166,#3756,.T.);
#27567=EDGE_CURVE('',#22167,#22166,#1427,.T.);
#27568=EDGE_CURVE('',#21642,#22167,#3757,.T.);
#27569=EDGE_CURVE('',#22168,#22167,#1428,.T.);
#27570=EDGE_CURVE('',#21643,#22168,#3758,.T.);
#27571=EDGE_CURVE('',#22169,#22168,#1429,.T.);
#27572=EDGE_CURVE('',#21644,#22169,#3759,.T.);
#27573=EDGE_CURVE('',#22170,#22169,#1430,.T.);
#27574=EDGE_CURVE('',#21645,#22170,#3760,.T.);
#27575=EDGE_CURVE('',#22171,#22170,#1431,.T.);
#27576=EDGE_CURVE('',#21646,#22171,#3761,.T.);
#27577=EDGE_CURVE('',#22172,#22171,#3762,.T.);
#27578=EDGE_CURVE('',#21647,#22172,#3763,.T.);
#27579=EDGE_CURVE('',#22173,#22172,#1432,.T.);
#27580=EDGE_CURVE('',#21648,#22173,#3764,.T.);
#27581=EDGE_CURVE('',#22174,#22173,#1433,.T.);
#27582=EDGE_CURVE('',#21649,#22174,#3765,.T.);
#27583=EDGE_CURVE('',#22175,#22174,#1434,.T.);
#27584=EDGE_CURVE('',#21650,#22175,#3766,.T.);
#27585=EDGE_CURVE('',#22176,#22175,#1435,.T.);
#27586=EDGE_CURVE('',#21651,#22176,#3767,.T.);
#27587=EDGE_CURVE('',#22177,#22176,#1436,.T.);
#27588=EDGE_CURVE('',#21652,#22177,#3768,.T.);
#27589=EDGE_CURVE('',#21947,#22177,#3769,.T.);
#27590=EDGE_CURVE('',#22178,#21902,#19684,.T.);
#27591=EDGE_CURVE('',#22178,#22179,#1437,.T.);
#27592=EDGE_CURVE('',#22179,#22180,#3770,.T.);
#27593=EDGE_CURVE('',#22180,#22181,#1438,.T.);
#27594=EDGE_CURVE('',#22181,#22182,#1439,.T.);
#27595=EDGE_CURVE('',#22182,#22183,#1440,.T.);
#27596=EDGE_CURVE('',#22183,#22184,#1441,.T.);
#27597=EDGE_CURVE('',#22184,#22185,#1442,.T.);
#27598=EDGE_CURVE('',#22185,#22186,#3771,.T.);
#27599=EDGE_CURVE('',#22186,#22187,#1443,.T.);
#27600=EDGE_CURVE('',#22187,#22188,#1444,.T.);
#27601=EDGE_CURVE('',#22188,#22189,#1445,.T.);
#27602=EDGE_CURVE('',#22189,#22190,#1446,.T.);
#27603=EDGE_CURVE('',#22190,#22191,#1447,.T.);
#27604=EDGE_CURVE('',#22191,#21623,#3772,.T.);
#27605=EDGE_CURVE('',#21591,#22191,#3773,.T.);
#27606=EDGE_CURVE('',#21592,#22190,#3774,.T.);
#27607=EDGE_CURVE('',#21593,#22189,#3775,.T.);
#27608=EDGE_CURVE('',#21594,#22188,#3776,.T.);
#27609=EDGE_CURVE('',#21595,#22187,#3777,.T.);
#27610=EDGE_CURVE('',#21596,#22186,#3778,.T.);
#27611=EDGE_CURVE('',#21597,#22185,#3779,.T.);
#27612=EDGE_CURVE('',#21598,#22184,#3780,.T.);
#27613=EDGE_CURVE('',#21599,#22183,#3781,.T.);
#27614=EDGE_CURVE('',#21600,#22182,#3782,.T.);
#27615=EDGE_CURVE('',#21601,#22181,#3783,.T.);
#27616=EDGE_CURVE('',#21602,#22180,#3784,.T.);
#27617=EDGE_CURVE('',#21603,#22179,#3785,.T.);
#27618=EDGE_CURVE('',#22088,#22178,#19098,.T.);
#27619=EDGE_CURVE('',#22192,#21899,#3786,.T.);
#27620=EDGE_CURVE('',#21607,#22192,#3787,.T.);
#27621=EDGE_CURVE('',#22193,#22192,#1448,.T.);
#27622=EDGE_CURVE('',#21608,#22193,#3788,.T.);
#27623=EDGE_CURVE('',#22194,#22193,#1449,.T.);
#27624=EDGE_CURVE('',#21609,#22194,#3789,.T.);
#27625=EDGE_CURVE('',#22195,#22194,#1450,.T.);
#27626=EDGE_CURVE('',#21610,#22195,#3790,.T.);
#27627=EDGE_CURVE('',#22196,#22195,#1451,.T.);
#27628=EDGE_CURVE('',#21611,#22196,#3791,.T.);
#27629=EDGE_CURVE('',#22197,#22196,#1452,.T.);
#27630=EDGE_CURVE('',#21612,#22197,#3792,.T.);
#27631=EDGE_CURVE('',#22198,#22197,#3793,.T.);
#27632=EDGE_CURVE('',#21613,#22198,#3794,.T.);
#27633=EDGE_CURVE('',#22199,#22198,#1453,.T.);
#27634=EDGE_CURVE('',#21614,#22199,#3795,.T.);
#27635=EDGE_CURVE('',#22200,#22199,#1454,.T.);
#27636=EDGE_CURVE('',#21615,#22200,#3796,.T.);
#27637=EDGE_CURVE('',#22201,#22200,#1455,.T.);
#27638=EDGE_CURVE('',#21616,#22201,#3797,.T.);
#27639=EDGE_CURVE('',#22202,#22201,#1456,.T.);
#27640=EDGE_CURVE('',#21617,#22202,#3798,.T.);
#27641=EDGE_CURVE('',#22203,#22202,#1457,.T.);
#27642=EDGE_CURVE('',#21618,#22203,#3799,.T.);
#27643=EDGE_CURVE('',#21950,#22203,#3800,.T.);
#27644=EDGE_CURVE('',#22204,#21898,#19685,.T.);
#27645=EDGE_CURVE('',#22204,#22205,#1458,.T.);
#27646=EDGE_CURVE('',#22205,#22206,#3801,.T.);
#27647=EDGE_CURVE('',#22206,#22207,#1459,.T.);
#27648=EDGE_CURVE('',#22207,#22208,#1460,.T.);
#27649=EDGE_CURVE('',#22208,#22209,#1461,.T.);
#27650=EDGE_CURVE('',#22209,#22210,#1462,.T.);
#27651=EDGE_CURVE('',#22210,#22211,#1463,.T.);
#27652=EDGE_CURVE('',#22211,#22212,#3802,.T.);
#27653=EDGE_CURVE('',#22212,#22213,#1464,.T.);
#27654=EDGE_CURVE('',#22213,#22214,#1465,.T.);
#27655=EDGE_CURVE('',#22214,#22215,#1466,.T.);
#27656=EDGE_CURVE('',#22215,#22216,#1467,.T.);
#27657=EDGE_CURVE('',#22216,#22217,#1468,.T.);
#27658=EDGE_CURVE('',#22217,#21589,#3803,.T.);
#27659=EDGE_CURVE('',#21557,#22217,#3804,.T.);
#27660=EDGE_CURVE('',#21558,#22216,#3805,.T.);
#27661=EDGE_CURVE('',#21559,#22215,#3806,.T.);
#27662=EDGE_CURVE('',#21560,#22214,#3807,.T.);
#27663=EDGE_CURVE('',#21561,#22213,#3808,.T.);
#27664=EDGE_CURVE('',#21562,#22212,#3809,.T.);
#27665=EDGE_CURVE('',#21563,#22211,#3810,.T.);
#27666=EDGE_CURVE('',#21564,#22210,#3811,.T.);
#27667=EDGE_CURVE('',#21565,#22209,#3812,.T.);
#27668=EDGE_CURVE('',#21566,#22208,#3813,.T.);
#27669=EDGE_CURVE('',#21567,#22207,#3814,.T.);
#27670=EDGE_CURVE('',#21568,#22206,#3815,.T.);
#27671=EDGE_CURVE('',#21569,#22205,#3816,.T.);
#27672=EDGE_CURVE('',#22089,#22204,#19099,.T.);
#27673=EDGE_CURVE('',#22218,#21895,#3817,.T.);
#27674=EDGE_CURVE('',#21573,#22218,#3818,.T.);
#27675=EDGE_CURVE('',#22219,#22218,#1469,.T.);
#27676=EDGE_CURVE('',#21574,#22219,#3819,.T.);
#27677=EDGE_CURVE('',#22220,#22219,#1470,.T.);
#27678=EDGE_CURVE('',#21575,#22220,#3820,.T.);
#27679=EDGE_CURVE('',#22221,#22220,#1471,.T.);
#27680=EDGE_CURVE('',#21576,#22221,#3821,.T.);
#27681=EDGE_CURVE('',#22222,#22221,#1472,.T.);
#27682=EDGE_CURVE('',#21577,#22222,#3822,.T.);
#27683=EDGE_CURVE('',#22223,#22222,#1473,.T.);
#27684=EDGE_CURVE('',#21578,#22223,#3823,.T.);
#27685=EDGE_CURVE('',#22224,#22223,#3824,.T.);
#27686=EDGE_CURVE('',#21579,#22224,#3825,.T.);
#27687=EDGE_CURVE('',#22225,#22224,#1474,.T.);
#27688=EDGE_CURVE('',#21580,#22225,#3826,.T.);
#27689=EDGE_CURVE('',#22226,#22225,#1475,.T.);
#27690=EDGE_CURVE('',#21581,#22226,#3827,.T.);
#27691=EDGE_CURVE('',#22227,#22226,#1476,.T.);
#27692=EDGE_CURVE('',#21582,#22227,#3828,.T.);
#27693=EDGE_CURVE('',#22228,#22227,#1477,.T.);
#27694=EDGE_CURVE('',#21583,#22228,#3829,.T.);
#27695=EDGE_CURVE('',#22229,#22228,#1478,.T.);
#27696=EDGE_CURVE('',#21584,#22229,#3830,.T.);
#27697=EDGE_CURVE('',#21953,#22229,#3831,.T.);
#27698=EDGE_CURVE('',#22230,#21894,#19686,.T.);
#27699=EDGE_CURVE('',#22230,#22231,#1479,.T.);
#27700=EDGE_CURVE('',#22231,#22232,#3832,.T.);
#27701=EDGE_CURVE('',#22232,#22233,#1480,.T.);
#27702=EDGE_CURVE('',#22233,#22234,#1481,.T.);
#27703=EDGE_CURVE('',#22234,#22235,#1482,.T.);
#27704=EDGE_CURVE('',#22235,#22236,#1483,.T.);
#27705=EDGE_CURVE('',#22236,#22237,#1484,.T.);
#27706=EDGE_CURVE('',#22237,#22238,#3833,.T.);
#27707=EDGE_CURVE('',#22238,#22239,#1485,.T.);
#27708=EDGE_CURVE('',#22239,#22240,#1486,.T.);
#27709=EDGE_CURVE('',#22240,#22241,#1487,.T.);
#27710=EDGE_CURVE('',#22241,#22242,#1488,.T.);
#27711=EDGE_CURVE('',#22242,#22243,#1489,.T.);
#27712=EDGE_CURVE('',#22243,#21555,#3834,.T.);
#27713=EDGE_CURVE('',#21523,#22243,#3835,.T.);
#27714=EDGE_CURVE('',#21524,#22242,#3836,.T.);
#27715=EDGE_CURVE('',#21525,#22241,#3837,.T.);
#27716=EDGE_CURVE('',#21526,#22240,#3838,.T.);
#27717=EDGE_CURVE('',#21527,#22239,#3839,.T.);
#27718=EDGE_CURVE('',#21528,#22238,#3840,.T.);
#27719=EDGE_CURVE('',#21529,#22237,#3841,.T.);
#27720=EDGE_CURVE('',#21530,#22236,#3842,.T.);
#27721=EDGE_CURVE('',#21531,#22235,#3843,.T.);
#27722=EDGE_CURVE('',#21532,#22234,#3844,.T.);
#27723=EDGE_CURVE('',#21533,#22233,#3845,.T.);
#27724=EDGE_CURVE('',#21534,#22232,#3846,.T.);
#27725=EDGE_CURVE('',#21535,#22231,#3847,.T.);
#27726=EDGE_CURVE('',#22090,#22230,#19100,.T.);
#27727=EDGE_CURVE('',#22244,#21891,#3848,.T.);
#27728=EDGE_CURVE('',#21539,#22244,#3849,.T.);
#27729=EDGE_CURVE('',#22245,#22244,#1490,.T.);
#27730=EDGE_CURVE('',#21540,#22245,#3850,.T.);
#27731=EDGE_CURVE('',#22246,#22245,#1491,.T.);
#27732=EDGE_CURVE('',#21541,#22246,#3851,.T.);
#27733=EDGE_CURVE('',#22247,#22246,#1492,.T.);
#27734=EDGE_CURVE('',#21542,#22247,#3852,.T.);
#27735=EDGE_CURVE('',#22248,#22247,#1493,.T.);
#27736=EDGE_CURVE('',#21543,#22248,#3853,.T.);
#27737=EDGE_CURVE('',#22249,#22248,#1494,.T.);
#27738=EDGE_CURVE('',#21544,#22249,#3854,.T.);
#27739=EDGE_CURVE('',#22250,#22249,#3855,.T.);
#27740=EDGE_CURVE('',#21545,#22250,#3856,.T.);
#27741=EDGE_CURVE('',#22251,#22250,#1495,.T.);
#27742=EDGE_CURVE('',#21546,#22251,#3857,.T.);
#27743=EDGE_CURVE('',#22252,#22251,#1496,.T.);
#27744=EDGE_CURVE('',#21547,#22252,#3858,.T.);
#27745=EDGE_CURVE('',#22253,#22252,#1497,.T.);
#27746=EDGE_CURVE('',#21548,#22253,#3859,.T.);
#27747=EDGE_CURVE('',#22254,#22253,#1498,.T.);
#27748=EDGE_CURVE('',#21549,#22254,#3860,.T.);
#27749=EDGE_CURVE('',#22255,#22254,#1499,.T.);
#27750=EDGE_CURVE('',#21550,#22255,#3861,.T.);
#27751=EDGE_CURVE('',#21956,#22255,#3862,.T.);
#27752=EDGE_CURVE('',#22256,#21890,#19687,.T.);
#27753=EDGE_CURVE('',#22256,#22257,#1500,.T.);
#27754=EDGE_CURVE('',#22257,#22258,#3863,.T.);
#27755=EDGE_CURVE('',#22258,#22259,#1501,.T.);
#27756=EDGE_CURVE('',#22259,#22260,#1502,.T.);
#27757=EDGE_CURVE('',#22260,#22261,#1503,.T.);
#27758=EDGE_CURVE('',#22261,#22262,#1504,.T.);
#27759=EDGE_CURVE('',#22262,#22263,#1505,.T.);
#27760=EDGE_CURVE('',#22263,#22264,#3864,.T.);
#27761=EDGE_CURVE('',#22264,#22265,#1506,.T.);
#27762=EDGE_CURVE('',#22265,#22266,#1507,.T.);
#27763=EDGE_CURVE('',#22266,#22267,#1508,.T.);
#27764=EDGE_CURVE('',#22267,#22268,#1509,.T.);
#27765=EDGE_CURVE('',#22268,#22269,#1510,.T.);
#27766=EDGE_CURVE('',#22269,#21521,#3865,.T.);
#27767=EDGE_CURVE('',#21489,#22269,#3866,.T.);
#27768=EDGE_CURVE('',#21490,#22268,#3867,.T.);
#27769=EDGE_CURVE('',#21491,#22267,#3868,.T.);
#27770=EDGE_CURVE('',#21492,#22266,#3869,.T.);
#27771=EDGE_CURVE('',#21493,#22265,#3870,.T.);
#27772=EDGE_CURVE('',#21494,#22264,#3871,.T.);
#27773=EDGE_CURVE('',#21495,#22263,#3872,.T.);
#27774=EDGE_CURVE('',#21496,#22262,#3873,.T.);
#27775=EDGE_CURVE('',#21497,#22261,#3874,.T.);
#27776=EDGE_CURVE('',#21498,#22260,#3875,.T.);
#27777=EDGE_CURVE('',#21499,#22259,#3876,.T.);
#27778=EDGE_CURVE('',#21500,#22258,#3877,.T.);
#27779=EDGE_CURVE('',#21501,#22257,#3878,.T.);
#27780=EDGE_CURVE('',#22091,#22256,#19101,.T.);
#27781=EDGE_CURVE('',#22270,#21887,#3879,.T.);
#27782=EDGE_CURVE('',#21505,#22270,#3880,.T.);
#27783=EDGE_CURVE('',#22271,#22270,#1511,.T.);
#27784=EDGE_CURVE('',#21506,#22271,#3881,.T.);
#27785=EDGE_CURVE('',#22272,#22271,#1512,.T.);
#27786=EDGE_CURVE('',#21507,#22272,#3882,.T.);
#27787=EDGE_CURVE('',#22273,#22272,#1513,.T.);
#27788=EDGE_CURVE('',#21508,#22273,#3883,.T.);
#27789=EDGE_CURVE('',#22274,#22273,#1514,.T.);
#27790=EDGE_CURVE('',#21509,#22274,#3884,.T.);
#27791=EDGE_CURVE('',#22275,#22274,#1515,.T.);
#27792=EDGE_CURVE('',#21510,#22275,#3885,.T.);
#27793=EDGE_CURVE('',#22276,#22275,#3886,.T.);
#27794=EDGE_CURVE('',#21511,#22276,#3887,.T.);
#27795=EDGE_CURVE('',#22277,#22276,#1516,.T.);
#27796=EDGE_CURVE('',#21512,#22277,#3888,.T.);
#27797=EDGE_CURVE('',#22278,#22277,#1517,.T.);
#27798=EDGE_CURVE('',#21513,#22278,#3889,.T.);
#27799=EDGE_CURVE('',#22279,#22278,#1518,.T.);
#27800=EDGE_CURVE('',#21514,#22279,#3890,.T.);
#27801=EDGE_CURVE('',#22280,#22279,#1519,.T.);
#27802=EDGE_CURVE('',#21515,#22280,#3891,.T.);
#27803=EDGE_CURVE('',#22281,#22280,#1520,.T.);
#27804=EDGE_CURVE('',#21516,#22281,#3892,.T.);
#27805=EDGE_CURVE('',#21959,#22281,#3893,.T.);
#27806=EDGE_CURVE('',#22282,#21886,#19688,.T.);
#27807=EDGE_CURVE('',#22282,#22283,#1521,.T.);
#27808=EDGE_CURVE('',#22283,#22284,#3894,.T.);
#27809=EDGE_CURVE('',#22284,#22285,#1522,.T.);
#27810=EDGE_CURVE('',#22285,#22286,#1523,.T.);
#27811=EDGE_CURVE('',#22286,#22287,#1524,.T.);
#27812=EDGE_CURVE('',#22287,#22288,#1525,.T.);
#27813=EDGE_CURVE('',#22288,#22289,#1526,.T.);
#27814=EDGE_CURVE('',#22289,#22290,#3895,.T.);
#27815=EDGE_CURVE('',#22290,#22291,#1527,.T.);
#27816=EDGE_CURVE('',#22291,#22292,#1528,.T.);
#27817=EDGE_CURVE('',#22292,#22293,#1529,.T.);
#27818=EDGE_CURVE('',#22293,#22294,#1530,.T.);
#27819=EDGE_CURVE('',#22294,#22295,#1531,.T.);
#27820=EDGE_CURVE('',#22295,#21487,#3896,.T.);
#27821=EDGE_CURVE('',#21455,#22295,#3897,.T.);
#27822=EDGE_CURVE('',#21456,#22294,#3898,.T.);
#27823=EDGE_CURVE('',#21457,#22293,#3899,.T.);
#27824=EDGE_CURVE('',#21458,#22292,#3900,.T.);
#27825=EDGE_CURVE('',#21459,#22291,#3901,.T.);
#27826=EDGE_CURVE('',#21460,#22290,#3902,.T.);
#27827=EDGE_CURVE('',#21461,#22289,#3903,.T.);
#27828=EDGE_CURVE('',#21462,#22288,#3904,.T.);
#27829=EDGE_CURVE('',#21463,#22287,#3905,.T.);
#27830=EDGE_CURVE('',#21464,#22286,#3906,.T.);
#27831=EDGE_CURVE('',#21465,#22285,#3907,.T.);
#27832=EDGE_CURVE('',#21466,#22284,#3908,.T.);
#27833=EDGE_CURVE('',#21467,#22283,#3909,.T.);
#27834=EDGE_CURVE('',#22092,#22282,#19102,.T.);
#27835=EDGE_CURVE('',#22296,#21883,#3910,.T.);
#27836=EDGE_CURVE('',#21471,#22296,#3911,.T.);
#27837=EDGE_CURVE('',#22297,#22296,#1532,.T.);
#27838=EDGE_CURVE('',#21472,#22297,#3912,.T.);
#27839=EDGE_CURVE('',#22298,#22297,#1533,.T.);
#27840=EDGE_CURVE('',#21473,#22298,#3913,.T.);
#27841=EDGE_CURVE('',#22299,#22298,#1534,.T.);
#27842=EDGE_CURVE('',#21474,#22299,#3914,.T.);
#27843=EDGE_CURVE('',#22300,#22299,#1535,.T.);
#27844=EDGE_CURVE('',#21475,#22300,#3915,.T.);
#27845=EDGE_CURVE('',#22301,#22300,#1536,.T.);
#27846=EDGE_CURVE('',#21476,#22301,#3916,.T.);
#27847=EDGE_CURVE('',#22302,#22301,#3917,.T.);
#27848=EDGE_CURVE('',#21477,#22302,#3918,.T.);
#27849=EDGE_CURVE('',#22303,#22302,#1537,.T.);
#27850=EDGE_CURVE('',#21478,#22303,#3919,.T.);
#27851=EDGE_CURVE('',#22304,#22303,#1538,.T.);
#27852=EDGE_CURVE('',#21479,#22304,#3920,.T.);
#27853=EDGE_CURVE('',#22305,#22304,#1539,.T.);
#27854=EDGE_CURVE('',#21480,#22305,#3921,.T.);
#27855=EDGE_CURVE('',#22306,#22305,#1540,.T.);
#27856=EDGE_CURVE('',#21481,#22306,#3922,.T.);
#27857=EDGE_CURVE('',#22307,#22306,#1541,.T.);
#27858=EDGE_CURVE('',#21482,#22307,#3923,.T.);
#27859=EDGE_CURVE('',#21962,#22307,#3924,.T.);
#27860=EDGE_CURVE('',#22308,#21882,#19689,.T.);
#27861=EDGE_CURVE('',#22308,#22309,#1542,.T.);
#27862=EDGE_CURVE('',#22309,#22310,#3925,.T.);
#27863=EDGE_CURVE('',#22310,#22311,#1543,.T.);
#27864=EDGE_CURVE('',#22311,#22312,#1544,.T.);
#27865=EDGE_CURVE('',#22312,#22313,#1545,.T.);
#27866=EDGE_CURVE('',#22313,#22314,#1546,.T.);
#27867=EDGE_CURVE('',#22314,#22315,#1547,.T.);
#27868=EDGE_CURVE('',#22315,#22316,#3926,.T.);
#27869=EDGE_CURVE('',#22316,#22317,#1548,.T.);
#27870=EDGE_CURVE('',#22317,#22318,#1549,.T.);
#27871=EDGE_CURVE('',#22318,#22319,#1550,.T.);
#27872=EDGE_CURVE('',#22319,#22320,#1551,.T.);
#27873=EDGE_CURVE('',#22320,#22321,#1552,.T.);
#27874=EDGE_CURVE('',#22321,#21453,#3927,.T.);
#27875=EDGE_CURVE('',#21421,#22321,#3928,.T.);
#27876=EDGE_CURVE('',#21422,#22320,#3929,.T.);
#27877=EDGE_CURVE('',#21423,#22319,#3930,.T.);
#27878=EDGE_CURVE('',#21424,#22318,#3931,.T.);
#27879=EDGE_CURVE('',#21425,#22317,#3932,.T.);
#27880=EDGE_CURVE('',#21426,#22316,#3933,.T.);
#27881=EDGE_CURVE('',#21427,#22315,#3934,.T.);
#27882=EDGE_CURVE('',#21428,#22314,#3935,.T.);
#27883=EDGE_CURVE('',#21429,#22313,#3936,.T.);
#27884=EDGE_CURVE('',#21430,#22312,#3937,.T.);
#27885=EDGE_CURVE('',#21431,#22311,#3938,.T.);
#27886=EDGE_CURVE('',#21432,#22310,#3939,.T.);
#27887=EDGE_CURVE('',#21433,#22309,#3940,.T.);
#27888=EDGE_CURVE('',#22093,#22308,#19103,.T.);
#27889=EDGE_CURVE('',#22322,#21879,#3941,.T.);
#27890=EDGE_CURVE('',#21437,#22322,#3942,.T.);
#27891=EDGE_CURVE('',#22323,#22322,#1553,.T.);
#27892=EDGE_CURVE('',#21438,#22323,#3943,.T.);
#27893=EDGE_CURVE('',#22324,#22323,#1554,.T.);
#27894=EDGE_CURVE('',#21439,#22324,#3944,.T.);
#27895=EDGE_CURVE('',#22325,#22324,#1555,.T.);
#27896=EDGE_CURVE('',#21440,#22325,#3945,.T.);
#27897=EDGE_CURVE('',#22326,#22325,#1556,.T.);
#27898=EDGE_CURVE('',#21441,#22326,#3946,.T.);
#27899=EDGE_CURVE('',#22327,#22326,#1557,.T.);
#27900=EDGE_CURVE('',#21442,#22327,#3947,.T.);
#27901=EDGE_CURVE('',#22328,#22327,#3948,.T.);
#27902=EDGE_CURVE('',#21443,#22328,#3949,.T.);
#27903=EDGE_CURVE('',#22329,#22328,#1558,.T.);
#27904=EDGE_CURVE('',#21444,#22329,#3950,.T.);
#27905=EDGE_CURVE('',#22330,#22329,#1559,.T.);
#27906=EDGE_CURVE('',#21445,#22330,#3951,.T.);
#27907=EDGE_CURVE('',#22331,#22330,#1560,.T.);
#27908=EDGE_CURVE('',#21446,#22331,#3952,.T.);
#27909=EDGE_CURVE('',#22332,#22331,#1561,.T.);
#27910=EDGE_CURVE('',#21447,#22332,#3953,.T.);
#27911=EDGE_CURVE('',#22333,#22332,#1562,.T.);
#27912=EDGE_CURVE('',#21448,#22333,#3954,.T.);
#27913=EDGE_CURVE('',#21965,#22333,#3955,.T.);
#27914=EDGE_CURVE('',#22334,#21878,#19690,.T.);
#27915=EDGE_CURVE('',#22334,#22335,#1563,.T.);
#27916=EDGE_CURVE('',#22335,#22336,#3956,.T.);
#27917=EDGE_CURVE('',#22336,#22337,#1564,.T.);
#27918=EDGE_CURVE('',#22337,#22338,#1565,.T.);
#27919=EDGE_CURVE('',#22338,#22339,#1566,.T.);
#27920=EDGE_CURVE('',#22339,#22340,#1567,.T.);
#27921=EDGE_CURVE('',#22340,#22341,#1568,.T.);
#27922=EDGE_CURVE('',#22341,#22342,#3957,.T.);
#27923=EDGE_CURVE('',#22342,#22343,#1569,.T.);
#27924=EDGE_CURVE('',#22343,#22344,#1570,.T.);
#27925=EDGE_CURVE('',#22344,#22345,#1571,.T.);
#27926=EDGE_CURVE('',#22345,#22346,#1572,.T.);
#27927=EDGE_CURVE('',#22346,#22347,#1573,.T.);
#27928=EDGE_CURVE('',#22347,#21419,#3958,.T.);
#27929=EDGE_CURVE('',#21387,#22347,#3959,.T.);
#27930=EDGE_CURVE('',#21388,#22346,#3960,.T.);
#27931=EDGE_CURVE('',#21389,#22345,#3961,.T.);
#27932=EDGE_CURVE('',#21390,#22344,#3962,.T.);
#27933=EDGE_CURVE('',#21391,#22343,#3963,.T.);
#27934=EDGE_CURVE('',#21392,#22342,#3964,.T.);
#27935=EDGE_CURVE('',#21393,#22341,#3965,.T.);
#27936=EDGE_CURVE('',#21394,#22340,#3966,.T.);
#27937=EDGE_CURVE('',#21395,#22339,#3967,.T.);
#27938=EDGE_CURVE('',#21396,#22338,#3968,.T.);
#27939=EDGE_CURVE('',#21397,#22337,#3969,.T.);
#27940=EDGE_CURVE('',#21398,#22336,#3970,.T.);
#27941=EDGE_CURVE('',#21399,#22335,#3971,.T.);
#27942=EDGE_CURVE('',#22094,#22334,#19104,.T.);
#27943=EDGE_CURVE('',#22348,#21875,#3972,.T.);
#27944=EDGE_CURVE('',#21403,#22348,#3973,.T.);
#27945=EDGE_CURVE('',#22349,#22348,#1574,.T.);
#27946=EDGE_CURVE('',#21404,#22349,#3974,.T.);
#27947=EDGE_CURVE('',#22350,#22349,#1575,.T.);
#27948=EDGE_CURVE('',#21405,#22350,#3975,.T.);
#27949=EDGE_CURVE('',#22351,#22350,#1576,.T.);
#27950=EDGE_CURVE('',#21406,#22351,#3976,.T.);
#27951=EDGE_CURVE('',#22352,#22351,#1577,.T.);
#27952=EDGE_CURVE('',#21407,#22352,#3977,.T.);
#27953=EDGE_CURVE('',#22353,#22352,#1578,.T.);
#27954=EDGE_CURVE('',#21408,#22353,#3978,.T.);
#27955=EDGE_CURVE('',#22354,#22353,#3979,.T.);
#27956=EDGE_CURVE('',#21409,#22354,#3980,.T.);
#27957=EDGE_CURVE('',#22355,#22354,#1579,.T.);
#27958=EDGE_CURVE('',#21410,#22355,#3981,.T.);
#27959=EDGE_CURVE('',#22356,#22355,#1580,.T.);
#27960=EDGE_CURVE('',#21411,#22356,#3982,.T.);
#27961=EDGE_CURVE('',#22357,#22356,#1581,.T.);
#27962=EDGE_CURVE('',#21412,#22357,#3983,.T.);
#27963=EDGE_CURVE('',#22358,#22357,#1582,.T.);
#27964=EDGE_CURVE('',#21413,#22358,#3984,.T.);
#27965=EDGE_CURVE('',#22359,#22358,#1583,.T.);
#27966=EDGE_CURVE('',#21414,#22359,#3985,.T.);
#27967=EDGE_CURVE('',#21968,#22359,#3986,.T.);
#27968=EDGE_CURVE('',#22360,#21874,#19691,.T.);
#27969=EDGE_CURVE('',#22360,#22361,#1584,.T.);
#27970=EDGE_CURVE('',#22361,#22362,#3987,.T.);
#27971=EDGE_CURVE('',#22362,#22363,#1585,.T.);
#27972=EDGE_CURVE('',#22363,#22364,#1586,.T.);
#27973=EDGE_CURVE('',#22364,#22365,#1587,.T.);
#27974=EDGE_CURVE('',#22365,#22366,#1588,.T.);
#27975=EDGE_CURVE('',#22366,#22367,#1589,.T.);
#27976=EDGE_CURVE('',#22367,#22368,#3988,.T.);
#27977=EDGE_CURVE('',#22368,#22369,#1590,.T.);
#27978=EDGE_CURVE('',#22369,#22370,#1591,.T.);
#27979=EDGE_CURVE('',#22370,#22371,#1592,.T.);
#27980=EDGE_CURVE('',#22371,#22372,#1593,.T.);
#27981=EDGE_CURVE('',#22372,#22373,#1594,.T.);
#27982=EDGE_CURVE('',#22373,#21385,#3989,.T.);
#27983=EDGE_CURVE('',#21353,#22373,#3990,.T.);
#27984=EDGE_CURVE('',#21354,#22372,#3991,.T.);
#27985=EDGE_CURVE('',#21355,#22371,#3992,.T.);
#27986=EDGE_CURVE('',#21356,#22370,#3993,.T.);
#27987=EDGE_CURVE('',#21357,#22369,#3994,.T.);
#27988=EDGE_CURVE('',#21358,#22368,#3995,.T.);
#27989=EDGE_CURVE('',#21359,#22367,#3996,.T.);
#27990=EDGE_CURVE('',#21360,#22366,#3997,.T.);
#27991=EDGE_CURVE('',#21361,#22365,#3998,.T.);
#27992=EDGE_CURVE('',#21362,#22364,#3999,.T.);
#27993=EDGE_CURVE('',#21363,#22363,#4000,.T.);
#27994=EDGE_CURVE('',#21364,#22362,#4001,.T.);
#27995=EDGE_CURVE('',#21365,#22361,#4002,.T.);
#27996=EDGE_CURVE('',#22095,#22360,#19105,.T.);
#27997=EDGE_CURVE('',#22374,#21871,#4003,.T.);
#27998=EDGE_CURVE('',#21369,#22374,#4004,.T.);
#27999=EDGE_CURVE('',#22375,#22374,#1595,.T.);
#28000=EDGE_CURVE('',#21370,#22375,#4005,.T.);
#28001=EDGE_CURVE('',#22376,#22375,#1596,.T.);
#28002=EDGE_CURVE('',#21371,#22376,#4006,.T.);
#28003=EDGE_CURVE('',#22377,#22376,#1597,.T.);
#28004=EDGE_CURVE('',#21372,#22377,#4007,.T.);
#28005=EDGE_CURVE('',#22378,#22377,#1598,.T.);
#28006=EDGE_CURVE('',#21373,#22378,#4008,.T.);
#28007=EDGE_CURVE('',#22379,#22378,#1599,.T.);
#28008=EDGE_CURVE('',#21374,#22379,#4009,.T.);
#28009=EDGE_CURVE('',#22380,#22379,#4010,.T.);
#28010=EDGE_CURVE('',#21375,#22380,#4011,.T.);
#28011=EDGE_CURVE('',#22381,#22380,#1600,.T.);
#28012=EDGE_CURVE('',#21376,#22381,#4012,.T.);
#28013=EDGE_CURVE('',#22382,#22381,#1601,.T.);
#28014=EDGE_CURVE('',#21377,#22382,#4013,.T.);
#28015=EDGE_CURVE('',#22383,#22382,#1602,.T.);
#28016=EDGE_CURVE('',#21378,#22383,#4014,.T.);
#28017=EDGE_CURVE('',#22384,#22383,#1603,.T.);
#28018=EDGE_CURVE('',#21379,#22384,#4015,.T.);
#28019=EDGE_CURVE('',#22385,#22384,#1604,.T.);
#28020=EDGE_CURVE('',#21380,#22385,#4016,.T.);
#28021=EDGE_CURVE('',#21971,#22385,#4017,.T.);
#28022=EDGE_CURVE('',#22386,#21870,#19692,.T.);
#28023=EDGE_CURVE('',#22386,#22387,#1605,.T.);
#28024=EDGE_CURVE('',#22387,#22388,#4018,.T.);
#28025=EDGE_CURVE('',#22388,#22389,#1606,.T.);
#28026=EDGE_CURVE('',#22389,#22390,#1607,.T.);
#28027=EDGE_CURVE('',#22390,#22391,#1608,.T.);
#28028=EDGE_CURVE('',#22391,#22392,#1609,.T.);
#28029=EDGE_CURVE('',#22392,#22393,#1610,.T.);
#28030=EDGE_CURVE('',#22393,#22394,#4019,.T.);
#28031=EDGE_CURVE('',#22394,#22395,#1611,.T.);
#28032=EDGE_CURVE('',#22395,#22396,#1612,.T.);
#28033=EDGE_CURVE('',#22396,#22397,#1613,.T.);
#28034=EDGE_CURVE('',#22397,#22398,#1614,.T.);
#28035=EDGE_CURVE('',#22398,#22399,#1615,.T.);
#28036=EDGE_CURVE('',#22399,#21351,#4020,.T.);
#28037=EDGE_CURVE('',#21319,#22399,#4021,.T.);
#28038=EDGE_CURVE('',#21320,#22398,#4022,.T.);
#28039=EDGE_CURVE('',#21321,#22397,#4023,.T.);
#28040=EDGE_CURVE('',#21322,#22396,#4024,.T.);
#28041=EDGE_CURVE('',#21323,#22395,#4025,.T.);
#28042=EDGE_CURVE('',#21324,#22394,#4026,.T.);
#28043=EDGE_CURVE('',#21325,#22393,#4027,.T.);
#28044=EDGE_CURVE('',#21326,#22392,#4028,.T.);
#28045=EDGE_CURVE('',#21327,#22391,#4029,.T.);
#28046=EDGE_CURVE('',#21328,#22390,#4030,.T.);
#28047=EDGE_CURVE('',#21329,#22389,#4031,.T.);
#28048=EDGE_CURVE('',#21330,#22388,#4032,.T.);
#28049=EDGE_CURVE('',#21331,#22387,#4033,.T.);
#28050=EDGE_CURVE('',#22096,#22386,#19106,.T.);
#28051=EDGE_CURVE('',#22400,#21867,#4034,.T.);
#28052=EDGE_CURVE('',#21335,#22400,#4035,.T.);
#28053=EDGE_CURVE('',#22401,#22400,#1616,.T.);
#28054=EDGE_CURVE('',#21336,#22401,#4036,.T.);
#28055=EDGE_CURVE('',#22402,#22401,#1617,.T.);
#28056=EDGE_CURVE('',#21337,#22402,#4037,.T.);
#28057=EDGE_CURVE('',#22403,#22402,#1618,.T.);
#28058=EDGE_CURVE('',#21338,#22403,#4038,.T.);
#28059=EDGE_CURVE('',#22404,#22403,#1619,.T.);
#28060=EDGE_CURVE('',#21339,#22404,#4039,.T.);
#28061=EDGE_CURVE('',#22405,#22404,#1620,.T.);
#28062=EDGE_CURVE('',#21340,#22405,#4040,.T.);
#28063=EDGE_CURVE('',#22406,#22405,#4041,.T.);
#28064=EDGE_CURVE('',#21341,#22406,#4042,.T.);
#28065=EDGE_CURVE('',#22407,#22406,#1621,.T.);
#28066=EDGE_CURVE('',#21342,#22407,#4043,.T.);
#28067=EDGE_CURVE('',#22408,#22407,#1622,.T.);
#28068=EDGE_CURVE('',#21343,#22408,#4044,.T.);
#28069=EDGE_CURVE('',#22409,#22408,#1623,.T.);
#28070=EDGE_CURVE('',#21344,#22409,#4045,.T.);
#28071=EDGE_CURVE('',#22410,#22409,#1624,.T.);
#28072=EDGE_CURVE('',#21345,#22410,#4046,.T.);
#28073=EDGE_CURVE('',#22411,#22410,#1625,.T.);
#28074=EDGE_CURVE('',#21346,#22411,#4047,.T.);
#28075=EDGE_CURVE('',#21974,#22411,#4048,.T.);
#28076=EDGE_CURVE('',#22412,#21866,#19693,.T.);
#28077=EDGE_CURVE('',#22412,#22413,#1626,.T.);
#28078=EDGE_CURVE('',#22413,#22414,#4049,.T.);
#28079=EDGE_CURVE('',#22414,#22415,#1627,.T.);
#28080=EDGE_CURVE('',#22415,#22416,#1628,.T.);
#28081=EDGE_CURVE('',#22416,#22417,#1629,.T.);
#28082=EDGE_CURVE('',#22417,#22418,#1630,.T.);
#28083=EDGE_CURVE('',#22418,#22419,#1631,.T.);
#28084=EDGE_CURVE('',#22419,#22420,#4050,.T.);
#28085=EDGE_CURVE('',#22420,#22421,#1632,.T.);
#28086=EDGE_CURVE('',#22421,#22422,#1633,.T.);
#28087=EDGE_CURVE('',#22422,#22423,#1634,.T.);
#28088=EDGE_CURVE('',#22423,#22424,#1635,.T.);
#28089=EDGE_CURVE('',#22424,#22425,#1636,.T.);
#28090=EDGE_CURVE('',#22425,#21317,#4051,.T.);
#28091=EDGE_CURVE('',#21285,#22425,#4052,.T.);
#28092=EDGE_CURVE('',#21286,#22424,#4053,.T.);
#28093=EDGE_CURVE('',#21287,#22423,#4054,.T.);
#28094=EDGE_CURVE('',#21288,#22422,#4055,.T.);
#28095=EDGE_CURVE('',#21289,#22421,#4056,.T.);
#28096=EDGE_CURVE('',#21290,#22420,#4057,.T.);
#28097=EDGE_CURVE('',#21291,#22419,#4058,.T.);
#28098=EDGE_CURVE('',#21292,#22418,#4059,.T.);
#28099=EDGE_CURVE('',#21293,#22417,#4060,.T.);
#28100=EDGE_CURVE('',#21294,#22416,#4061,.T.);
#28101=EDGE_CURVE('',#21295,#22415,#4062,.T.);
#28102=EDGE_CURVE('',#21296,#22414,#4063,.T.);
#28103=EDGE_CURVE('',#21297,#22413,#4064,.T.);
#28104=EDGE_CURVE('',#22097,#22412,#19107,.T.);
#28105=EDGE_CURVE('',#22426,#21863,#4065,.T.);
#28106=EDGE_CURVE('',#21301,#22426,#4066,.T.);
#28107=EDGE_CURVE('',#22427,#22426,#1637,.T.);
#28108=EDGE_CURVE('',#21302,#22427,#4067,.T.);
#28109=EDGE_CURVE('',#22428,#22427,#1638,.T.);
#28110=EDGE_CURVE('',#21303,#22428,#4068,.T.);
#28111=EDGE_CURVE('',#22429,#22428,#1639,.T.);
#28112=EDGE_CURVE('',#21304,#22429,#4069,.T.);
#28113=EDGE_CURVE('',#22430,#22429,#1640,.T.);
#28114=EDGE_CURVE('',#21305,#22430,#4070,.T.);
#28115=EDGE_CURVE('',#22431,#22430,#1641,.T.);
#28116=EDGE_CURVE('',#21306,#22431,#4071,.T.);
#28117=EDGE_CURVE('',#22432,#22431,#4072,.T.);
#28118=EDGE_CURVE('',#21307,#22432,#4073,.T.);
#28119=EDGE_CURVE('',#22433,#22432,#1642,.T.);
#28120=EDGE_CURVE('',#21308,#22433,#4074,.T.);
#28121=EDGE_CURVE('',#22434,#22433,#1643,.T.);
#28122=EDGE_CURVE('',#21309,#22434,#4075,.T.);
#28123=EDGE_CURVE('',#22435,#22434,#1644,.T.);
#28124=EDGE_CURVE('',#21310,#22435,#4076,.T.);
#28125=EDGE_CURVE('',#22436,#22435,#1645,.T.);
#28126=EDGE_CURVE('',#21311,#22436,#4077,.T.);
#28127=EDGE_CURVE('',#22437,#22436,#1646,.T.);
#28128=EDGE_CURVE('',#21312,#22437,#4078,.T.);
#28129=EDGE_CURVE('',#21977,#22437,#4079,.T.);
#28130=EDGE_CURVE('',#22438,#21862,#19694,.T.);
#28131=EDGE_CURVE('',#22438,#22439,#1647,.T.);
#28132=EDGE_CURVE('',#22439,#22440,#4080,.T.);
#28133=EDGE_CURVE('',#22440,#22441,#1648,.T.);
#28134=EDGE_CURVE('',#22441,#22442,#1649,.T.);
#28135=EDGE_CURVE('',#22442,#22443,#1650,.T.);
#28136=EDGE_CURVE('',#22443,#22444,#1651,.T.);
#28137=EDGE_CURVE('',#22444,#22445,#1652,.T.);
#28138=EDGE_CURVE('',#22445,#22446,#4081,.T.);
#28139=EDGE_CURVE('',#22446,#22447,#1653,.T.);
#28140=EDGE_CURVE('',#22447,#22448,#1654,.T.);
#28141=EDGE_CURVE('',#22448,#22449,#1655,.T.);
#28142=EDGE_CURVE('',#22449,#22450,#1656,.T.);
#28143=EDGE_CURVE('',#22450,#22451,#1657,.T.);
#28144=EDGE_CURVE('',#22451,#21283,#4082,.T.);
#28145=EDGE_CURVE('',#21251,#22451,#4083,.T.);
#28146=EDGE_CURVE('',#21252,#22450,#4084,.T.);
#28147=EDGE_CURVE('',#21253,#22449,#4085,.T.);
#28148=EDGE_CURVE('',#21254,#22448,#4086,.T.);
#28149=EDGE_CURVE('',#21255,#22447,#4087,.T.);
#28150=EDGE_CURVE('',#21256,#22446,#4088,.T.);
#28151=EDGE_CURVE('',#21257,#22445,#4089,.T.);
#28152=EDGE_CURVE('',#21258,#22444,#4090,.T.);
#28153=EDGE_CURVE('',#21259,#22443,#4091,.T.);
#28154=EDGE_CURVE('',#21260,#22442,#4092,.T.);
#28155=EDGE_CURVE('',#21261,#22441,#4093,.T.);
#28156=EDGE_CURVE('',#21262,#22440,#4094,.T.);
#28157=EDGE_CURVE('',#21263,#22439,#4095,.T.);
#28158=EDGE_CURVE('',#22098,#22438,#19108,.T.);
#28159=EDGE_CURVE('',#22452,#21859,#4096,.T.);
#28160=EDGE_CURVE('',#21267,#22452,#4097,.T.);
#28161=EDGE_CURVE('',#22453,#22452,#1658,.T.);
#28162=EDGE_CURVE('',#21268,#22453,#4098,.T.);
#28163=EDGE_CURVE('',#22454,#22453,#1659,.T.);
#28164=EDGE_CURVE('',#21269,#22454,#4099,.T.);
#28165=EDGE_CURVE('',#22455,#22454,#1660,.T.);
#28166=EDGE_CURVE('',#21270,#22455,#4100,.T.);
#28167=EDGE_CURVE('',#22456,#22455,#1661,.T.);
#28168=EDGE_CURVE('',#21271,#22456,#4101,.T.);
#28169=EDGE_CURVE('',#22457,#22456,#1662,.T.);
#28170=EDGE_CURVE('',#21272,#22457,#4102,.T.);
#28171=EDGE_CURVE('',#22458,#22457,#4103,.T.);
#28172=EDGE_CURVE('',#21273,#22458,#4104,.T.);
#28173=EDGE_CURVE('',#22459,#22458,#1663,.T.);
#28174=EDGE_CURVE('',#21274,#22459,#4105,.T.);
#28175=EDGE_CURVE('',#22460,#22459,#1664,.T.);
#28176=EDGE_CURVE('',#21275,#22460,#4106,.T.);
#28177=EDGE_CURVE('',#22461,#22460,#1665,.T.);
#28178=EDGE_CURVE('',#21276,#22461,#4107,.T.);
#28179=EDGE_CURVE('',#22462,#22461,#1666,.T.);
#28180=EDGE_CURVE('',#21277,#22462,#4108,.T.);
#28181=EDGE_CURVE('',#22463,#22462,#1667,.T.);
#28182=EDGE_CURVE('',#21278,#22463,#4109,.T.);
#28183=EDGE_CURVE('',#21980,#22463,#4110,.T.);
#28184=EDGE_CURVE('',#22464,#21858,#19695,.T.);
#28185=EDGE_CURVE('',#22464,#22465,#1668,.T.);
#28186=EDGE_CURVE('',#22465,#22466,#4111,.T.);
#28187=EDGE_CURVE('',#22466,#22467,#1669,.T.);
#28188=EDGE_CURVE('',#22467,#22468,#1670,.T.);
#28189=EDGE_CURVE('',#22468,#22469,#1671,.T.);
#28190=EDGE_CURVE('',#22469,#22470,#1672,.T.);
#28191=EDGE_CURVE('',#22470,#22471,#1673,.T.);
#28192=EDGE_CURVE('',#22471,#22472,#4112,.T.);
#28193=EDGE_CURVE('',#22472,#22473,#1674,.T.);
#28194=EDGE_CURVE('',#22473,#22474,#1675,.T.);
#28195=EDGE_CURVE('',#22474,#22475,#1676,.T.);
#28196=EDGE_CURVE('',#22475,#22476,#1677,.T.);
#28197=EDGE_CURVE('',#22476,#22477,#1678,.T.);
#28198=EDGE_CURVE('',#22477,#21249,#4113,.T.);
#28199=EDGE_CURVE('',#21217,#22477,#4114,.T.);
#28200=EDGE_CURVE('',#21218,#22476,#4115,.T.);
#28201=EDGE_CURVE('',#21219,#22475,#4116,.T.);
#28202=EDGE_CURVE('',#21220,#22474,#4117,.T.);
#28203=EDGE_CURVE('',#21221,#22473,#4118,.T.);
#28204=EDGE_CURVE('',#21222,#22472,#4119,.T.);
#28205=EDGE_CURVE('',#21223,#22471,#4120,.T.);
#28206=EDGE_CURVE('',#21224,#22470,#4121,.T.);
#28207=EDGE_CURVE('',#21225,#22469,#4122,.T.);
#28208=EDGE_CURVE('',#21226,#22468,#4123,.T.);
#28209=EDGE_CURVE('',#21227,#22467,#4124,.T.);
#28210=EDGE_CURVE('',#21228,#22466,#4125,.T.);
#28211=EDGE_CURVE('',#21229,#22465,#4126,.T.);
#28212=EDGE_CURVE('',#22099,#22464,#19109,.T.);
#28213=EDGE_CURVE('',#22478,#21855,#4127,.T.);
#28214=EDGE_CURVE('',#21233,#22478,#4128,.T.);
#28215=EDGE_CURVE('',#22479,#22478,#1679,.T.);
#28216=EDGE_CURVE('',#21234,#22479,#4129,.T.);
#28217=EDGE_CURVE('',#22480,#22479,#1680,.T.);
#28218=EDGE_CURVE('',#21235,#22480,#4130,.T.);
#28219=EDGE_CURVE('',#22481,#22480,#1681,.T.);
#28220=EDGE_CURVE('',#21236,#22481,#4131,.T.);
#28221=EDGE_CURVE('',#22482,#22481,#1682,.T.);
#28222=EDGE_CURVE('',#21237,#22482,#4132,.T.);
#28223=EDGE_CURVE('',#22483,#22482,#1683,.T.);
#28224=EDGE_CURVE('',#21238,#22483,#4133,.T.);
#28225=EDGE_CURVE('',#22484,#22483,#4134,.T.);
#28226=EDGE_CURVE('',#21239,#22484,#4135,.T.);
#28227=EDGE_CURVE('',#22485,#22484,#1684,.T.);
#28228=EDGE_CURVE('',#21240,#22485,#4136,.T.);
#28229=EDGE_CURVE('',#22486,#22485,#1685,.T.);
#28230=EDGE_CURVE('',#21241,#22486,#4137,.T.);
#28231=EDGE_CURVE('',#22487,#22486,#1686,.T.);
#28232=EDGE_CURVE('',#21242,#22487,#4138,.T.);
#28233=EDGE_CURVE('',#22488,#22487,#1687,.T.);
#28234=EDGE_CURVE('',#21243,#22488,#4139,.T.);
#28235=EDGE_CURVE('',#22489,#22488,#1688,.T.);
#28236=EDGE_CURVE('',#21244,#22489,#4140,.T.);
#28237=EDGE_CURVE('',#21983,#22489,#4141,.T.);
#28238=EDGE_CURVE('',#22490,#21854,#19696,.T.);
#28239=EDGE_CURVE('',#22490,#22491,#1689,.T.);
#28240=EDGE_CURVE('',#22491,#22492,#4142,.T.);
#28241=EDGE_CURVE('',#22492,#22493,#1690,.T.);
#28242=EDGE_CURVE('',#22493,#22494,#1691,.T.);
#28243=EDGE_CURVE('',#22494,#22495,#1692,.T.);
#28244=EDGE_CURVE('',#22495,#22496,#1693,.T.);
#28245=EDGE_CURVE('',#22496,#22497,#1694,.T.);
#28246=EDGE_CURVE('',#22497,#22498,#4143,.T.);
#28247=EDGE_CURVE('',#22498,#22499,#1695,.T.);
#28248=EDGE_CURVE('',#22499,#22500,#1696,.T.);
#28249=EDGE_CURVE('',#22500,#22501,#1697,.T.);
#28250=EDGE_CURVE('',#22501,#22502,#1698,.T.);
#28251=EDGE_CURVE('',#22502,#22503,#1699,.T.);
#28252=EDGE_CURVE('',#22503,#21215,#4144,.T.);
#28253=EDGE_CURVE('',#21183,#22503,#4145,.T.);
#28254=EDGE_CURVE('',#21184,#22502,#4146,.T.);
#28255=EDGE_CURVE('',#21185,#22501,#4147,.T.);
#28256=EDGE_CURVE('',#21186,#22500,#4148,.T.);
#28257=EDGE_CURVE('',#21187,#22499,#4149,.T.);
#28258=EDGE_CURVE('',#21188,#22498,#4150,.T.);
#28259=EDGE_CURVE('',#21189,#22497,#4151,.T.);
#28260=EDGE_CURVE('',#21190,#22496,#4152,.T.);
#28261=EDGE_CURVE('',#21191,#22495,#4153,.T.);
#28262=EDGE_CURVE('',#21192,#22494,#4154,.T.);
#28263=EDGE_CURVE('',#21193,#22493,#4155,.T.);
#28264=EDGE_CURVE('',#21194,#22492,#4156,.T.);
#28265=EDGE_CURVE('',#21195,#22491,#4157,.T.);
#28266=EDGE_CURVE('',#22100,#22490,#19110,.T.);
#28267=EDGE_CURVE('',#22504,#21851,#4158,.T.);
#28268=EDGE_CURVE('',#21199,#22504,#4159,.T.);
#28269=EDGE_CURVE('',#22505,#22504,#1700,.T.);
#28270=EDGE_CURVE('',#21200,#22505,#4160,.T.);
#28271=EDGE_CURVE('',#22506,#22505,#1701,.T.);
#28272=EDGE_CURVE('',#21201,#22506,#4161,.T.);
#28273=EDGE_CURVE('',#22507,#22506,#1702,.T.);
#28274=EDGE_CURVE('',#21202,#22507,#4162,.T.);
#28275=EDGE_CURVE('',#22508,#22507,#1703,.T.);
#28276=EDGE_CURVE('',#21203,#22508,#4163,.T.);
#28277=EDGE_CURVE('',#22509,#22508,#1704,.T.);
#28278=EDGE_CURVE('',#21204,#22509,#4164,.T.);
#28279=EDGE_CURVE('',#22510,#22509,#4165,.T.);
#28280=EDGE_CURVE('',#21205,#22510,#4166,.T.);
#28281=EDGE_CURVE('',#22511,#22510,#1705,.T.);
#28282=EDGE_CURVE('',#21206,#22511,#4167,.T.);
#28283=EDGE_CURVE('',#22512,#22511,#1706,.T.);
#28284=EDGE_CURVE('',#21207,#22512,#4168,.T.);
#28285=EDGE_CURVE('',#22513,#22512,#1707,.T.);
#28286=EDGE_CURVE('',#21208,#22513,#4169,.T.);
#28287=EDGE_CURVE('',#22514,#22513,#1708,.T.);
#28288=EDGE_CURVE('',#21209,#22514,#4170,.T.);
#28289=EDGE_CURVE('',#22515,#22514,#1709,.T.);
#28290=EDGE_CURVE('',#21210,#22515,#4171,.T.);
#28291=EDGE_CURVE('',#21986,#22515,#4172,.T.);
#28292=EDGE_CURVE('',#22516,#21850,#19697,.T.);
#28293=EDGE_CURVE('',#22516,#22517,#1710,.T.);
#28294=EDGE_CURVE('',#22517,#22518,#4173,.T.);
#28295=EDGE_CURVE('',#22518,#22519,#1711,.T.);
#28296=EDGE_CURVE('',#22519,#22520,#1712,.T.);
#28297=EDGE_CURVE('',#22520,#22521,#1713,.T.);
#28298=EDGE_CURVE('',#22521,#22522,#1714,.T.);
#28299=EDGE_CURVE('',#22522,#22523,#1715,.T.);
#28300=EDGE_CURVE('',#22523,#22524,#4174,.T.);
#28301=EDGE_CURVE('',#22524,#22525,#1716,.T.);
#28302=EDGE_CURVE('',#22525,#22526,#1717,.T.);
#28303=EDGE_CURVE('',#22526,#22527,#1718,.T.);
#28304=EDGE_CURVE('',#22527,#22528,#1719,.T.);
#28305=EDGE_CURVE('',#22528,#22529,#1720,.T.);
#28306=EDGE_CURVE('',#22529,#21181,#4175,.T.);
#28307=EDGE_CURVE('',#21149,#22529,#4176,.T.);
#28308=EDGE_CURVE('',#21150,#22528,#4177,.T.);
#28309=EDGE_CURVE('',#21151,#22527,#4178,.T.);
#28310=EDGE_CURVE('',#21152,#22526,#4179,.T.);
#28311=EDGE_CURVE('',#21153,#22525,#4180,.T.);
#28312=EDGE_CURVE('',#21154,#22524,#4181,.T.);
#28313=EDGE_CURVE('',#21155,#22523,#4182,.T.);
#28314=EDGE_CURVE('',#21156,#22522,#4183,.T.);
#28315=EDGE_CURVE('',#21157,#22521,#4184,.T.);
#28316=EDGE_CURVE('',#21158,#22520,#4185,.T.);
#28317=EDGE_CURVE('',#21159,#22519,#4186,.T.);
#28318=EDGE_CURVE('',#21160,#22518,#4187,.T.);
#28319=EDGE_CURVE('',#21161,#22517,#4188,.T.);
#28320=EDGE_CURVE('',#22101,#22516,#19111,.T.);
#28321=EDGE_CURVE('',#22530,#21847,#4189,.T.);
#28322=EDGE_CURVE('',#21165,#22530,#4190,.T.);
#28323=EDGE_CURVE('',#22531,#22530,#1721,.T.);
#28324=EDGE_CURVE('',#21166,#22531,#4191,.T.);
#28325=EDGE_CURVE('',#22532,#22531,#1722,.T.);
#28326=EDGE_CURVE('',#21167,#22532,#4192,.T.);
#28327=EDGE_CURVE('',#22533,#22532,#1723,.T.);
#28328=EDGE_CURVE('',#21168,#22533,#4193,.T.);
#28329=EDGE_CURVE('',#22534,#22533,#1724,.T.);
#28330=EDGE_CURVE('',#21169,#22534,#4194,.T.);
#28331=EDGE_CURVE('',#22535,#22534,#1725,.T.);
#28332=EDGE_CURVE('',#21170,#22535,#4195,.T.);
#28333=EDGE_CURVE('',#22536,#22535,#4196,.T.);
#28334=EDGE_CURVE('',#21171,#22536,#4197,.T.);
#28335=EDGE_CURVE('',#22537,#22536,#1726,.T.);
#28336=EDGE_CURVE('',#21172,#22537,#4198,.T.);
#28337=EDGE_CURVE('',#22538,#22537,#1727,.T.);
#28338=EDGE_CURVE('',#21173,#22538,#4199,.T.);
#28339=EDGE_CURVE('',#22539,#22538,#1728,.T.);
#28340=EDGE_CURVE('',#21174,#22539,#4200,.T.);
#28341=EDGE_CURVE('',#22540,#22539,#1729,.T.);
#28342=EDGE_CURVE('',#21175,#22540,#4201,.T.);
#28343=EDGE_CURVE('',#22541,#22540,#1730,.T.);
#28344=EDGE_CURVE('',#21176,#22541,#4202,.T.);
#28345=EDGE_CURVE('',#21989,#22541,#4203,.T.);
#28346=EDGE_CURVE('',#22542,#21846,#19698,.T.);
#28347=EDGE_CURVE('',#22542,#22543,#1731,.T.);
#28348=EDGE_CURVE('',#22543,#22544,#4204,.T.);
#28349=EDGE_CURVE('',#22544,#22545,#1732,.T.);
#28350=EDGE_CURVE('',#22545,#22546,#1733,.T.);
#28351=EDGE_CURVE('',#22546,#22547,#1734,.T.);
#28352=EDGE_CURVE('',#22547,#22548,#1735,.T.);
#28353=EDGE_CURVE('',#22548,#22549,#1736,.T.);
#28354=EDGE_CURVE('',#22549,#22550,#4205,.T.);
#28355=EDGE_CURVE('',#22550,#22551,#1737,.T.);
#28356=EDGE_CURVE('',#22551,#22552,#1738,.T.);
#28357=EDGE_CURVE('',#22552,#22553,#1739,.T.);
#28358=EDGE_CURVE('',#22553,#22554,#1740,.T.);
#28359=EDGE_CURVE('',#22554,#22555,#1741,.T.);
#28360=EDGE_CURVE('',#22555,#21147,#4206,.T.);
#28361=EDGE_CURVE('',#21115,#22555,#4207,.T.);
#28362=EDGE_CURVE('',#21116,#22554,#4208,.T.);
#28363=EDGE_CURVE('',#21117,#22553,#4209,.T.);
#28364=EDGE_CURVE('',#21118,#22552,#4210,.T.);
#28365=EDGE_CURVE('',#21119,#22551,#4211,.T.);
#28366=EDGE_CURVE('',#21120,#22550,#4212,.T.);
#28367=EDGE_CURVE('',#21121,#22549,#4213,.T.);
#28368=EDGE_CURVE('',#21122,#22548,#4214,.T.);
#28369=EDGE_CURVE('',#21123,#22547,#4215,.T.);
#28370=EDGE_CURVE('',#21124,#22546,#4216,.T.);
#28371=EDGE_CURVE('',#21125,#22545,#4217,.T.);
#28372=EDGE_CURVE('',#21126,#22544,#4218,.T.);
#28373=EDGE_CURVE('',#21127,#22543,#4219,.T.);
#28374=EDGE_CURVE('',#22102,#22542,#19112,.T.);
#28375=EDGE_CURVE('',#22556,#21843,#4220,.T.);
#28376=EDGE_CURVE('',#21131,#22556,#4221,.T.);
#28377=EDGE_CURVE('',#22557,#22556,#1742,.T.);
#28378=EDGE_CURVE('',#21132,#22557,#4222,.T.);
#28379=EDGE_CURVE('',#22558,#22557,#1743,.T.);
#28380=EDGE_CURVE('',#21133,#22558,#4223,.T.);
#28381=EDGE_CURVE('',#22559,#22558,#1744,.T.);
#28382=EDGE_CURVE('',#21134,#22559,#4224,.T.);
#28383=EDGE_CURVE('',#22560,#22559,#1745,.T.);
#28384=EDGE_CURVE('',#21135,#22560,#4225,.T.);
#28385=EDGE_CURVE('',#22561,#22560,#1746,.T.);
#28386=EDGE_CURVE('',#21136,#22561,#4226,.T.);
#28387=EDGE_CURVE('',#22562,#22561,#4227,.T.);
#28388=EDGE_CURVE('',#21137,#22562,#4228,.T.);
#28389=EDGE_CURVE('',#22563,#22562,#1747,.T.);
#28390=EDGE_CURVE('',#21138,#22563,#4229,.T.);
#28391=EDGE_CURVE('',#22564,#22563,#1748,.T.);
#28392=EDGE_CURVE('',#21139,#22564,#4230,.T.);
#28393=EDGE_CURVE('',#22565,#22564,#1749,.T.);
#28394=EDGE_CURVE('',#21140,#22565,#4231,.T.);
#28395=EDGE_CURVE('',#22566,#22565,#1750,.T.);
#28396=EDGE_CURVE('',#21141,#22566,#4232,.T.);
#28397=EDGE_CURVE('',#22567,#22566,#1751,.T.);
#28398=EDGE_CURVE('',#21142,#22567,#4233,.T.);
#28399=EDGE_CURVE('',#21992,#22567,#4234,.T.);
#28400=EDGE_CURVE('',#22568,#21842,#19699,.T.);
#28401=EDGE_CURVE('',#22568,#22569,#1752,.T.);
#28402=EDGE_CURVE('',#22569,#22570,#4235,.T.);
#28403=EDGE_CURVE('',#22570,#22571,#1753,.T.);
#28404=EDGE_CURVE('',#22571,#22572,#1754,.T.);
#28405=EDGE_CURVE('',#22572,#22573,#1755,.T.);
#28406=EDGE_CURVE('',#22573,#22574,#1756,.T.);
#28407=EDGE_CURVE('',#22574,#22575,#1757,.T.);
#28408=EDGE_CURVE('',#22575,#22576,#4236,.T.);
#28409=EDGE_CURVE('',#22576,#22577,#1758,.T.);
#28410=EDGE_CURVE('',#22577,#22578,#1759,.T.);
#28411=EDGE_CURVE('',#22578,#22579,#1760,.T.);
#28412=EDGE_CURVE('',#22579,#22580,#1761,.T.);
#28413=EDGE_CURVE('',#22580,#22581,#1762,.T.);
#28414=EDGE_CURVE('',#22581,#21113,#4237,.T.);
#28415=EDGE_CURVE('',#21081,#22581,#4238,.T.);
#28416=EDGE_CURVE('',#21082,#22580,#4239,.T.);
#28417=EDGE_CURVE('',#21083,#22579,#4240,.T.);
#28418=EDGE_CURVE('',#21084,#22578,#4241,.T.);
#28419=EDGE_CURVE('',#21085,#22577,#4242,.T.);
#28420=EDGE_CURVE('',#21086,#22576,#4243,.T.);
#28421=EDGE_CURVE('',#21087,#22575,#4244,.T.);
#28422=EDGE_CURVE('',#21088,#22574,#4245,.T.);
#28423=EDGE_CURVE('',#21089,#22573,#4246,.T.);
#28424=EDGE_CURVE('',#21090,#22572,#4247,.T.);
#28425=EDGE_CURVE('',#21091,#22571,#4248,.T.);
#28426=EDGE_CURVE('',#21092,#22570,#4249,.T.);
#28427=EDGE_CURVE('',#21093,#22569,#4250,.T.);
#28428=EDGE_CURVE('',#22103,#22568,#19113,.T.);
#28429=EDGE_CURVE('',#22582,#21839,#4251,.T.);
#28430=EDGE_CURVE('',#21097,#22582,#4252,.T.);
#28431=EDGE_CURVE('',#22583,#22582,#1763,.T.);
#28432=EDGE_CURVE('',#21098,#22583,#4253,.T.);
#28433=EDGE_CURVE('',#22584,#22583,#1764,.T.);
#28434=EDGE_CURVE('',#21099,#22584,#4254,.T.);
#28435=EDGE_CURVE('',#22585,#22584,#1765,.T.);
#28436=EDGE_CURVE('',#21100,#22585,#4255,.T.);
#28437=EDGE_CURVE('',#22586,#22585,#1766,.T.);
#28438=EDGE_CURVE('',#21101,#22586,#4256,.T.);
#28439=EDGE_CURVE('',#22587,#22586,#1767,.T.);
#28440=EDGE_CURVE('',#21102,#22587,#4257,.T.);
#28441=EDGE_CURVE('',#22588,#22587,#4258,.T.);
#28442=EDGE_CURVE('',#21103,#22588,#4259,.T.);
#28443=EDGE_CURVE('',#22589,#22588,#1768,.T.);
#28444=EDGE_CURVE('',#21104,#22589,#4260,.T.);
#28445=EDGE_CURVE('',#22590,#22589,#1769,.T.);
#28446=EDGE_CURVE('',#21105,#22590,#4261,.T.);
#28447=EDGE_CURVE('',#22591,#22590,#1770,.T.);
#28448=EDGE_CURVE('',#21106,#22591,#4262,.T.);
#28449=EDGE_CURVE('',#22592,#22591,#1771,.T.);
#28450=EDGE_CURVE('',#21107,#22592,#4263,.T.);
#28451=EDGE_CURVE('',#22593,#22592,#1772,.T.);
#28452=EDGE_CURVE('',#21108,#22593,#4264,.T.);
#28453=EDGE_CURVE('',#21995,#22593,#4265,.T.);
#28454=EDGE_CURVE('',#22594,#21838,#19700,.T.);
#28455=EDGE_CURVE('',#22594,#22595,#1773,.T.);
#28456=EDGE_CURVE('',#22595,#22596,#4266,.T.);
#28457=EDGE_CURVE('',#22596,#22597,#1774,.T.);
#28458=EDGE_CURVE('',#22597,#22598,#1775,.T.);
#28459=EDGE_CURVE('',#22598,#22599,#1776,.T.);
#28460=EDGE_CURVE('',#22599,#22600,#1777,.T.);
#28461=EDGE_CURVE('',#22600,#22601,#1778,.T.);
#28462=EDGE_CURVE('',#22601,#22602,#4267,.T.);
#28463=EDGE_CURVE('',#22602,#22603,#1779,.T.);
#28464=EDGE_CURVE('',#22603,#22604,#1780,.T.);
#28465=EDGE_CURVE('',#22604,#22605,#1781,.T.);
#28466=EDGE_CURVE('',#22605,#22606,#1782,.T.);
#28467=EDGE_CURVE('',#22606,#22607,#1783,.T.);
#28468=EDGE_CURVE('',#22607,#21079,#4268,.T.);
#28469=EDGE_CURVE('',#21047,#22607,#4269,.T.);
#28470=EDGE_CURVE('',#21048,#22606,#4270,.T.);
#28471=EDGE_CURVE('',#21049,#22605,#4271,.T.);
#28472=EDGE_CURVE('',#21050,#22604,#4272,.T.);
#28473=EDGE_CURVE('',#21051,#22603,#4273,.T.);
#28474=EDGE_CURVE('',#21052,#22602,#4274,.T.);
#28475=EDGE_CURVE('',#21053,#22601,#4275,.T.);
#28476=EDGE_CURVE('',#21054,#22600,#4276,.T.);
#28477=EDGE_CURVE('',#21055,#22599,#4277,.T.);
#28478=EDGE_CURVE('',#21056,#22598,#4278,.T.);
#28479=EDGE_CURVE('',#21057,#22597,#4279,.T.);
#28480=EDGE_CURVE('',#21058,#22596,#4280,.T.);
#28481=EDGE_CURVE('',#21059,#22595,#4281,.T.);
#28482=EDGE_CURVE('',#22105,#22594,#19114,.T.);
#28483=EDGE_CURVE('',#22608,#21835,#4282,.T.);
#28484=EDGE_CURVE('',#21063,#22608,#4283,.T.);
#28485=EDGE_CURVE('',#22609,#22608,#1784,.T.);
#28486=EDGE_CURVE('',#21064,#22609,#4284,.T.);
#28487=EDGE_CURVE('',#22610,#22609,#1785,.T.);
#28488=EDGE_CURVE('',#21065,#22610,#4285,.T.);
#28489=EDGE_CURVE('',#22611,#22610,#1786,.T.);
#28490=EDGE_CURVE('',#21066,#22611,#4286,.T.);
#28491=EDGE_CURVE('',#22612,#22611,#1787,.T.);
#28492=EDGE_CURVE('',#21067,#22612,#4287,.T.);
#28493=EDGE_CURVE('',#22613,#22612,#1788,.T.);
#28494=EDGE_CURVE('',#21068,#22613,#4288,.T.);
#28495=EDGE_CURVE('',#22614,#22613,#4289,.T.);
#28496=EDGE_CURVE('',#21069,#22614,#4290,.T.);
#28497=EDGE_CURVE('',#22615,#22614,#1789,.T.);
#28498=EDGE_CURVE('',#21070,#22615,#4291,.T.);
#28499=EDGE_CURVE('',#22616,#22615,#1790,.T.);
#28500=EDGE_CURVE('',#21071,#22616,#4292,.T.);
#28501=EDGE_CURVE('',#22617,#22616,#1791,.T.);
#28502=EDGE_CURVE('',#21072,#22617,#4293,.T.);
#28503=EDGE_CURVE('',#22618,#22617,#1792,.T.);
#28504=EDGE_CURVE('',#21073,#22618,#4294,.T.);
#28505=EDGE_CURVE('',#22619,#22618,#1793,.T.);
#28506=EDGE_CURVE('',#21074,#22619,#4295,.T.);
#28507=EDGE_CURVE('',#21998,#22619,#4296,.T.);
#28508=EDGE_CURVE('',#22620,#21834,#19701,.T.);
#28509=EDGE_CURVE('',#22620,#22621,#1794,.T.);
#28510=EDGE_CURVE('',#22621,#22622,#4297,.T.);
#28511=EDGE_CURVE('',#22622,#22623,#1795,.T.);
#28512=EDGE_CURVE('',#22623,#22624,#1796,.T.);
#28513=EDGE_CURVE('',#22624,#22625,#1797,.T.);
#28514=EDGE_CURVE('',#22625,#22626,#1798,.T.);
#28515=EDGE_CURVE('',#22626,#22627,#1799,.T.);
#28516=EDGE_CURVE('',#22627,#22628,#4298,.T.);
#28517=EDGE_CURVE('',#22628,#22629,#1800,.T.);
#28518=EDGE_CURVE('',#22629,#22630,#1801,.T.);
#28519=EDGE_CURVE('',#22630,#22631,#1802,.T.);
#28520=EDGE_CURVE('',#22631,#22632,#1803,.T.);
#28521=EDGE_CURVE('',#22632,#22633,#1804,.T.);
#28522=EDGE_CURVE('',#22633,#21045,#4299,.T.);
#28523=EDGE_CURVE('',#21013,#22633,#4300,.T.);
#28524=EDGE_CURVE('',#21014,#22632,#4301,.T.);
#28525=EDGE_CURVE('',#21015,#22631,#4302,.T.);
#28526=EDGE_CURVE('',#21016,#22630,#4303,.T.);
#28527=EDGE_CURVE('',#21017,#22629,#4304,.T.);
#28528=EDGE_CURVE('',#21018,#22628,#4305,.T.);
#28529=EDGE_CURVE('',#21019,#22627,#4306,.T.);
#28530=EDGE_CURVE('',#21020,#22626,#4307,.T.);
#28531=EDGE_CURVE('',#21021,#22625,#4308,.T.);
#28532=EDGE_CURVE('',#21022,#22624,#4309,.T.);
#28533=EDGE_CURVE('',#21023,#22623,#4310,.T.);
#28534=EDGE_CURVE('',#21024,#22622,#4311,.T.);
#28535=EDGE_CURVE('',#21025,#22621,#4312,.T.);
#28536=EDGE_CURVE('',#22106,#22620,#19115,.T.);
#28537=EDGE_CURVE('',#22634,#21831,#4313,.T.);
#28538=EDGE_CURVE('',#21029,#22634,#4314,.T.);
#28539=EDGE_CURVE('',#22635,#22634,#1805,.T.);
#28540=EDGE_CURVE('',#21030,#22635,#4315,.T.);
#28541=EDGE_CURVE('',#22636,#22635,#1806,.T.);
#28542=EDGE_CURVE('',#21031,#22636,#4316,.T.);
#28543=EDGE_CURVE('',#22637,#22636,#1807,.T.);
#28544=EDGE_CURVE('',#21032,#22637,#4317,.T.);
#28545=EDGE_CURVE('',#22638,#22637,#1808,.T.);
#28546=EDGE_CURVE('',#21033,#22638,#4318,.T.);
#28547=EDGE_CURVE('',#22639,#22638,#1809,.T.);
#28548=EDGE_CURVE('',#21034,#22639,#4319,.T.);
#28549=EDGE_CURVE('',#22640,#22639,#4320,.T.);
#28550=EDGE_CURVE('',#21035,#22640,#4321,.T.);
#28551=EDGE_CURVE('',#22641,#22640,#1810,.T.);
#28552=EDGE_CURVE('',#21036,#22641,#4322,.T.);
#28553=EDGE_CURVE('',#22642,#22641,#1811,.T.);
#28554=EDGE_CURVE('',#21037,#22642,#4323,.T.);
#28555=EDGE_CURVE('',#22643,#22642,#1812,.T.);
#28556=EDGE_CURVE('',#21038,#22643,#4324,.T.);
#28557=EDGE_CURVE('',#22644,#22643,#1813,.T.);
#28558=EDGE_CURVE('',#21039,#22644,#4325,.T.);
#28559=EDGE_CURVE('',#22645,#22644,#1814,.T.);
#28560=EDGE_CURVE('',#21040,#22645,#4326,.T.);
#28561=EDGE_CURVE('',#22001,#22645,#4327,.T.);
#28562=EDGE_CURVE('',#22646,#21830,#19702,.T.);
#28563=EDGE_CURVE('',#22646,#22647,#1815,.T.);
#28564=EDGE_CURVE('',#22647,#22648,#4328,.T.);
#28565=EDGE_CURVE('',#22648,#22649,#1816,.T.);
#28566=EDGE_CURVE('',#22649,#22650,#1817,.T.);
#28567=EDGE_CURVE('',#22650,#22651,#1818,.T.);
#28568=EDGE_CURVE('',#22651,#22652,#1819,.T.);
#28569=EDGE_CURVE('',#22652,#22653,#1820,.T.);
#28570=EDGE_CURVE('',#22653,#22654,#4329,.T.);
#28571=EDGE_CURVE('',#22654,#22655,#1821,.T.);
#28572=EDGE_CURVE('',#22655,#22656,#1822,.T.);
#28573=EDGE_CURVE('',#22656,#22657,#1823,.T.);
#28574=EDGE_CURVE('',#22657,#22658,#1824,.T.);
#28575=EDGE_CURVE('',#22658,#22659,#1825,.T.);
#28576=EDGE_CURVE('',#22659,#21011,#4330,.T.);
#28577=EDGE_CURVE('',#20979,#22659,#4331,.T.);
#28578=EDGE_CURVE('',#20980,#22658,#4332,.T.);
#28579=EDGE_CURVE('',#20981,#22657,#4333,.T.);
#28580=EDGE_CURVE('',#20982,#22656,#4334,.T.);
#28581=EDGE_CURVE('',#20983,#22655,#4335,.T.);
#28582=EDGE_CURVE('',#20984,#22654,#4336,.T.);
#28583=EDGE_CURVE('',#20985,#22653,#4337,.T.);
#28584=EDGE_CURVE('',#20986,#22652,#4338,.T.);
#28585=EDGE_CURVE('',#20987,#22651,#4339,.T.);
#28586=EDGE_CURVE('',#20988,#22650,#4340,.T.);
#28587=EDGE_CURVE('',#20989,#22649,#4341,.T.);
#28588=EDGE_CURVE('',#20990,#22648,#4342,.T.);
#28589=EDGE_CURVE('',#20991,#22647,#4343,.T.);
#28590=EDGE_CURVE('',#22107,#22646,#19116,.T.);
#28591=EDGE_CURVE('',#22660,#21827,#4344,.T.);
#28592=EDGE_CURVE('',#20995,#22660,#4345,.T.);
#28593=EDGE_CURVE('',#22661,#22660,#1826,.T.);
#28594=EDGE_CURVE('',#20996,#22661,#4346,.T.);
#28595=EDGE_CURVE('',#22662,#22661,#1827,.T.);
#28596=EDGE_CURVE('',#20997,#22662,#4347,.T.);
#28597=EDGE_CURVE('',#22663,#22662,#1828,.T.);
#28598=EDGE_CURVE('',#20998,#22663,#4348,.T.);
#28599=EDGE_CURVE('',#22664,#22663,#1829,.T.);
#28600=EDGE_CURVE('',#20999,#22664,#4349,.T.);
#28601=EDGE_CURVE('',#22665,#22664,#1830,.T.);
#28602=EDGE_CURVE('',#21000,#22665,#4350,.T.);
#28603=EDGE_CURVE('',#22666,#22665,#4351,.T.);
#28604=EDGE_CURVE('',#21001,#22666,#4352,.T.);
#28605=EDGE_CURVE('',#22667,#22666,#1831,.T.);
#28606=EDGE_CURVE('',#21002,#22667,#4353,.T.);
#28607=EDGE_CURVE('',#22668,#22667,#1832,.T.);
#28608=EDGE_CURVE('',#21003,#22668,#4354,.T.);
#28609=EDGE_CURVE('',#22669,#22668,#1833,.T.);
#28610=EDGE_CURVE('',#21004,#22669,#4355,.T.);
#28611=EDGE_CURVE('',#22670,#22669,#1834,.T.);
#28612=EDGE_CURVE('',#21005,#22670,#4356,.T.);
#28613=EDGE_CURVE('',#22671,#22670,#1835,.T.);
#28614=EDGE_CURVE('',#21006,#22671,#4357,.T.);
#28615=EDGE_CURVE('',#22004,#22671,#4358,.T.);
#28616=EDGE_CURVE('',#22672,#21826,#19703,.T.);
#28617=EDGE_CURVE('',#22672,#22673,#1836,.T.);
#28618=EDGE_CURVE('',#22673,#22674,#4359,.T.);
#28619=EDGE_CURVE('',#22674,#22675,#1837,.T.);
#28620=EDGE_CURVE('',#22675,#22676,#1838,.T.);
#28621=EDGE_CURVE('',#22676,#22677,#1839,.T.);
#28622=EDGE_CURVE('',#22677,#22678,#1840,.T.);
#28623=EDGE_CURVE('',#22678,#22679,#1841,.T.);
#28624=EDGE_CURVE('',#22679,#22680,#4360,.T.);
#28625=EDGE_CURVE('',#22680,#22681,#1842,.T.);
#28626=EDGE_CURVE('',#22681,#22682,#1843,.T.);
#28627=EDGE_CURVE('',#22682,#22683,#1844,.T.);
#28628=EDGE_CURVE('',#22683,#22684,#1845,.T.);
#28629=EDGE_CURVE('',#22684,#22685,#1846,.T.);
#28630=EDGE_CURVE('',#22685,#20977,#4361,.T.);
#28631=EDGE_CURVE('',#20945,#22685,#4362,.T.);
#28632=EDGE_CURVE('',#20946,#22684,#4363,.T.);
#28633=EDGE_CURVE('',#20947,#22683,#4364,.T.);
#28634=EDGE_CURVE('',#20948,#22682,#4365,.T.);
#28635=EDGE_CURVE('',#20949,#22681,#4366,.T.);
#28636=EDGE_CURVE('',#20950,#22680,#4367,.T.);
#28637=EDGE_CURVE('',#20951,#22679,#4368,.T.);
#28638=EDGE_CURVE('',#20952,#22678,#4369,.T.);
#28639=EDGE_CURVE('',#20953,#22677,#4370,.T.);
#28640=EDGE_CURVE('',#20954,#22676,#4371,.T.);
#28641=EDGE_CURVE('',#20955,#22675,#4372,.T.);
#28642=EDGE_CURVE('',#20956,#22674,#4373,.T.);
#28643=EDGE_CURVE('',#20957,#22673,#4374,.T.);
#28644=EDGE_CURVE('',#22108,#22672,#19117,.T.);
#28645=EDGE_CURVE('',#22686,#21823,#4375,.T.);
#28646=EDGE_CURVE('',#20961,#22686,#4376,.T.);
#28647=EDGE_CURVE('',#22687,#22686,#1847,.T.);
#28648=EDGE_CURVE('',#20962,#22687,#4377,.T.);
#28649=EDGE_CURVE('',#22688,#22687,#1848,.T.);
#28650=EDGE_CURVE('',#20963,#22688,#4378,.T.);
#28651=EDGE_CURVE('',#22689,#22688,#1849,.T.);
#28652=EDGE_CURVE('',#20964,#22689,#4379,.T.);
#28653=EDGE_CURVE('',#22690,#22689,#1850,.T.);
#28654=EDGE_CURVE('',#20965,#22690,#4380,.T.);
#28655=EDGE_CURVE('',#22691,#22690,#1851,.T.);
#28656=EDGE_CURVE('',#20966,#22691,#4381,.T.);
#28657=EDGE_CURVE('',#22692,#22691,#4382,.T.);
#28658=EDGE_CURVE('',#20967,#22692,#4383,.T.);
#28659=EDGE_CURVE('',#22693,#22692,#1852,.T.);
#28660=EDGE_CURVE('',#20968,#22693,#4384,.T.);
#28661=EDGE_CURVE('',#22694,#22693,#1853,.T.);
#28662=EDGE_CURVE('',#20969,#22694,#4385,.T.);
#28663=EDGE_CURVE('',#22695,#22694,#1854,.T.);
#28664=EDGE_CURVE('',#20970,#22695,#4386,.T.);
#28665=EDGE_CURVE('',#22696,#22695,#1855,.T.);
#28666=EDGE_CURVE('',#20971,#22696,#4387,.T.);
#28667=EDGE_CURVE('',#22697,#22696,#1856,.T.);
#28668=EDGE_CURVE('',#20972,#22697,#4388,.T.);
#28669=EDGE_CURVE('',#22007,#22697,#4389,.T.);
#28670=EDGE_CURVE('',#22698,#21822,#19704,.T.);
#28671=EDGE_CURVE('',#22698,#22699,#1857,.T.);
#28672=EDGE_CURVE('',#22699,#22700,#4390,.T.);
#28673=EDGE_CURVE('',#22700,#22701,#1858,.T.);
#28674=EDGE_CURVE('',#22701,#22702,#1859,.T.);
#28675=EDGE_CURVE('',#22702,#22703,#1860,.T.);
#28676=EDGE_CURVE('',#22703,#22704,#1861,.T.);
#28677=EDGE_CURVE('',#22704,#22705,#1862,.T.);
#28678=EDGE_CURVE('',#22705,#22706,#4391,.T.);
#28679=EDGE_CURVE('',#22706,#22707,#1863,.T.);
#28680=EDGE_CURVE('',#22707,#22708,#1864,.T.);
#28681=EDGE_CURVE('',#22708,#22709,#1865,.T.);
#28682=EDGE_CURVE('',#22709,#22710,#1866,.T.);
#28683=EDGE_CURVE('',#22710,#22711,#1867,.T.);
#28684=EDGE_CURVE('',#22711,#20943,#4392,.T.);
#28685=EDGE_CURVE('',#20911,#22711,#4393,.T.);
#28686=EDGE_CURVE('',#20912,#22710,#4394,.T.);
#28687=EDGE_CURVE('',#20913,#22709,#4395,.T.);
#28688=EDGE_CURVE('',#20914,#22708,#4396,.T.);
#28689=EDGE_CURVE('',#20915,#22707,#4397,.T.);
#28690=EDGE_CURVE('',#20916,#22706,#4398,.T.);
#28691=EDGE_CURVE('',#20917,#22705,#4399,.T.);
#28692=EDGE_CURVE('',#20918,#22704,#4400,.T.);
#28693=EDGE_CURVE('',#20919,#22703,#4401,.T.);
#28694=EDGE_CURVE('',#20920,#22702,#4402,.T.);
#28695=EDGE_CURVE('',#20921,#22701,#4403,.T.);
#28696=EDGE_CURVE('',#20922,#22700,#4404,.T.);
#28697=EDGE_CURVE('',#20923,#22699,#4405,.T.);
#28698=EDGE_CURVE('',#22109,#22698,#19118,.T.);
#28699=EDGE_CURVE('',#22712,#21819,#4406,.T.);
#28700=EDGE_CURVE('',#20927,#22712,#4407,.T.);
#28701=EDGE_CURVE('',#22713,#22712,#1868,.T.);
#28702=EDGE_CURVE('',#20928,#22713,#4408,.T.);
#28703=EDGE_CURVE('',#22714,#22713,#1869,.T.);
#28704=EDGE_CURVE('',#20929,#22714,#4409,.T.);
#28705=EDGE_CURVE('',#22715,#22714,#1870,.T.);
#28706=EDGE_CURVE('',#20930,#22715,#4410,.T.);
#28707=EDGE_CURVE('',#22716,#22715,#1871,.T.);
#28708=EDGE_CURVE('',#20931,#22716,#4411,.T.);
#28709=EDGE_CURVE('',#22717,#22716,#1872,.T.);
#28710=EDGE_CURVE('',#20932,#22717,#4412,.T.);
#28711=EDGE_CURVE('',#22718,#22717,#4413,.T.);
#28712=EDGE_CURVE('',#20933,#22718,#4414,.T.);
#28713=EDGE_CURVE('',#22719,#22718,#1873,.T.);
#28714=EDGE_CURVE('',#20934,#22719,#4415,.T.);
#28715=EDGE_CURVE('',#22720,#22719,#1874,.T.);
#28716=EDGE_CURVE('',#20935,#22720,#4416,.T.);
#28717=EDGE_CURVE('',#22721,#22720,#1875,.T.);
#28718=EDGE_CURVE('',#20936,#22721,#4417,.T.);
#28719=EDGE_CURVE('',#22722,#22721,#1876,.T.);
#28720=EDGE_CURVE('',#20937,#22722,#4418,.T.);
#28721=EDGE_CURVE('',#22723,#22722,#1877,.T.);
#28722=EDGE_CURVE('',#20938,#22723,#4419,.T.);
#28723=EDGE_CURVE('',#22010,#22723,#4420,.T.);
#28724=EDGE_CURVE('',#22724,#21818,#19705,.T.);
#28725=EDGE_CURVE('',#22724,#22725,#1878,.T.);
#28726=EDGE_CURVE('',#22725,#22726,#4421,.T.);
#28727=EDGE_CURVE('',#22726,#22727,#1879,.T.);
#28728=EDGE_CURVE('',#22727,#22728,#1880,.T.);
#28729=EDGE_CURVE('',#22728,#22729,#1881,.T.);
#28730=EDGE_CURVE('',#22729,#22730,#1882,.T.);
#28731=EDGE_CURVE('',#22730,#22731,#1883,.T.);
#28732=EDGE_CURVE('',#22731,#22732,#4422,.T.);
#28733=EDGE_CURVE('',#22732,#22733,#1884,.T.);
#28734=EDGE_CURVE('',#22733,#22734,#1885,.T.);
#28735=EDGE_CURVE('',#22734,#22735,#1886,.T.);
#28736=EDGE_CURVE('',#22735,#22736,#1887,.T.);
#28737=EDGE_CURVE('',#22736,#22737,#1888,.T.);
#28738=EDGE_CURVE('',#22737,#20909,#4423,.T.);
#28739=EDGE_CURVE('',#20877,#22737,#4424,.T.);
#28740=EDGE_CURVE('',#20878,#22736,#4425,.T.);
#28741=EDGE_CURVE('',#20879,#22735,#4426,.T.);
#28742=EDGE_CURVE('',#20880,#22734,#4427,.T.);
#28743=EDGE_CURVE('',#20881,#22733,#4428,.T.);
#28744=EDGE_CURVE('',#20882,#22732,#4429,.T.);
#28745=EDGE_CURVE('',#20883,#22731,#4430,.T.);
#28746=EDGE_CURVE('',#20884,#22730,#4431,.T.);
#28747=EDGE_CURVE('',#20885,#22729,#4432,.T.);
#28748=EDGE_CURVE('',#20886,#22728,#4433,.T.);
#28749=EDGE_CURVE('',#20887,#22727,#4434,.T.);
#28750=EDGE_CURVE('',#20888,#22726,#4435,.T.);
#28751=EDGE_CURVE('',#20889,#22725,#4436,.T.);
#28752=EDGE_CURVE('',#22110,#22724,#19119,.T.);
#28753=EDGE_CURVE('',#22738,#21815,#4437,.T.);
#28754=EDGE_CURVE('',#20893,#22738,#4438,.T.);
#28755=EDGE_CURVE('',#22739,#22738,#1889,.T.);
#28756=EDGE_CURVE('',#20894,#22739,#4439,.T.);
#28757=EDGE_CURVE('',#22740,#22739,#1890,.T.);
#28758=EDGE_CURVE('',#20895,#22740,#4440,.T.);
#28759=EDGE_CURVE('',#22741,#22740,#1891,.T.);
#28760=EDGE_CURVE('',#20896,#22741,#4441,.T.);
#28761=EDGE_CURVE('',#22742,#22741,#1892,.T.);
#28762=EDGE_CURVE('',#20897,#22742,#4442,.T.);
#28763=EDGE_CURVE('',#22743,#22742,#1893,.T.);
#28764=EDGE_CURVE('',#20898,#22743,#4443,.T.);
#28765=EDGE_CURVE('',#22744,#22743,#4444,.T.);
#28766=EDGE_CURVE('',#20899,#22744,#4445,.T.);
#28767=EDGE_CURVE('',#22745,#22744,#1894,.T.);
#28768=EDGE_CURVE('',#20900,#22745,#4446,.T.);
#28769=EDGE_CURVE('',#22746,#22745,#1895,.T.);
#28770=EDGE_CURVE('',#20901,#22746,#4447,.T.);
#28771=EDGE_CURVE('',#22747,#22746,#1896,.T.);
#28772=EDGE_CURVE('',#20902,#22747,#4448,.T.);
#28773=EDGE_CURVE('',#22748,#22747,#1897,.T.);
#28774=EDGE_CURVE('',#20903,#22748,#4449,.T.);
#28775=EDGE_CURVE('',#22749,#22748,#1898,.T.);
#28776=EDGE_CURVE('',#20904,#22749,#4450,.T.);
#28777=EDGE_CURVE('',#22013,#22749,#4451,.T.);
#28778=EDGE_CURVE('',#22750,#21814,#19706,.T.);
#28779=EDGE_CURVE('',#22750,#22751,#1899,.T.);
#28780=EDGE_CURVE('',#22751,#22752,#4452,.T.);
#28781=EDGE_CURVE('',#22752,#22753,#1900,.T.);
#28782=EDGE_CURVE('',#22753,#22754,#1901,.T.);
#28783=EDGE_CURVE('',#22754,#22755,#1902,.T.);
#28784=EDGE_CURVE('',#22755,#22756,#1903,.T.);
#28785=EDGE_CURVE('',#22756,#22757,#1904,.T.);
#28786=EDGE_CURVE('',#22757,#22758,#4453,.T.);
#28787=EDGE_CURVE('',#22758,#22759,#1905,.T.);
#28788=EDGE_CURVE('',#22759,#22760,#1906,.T.);
#28789=EDGE_CURVE('',#22760,#22761,#1907,.T.);
#28790=EDGE_CURVE('',#22761,#22762,#1908,.T.);
#28791=EDGE_CURVE('',#22762,#22763,#1909,.T.);
#28792=EDGE_CURVE('',#22763,#20875,#4454,.T.);
#28793=EDGE_CURVE('',#20843,#22763,#4455,.T.);
#28794=EDGE_CURVE('',#20844,#22762,#4456,.T.);
#28795=EDGE_CURVE('',#20845,#22761,#4457,.T.);
#28796=EDGE_CURVE('',#20846,#22760,#4458,.T.);
#28797=EDGE_CURVE('',#20847,#22759,#4459,.T.);
#28798=EDGE_CURVE('',#20848,#22758,#4460,.T.);
#28799=EDGE_CURVE('',#20849,#22757,#4461,.T.);
#28800=EDGE_CURVE('',#20850,#22756,#4462,.T.);
#28801=EDGE_CURVE('',#20851,#22755,#4463,.T.);
#28802=EDGE_CURVE('',#20852,#22754,#4464,.T.);
#28803=EDGE_CURVE('',#20853,#22753,#4465,.T.);
#28804=EDGE_CURVE('',#20854,#22752,#4466,.T.);
#28805=EDGE_CURVE('',#20855,#22751,#4467,.T.);
#28806=EDGE_CURVE('',#22111,#22750,#19120,.T.);
#28807=EDGE_CURVE('',#22764,#21811,#4468,.T.);
#28808=EDGE_CURVE('',#20859,#22764,#4469,.T.);
#28809=EDGE_CURVE('',#22765,#22764,#1910,.T.);
#28810=EDGE_CURVE('',#20860,#22765,#4470,.T.);
#28811=EDGE_CURVE('',#22766,#22765,#1911,.T.);
#28812=EDGE_CURVE('',#20861,#22766,#4471,.T.);
#28813=EDGE_CURVE('',#22767,#22766,#1912,.T.);
#28814=EDGE_CURVE('',#20862,#22767,#4472,.T.);
#28815=EDGE_CURVE('',#22768,#22767,#1913,.T.);
#28816=EDGE_CURVE('',#20863,#22768,#4473,.T.);
#28817=EDGE_CURVE('',#22769,#22768,#1914,.T.);
#28818=EDGE_CURVE('',#20864,#22769,#4474,.T.);
#28819=EDGE_CURVE('',#22770,#22769,#4475,.T.);
#28820=EDGE_CURVE('',#20865,#22770,#4476,.T.);
#28821=EDGE_CURVE('',#22771,#22770,#1915,.T.);
#28822=EDGE_CURVE('',#20866,#22771,#4477,.T.);
#28823=EDGE_CURVE('',#22772,#22771,#1916,.T.);
#28824=EDGE_CURVE('',#20867,#22772,#4478,.T.);
#28825=EDGE_CURVE('',#22773,#22772,#1917,.T.);
#28826=EDGE_CURVE('',#20868,#22773,#4479,.T.);
#28827=EDGE_CURVE('',#22774,#22773,#1918,.T.);
#28828=EDGE_CURVE('',#20869,#22774,#4480,.T.);
#28829=EDGE_CURVE('',#22775,#22774,#1919,.T.);
#28830=EDGE_CURVE('',#20870,#22775,#4481,.T.);
#28831=EDGE_CURVE('',#22016,#22775,#4482,.T.);
#28832=EDGE_CURVE('',#22776,#21810,#19707,.T.);
#28833=EDGE_CURVE('',#22776,#22777,#1920,.T.);
#28834=EDGE_CURVE('',#22777,#22778,#4483,.T.);
#28835=EDGE_CURVE('',#22778,#22779,#1921,.T.);
#28836=EDGE_CURVE('',#22779,#22780,#1922,.T.);
#28837=EDGE_CURVE('',#22780,#22781,#1923,.T.);
#28838=EDGE_CURVE('',#22781,#22782,#1924,.T.);
#28839=EDGE_CURVE('',#22782,#22783,#1925,.T.);
#28840=EDGE_CURVE('',#22783,#22784,#4484,.T.);
#28841=EDGE_CURVE('',#22784,#22785,#1926,.T.);
#28842=EDGE_CURVE('',#22785,#22786,#1927,.T.);
#28843=EDGE_CURVE('',#22786,#22787,#1928,.T.);
#28844=EDGE_CURVE('',#22787,#22788,#1929,.T.);
#28845=EDGE_CURVE('',#22788,#22789,#1930,.T.);
#28846=EDGE_CURVE('',#22789,#20841,#4485,.T.);
#28847=EDGE_CURVE('',#20809,#22789,#4486,.T.);
#28848=EDGE_CURVE('',#20810,#22788,#4487,.T.);
#28849=EDGE_CURVE('',#20811,#22787,#4488,.T.);
#28850=EDGE_CURVE('',#20812,#22786,#4489,.T.);
#28851=EDGE_CURVE('',#20813,#22785,#4490,.T.);
#28852=EDGE_CURVE('',#20814,#22784,#4491,.T.);
#28853=EDGE_CURVE('',#20815,#22783,#4492,.T.);
#28854=EDGE_CURVE('',#20816,#22782,#4493,.T.);
#28855=EDGE_CURVE('',#20817,#22781,#4494,.T.);
#28856=EDGE_CURVE('',#20818,#22780,#4495,.T.);
#28857=EDGE_CURVE('',#20819,#22779,#4496,.T.);
#28858=EDGE_CURVE('',#20820,#22778,#4497,.T.);
#28859=EDGE_CURVE('',#20821,#22777,#4498,.T.);
#28860=EDGE_CURVE('',#22112,#22776,#19121,.T.);
#28861=EDGE_CURVE('',#22790,#21807,#4499,.T.);
#28862=EDGE_CURVE('',#20825,#22790,#4500,.T.);
#28863=EDGE_CURVE('',#22791,#22790,#1931,.T.);
#28864=EDGE_CURVE('',#20826,#22791,#4501,.T.);
#28865=EDGE_CURVE('',#22792,#22791,#1932,.T.);
#28866=EDGE_CURVE('',#20827,#22792,#4502,.T.);
#28867=EDGE_CURVE('',#22793,#22792,#1933,.T.);
#28868=EDGE_CURVE('',#20828,#22793,#4503,.T.);
#28869=EDGE_CURVE('',#22794,#22793,#1934,.T.);
#28870=EDGE_CURVE('',#20829,#22794,#4504,.T.);
#28871=EDGE_CURVE('',#22795,#22794,#1935,.T.);
#28872=EDGE_CURVE('',#20830,#22795,#4505,.T.);
#28873=EDGE_CURVE('',#22796,#22795,#4506,.T.);
#28874=EDGE_CURVE('',#20831,#22796,#4507,.T.);
#28875=EDGE_CURVE('',#22797,#22796,#1936,.T.);
#28876=EDGE_CURVE('',#20832,#22797,#4508,.T.);
#28877=EDGE_CURVE('',#22798,#22797,#1937,.T.);
#28878=EDGE_CURVE('',#20833,#22798,#4509,.T.);
#28879=EDGE_CURVE('',#22799,#22798,#1938,.T.);
#28880=EDGE_CURVE('',#20834,#22799,#4510,.T.);
#28881=EDGE_CURVE('',#22800,#22799,#1939,.T.);
#28882=EDGE_CURVE('',#20835,#22800,#4511,.T.);
#28883=EDGE_CURVE('',#22801,#22800,#1940,.T.);
#28884=EDGE_CURVE('',#20836,#22801,#4512,.T.);
#28885=EDGE_CURVE('',#22019,#22801,#4513,.T.);
#28886=EDGE_CURVE('',#22802,#21806,#19708,.T.);
#28887=EDGE_CURVE('',#22802,#22803,#1941,.T.);
#28888=EDGE_CURVE('',#22803,#22804,#4514,.T.);
#28889=EDGE_CURVE('',#22804,#22805,#1942,.T.);
#28890=EDGE_CURVE('',#22805,#22806,#1943,.T.);
#28891=EDGE_CURVE('',#22806,#22807,#1944,.T.);
#28892=EDGE_CURVE('',#22807,#22808,#1945,.T.);
#28893=EDGE_CURVE('',#22808,#22809,#1946,.T.);
#28894=EDGE_CURVE('',#22809,#22810,#4515,.T.);
#28895=EDGE_CURVE('',#22810,#22811,#1947,.T.);
#28896=EDGE_CURVE('',#22811,#22812,#1948,.T.);
#28897=EDGE_CURVE('',#22812,#22813,#1949,.T.);
#28898=EDGE_CURVE('',#22813,#22814,#1950,.T.);
#28899=EDGE_CURVE('',#22814,#22815,#1951,.T.);
#28900=EDGE_CURVE('',#22815,#20807,#4516,.T.);
#28901=EDGE_CURVE('',#20775,#22815,#4517,.T.);
#28902=EDGE_CURVE('',#20776,#22814,#4518,.T.);
#28903=EDGE_CURVE('',#20777,#22813,#4519,.T.);
#28904=EDGE_CURVE('',#20778,#22812,#4520,.T.);
#28905=EDGE_CURVE('',#20779,#22811,#4521,.T.);
#28906=EDGE_CURVE('',#20780,#22810,#4522,.T.);
#28907=EDGE_CURVE('',#20781,#22809,#4523,.T.);
#28908=EDGE_CURVE('',#20782,#22808,#4524,.T.);
#28909=EDGE_CURVE('',#20783,#22807,#4525,.T.);
#28910=EDGE_CURVE('',#20784,#22806,#4526,.T.);
#28911=EDGE_CURVE('',#20785,#22805,#4527,.T.);
#28912=EDGE_CURVE('',#20786,#22804,#4528,.T.);
#28913=EDGE_CURVE('',#20787,#22803,#4529,.T.);
#28914=EDGE_CURVE('',#22113,#22802,#19122,.T.);
#28915=EDGE_CURVE('',#22816,#21803,#4530,.T.);
#28916=EDGE_CURVE('',#20791,#22816,#4531,.T.);
#28917=EDGE_CURVE('',#22817,#22816,#1952,.T.);
#28918=EDGE_CURVE('',#20792,#22817,#4532,.T.);
#28919=EDGE_CURVE('',#22818,#22817,#1953,.T.);
#28920=EDGE_CURVE('',#20793,#22818,#4533,.T.);
#28921=EDGE_CURVE('',#22819,#22818,#1954,.T.);
#28922=EDGE_CURVE('',#20794,#22819,#4534,.T.);
#28923=EDGE_CURVE('',#22820,#22819,#1955,.T.);
#28924=EDGE_CURVE('',#20795,#22820,#4535,.T.);
#28925=EDGE_CURVE('',#22821,#22820,#1956,.T.);
#28926=EDGE_CURVE('',#20796,#22821,#4536,.T.);
#28927=EDGE_CURVE('',#22822,#22821,#4537,.T.);
#28928=EDGE_CURVE('',#20797,#22822,#4538,.T.);
#28929=EDGE_CURVE('',#22823,#22822,#1957,.T.);
#28930=EDGE_CURVE('',#20798,#22823,#4539,.T.);
#28931=EDGE_CURVE('',#22824,#22823,#1958,.T.);
#28932=EDGE_CURVE('',#20799,#22824,#4540,.T.);
#28933=EDGE_CURVE('',#22825,#22824,#1959,.T.);
#28934=EDGE_CURVE('',#20800,#22825,#4541,.T.);
#28935=EDGE_CURVE('',#22826,#22825,#1960,.T.);
#28936=EDGE_CURVE('',#20801,#22826,#4542,.T.);
#28937=EDGE_CURVE('',#22827,#22826,#1961,.T.);
#28938=EDGE_CURVE('',#20802,#22827,#4543,.T.);
#28939=EDGE_CURVE('',#22022,#22827,#4544,.T.);
#28940=EDGE_CURVE('',#22828,#21802,#19709,.T.);
#28941=EDGE_CURVE('',#22828,#22829,#1962,.T.);
#28942=EDGE_CURVE('',#22829,#22830,#4545,.T.);
#28943=EDGE_CURVE('',#22830,#22831,#1963,.T.);
#28944=EDGE_CURVE('',#22831,#22832,#1964,.T.);
#28945=EDGE_CURVE('',#22832,#22833,#1965,.T.);
#28946=EDGE_CURVE('',#22833,#22834,#1966,.T.);
#28947=EDGE_CURVE('',#22834,#22835,#1967,.T.);
#28948=EDGE_CURVE('',#22835,#22836,#4546,.T.);
#28949=EDGE_CURVE('',#22836,#22837,#1968,.T.);
#28950=EDGE_CURVE('',#22837,#22838,#1969,.T.);
#28951=EDGE_CURVE('',#22838,#22839,#1970,.T.);
#28952=EDGE_CURVE('',#22839,#22840,#1971,.T.);
#28953=EDGE_CURVE('',#22840,#22841,#1972,.T.);
#28954=EDGE_CURVE('',#22841,#20773,#4547,.T.);
#28955=EDGE_CURVE('',#20741,#22841,#4548,.T.);
#28956=EDGE_CURVE('',#20742,#22840,#4549,.T.);
#28957=EDGE_CURVE('',#20743,#22839,#4550,.T.);
#28958=EDGE_CURVE('',#20744,#22838,#4551,.T.);
#28959=EDGE_CURVE('',#20745,#22837,#4552,.T.);
#28960=EDGE_CURVE('',#20746,#22836,#4553,.T.);
#28961=EDGE_CURVE('',#20747,#22835,#4554,.T.);
#28962=EDGE_CURVE('',#20748,#22834,#4555,.T.);
#28963=EDGE_CURVE('',#20749,#22833,#4556,.T.);
#28964=EDGE_CURVE('',#20750,#22832,#4557,.T.);
#28965=EDGE_CURVE('',#20751,#22831,#4558,.T.);
#28966=EDGE_CURVE('',#20752,#22830,#4559,.T.);
#28967=EDGE_CURVE('',#20753,#22829,#4560,.T.);
#28968=EDGE_CURVE('',#22114,#22828,#19123,.T.);
#28969=EDGE_CURVE('',#22842,#21799,#4561,.T.);
#28970=EDGE_CURVE('',#20757,#22842,#4562,.T.);
#28971=EDGE_CURVE('',#22843,#22842,#1973,.T.);
#28972=EDGE_CURVE('',#20758,#22843,#4563,.T.);
#28973=EDGE_CURVE('',#22844,#22843,#1974,.T.);
#28974=EDGE_CURVE('',#20759,#22844,#4564,.T.);
#28975=EDGE_CURVE('',#22845,#22844,#1975,.T.);
#28976=EDGE_CURVE('',#20760,#22845,#4565,.T.);
#28977=EDGE_CURVE('',#22846,#22845,#1976,.T.);
#28978=EDGE_CURVE('',#20761,#22846,#4566,.T.);
#28979=EDGE_CURVE('',#22847,#22846,#1977,.T.);
#28980=EDGE_CURVE('',#20762,#22847,#4567,.T.);
#28981=EDGE_CURVE('',#22848,#22847,#4568,.T.);
#28982=EDGE_CURVE('',#20763,#22848,#4569,.T.);
#28983=EDGE_CURVE('',#22849,#22848,#1978,.T.);
#28984=EDGE_CURVE('',#20764,#22849,#4570,.T.);
#28985=EDGE_CURVE('',#22850,#22849,#1979,.T.);
#28986=EDGE_CURVE('',#20765,#22850,#4571,.T.);
#28987=EDGE_CURVE('',#22851,#22850,#1980,.T.);
#28988=EDGE_CURVE('',#20766,#22851,#4572,.T.);
#28989=EDGE_CURVE('',#22852,#22851,#1981,.T.);
#28990=EDGE_CURVE('',#20767,#22852,#4573,.T.);
#28991=EDGE_CURVE('',#22853,#22852,#1982,.T.);
#28992=EDGE_CURVE('',#20768,#22853,#4574,.T.);
#28993=EDGE_CURVE('',#22025,#22853,#4575,.T.);
#28994=EDGE_CURVE('',#22854,#21798,#19710,.T.);
#28995=EDGE_CURVE('',#22854,#22855,#1983,.T.);
#28996=EDGE_CURVE('',#22855,#22856,#4576,.T.);
#28997=EDGE_CURVE('',#22856,#22857,#1984,.T.);
#28998=EDGE_CURVE('',#22857,#22858,#1985,.T.);
#28999=EDGE_CURVE('',#22858,#22859,#1986,.T.);
#29000=EDGE_CURVE('',#22859,#22860,#1987,.T.);
#29001=EDGE_CURVE('',#22860,#22861,#1988,.T.);
#29002=EDGE_CURVE('',#22861,#22862,#4577,.T.);
#29003=EDGE_CURVE('',#22862,#22863,#1989,.T.);
#29004=EDGE_CURVE('',#22863,#22864,#1990,.T.);
#29005=EDGE_CURVE('',#22864,#22865,#1991,.T.);
#29006=EDGE_CURVE('',#22865,#22866,#1992,.T.);
#29007=EDGE_CURVE('',#22866,#22867,#1993,.T.);
#29008=EDGE_CURVE('',#22867,#20739,#4578,.T.);
#29009=EDGE_CURVE('',#20707,#22867,#4579,.T.);
#29010=EDGE_CURVE('',#20708,#22866,#4580,.T.);
#29011=EDGE_CURVE('',#20709,#22865,#4581,.T.);
#29012=EDGE_CURVE('',#20710,#22864,#4582,.T.);
#29013=EDGE_CURVE('',#20711,#22863,#4583,.T.);
#29014=EDGE_CURVE('',#20712,#22862,#4584,.T.);
#29015=EDGE_CURVE('',#20713,#22861,#4585,.T.);
#29016=EDGE_CURVE('',#20714,#22860,#4586,.T.);
#29017=EDGE_CURVE('',#20715,#22859,#4587,.T.);
#29018=EDGE_CURVE('',#20716,#22858,#4588,.T.);
#29019=EDGE_CURVE('',#20717,#22857,#4589,.T.);
#29020=EDGE_CURVE('',#20718,#22856,#4590,.T.);
#29021=EDGE_CURVE('',#20719,#22855,#4591,.T.);
#29022=EDGE_CURVE('',#22115,#22854,#19124,.T.);
#29023=EDGE_CURVE('',#22868,#21795,#4592,.T.);
#29024=EDGE_CURVE('',#20723,#22868,#4593,.T.);
#29025=EDGE_CURVE('',#22869,#22868,#1994,.T.);
#29026=EDGE_CURVE('',#20724,#22869,#4594,.T.);
#29027=EDGE_CURVE('',#22870,#22869,#1995,.T.);
#29028=EDGE_CURVE('',#20725,#22870,#4595,.T.);
#29029=EDGE_CURVE('',#22871,#22870,#1996,.T.);
#29030=EDGE_CURVE('',#20726,#22871,#4596,.T.);
#29031=EDGE_CURVE('',#22872,#22871,#1997,.T.);
#29032=EDGE_CURVE('',#20727,#22872,#4597,.T.);
#29033=EDGE_CURVE('',#22873,#22872,#1998,.T.);
#29034=EDGE_CURVE('',#20728,#22873,#4598,.T.);
#29035=EDGE_CURVE('',#22874,#22873,#4599,.T.);
#29036=EDGE_CURVE('',#20729,#22874,#4600,.T.);
#29037=EDGE_CURVE('',#22875,#22874,#1999,.T.);
#29038=EDGE_CURVE('',#20730,#22875,#4601,.T.);
#29039=EDGE_CURVE('',#22876,#22875,#2000,.T.);
#29040=EDGE_CURVE('',#20731,#22876,#4602,.T.);
#29041=EDGE_CURVE('',#22877,#22876,#2001,.T.);
#29042=EDGE_CURVE('',#20732,#22877,#4603,.T.);
#29043=EDGE_CURVE('',#22878,#22877,#2002,.T.);
#29044=EDGE_CURVE('',#20733,#22878,#4604,.T.);
#29045=EDGE_CURVE('',#22879,#22878,#2003,.T.);
#29046=EDGE_CURVE('',#20734,#22879,#4605,.T.);
#29047=EDGE_CURVE('',#22028,#22879,#4606,.T.);
#29048=EDGE_CURVE('',#22880,#21794,#19711,.T.);
#29049=EDGE_CURVE('',#22880,#22881,#2004,.T.);
#29050=EDGE_CURVE('',#22881,#22882,#4607,.T.);
#29051=EDGE_CURVE('',#22882,#22883,#2005,.T.);
#29052=EDGE_CURVE('',#22883,#22884,#2006,.T.);
#29053=EDGE_CURVE('',#22884,#22885,#2007,.T.);
#29054=EDGE_CURVE('',#22885,#22886,#2008,.T.);
#29055=EDGE_CURVE('',#22886,#22887,#2009,.T.);
#29056=EDGE_CURVE('',#22887,#22888,#4608,.T.);
#29057=EDGE_CURVE('',#22888,#22889,#2010,.T.);
#29058=EDGE_CURVE('',#22889,#22890,#2011,.T.);
#29059=EDGE_CURVE('',#22890,#22891,#2012,.T.);
#29060=EDGE_CURVE('',#22891,#22892,#2013,.T.);
#29061=EDGE_CURVE('',#22892,#22893,#2014,.T.);
#29062=EDGE_CURVE('',#22893,#20705,#4609,.T.);
#29063=EDGE_CURVE('',#20673,#22893,#4610,.T.);
#29064=EDGE_CURVE('',#20674,#22892,#4611,.T.);
#29065=EDGE_CURVE('',#20675,#22891,#4612,.T.);
#29066=EDGE_CURVE('',#20676,#22890,#4613,.T.);
#29067=EDGE_CURVE('',#20677,#22889,#4614,.T.);
#29068=EDGE_CURVE('',#20678,#22888,#4615,.T.);
#29069=EDGE_CURVE('',#20679,#22887,#4616,.T.);
#29070=EDGE_CURVE('',#20680,#22886,#4617,.T.);
#29071=EDGE_CURVE('',#20681,#22885,#4618,.T.);
#29072=EDGE_CURVE('',#20682,#22884,#4619,.T.);
#29073=EDGE_CURVE('',#20683,#22883,#4620,.T.);
#29074=EDGE_CURVE('',#20684,#22882,#4621,.T.);
#29075=EDGE_CURVE('',#20685,#22881,#4622,.T.);
#29076=EDGE_CURVE('',#22116,#22880,#19125,.T.);
#29077=EDGE_CURVE('',#22894,#21791,#4623,.T.);
#29078=EDGE_CURVE('',#20689,#22894,#4624,.T.);
#29079=EDGE_CURVE('',#22895,#22894,#2015,.T.);
#29080=EDGE_CURVE('',#20690,#22895,#4625,.T.);
#29081=EDGE_CURVE('',#22896,#22895,#2016,.T.);
#29082=EDGE_CURVE('',#20691,#22896,#4626,.T.);
#29083=EDGE_CURVE('',#22897,#22896,#2017,.T.);
#29084=EDGE_CURVE('',#20692,#22897,#4627,.T.);
#29085=EDGE_CURVE('',#22898,#22897,#2018,.T.);
#29086=EDGE_CURVE('',#20693,#22898,#4628,.T.);
#29087=EDGE_CURVE('',#22899,#22898,#2019,.T.);
#29088=EDGE_CURVE('',#20694,#22899,#4629,.T.);
#29089=EDGE_CURVE('',#22900,#22899,#4630,.T.);
#29090=EDGE_CURVE('',#20695,#22900,#4631,.T.);
#29091=EDGE_CURVE('',#22901,#22900,#2020,.T.);
#29092=EDGE_CURVE('',#20696,#22901,#4632,.T.);
#29093=EDGE_CURVE('',#22902,#22901,#2021,.T.);
#29094=EDGE_CURVE('',#20697,#22902,#4633,.T.);
#29095=EDGE_CURVE('',#22903,#22902,#2022,.T.);
#29096=EDGE_CURVE('',#20698,#22903,#4634,.T.);
#29097=EDGE_CURVE('',#22904,#22903,#2023,.T.);
#29098=EDGE_CURVE('',#20699,#22904,#4635,.T.);
#29099=EDGE_CURVE('',#22905,#22904,#2024,.T.);
#29100=EDGE_CURVE('',#20700,#22905,#4636,.T.);
#29101=EDGE_CURVE('',#22031,#22905,#4637,.T.);
#29102=EDGE_CURVE('',#22906,#21790,#19712,.T.);
#29103=EDGE_CURVE('',#22906,#22907,#2025,.T.);
#29104=EDGE_CURVE('',#22907,#22908,#4638,.T.);
#29105=EDGE_CURVE('',#22908,#22909,#2026,.T.);
#29106=EDGE_CURVE('',#22909,#22910,#2027,.T.);
#29107=EDGE_CURVE('',#22910,#22911,#2028,.T.);
#29108=EDGE_CURVE('',#22911,#22912,#2029,.T.);
#29109=EDGE_CURVE('',#22912,#22913,#2030,.T.);
#29110=EDGE_CURVE('',#22913,#22914,#4639,.T.);
#29111=EDGE_CURVE('',#22914,#22915,#2031,.T.);
#29112=EDGE_CURVE('',#22915,#22916,#2032,.T.);
#29113=EDGE_CURVE('',#22916,#22917,#2033,.T.);
#29114=EDGE_CURVE('',#22917,#22918,#2034,.T.);
#29115=EDGE_CURVE('',#22918,#22919,#2035,.T.);
#29116=EDGE_CURVE('',#22919,#20671,#4640,.T.);
#29117=EDGE_CURVE('',#20639,#22919,#4641,.T.);
#29118=EDGE_CURVE('',#20640,#22918,#4642,.T.);
#29119=EDGE_CURVE('',#20641,#22917,#4643,.T.);
#29120=EDGE_CURVE('',#20642,#22916,#4644,.T.);
#29121=EDGE_CURVE('',#20643,#22915,#4645,.T.);
#29122=EDGE_CURVE('',#20644,#22914,#4646,.T.);
#29123=EDGE_CURVE('',#20645,#22913,#4647,.T.);
#29124=EDGE_CURVE('',#20646,#22912,#4648,.T.);
#29125=EDGE_CURVE('',#20647,#22911,#4649,.T.);
#29126=EDGE_CURVE('',#20648,#22910,#4650,.T.);
#29127=EDGE_CURVE('',#20649,#22909,#4651,.T.);
#29128=EDGE_CURVE('',#20650,#22908,#4652,.T.);
#29129=EDGE_CURVE('',#20651,#22907,#4653,.T.);
#29130=EDGE_CURVE('',#22117,#22906,#19126,.T.);
#29131=EDGE_CURVE('',#22920,#21787,#4654,.T.);
#29132=EDGE_CURVE('',#20655,#22920,#4655,.T.);
#29133=EDGE_CURVE('',#22921,#22920,#2036,.T.);
#29134=EDGE_CURVE('',#20656,#22921,#4656,.T.);
#29135=EDGE_CURVE('',#22922,#22921,#2037,.T.);
#29136=EDGE_CURVE('',#20657,#22922,#4657,.T.);
#29137=EDGE_CURVE('',#22923,#22922,#2038,.T.);
#29138=EDGE_CURVE('',#20658,#22923,#4658,.T.);
#29139=EDGE_CURVE('',#22924,#22923,#2039,.T.);
#29140=EDGE_CURVE('',#20659,#22924,#4659,.T.);
#29141=EDGE_CURVE('',#22925,#22924,#2040,.T.);
#29142=EDGE_CURVE('',#20660,#22925,#4660,.T.);
#29143=EDGE_CURVE('',#22926,#22925,#4661,.T.);
#29144=EDGE_CURVE('',#20661,#22926,#4662,.T.);
#29145=EDGE_CURVE('',#22927,#22926,#2041,.T.);
#29146=EDGE_CURVE('',#20662,#22927,#4663,.T.);
#29147=EDGE_CURVE('',#22928,#22927,#2042,.T.);
#29148=EDGE_CURVE('',#20663,#22928,#4664,.T.);
#29149=EDGE_CURVE('',#22929,#22928,#2043,.T.);
#29150=EDGE_CURVE('',#20664,#22929,#4665,.T.);
#29151=EDGE_CURVE('',#22930,#22929,#2044,.T.);
#29152=EDGE_CURVE('',#20665,#22930,#4666,.T.);
#29153=EDGE_CURVE('',#22931,#22930,#2045,.T.);
#29154=EDGE_CURVE('',#20666,#22931,#4667,.T.);
#29155=EDGE_CURVE('',#22034,#22931,#4668,.T.);
#29156=EDGE_CURVE('',#22932,#21786,#19713,.T.);
#29157=EDGE_CURVE('',#22932,#22933,#2046,.T.);
#29158=EDGE_CURVE('',#22933,#22934,#4669,.T.);
#29159=EDGE_CURVE('',#22934,#22935,#2047,.T.);
#29160=EDGE_CURVE('',#22935,#22936,#2048,.T.);
#29161=EDGE_CURVE('',#22936,#22937,#2049,.T.);
#29162=EDGE_CURVE('',#22937,#22938,#2050,.T.);
#29163=EDGE_CURVE('',#22938,#22939,#2051,.T.);
#29164=EDGE_CURVE('',#22939,#22940,#4670,.T.);
#29165=EDGE_CURVE('',#22940,#22941,#2052,.T.);
#29166=EDGE_CURVE('',#22941,#22942,#2053,.T.);
#29167=EDGE_CURVE('',#22942,#22943,#2054,.T.);
#29168=EDGE_CURVE('',#22943,#22944,#2055,.T.);
#29169=EDGE_CURVE('',#22944,#22945,#2056,.T.);
#29170=EDGE_CURVE('',#22945,#20637,#4671,.T.);
#29171=EDGE_CURVE('',#20605,#22945,#4672,.T.);
#29172=EDGE_CURVE('',#20606,#22944,#4673,.T.);
#29173=EDGE_CURVE('',#20607,#22943,#4674,.T.);
#29174=EDGE_CURVE('',#20608,#22942,#4675,.T.);
#29175=EDGE_CURVE('',#20609,#22941,#4676,.T.);
#29176=EDGE_CURVE('',#20610,#22940,#4677,.T.);
#29177=EDGE_CURVE('',#20611,#22939,#4678,.T.);
#29178=EDGE_CURVE('',#20612,#22938,#4679,.T.);
#29179=EDGE_CURVE('',#20613,#22937,#4680,.T.);
#29180=EDGE_CURVE('',#20614,#22936,#4681,.T.);
#29181=EDGE_CURVE('',#20615,#22935,#4682,.T.);
#29182=EDGE_CURVE('',#20616,#22934,#4683,.T.);
#29183=EDGE_CURVE('',#20617,#22933,#4684,.T.);
#29184=EDGE_CURVE('',#22118,#22932,#19127,.T.);
#29185=EDGE_CURVE('',#22946,#21783,#4685,.T.);
#29186=EDGE_CURVE('',#20621,#22946,#4686,.T.);
#29187=EDGE_CURVE('',#22947,#22946,#2057,.T.);
#29188=EDGE_CURVE('',#20622,#22947,#4687,.T.);
#29189=EDGE_CURVE('',#22948,#22947,#2058,.T.);
#29190=EDGE_CURVE('',#20623,#22948,#4688,.T.);
#29191=EDGE_CURVE('',#22949,#22948,#2059,.T.);
#29192=EDGE_CURVE('',#20624,#22949,#4689,.T.);
#29193=EDGE_CURVE('',#22950,#22949,#2060,.T.);
#29194=EDGE_CURVE('',#20625,#22950,#4690,.T.);
#29195=EDGE_CURVE('',#22951,#22950,#2061,.T.);
#29196=EDGE_CURVE('',#20626,#22951,#4691,.T.);
#29197=EDGE_CURVE('',#22952,#22951,#4692,.T.);
#29198=EDGE_CURVE('',#20627,#22952,#4693,.T.);
#29199=EDGE_CURVE('',#22953,#22952,#2062,.T.);
#29200=EDGE_CURVE('',#20628,#22953,#4694,.T.);
#29201=EDGE_CURVE('',#22954,#22953,#2063,.T.);
#29202=EDGE_CURVE('',#20629,#22954,#4695,.T.);
#29203=EDGE_CURVE('',#22955,#22954,#2064,.T.);
#29204=EDGE_CURVE('',#20630,#22955,#4696,.T.);
#29205=EDGE_CURVE('',#22956,#22955,#2065,.T.);
#29206=EDGE_CURVE('',#20631,#22956,#4697,.T.);
#29207=EDGE_CURVE('',#22957,#22956,#2066,.T.);
#29208=EDGE_CURVE('',#20632,#22957,#4698,.T.);
#29209=EDGE_CURVE('',#22037,#22957,#4699,.T.);
#29210=EDGE_CURVE('',#22958,#21782,#19714,.T.);
#29211=EDGE_CURVE('',#22958,#22959,#2067,.T.);
#29212=EDGE_CURVE('',#22959,#22960,#4700,.T.);
#29213=EDGE_CURVE('',#22960,#22961,#2068,.T.);
#29214=EDGE_CURVE('',#22961,#22962,#2069,.T.);
#29215=EDGE_CURVE('',#22962,#22963,#2070,.T.);
#29216=EDGE_CURVE('',#22963,#22964,#2071,.T.);
#29217=EDGE_CURVE('',#22964,#22965,#2072,.T.);
#29218=EDGE_CURVE('',#22965,#22966,#4701,.T.);
#29219=EDGE_CURVE('',#22966,#22967,#2073,.T.);
#29220=EDGE_CURVE('',#22967,#22968,#2074,.T.);
#29221=EDGE_CURVE('',#22968,#22969,#2075,.T.);
#29222=EDGE_CURVE('',#22969,#22970,#2076,.T.);
#29223=EDGE_CURVE('',#22970,#22971,#2077,.T.);
#29224=EDGE_CURVE('',#22971,#20603,#4702,.T.);
#29225=EDGE_CURVE('',#20571,#22971,#4703,.T.);
#29226=EDGE_CURVE('',#20572,#22970,#4704,.T.);
#29227=EDGE_CURVE('',#20573,#22969,#4705,.T.);
#29228=EDGE_CURVE('',#20574,#22968,#4706,.T.);
#29229=EDGE_CURVE('',#20575,#22967,#4707,.T.);
#29230=EDGE_CURVE('',#20576,#22966,#4708,.T.);
#29231=EDGE_CURVE('',#20577,#22965,#4709,.T.);
#29232=EDGE_CURVE('',#20578,#22964,#4710,.T.);
#29233=EDGE_CURVE('',#20579,#22963,#4711,.T.);
#29234=EDGE_CURVE('',#20580,#22962,#4712,.T.);
#29235=EDGE_CURVE('',#20581,#22961,#4713,.T.);
#29236=EDGE_CURVE('',#20582,#22960,#4714,.T.);
#29237=EDGE_CURVE('',#20583,#22959,#4715,.T.);
#29238=EDGE_CURVE('',#22119,#22958,#19128,.T.);
#29239=EDGE_CURVE('',#22972,#21779,#4716,.T.);
#29240=EDGE_CURVE('',#20587,#22972,#4717,.T.);
#29241=EDGE_CURVE('',#22973,#22972,#2078,.T.);
#29242=EDGE_CURVE('',#20588,#22973,#4718,.T.);
#29243=EDGE_CURVE('',#22974,#22973,#2079,.T.);
#29244=EDGE_CURVE('',#20589,#22974,#4719,.T.);
#29245=EDGE_CURVE('',#22975,#22974,#2080,.T.);
#29246=EDGE_CURVE('',#20590,#22975,#4720,.T.);
#29247=EDGE_CURVE('',#22976,#22975,#2081,.T.);
#29248=EDGE_CURVE('',#20591,#22976,#4721,.T.);
#29249=EDGE_CURVE('',#22977,#22976,#2082,.T.);
#29250=EDGE_CURVE('',#20592,#22977,#4722,.T.);
#29251=EDGE_CURVE('',#22978,#22977,#4723,.T.);
#29252=EDGE_CURVE('',#20593,#22978,#4724,.T.);
#29253=EDGE_CURVE('',#22979,#22978,#2083,.T.);
#29254=EDGE_CURVE('',#20594,#22979,#4725,.T.);
#29255=EDGE_CURVE('',#22980,#22979,#2084,.T.);
#29256=EDGE_CURVE('',#20595,#22980,#4726,.T.);
#29257=EDGE_CURVE('',#22981,#22980,#2085,.T.);
#29258=EDGE_CURVE('',#20596,#22981,#4727,.T.);
#29259=EDGE_CURVE('',#22982,#22981,#2086,.T.);
#29260=EDGE_CURVE('',#20597,#22982,#4728,.T.);
#29261=EDGE_CURVE('',#22983,#22982,#2087,.T.);
#29262=EDGE_CURVE('',#20598,#22983,#4729,.T.);
#29263=EDGE_CURVE('',#22040,#22983,#4730,.T.);
#29264=EDGE_CURVE('',#22984,#21778,#19715,.T.);
#29265=EDGE_CURVE('',#22984,#22985,#2088,.T.);
#29266=EDGE_CURVE('',#22985,#22986,#4731,.T.);
#29267=EDGE_CURVE('',#22986,#22987,#2089,.T.);
#29268=EDGE_CURVE('',#22987,#22988,#2090,.T.);
#29269=EDGE_CURVE('',#22988,#22989,#2091,.T.);
#29270=EDGE_CURVE('',#22989,#22990,#2092,.T.);
#29271=EDGE_CURVE('',#22990,#22991,#2093,.T.);
#29272=EDGE_CURVE('',#22991,#22992,#4732,.T.);
#29273=EDGE_CURVE('',#22992,#22993,#2094,.T.);
#29274=EDGE_CURVE('',#22993,#22994,#2095,.T.);
#29275=EDGE_CURVE('',#22994,#22995,#2096,.T.);
#29276=EDGE_CURVE('',#22995,#22996,#2097,.T.);
#29277=EDGE_CURVE('',#22996,#22997,#2098,.T.);
#29278=EDGE_CURVE('',#22997,#20569,#4733,.T.);
#29279=EDGE_CURVE('',#20537,#22997,#4734,.T.);
#29280=EDGE_CURVE('',#20538,#22996,#4735,.T.);
#29281=EDGE_CURVE('',#20539,#22995,#4736,.T.);
#29282=EDGE_CURVE('',#20540,#22994,#4737,.T.);
#29283=EDGE_CURVE('',#20541,#22993,#4738,.T.);
#29284=EDGE_CURVE('',#20542,#22992,#4739,.T.);
#29285=EDGE_CURVE('',#20543,#22991,#4740,.T.);
#29286=EDGE_CURVE('',#20544,#22990,#4741,.T.);
#29287=EDGE_CURVE('',#20545,#22989,#4742,.T.);
#29288=EDGE_CURVE('',#20546,#22988,#4743,.T.);
#29289=EDGE_CURVE('',#20547,#22987,#4744,.T.);
#29290=EDGE_CURVE('',#20548,#22986,#4745,.T.);
#29291=EDGE_CURVE('',#20549,#22985,#4746,.T.);
#29292=EDGE_CURVE('',#22120,#22984,#19129,.T.);
#29293=EDGE_CURVE('',#22998,#21775,#4747,.T.);
#29294=EDGE_CURVE('',#20553,#22998,#4748,.T.);
#29295=EDGE_CURVE('',#22999,#22998,#2099,.T.);
#29296=EDGE_CURVE('',#20554,#22999,#4749,.T.);
#29297=EDGE_CURVE('',#23000,#22999,#2100,.T.);
#29298=EDGE_CURVE('',#20555,#23000,#4750,.T.);
#29299=EDGE_CURVE('',#23001,#23000,#2101,.T.);
#29300=EDGE_CURVE('',#20556,#23001,#4751,.T.);
#29301=EDGE_CURVE('',#23002,#23001,#2102,.T.);
#29302=EDGE_CURVE('',#20557,#23002,#4752,.T.);
#29303=EDGE_CURVE('',#23003,#23002,#2103,.T.);
#29304=EDGE_CURVE('',#20558,#23003,#4753,.T.);
#29305=EDGE_CURVE('',#23004,#23003,#4754,.T.);
#29306=EDGE_CURVE('',#20559,#23004,#4755,.T.);
#29307=EDGE_CURVE('',#23005,#23004,#2104,.T.);
#29308=EDGE_CURVE('',#20560,#23005,#4756,.T.);
#29309=EDGE_CURVE('',#23006,#23005,#2105,.T.);
#29310=EDGE_CURVE('',#20561,#23006,#4757,.T.);
#29311=EDGE_CURVE('',#23007,#23006,#2106,.T.);
#29312=EDGE_CURVE('',#20562,#23007,#4758,.T.);
#29313=EDGE_CURVE('',#23008,#23007,#2107,.T.);
#29314=EDGE_CURVE('',#20563,#23008,#4759,.T.);
#29315=EDGE_CURVE('',#23009,#23008,#2108,.T.);
#29316=EDGE_CURVE('',#20564,#23009,#4760,.T.);
#29317=EDGE_CURVE('',#22043,#23009,#4761,.T.);
#29318=EDGE_CURVE('',#23010,#21774,#19716,.T.);
#29319=EDGE_CURVE('',#23010,#23011,#2109,.T.);
#29320=EDGE_CURVE('',#23011,#23012,#4762,.T.);
#29321=EDGE_CURVE('',#23012,#23013,#2110,.T.);
#29322=EDGE_CURVE('',#23013,#23014,#2111,.T.);
#29323=EDGE_CURVE('',#23014,#23015,#2112,.T.);
#29324=EDGE_CURVE('',#23015,#23016,#2113,.T.);
#29325=EDGE_CURVE('',#23016,#23017,#2114,.T.);
#29326=EDGE_CURVE('',#23017,#23018,#4763,.T.);
#29327=EDGE_CURVE('',#23018,#23019,#2115,.T.);
#29328=EDGE_CURVE('',#23019,#23020,#2116,.T.);
#29329=EDGE_CURVE('',#23020,#23021,#2117,.T.);
#29330=EDGE_CURVE('',#23021,#23022,#2118,.T.);
#29331=EDGE_CURVE('',#23022,#23023,#2119,.T.);
#29332=EDGE_CURVE('',#23023,#20535,#4764,.T.);
#29333=EDGE_CURVE('',#20503,#23023,#4765,.T.);
#29334=EDGE_CURVE('',#20504,#23022,#4766,.T.);
#29335=EDGE_CURVE('',#20505,#23021,#4767,.T.);
#29336=EDGE_CURVE('',#20506,#23020,#4768,.T.);
#29337=EDGE_CURVE('',#20507,#23019,#4769,.T.);
#29338=EDGE_CURVE('',#20508,#23018,#4770,.T.);
#29339=EDGE_CURVE('',#20509,#23017,#4771,.T.);
#29340=EDGE_CURVE('',#20510,#23016,#4772,.T.);
#29341=EDGE_CURVE('',#20511,#23015,#4773,.T.);
#29342=EDGE_CURVE('',#20512,#23014,#4774,.T.);
#29343=EDGE_CURVE('',#20513,#23013,#4775,.T.);
#29344=EDGE_CURVE('',#20514,#23012,#4776,.T.);
#29345=EDGE_CURVE('',#20515,#23011,#4777,.T.);
#29346=EDGE_CURVE('',#22121,#23010,#19130,.T.);
#29347=EDGE_CURVE('',#23024,#21771,#4778,.T.);
#29348=EDGE_CURVE('',#20519,#23024,#4779,.T.);
#29349=EDGE_CURVE('',#23025,#23024,#2120,.T.);
#29350=EDGE_CURVE('',#20520,#23025,#4780,.T.);
#29351=EDGE_CURVE('',#23026,#23025,#2121,.T.);
#29352=EDGE_CURVE('',#20521,#23026,#4781,.T.);
#29353=EDGE_CURVE('',#23027,#23026,#2122,.T.);
#29354=EDGE_CURVE('',#20522,#23027,#4782,.T.);
#29355=EDGE_CURVE('',#23028,#23027,#2123,.T.);
#29356=EDGE_CURVE('',#20523,#23028,#4783,.T.);
#29357=EDGE_CURVE('',#23029,#23028,#2124,.T.);
#29358=EDGE_CURVE('',#20524,#23029,#4784,.T.);
#29359=EDGE_CURVE('',#23030,#23029,#4785,.T.);
#29360=EDGE_CURVE('',#20525,#23030,#4786,.T.);
#29361=EDGE_CURVE('',#23031,#23030,#2125,.T.);
#29362=EDGE_CURVE('',#20526,#23031,#4787,.T.);
#29363=EDGE_CURVE('',#23032,#23031,#2126,.T.);
#29364=EDGE_CURVE('',#20527,#23032,#4788,.T.);
#29365=EDGE_CURVE('',#23033,#23032,#2127,.T.);
#29366=EDGE_CURVE('',#20528,#23033,#4789,.T.);
#29367=EDGE_CURVE('',#23034,#23033,#2128,.T.);
#29368=EDGE_CURVE('',#20529,#23034,#4790,.T.);
#29369=EDGE_CURVE('',#23035,#23034,#2129,.T.);
#29370=EDGE_CURVE('',#20530,#23035,#4791,.T.);
#29371=EDGE_CURVE('',#22046,#23035,#4792,.T.);
#29372=EDGE_CURVE('',#23036,#21770,#19717,.T.);
#29373=EDGE_CURVE('',#23036,#23037,#2130,.T.);
#29374=EDGE_CURVE('',#23037,#23038,#4793,.T.);
#29375=EDGE_CURVE('',#23038,#23039,#2131,.T.);
#29376=EDGE_CURVE('',#23039,#23040,#2132,.T.);
#29377=EDGE_CURVE('',#23040,#23041,#2133,.T.);
#29378=EDGE_CURVE('',#23041,#23042,#2134,.T.);
#29379=EDGE_CURVE('',#23042,#23043,#2135,.T.);
#29380=EDGE_CURVE('',#23043,#23044,#4794,.T.);
#29381=EDGE_CURVE('',#23044,#23045,#2136,.T.);
#29382=EDGE_CURVE('',#23045,#23046,#2137,.T.);
#29383=EDGE_CURVE('',#23046,#23047,#2138,.T.);
#29384=EDGE_CURVE('',#23047,#23048,#2139,.T.);
#29385=EDGE_CURVE('',#23048,#23049,#2140,.T.);
#29386=EDGE_CURVE('',#23049,#20501,#4795,.T.);
#29387=EDGE_CURVE('',#23050,#21767,#4796,.T.);
#29388=EDGE_CURVE('',#20485,#23050,#4797,.T.);
#29389=EDGE_CURVE('',#23051,#23050,#2141,.T.);
#29390=EDGE_CURVE('',#20486,#23051,#4798,.T.);
#29391=EDGE_CURVE('',#23052,#23051,#2142,.T.);
#29392=EDGE_CURVE('',#20487,#23052,#4799,.T.);
#29393=EDGE_CURVE('',#23053,#23052,#2143,.T.);
#29394=EDGE_CURVE('',#20488,#23053,#4800,.T.);
#29395=EDGE_CURVE('',#23054,#23053,#2144,.T.);
#29396=EDGE_CURVE('',#20489,#23054,#4801,.T.);
#29397=EDGE_CURVE('',#23055,#23054,#2145,.T.);
#29398=EDGE_CURVE('',#20490,#23055,#4802,.T.);
#29399=EDGE_CURVE('',#23056,#23055,#4803,.T.);
#29400=EDGE_CURVE('',#20491,#23056,#4804,.T.);
#29401=EDGE_CURVE('',#23057,#23056,#2146,.T.);
#29402=EDGE_CURVE('',#20492,#23057,#4805,.T.);
#29403=EDGE_CURVE('',#23058,#23057,#2147,.T.);
#29404=EDGE_CURVE('',#20493,#23058,#4806,.T.);
#29405=EDGE_CURVE('',#23059,#23058,#2148,.T.);
#29406=EDGE_CURVE('',#20494,#23059,#4807,.T.);
#29407=EDGE_CURVE('',#23060,#23059,#2149,.T.);
#29408=EDGE_CURVE('',#20495,#23060,#4808,.T.);
#29409=EDGE_CURVE('',#23061,#23060,#2150,.T.);
#29410=EDGE_CURVE('',#20496,#23061,#4809,.T.);
#29411=EDGE_CURVE('',#23062,#23061,#4810,.T.);
#29412=EDGE_CURVE('',#20497,#23062,#4811,.T.);
#29413=EDGE_CURVE('',#22151,#23062,#2151,.T.);
#29414=EDGE_CURVE('',#20469,#23049,#4812,.T.);
#29415=EDGE_CURVE('',#20470,#23048,#4813,.T.);
#29416=EDGE_CURVE('',#20471,#23047,#4814,.T.);
#29417=EDGE_CURVE('',#20472,#23046,#4815,.T.);
#29418=EDGE_CURVE('',#20473,#23045,#4816,.T.);
#29419=EDGE_CURVE('',#20474,#23044,#4817,.T.);
#29420=EDGE_CURVE('',#20475,#23043,#4818,.T.);
#29421=EDGE_CURVE('',#20476,#23042,#4819,.T.);
#29422=EDGE_CURVE('',#20477,#23041,#4820,.T.);
#29423=EDGE_CURVE('',#20478,#23040,#4821,.T.);
#29424=EDGE_CURVE('',#20479,#23039,#4822,.T.);
#29425=EDGE_CURVE('',#20480,#23038,#4823,.T.);
#29426=EDGE_CURVE('',#20481,#23037,#4824,.T.);
#29427=EDGE_CURVE('',#22122,#23036,#19131,.T.);
#29428=EDGE_CURVE('',#22136,#21766,#19718,.T.);
#29429=EDGE_CURVE('',#22104,#23063,#4825,.T.);
#29430=EDGE_CURVE('',#23063,#23063,#19719,.T.);
#29431=EDGE_CURVE('',#23064,#23064,#19720,.T.);
#29432=EDGE_CURVE('',#23064,#23065,#4826,.T.);
#29433=EDGE_CURVE('',#23065,#23066,#19721,.T.);
#29434=EDGE_CURVE('',#23066,#23065,#19722,.T.);
#29435=EDGE_CURVE('',#23066,#23067,#4827,.T.);
#29436=EDGE_CURVE('',#23068,#23067,#19723,.T.);
#29437=EDGE_CURVE('',#23067,#23068,#19724,.T.);
#29438=EDGE_CURVE('',#23068,#23069,#19725,.T.);
#29439=EDGE_CURVE('',#23069,#23070,#19726,.T.);
#29440=EDGE_CURVE('',#23070,#23069,#19727,.T.);
#29441=EDGE_CURVE('',#23070,#23071,#4828,.T.);
#29442=EDGE_CURVE('',#23071,#23071,#19728,.T.);
#29443=EDGE_CURVE('',#23072,#23073,#19729,.T.);
#29444=EDGE_CURVE('',#23073,#23074,#19730,.T.);
#29445=EDGE_CURVE('',#23074,#23074,#19731,.T.);
#29446=EDGE_CURVE('',#23073,#23072,#19732,.T.);
#29447=EDGE_CURVE('',#23072,#23075,#4829,.T.);
#29448=EDGE_CURVE('',#23076,#23075,#19733,.T.);
#29449=EDGE_CURVE('',#23075,#23076,#19734,.T.);
#29450=EDGE_CURVE('',#23077,#23077,#19735,.T.);
#29451=EDGE_CURVE('',#23078,#23078,#19736,.T.);
#29452=EDGE_CURVE('',#23078,#23076,#19737,.T.);
#29453=EDGE_CURVE('',#23079,#23079,#19738,.T.);
#29454=EDGE_CURVE('',#23080,#23080,#19739,.T.);
#29455=EDGE_CURVE('',#23081,#23081,#19740,.T.);
#29456=EDGE_CURVE('',#23081,#23080,#4830,.T.);
#29457=EDGE_CURVE('',#23082,#23082,#19741,.T.);
#29458=EDGE_CURVE('',#23082,#23081,#4831,.T.);
#29459=EDGE_CURVE('',#23079,#23082,#4832,.T.);
#29460=EDGE_CURVE('',#23083,#23083,#19742,.T.);
#29461=EDGE_CURVE('',#23083,#23077,#4833,.T.);
#29462=EDGE_CURVE('',#23071,#23083,#4834,.T.);
#29463=EDGE_CURVE('',#23084,#23085,#19132,.T.);
#29464=EDGE_CURVE('',#23086,#23084,#4835,.T.);
#29465=EDGE_CURVE('',#23087,#23086,#4836,.T.);
#29466=EDGE_CURVE('',#23088,#23087,#4837,.T.);
#29467=EDGE_CURVE('',#23089,#23088,#19133,.T.);
#29468=EDGE_CURVE('',#23085,#23089,#4838,.T.);
#29469=EDGE_CURVE('',#23090,#23091,#19134,.T.);
#29470=EDGE_CURVE('',#23092,#23090,#4839,.T.);
#29471=EDGE_CURVE('',#23093,#23092,#19135,.T.);
#29472=EDGE_CURVE('',#23094,#23093,#4840,.T.);
#29473=EDGE_CURVE('',#23094,#23095,#4841,.T.);
#29474=EDGE_CURVE('',#23091,#23095,#4842,.T.);
#29475=EDGE_CURVE('',#23087,#23094,#4843,.T.);
#29476=EDGE_CURVE('',#23095,#23086,#4844,.T.);
#29477=EDGE_CURVE('',#23089,#23096,#19743,.T.);
#29478=EDGE_CURVE('',#23096,#23097,#4845,.T.);
#29479=EDGE_CURVE('',#23085,#23097,#19744,.T.);
#29480=EDGE_CURVE('',#23098,#23091,#19745,.T.);
#29481=EDGE_CURVE('',#23098,#23099,#19136,.T.);
#29482=EDGE_CURVE('',#23099,#23100,#19746,.T.);
#29483=EDGE_CURVE('',#23100,#23101,#19137,.T.);
#29484=EDGE_CURVE('',#23101,#23102,#19138,.T.);
#29485=EDGE_CURVE('',#23102,#23103,#19139,.T.);
#29486=EDGE_CURVE('',#23103,#23104,#19747,.T.);
#29487=EDGE_CURVE('',#23104,#23105,#19140,.T.);
#29488=EDGE_CURVE('',#23105,#23106,#19141,.T.);
#29489=EDGE_CURVE('',#23106,#23107,#19142,.T.);
#29490=EDGE_CURVE('',#23107,#23108,#19748,.T.);
#29491=EDGE_CURVE('',#23108,#23109,#19143,.T.);
#29492=EDGE_CURVE('',#23109,#23110,#19144,.T.);
#29493=EDGE_CURVE('',#23110,#23111,#19145,.T.);
#29494=EDGE_CURVE('',#23111,#23112,#19749,.T.);
#29495=EDGE_CURVE('',#23112,#23113,#19146,.T.);
#29496=EDGE_CURVE('',#23113,#23114,#19147,.T.);
#29497=EDGE_CURVE('',#23114,#23115,#19148,.T.);
#29498=EDGE_CURVE('',#23115,#23116,#19750,.T.);
#29499=EDGE_CURVE('',#23116,#23117,#19149,.T.);
#29500=EDGE_CURVE('',#23117,#23118,#19150,.T.);
#29501=EDGE_CURVE('',#23118,#23119,#19151,.T.);
#29502=EDGE_CURVE('',#23119,#23120,#19751,.T.);
#29503=EDGE_CURVE('',#23120,#23121,#19152,.T.);
#29504=EDGE_CURVE('',#23121,#23122,#19153,.T.);
#29505=EDGE_CURVE('',#23122,#23123,#19154,.T.);
#29506=EDGE_CURVE('',#23123,#23124,#19752,.T.);
#29507=EDGE_CURVE('',#23124,#23125,#19155,.T.);
#29508=EDGE_CURVE('',#23125,#23126,#19156,.T.);
#29509=EDGE_CURVE('',#23126,#23127,#19157,.T.);
#29510=EDGE_CURVE('',#23127,#23128,#19753,.T.);
#29511=EDGE_CURVE('',#23128,#23129,#19158,.T.);
#29512=EDGE_CURVE('',#23129,#23130,#19159,.T.);
#29513=EDGE_CURVE('',#23130,#23131,#19160,.T.);
#29514=EDGE_CURVE('',#23131,#23132,#19754,.T.);
#29515=EDGE_CURVE('',#23132,#23133,#19161,.T.);
#29516=EDGE_CURVE('',#23133,#23134,#19162,.T.);
#29517=EDGE_CURVE('',#23134,#23135,#19163,.T.);
#29518=EDGE_CURVE('',#23135,#23136,#19755,.T.);
#29519=EDGE_CURVE('',#23136,#23137,#19164,.T.);
#29520=EDGE_CURVE('',#23137,#23138,#19165,.T.);
#29521=EDGE_CURVE('',#23138,#23139,#19166,.T.);
#29522=EDGE_CURVE('',#23139,#23140,#19756,.T.);
#29523=EDGE_CURVE('',#23140,#23141,#19167,.T.);
#29524=EDGE_CURVE('',#23141,#23142,#19168,.T.);
#29525=EDGE_CURVE('',#23142,#23143,#19169,.T.);
#29526=EDGE_CURVE('',#23143,#23090,#19757,.T.);
#29527=EDGE_CURVE('',#23144,#23093,#19758,.T.);
#29528=EDGE_CURVE('',#23144,#23145,#4846,.T.);
#29529=EDGE_CURVE('',#23145,#23146,#4847,.T.);
#29530=EDGE_CURVE('',#23146,#23147,#4848,.T.);
#29531=EDGE_CURVE('',#23148,#23147,#19759,.T.);
#29532=EDGE_CURVE('',#23148,#23149,#4849,.T.);
#29533=EDGE_CURVE('',#23149,#23150,#4850,.T.);
#29534=EDGE_CURVE('',#23150,#23151,#4851,.T.);
#29535=EDGE_CURVE('',#23088,#23151,#19760,.T.);
#29536=EDGE_CURVE('',#23152,#23152,#19761,.T.);
#29537=EDGE_CURVE('',#23153,#23092,#19762,.T.);
#29538=EDGE_CURVE('',#23153,#23154,#19170,.T.);
#29539=EDGE_CURVE('',#23154,#23155,#19171,.T.);
#29540=EDGE_CURVE('',#23155,#23156,#19172,.T.);
#29541=EDGE_CURVE('',#23157,#23156,#19763,.T.);
#29542=EDGE_CURVE('',#23157,#23158,#19173,.T.);
#29543=EDGE_CURVE('',#23158,#23159,#19174,.T.);
#29544=EDGE_CURVE('',#23159,#23160,#19175,.T.);
#29545=EDGE_CURVE('',#23161,#23160,#19764,.T.);
#29546=EDGE_CURVE('',#23161,#23162,#19176,.T.);
#29547=EDGE_CURVE('',#23162,#23163,#19177,.T.);
#29548=EDGE_CURVE('',#23163,#23164,#19178,.T.);
#29549=EDGE_CURVE('',#23165,#23164,#19765,.T.);
#29550=EDGE_CURVE('',#23165,#23166,#19179,.T.);
#29551=EDGE_CURVE('',#23166,#23167,#19180,.T.);
#29552=EDGE_CURVE('',#23167,#23168,#19181,.T.);
#29553=EDGE_CURVE('',#23169,#23168,#19766,.T.);
#29554=EDGE_CURVE('',#23169,#23170,#19182,.T.);
#29555=EDGE_CURVE('',#23170,#23171,#19183,.T.);
#29556=EDGE_CURVE('',#23171,#23172,#19184,.T.);
#29557=EDGE_CURVE('',#23173,#23172,#19767,.T.);
#29558=EDGE_CURVE('',#23173,#23174,#19185,.T.);
#29559=EDGE_CURVE('',#23174,#23175,#19186,.T.);
#29560=EDGE_CURVE('',#23175,#23176,#19187,.T.);
#29561=EDGE_CURVE('',#23177,#23176,#19768,.T.);
#29562=EDGE_CURVE('',#23177,#23178,#19188,.T.);
#29563=EDGE_CURVE('',#23178,#23179,#19189,.T.);
#29564=EDGE_CURVE('',#23179,#23180,#19190,.T.);
#29565=EDGE_CURVE('',#23181,#23180,#19769,.T.);
#29566=EDGE_CURVE('',#23181,#23182,#19191,.T.);
#29567=EDGE_CURVE('',#23182,#23183,#19192,.T.);
#29568=EDGE_CURVE('',#23183,#23184,#19193,.T.);
#29569=EDGE_CURVE('',#23185,#23184,#19770,.T.);
#29570=EDGE_CURVE('',#23185,#23186,#19194,.T.);
#29571=EDGE_CURVE('',#23186,#23187,#19195,.T.);
#29572=EDGE_CURVE('',#23187,#23188,#19196,.T.);
#29573=EDGE_CURVE('',#23189,#23188,#19771,.T.);
#29574=EDGE_CURVE('',#23189,#23190,#19197,.T.);
#29575=EDGE_CURVE('',#23190,#23191,#19198,.T.);
#29576=EDGE_CURVE('',#23191,#23192,#19199,.T.);
#29577=EDGE_CURVE('',#23193,#23192,#19772,.T.);
#29578=EDGE_CURVE('',#23193,#23194,#19200,.T.);
#29579=EDGE_CURVE('',#23194,#23195,#19201,.T.);
#29580=EDGE_CURVE('',#23195,#23196,#19202,.T.);
#29581=EDGE_CURVE('',#23197,#23196,#19773,.T.);
#29582=EDGE_CURVE('',#23197,#23144,#19203,.T.);
#29583=EDGE_CURVE('',#23151,#23198,#19204,.T.);
#29584=EDGE_CURVE('',#23199,#23198,#19774,.T.);
#29585=EDGE_CURVE('',#23199,#23200,#19205,.T.);
#29586=EDGE_CURVE('',#23200,#23201,#19206,.T.);
#29587=EDGE_CURVE('',#23201,#23202,#19207,.T.);
#29588=EDGE_CURVE('',#23203,#23202,#19775,.T.);
#29589=EDGE_CURVE('',#23203,#23204,#19208,.T.);
#29590=EDGE_CURVE('',#23204,#23205,#19209,.T.);
#29591=EDGE_CURVE('',#23205,#23206,#19210,.T.);
#29592=EDGE_CURVE('',#23207,#23206,#19776,.T.);
#29593=EDGE_CURVE('',#23207,#23208,#19211,.T.);
#29594=EDGE_CURVE('',#23208,#23209,#19212,.T.);
#29595=EDGE_CURVE('',#23209,#23210,#19213,.T.);
#29596=EDGE_CURVE('',#23211,#23210,#19777,.T.);
#29597=EDGE_CURVE('',#23211,#23212,#19214,.T.);
#29598=EDGE_CURVE('',#23212,#23213,#19215,.T.);
#29599=EDGE_CURVE('',#23213,#23214,#19216,.T.);
#29600=EDGE_CURVE('',#23215,#23214,#19778,.T.);
#29601=EDGE_CURVE('',#23215,#23216,#19217,.T.);
#29602=EDGE_CURVE('',#23216,#23217,#19218,.T.);
#29603=EDGE_CURVE('',#23217,#23218,#19219,.T.);
#29604=EDGE_CURVE('',#23219,#23218,#19779,.T.);
#29605=EDGE_CURVE('',#23219,#23220,#19220,.T.);
#29606=EDGE_CURVE('',#23220,#23221,#19221,.T.);
#29607=EDGE_CURVE('',#23221,#23222,#19222,.T.);
#29608=EDGE_CURVE('',#23223,#23222,#19780,.T.);
#29609=EDGE_CURVE('',#23223,#23224,#19223,.T.);
#29610=EDGE_CURVE('',#23224,#23225,#19224,.T.);
#29611=EDGE_CURVE('',#23225,#23226,#19225,.T.);
#29612=EDGE_CURVE('',#23227,#23226,#19781,.T.);
#29613=EDGE_CURVE('',#23227,#23228,#19226,.T.);
#29614=EDGE_CURVE('',#23228,#23229,#19227,.T.);
#29615=EDGE_CURVE('',#23229,#23230,#19228,.T.);
#29616=EDGE_CURVE('',#23231,#23230,#19782,.T.);
#29617=EDGE_CURVE('',#23231,#23232,#19229,.T.);
#29618=EDGE_CURVE('',#23232,#23233,#19230,.T.);
#29619=EDGE_CURVE('',#23233,#23234,#19231,.T.);
#29620=EDGE_CURVE('',#23235,#23234,#19783,.T.);
#29621=EDGE_CURVE('',#23235,#23236,#19232,.T.);
#29622=EDGE_CURVE('',#23236,#23237,#19233,.T.);
#29623=EDGE_CURVE('',#23237,#23238,#19234,.T.);
#29624=EDGE_CURVE('',#23239,#23238,#19784,.T.);
#29625=EDGE_CURVE('',#23239,#23240,#19235,.T.);
#29626=EDGE_CURVE('',#23240,#23241,#19236,.T.);
#29627=EDGE_CURVE('',#23241,#23096,#19237,.T.);
#29628=EDGE_CURVE('',#23242,#23098,#4852,.T.);
#29629=EDGE_CURVE('',#23145,#23242,#4853,.T.);
#29630=EDGE_CURVE('',#23099,#23197,#4854,.T.);
#29631=EDGE_CURVE('',#23243,#23244,#19238,.T.);
#29632=EDGE_CURVE('',#23245,#23243,#4855,.T.);
#29633=EDGE_CURVE('',#23147,#23245,#19239,.T.);
#29634=EDGE_CURVE('',#23146,#23246,#4856,.T.);
#29635=EDGE_CURVE('',#23244,#23246,#4857,.T.);
#29636=EDGE_CURVE('',#23246,#23242,#4858,.T.);
#29637=EDGE_CURVE('',#23247,#23244,#19785,.T.);
#29638=EDGE_CURVE('',#23247,#23248,#19240,.T.);
#29639=EDGE_CURVE('',#23248,#23249,#19786,.T.);
#29640=EDGE_CURVE('',#23249,#23250,#19241,.T.);
#29641=EDGE_CURVE('',#23250,#23251,#19242,.T.);
#29642=EDGE_CURVE('',#23251,#23252,#19243,.T.);
#29643=EDGE_CURVE('',#23252,#23253,#19787,.T.);
#29644=EDGE_CURVE('',#23253,#23254,#19244,.T.);
#29645=EDGE_CURVE('',#23254,#23255,#19245,.T.);
#29646=EDGE_CURVE('',#23255,#23256,#19246,.T.);
#29647=EDGE_CURVE('',#23256,#23257,#19788,.T.);
#29648=EDGE_CURVE('',#23257,#23258,#19247,.T.);
#29649=EDGE_CURVE('',#23258,#23259,#19248,.T.);
#29650=EDGE_CURVE('',#23259,#23260,#19249,.T.);
#29651=EDGE_CURVE('',#23260,#23261,#19789,.T.);
#29652=EDGE_CURVE('',#23261,#23262,#19250,.T.);
#29653=EDGE_CURVE('',#23262,#23263,#19251,.T.);
#29654=EDGE_CURVE('',#23263,#23264,#19252,.T.);
#29655=EDGE_CURVE('',#23264,#23265,#19790,.T.);
#29656=EDGE_CURVE('',#23265,#23266,#19253,.T.);
#29657=EDGE_CURVE('',#23266,#23267,#19254,.T.);
#29658=EDGE_CURVE('',#23267,#23268,#19255,.T.);
#29659=EDGE_CURVE('',#23268,#23269,#19791,.T.);
#29660=EDGE_CURVE('',#23269,#23270,#19256,.T.);
#29661=EDGE_CURVE('',#23270,#23271,#19257,.T.);
#29662=EDGE_CURVE('',#23271,#23272,#19258,.T.);
#29663=EDGE_CURVE('',#23272,#23273,#19792,.T.);
#29664=EDGE_CURVE('',#23273,#23274,#19259,.T.);
#29665=EDGE_CURVE('',#23274,#23275,#19260,.T.);
#29666=EDGE_CURVE('',#23275,#23276,#19261,.T.);
#29667=EDGE_CURVE('',#23276,#23277,#19793,.T.);
#29668=EDGE_CURVE('',#23277,#23278,#19262,.T.);
#29669=EDGE_CURVE('',#23278,#23279,#19263,.T.);
#29670=EDGE_CURVE('',#23279,#23280,#19264,.T.);
#29671=EDGE_CURVE('',#23280,#23281,#19794,.T.);
#29672=EDGE_CURVE('',#23281,#23282,#19265,.T.);
#29673=EDGE_CURVE('',#23282,#23283,#19266,.T.);
#29674=EDGE_CURVE('',#23283,#23284,#19267,.T.);
#29675=EDGE_CURVE('',#23284,#23285,#19795,.T.);
#29676=EDGE_CURVE('',#23285,#23286,#19268,.T.);
#29677=EDGE_CURVE('',#23286,#23287,#19269,.T.);
#29678=EDGE_CURVE('',#23287,#23288,#19270,.T.);
#29679=EDGE_CURVE('',#23288,#23289,#19796,.T.);
#29680=EDGE_CURVE('',#23289,#23290,#19271,.T.);
#29681=EDGE_CURVE('',#23290,#23291,#19272,.T.);
#29682=EDGE_CURVE('',#23291,#23292,#19273,.T.);
#29683=EDGE_CURVE('',#23292,#23243,#19797,.T.);
#29684=EDGE_CURVE('',#23097,#23293,#19274,.T.);
#29685=EDGE_CURVE('',#23293,#23294,#19275,.T.);
#29686=EDGE_CURVE('',#23294,#23295,#19276,.T.);
#29687=EDGE_CURVE('',#23295,#23296,#19798,.T.);
#29688=EDGE_CURVE('',#23296,#23297,#19277,.T.);
#29689=EDGE_CURVE('',#23297,#23298,#19278,.T.);
#29690=EDGE_CURVE('',#23298,#23299,#19279,.T.);
#29691=EDGE_CURVE('',#23299,#23300,#19799,.T.);
#29692=EDGE_CURVE('',#23300,#23301,#19280,.T.);
#29693=EDGE_CURVE('',#23301,#23302,#19281,.T.);
#29694=EDGE_CURVE('',#23302,#23303,#19282,.T.);
#29695=EDGE_CURVE('',#23303,#23304,#19800,.T.);
#29696=EDGE_CURVE('',#23304,#23305,#19283,.T.);
#29697=EDGE_CURVE('',#23305,#23306,#19284,.T.);
#29698=EDGE_CURVE('',#23306,#23307,#19285,.T.);
#29699=EDGE_CURVE('',#23307,#23308,#19801,.T.);
#29700=EDGE_CURVE('',#23308,#23309,#19286,.T.);
#29701=EDGE_CURVE('',#23309,#23310,#19287,.T.);
#29702=EDGE_CURVE('',#23310,#23311,#19288,.T.);
#29703=EDGE_CURVE('',#23311,#23312,#19802,.T.);
#29704=EDGE_CURVE('',#23312,#23313,#19289,.T.);
#29705=EDGE_CURVE('',#23313,#23314,#19290,.T.);
#29706=EDGE_CURVE('',#23314,#23315,#19291,.T.);
#29707=EDGE_CURVE('',#23315,#23316,#19803,.T.);
#29708=EDGE_CURVE('',#23316,#23317,#19292,.T.);
#29709=EDGE_CURVE('',#23317,#23318,#19293,.T.);
#29710=EDGE_CURVE('',#23318,#23319,#19294,.T.);
#29711=EDGE_CURVE('',#23319,#23320,#19804,.T.);
#29712=EDGE_CURVE('',#23320,#23321,#19295,.T.);
#29713=EDGE_CURVE('',#23321,#23322,#19296,.T.);
#29714=EDGE_CURVE('',#23322,#23323,#19297,.T.);
#29715=EDGE_CURVE('',#23323,#23324,#19805,.T.);
#29716=EDGE_CURVE('',#23324,#23325,#19298,.T.);
#29717=EDGE_CURVE('',#23325,#23326,#19299,.T.);
#29718=EDGE_CURVE('',#23326,#23327,#19300,.T.);
#29719=EDGE_CURVE('',#23327,#23328,#19806,.T.);
#29720=EDGE_CURVE('',#23328,#23329,#19301,.T.);
#29721=EDGE_CURVE('',#23329,#23330,#19302,.T.);
#29722=EDGE_CURVE('',#23330,#23331,#19303,.T.);
#29723=EDGE_CURVE('',#23331,#23332,#19807,.T.);
#29724=EDGE_CURVE('',#23332,#23333,#19304,.T.);
#29725=EDGE_CURVE('',#23333,#23334,#19305,.T.);
#29726=EDGE_CURVE('',#23334,#23335,#19306,.T.);
#29727=EDGE_CURVE('',#23335,#23336,#19808,.T.);
#29728=EDGE_CURVE('',#23336,#23337,#19307,.T.);
#29729=EDGE_CURVE('',#23084,#23337,#19809,.T.);
#29730=EDGE_CURVE('',#23196,#23100,#4859,.T.);
#29731=EDGE_CURVE('',#23338,#23245,#19810,.T.);
#29732=EDGE_CURVE('',#23338,#23339,#19308,.T.);
#29733=EDGE_CURVE('',#23339,#23340,#19309,.T.);
#29734=EDGE_CURVE('',#23340,#23341,#19310,.T.);
#29735=EDGE_CURVE('',#23342,#23341,#19811,.T.);
#29736=EDGE_CURVE('',#23342,#23343,#19311,.T.);
#29737=EDGE_CURVE('',#23343,#23344,#19312,.T.);
#29738=EDGE_CURVE('',#23344,#23345,#19313,.T.);
#29739=EDGE_CURVE('',#23346,#23345,#19812,.T.);
#29740=EDGE_CURVE('',#23346,#23347,#19314,.T.);
#29741=EDGE_CURVE('',#23347,#23348,#19315,.T.);
#29742=EDGE_CURVE('',#23348,#23349,#19316,.T.);
#29743=EDGE_CURVE('',#23350,#23349,#19813,.T.);
#29744=EDGE_CURVE('',#23350,#23351,#19317,.T.);
#29745=EDGE_CURVE('',#23351,#23352,#19318,.T.);
#29746=EDGE_CURVE('',#23352,#23353,#19319,.T.);
#29747=EDGE_CURVE('',#23354,#23353,#19814,.T.);
#29748=EDGE_CURVE('',#23354,#23355,#19320,.T.);
#29749=EDGE_CURVE('',#23355,#23356,#19321,.T.);
#29750=EDGE_CURVE('',#23356,#23357,#19322,.T.);
#29751=EDGE_CURVE('',#23358,#23357,#19815,.T.);
#29752=EDGE_CURVE('',#23358,#23359,#19323,.T.);
#29753=EDGE_CURVE('',#23359,#23360,#19324,.T.);
#29754=EDGE_CURVE('',#23360,#23361,#19325,.T.);
#29755=EDGE_CURVE('',#23362,#23361,#19816,.T.);
#29756=EDGE_CURVE('',#23362,#23363,#19326,.T.);
#29757=EDGE_CURVE('',#23363,#23364,#19327,.T.);
#29758=EDGE_CURVE('',#23364,#23365,#19328,.T.);
#29759=EDGE_CURVE('',#23366,#23365,#19817,.T.);
#29760=EDGE_CURVE('',#23366,#23367,#19329,.T.);
#29761=EDGE_CURVE('',#23367,#23368,#19330,.T.);
#29762=EDGE_CURVE('',#23368,#23369,#19331,.T.);
#29763=EDGE_CURVE('',#23370,#23369,#19818,.T.);
#29764=EDGE_CURVE('',#23370,#23371,#19332,.T.);
#29765=EDGE_CURVE('',#23371,#23372,#19333,.T.);
#29766=EDGE_CURVE('',#23372,#23373,#19334,.T.);
#29767=EDGE_CURVE('',#23374,#23373,#19819,.T.);
#29768=EDGE_CURVE('',#23374,#23375,#19335,.T.);
#29769=EDGE_CURVE('',#23375,#23376,#19336,.T.);
#29770=EDGE_CURVE('',#23376,#23377,#19337,.T.);
#29771=EDGE_CURVE('',#23378,#23377,#19820,.T.);
#29772=EDGE_CURVE('',#23378,#23379,#19338,.T.);
#29773=EDGE_CURVE('',#23379,#23380,#19339,.T.);
#29774=EDGE_CURVE('',#23380,#23381,#19340,.T.);
#29775=EDGE_CURVE('',#23382,#23381,#19821,.T.);
#29776=EDGE_CURVE('',#23382,#23148,#19341,.T.);
#29777=EDGE_CURVE('',#23383,#23247,#4860,.T.);
#29778=EDGE_CURVE('',#23149,#23383,#4861,.T.);
#29779=EDGE_CURVE('',#23248,#23382,#4862,.T.);
#29780=EDGE_CURVE('',#23198,#23336,#4863,.T.);
#29781=EDGE_CURVE('',#23150,#23384,#4864,.T.);
#29782=EDGE_CURVE('',#23337,#23384,#4865,.T.);
#29783=EDGE_CURVE('',#23384,#23383,#4866,.T.);
#29784=EDGE_CURVE('',#23381,#23249,#4867,.T.);
#29785=EDGE_CURVE('',#23385,#23386,#19342,.T.);
#29786=EDGE_CURVE('',#23387,#23385,#19343,.T.);
#29787=EDGE_CURVE('',#23388,#23387,#19344,.T.);
#29788=EDGE_CURVE('',#23386,#23388,#19822,.T.);
#29789=EDGE_CURVE('',#23389,#23390,#19345,.T.);
#29790=EDGE_CURVE('',#23391,#23389,#19346,.T.);
#29791=EDGE_CURVE('',#23392,#23391,#19347,.T.);
#29792=EDGE_CURVE('',#23390,#23392,#19823,.T.);
#29793=EDGE_CURVE('',#23393,#23394,#19348,.T.);
#29794=EDGE_CURVE('',#23395,#23393,#19349,.T.);
#29795=EDGE_CURVE('',#23396,#23395,#19350,.T.);
#29796=EDGE_CURVE('',#23394,#23396,#19824,.T.);
#29797=EDGE_CURVE('',#23397,#23398,#19351,.T.);
#29798=EDGE_CURVE('',#23399,#23397,#19352,.T.);
#29799=EDGE_CURVE('',#23400,#23399,#19353,.T.);
#29800=EDGE_CURVE('',#23398,#23400,#19825,.T.);
#29801=EDGE_CURVE('',#23401,#23402,#19354,.T.);
#29802=EDGE_CURVE('',#23403,#23401,#19355,.T.);
#29803=EDGE_CURVE('',#23404,#23403,#19356,.T.);
#29804=EDGE_CURVE('',#23402,#23404,#19826,.T.);
#29805=EDGE_CURVE('',#23405,#23406,#19357,.T.);
#29806=EDGE_CURVE('',#23407,#23405,#19358,.T.);
#29807=EDGE_CURVE('',#23408,#23407,#19359,.T.);
#29808=EDGE_CURVE('',#23406,#23408,#19827,.T.);
#29809=EDGE_CURVE('',#23409,#23410,#19360,.T.);
#29810=EDGE_CURVE('',#23411,#23409,#19361,.T.);
#29811=EDGE_CURVE('',#23412,#23411,#19362,.T.);
#29812=EDGE_CURVE('',#23410,#23412,#19828,.T.);
#29813=EDGE_CURVE('',#23413,#23414,#19363,.T.);
#29814=EDGE_CURVE('',#23415,#23413,#19364,.T.);
#29815=EDGE_CURVE('',#23416,#23415,#19365,.T.);
#29816=EDGE_CURVE('',#23414,#23416,#19829,.T.);
#29817=EDGE_CURVE('',#23417,#23418,#19366,.T.);
#29818=EDGE_CURVE('',#23419,#23417,#19367,.T.);
#29819=EDGE_CURVE('',#23420,#23419,#19368,.T.);
#29820=EDGE_CURVE('',#23418,#23420,#19830,.T.);
#29821=EDGE_CURVE('',#23421,#23422,#19369,.T.);
#29822=EDGE_CURVE('',#23423,#23421,#19370,.T.);
#29823=EDGE_CURVE('',#23424,#23423,#19371,.T.);
#29824=EDGE_CURVE('',#23422,#23424,#19831,.T.);
#29825=EDGE_CURVE('',#23425,#23426,#19372,.T.);
#29826=EDGE_CURVE('',#23427,#23425,#19373,.T.);
#29827=EDGE_CURVE('',#23428,#23427,#19374,.T.);
#29828=EDGE_CURVE('',#23426,#23428,#19832,.T.);
#29829=EDGE_CURVE('',#23429,#23430,#19375,.T.);
#29830=EDGE_CURVE('',#23431,#23429,#19376,.T.);
#29831=EDGE_CURVE('',#23432,#23431,#19377,.T.);
#29832=EDGE_CURVE('',#23430,#23432,#19833,.T.);
#29833=EDGE_CURVE('',#23433,#23434,#19378,.T.);
#29834=EDGE_CURVE('',#23435,#23433,#19379,.T.);
#29835=EDGE_CURVE('',#23436,#23435,#19380,.T.);
#29836=EDGE_CURVE('',#23434,#23436,#19834,.T.);
#29837=EDGE_CURVE('',#23437,#23438,#19381,.T.);
#29838=EDGE_CURVE('',#23439,#23437,#19382,.T.);
#29839=EDGE_CURVE('',#23440,#23439,#19383,.T.);
#29840=EDGE_CURVE('',#23438,#23440,#19835,.T.);
#29841=EDGE_CURVE('',#23441,#23442,#19384,.T.);
#29842=EDGE_CURVE('',#23443,#23441,#19385,.T.);
#29843=EDGE_CURVE('',#23444,#23443,#19386,.T.);
#29844=EDGE_CURVE('',#23442,#23444,#19836,.T.);
#29845=EDGE_CURVE('',#23445,#23446,#19387,.T.);
#29846=EDGE_CURVE('',#23447,#23445,#19388,.T.);
#29847=EDGE_CURVE('',#23448,#23447,#19389,.T.);
#29848=EDGE_CURVE('',#23446,#23448,#19837,.T.);
#29849=EDGE_CURVE('',#23449,#23450,#19390,.T.);
#29850=EDGE_CURVE('',#23451,#23449,#19391,.T.);
#29851=EDGE_CURVE('',#23452,#23451,#19392,.T.);
#29852=EDGE_CURVE('',#23450,#23452,#19838,.T.);
#29853=EDGE_CURVE('',#23453,#23454,#19393,.T.);
#29854=EDGE_CURVE('',#23455,#23453,#19394,.T.);
#29855=EDGE_CURVE('',#23456,#23455,#19395,.T.);
#29856=EDGE_CURVE('',#23454,#23456,#19839,.T.);
#29857=EDGE_CURVE('',#23457,#23458,#19396,.T.);
#29858=EDGE_CURVE('',#23459,#23457,#19397,.T.);
#29859=EDGE_CURVE('',#23460,#23459,#19398,.T.);
#29860=EDGE_CURVE('',#23458,#23460,#19840,.T.);
#29861=EDGE_CURVE('',#23461,#23462,#19399,.T.);
#29862=EDGE_CURVE('',#23463,#23461,#19400,.T.);
#29863=EDGE_CURVE('',#23464,#23463,#19401,.T.);
#29864=EDGE_CURVE('',#23462,#23464,#19841,.T.);
#29865=EDGE_CURVE('',#23465,#23466,#19402,.T.);
#29866=EDGE_CURVE('',#23467,#23465,#19403,.T.);
#29867=EDGE_CURVE('',#23468,#23467,#19404,.T.);
#29868=EDGE_CURVE('',#23466,#23468,#19842,.T.);
#29869=EDGE_CURVE('',#23469,#23470,#19405,.T.);
#29870=EDGE_CURVE('',#23471,#23469,#19406,.T.);
#29871=EDGE_CURVE('',#23472,#23471,#19407,.T.);
#29872=EDGE_CURVE('',#23470,#23472,#19843,.T.);
#29873=EDGE_CURVE('',#23473,#23474,#19408,.T.);
#29874=EDGE_CURVE('',#23475,#23473,#19409,.T.);
#29875=EDGE_CURVE('',#23476,#23475,#19410,.T.);
#29876=EDGE_CURVE('',#23474,#23476,#19844,.T.);
#29877=EDGE_CURVE('',#23477,#23478,#19411,.T.);
#29878=EDGE_CURVE('',#23479,#23477,#19412,.T.);
#29879=EDGE_CURVE('',#23480,#23479,#19413,.T.);
#29880=EDGE_CURVE('',#23478,#23480,#19845,.T.);
#29881=EDGE_CURVE('',#23481,#23482,#19414,.T.);
#29882=EDGE_CURVE('',#23483,#23481,#19415,.T.);
#29883=EDGE_CURVE('',#23484,#23483,#19416,.T.);
#29884=EDGE_CURVE('',#23482,#23484,#19846,.T.);
#29885=EDGE_CURVE('',#23485,#23486,#19417,.T.);
#29886=EDGE_CURVE('',#23487,#23485,#19418,.T.);
#29887=EDGE_CURVE('',#23488,#23487,#19419,.T.);
#29888=EDGE_CURVE('',#23486,#23488,#19847,.T.);
#29889=EDGE_CURVE('',#23489,#23490,#19420,.T.);
#29890=EDGE_CURVE('',#23491,#23489,#19421,.T.);
#29891=EDGE_CURVE('',#23492,#23491,#19422,.T.);
#29892=EDGE_CURVE('',#23490,#23492,#19848,.T.);
#29893=EDGE_CURVE('',#23493,#23494,#19423,.T.);
#29894=EDGE_CURVE('',#23495,#23493,#19424,.T.);
#29895=EDGE_CURVE('',#23496,#23495,#19425,.T.);
#29896=EDGE_CURVE('',#23494,#23496,#19849,.T.);
#29897=EDGE_CURVE('',#23497,#23498,#19426,.T.);
#29898=EDGE_CURVE('',#23499,#23497,#19427,.T.);
#29899=EDGE_CURVE('',#23500,#23499,#19428,.T.);
#29900=EDGE_CURVE('',#23498,#23500,#19850,.T.);
#29901=EDGE_CURVE('',#23501,#23502,#19429,.T.);
#29902=EDGE_CURVE('',#23503,#23501,#19430,.T.);
#29903=EDGE_CURVE('',#23504,#23503,#19431,.T.);
#29904=EDGE_CURVE('',#23502,#23504,#19851,.T.);
#29905=EDGE_CURVE('',#23505,#23506,#19432,.T.);
#29906=EDGE_CURVE('',#23507,#23505,#19433,.T.);
#29907=EDGE_CURVE('',#23508,#23507,#19434,.T.);
#29908=EDGE_CURVE('',#23506,#23508,#19852,.T.);
#29909=EDGE_CURVE('',#23509,#23510,#19435,.T.);
#29910=EDGE_CURVE('',#23511,#23509,#19436,.T.);
#29911=EDGE_CURVE('',#23512,#23511,#19437,.T.);
#29912=EDGE_CURVE('',#23510,#23512,#19853,.T.);
#29913=EDGE_CURVE('',#23513,#23514,#19438,.T.);
#29914=EDGE_CURVE('',#23515,#23513,#19439,.T.);
#29915=EDGE_CURVE('',#23516,#23515,#19440,.T.);
#29916=EDGE_CURVE('',#23514,#23516,#19854,.T.);
#29917=EDGE_CURVE('',#23517,#23515,#4868,.T.);
#29918=EDGE_CURVE('',#23517,#23518,#19441,.T.);
#29919=EDGE_CURVE('',#23518,#23519,#4869,.T.);
#29920=EDGE_CURVE('',#23519,#23200,#4870,.T.);
#29921=EDGE_CURVE('',#23335,#23199,#4871,.T.);
#29922=EDGE_CURVE('',#23334,#23520,#4872,.T.);
#29923=EDGE_CURVE('',#23516,#23520,#4873,.T.);
#29924=EDGE_CURVE('',#23521,#23513,#4874,.T.);
#29925=EDGE_CURVE('',#23521,#23517,#19442,.T.);
#29926=EDGE_CURVE('',#23522,#23511,#4875,.T.);
#29927=EDGE_CURVE('',#23522,#23523,#19443,.T.);
#29928=EDGE_CURVE('',#23523,#23524,#4876,.T.);
#29929=EDGE_CURVE('',#23524,#23204,#4877,.T.);
#29930=EDGE_CURVE('',#23331,#23203,#4878,.T.);
#29931=EDGE_CURVE('',#23330,#23525,#4879,.T.);
#29932=EDGE_CURVE('',#23512,#23525,#4880,.T.);
#29933=EDGE_CURVE('',#23526,#23509,#4881,.T.);
#29934=EDGE_CURVE('',#23526,#23522,#19444,.T.);
#29935=EDGE_CURVE('',#23527,#23507,#4882,.T.);
#29936=EDGE_CURVE('',#23527,#23528,#19445,.T.);
#29937=EDGE_CURVE('',#23528,#23529,#4883,.T.);
#29938=EDGE_CURVE('',#23529,#23208,#4884,.T.);
#29939=EDGE_CURVE('',#23327,#23207,#4885,.T.);
#29940=EDGE_CURVE('',#23326,#23530,#4886,.T.);
#29941=EDGE_CURVE('',#23508,#23530,#4887,.T.);
#29942=EDGE_CURVE('',#23531,#23505,#4888,.T.);
#29943=EDGE_CURVE('',#23531,#23527,#19446,.T.);
#29944=EDGE_CURVE('',#23532,#23503,#4889,.T.);
#29945=EDGE_CURVE('',#23532,#23533,#19447,.T.);
#29946=EDGE_CURVE('',#23533,#23534,#4890,.T.);
#29947=EDGE_CURVE('',#23534,#23212,#4891,.T.);
#29948=EDGE_CURVE('',#23323,#23211,#4892,.T.);
#29949=EDGE_CURVE('',#23322,#23535,#4893,.T.);
#29950=EDGE_CURVE('',#23504,#23535,#4894,.T.);
#29951=EDGE_CURVE('',#23536,#23501,#4895,.T.);
#29952=EDGE_CURVE('',#23536,#23532,#19448,.T.);
#29953=EDGE_CURVE('',#23537,#23499,#4896,.T.);
#29954=EDGE_CURVE('',#23537,#23538,#19449,.T.);
#29955=EDGE_CURVE('',#23538,#23539,#4897,.T.);
#29956=EDGE_CURVE('',#23539,#23216,#4898,.T.);
#29957=EDGE_CURVE('',#23319,#23215,#4899,.T.);
#29958=EDGE_CURVE('',#23318,#23540,#4900,.T.);
#29959=EDGE_CURVE('',#23500,#23540,#4901,.T.);
#29960=EDGE_CURVE('',#23541,#23497,#4902,.T.);
#29961=EDGE_CURVE('',#23541,#23537,#19450,.T.);
#29962=EDGE_CURVE('',#23542,#23495,#4903,.T.);
#29963=EDGE_CURVE('',#23542,#23543,#19451,.T.);
#29964=EDGE_CURVE('',#23543,#23544,#4904,.T.);
#29965=EDGE_CURVE('',#23544,#23220,#4905,.T.);
#29966=EDGE_CURVE('',#23315,#23219,#4906,.T.);
#29967=EDGE_CURVE('',#23314,#23545,#4907,.T.);
#29968=EDGE_CURVE('',#23496,#23545,#4908,.T.);
#29969=EDGE_CURVE('',#23546,#23493,#4909,.T.);
#29970=EDGE_CURVE('',#23546,#23542,#19452,.T.);
#29971=EDGE_CURVE('',#23547,#23491,#4910,.T.);
#29972=EDGE_CURVE('',#23547,#23548,#19453,.T.);
#29973=EDGE_CURVE('',#23548,#23549,#4911,.T.);
#29974=EDGE_CURVE('',#23549,#23224,#4912,.T.);
#29975=EDGE_CURVE('',#23311,#23223,#4913,.T.);
#29976=EDGE_CURVE('',#23310,#23550,#4914,.T.);
#29977=EDGE_CURVE('',#23492,#23550,#4915,.T.);
#29978=EDGE_CURVE('',#23551,#23489,#4916,.T.);
#29979=EDGE_CURVE('',#23551,#23547,#19454,.T.);
#29980=EDGE_CURVE('',#23552,#23487,#4917,.T.);
#29981=EDGE_CURVE('',#23552,#23553,#19455,.T.);
#29982=EDGE_CURVE('',#23553,#23554,#4918,.T.);
#29983=EDGE_CURVE('',#23554,#23228,#4919,.T.);
#29984=EDGE_CURVE('',#23307,#23227,#4920,.T.);
#29985=EDGE_CURVE('',#23306,#23555,#4921,.T.);
#29986=EDGE_CURVE('',#23488,#23555,#4922,.T.);
#29987=EDGE_CURVE('',#23556,#23485,#4923,.T.);
#29988=EDGE_CURVE('',#23556,#23552,#19456,.T.);
#29989=EDGE_CURVE('',#23557,#23483,#4924,.T.);
#29990=EDGE_CURVE('',#23557,#23558,#19457,.T.);
#29991=EDGE_CURVE('',#23558,#23559,#4925,.T.);
#29992=EDGE_CURVE('',#23559,#23232,#4926,.T.);
#29993=EDGE_CURVE('',#23303,#23231,#4927,.T.);
#29994=EDGE_CURVE('',#23302,#23560,#4928,.T.);
#29995=EDGE_CURVE('',#23484,#23560,#4929,.T.);
#29996=EDGE_CURVE('',#23561,#23481,#4930,.T.);
#29997=EDGE_CURVE('',#23561,#23557,#19458,.T.);
#29998=EDGE_CURVE('',#23562,#23479,#4931,.T.);
#29999=EDGE_CURVE('',#23562,#23563,#19459,.T.);
#30000=EDGE_CURVE('',#23563,#23564,#4932,.T.);
#30001=EDGE_CURVE('',#23564,#23236,#4933,.T.);
#30002=EDGE_CURVE('',#23299,#23235,#4934,.T.);
#30003=EDGE_CURVE('',#23298,#23565,#4935,.T.);
#30004=EDGE_CURVE('',#23480,#23565,#4936,.T.);
#30005=EDGE_CURVE('',#23566,#23477,#4937,.T.);
#30006=EDGE_CURVE('',#23566,#23562,#19460,.T.);
#30007=EDGE_CURVE('',#23567,#23475,#4938,.T.);
#30008=EDGE_CURVE('',#23567,#23568,#19461,.T.);
#30009=EDGE_CURVE('',#23568,#23569,#4939,.T.);
#30010=EDGE_CURVE('',#23569,#23240,#4940,.T.);
#30011=EDGE_CURVE('',#23295,#23239,#4941,.T.);
#30012=EDGE_CURVE('',#23294,#23570,#4942,.T.);
#30013=EDGE_CURVE('',#23476,#23570,#4943,.T.);
#30014=EDGE_CURVE('',#23571,#23473,#4944,.T.);
#30015=EDGE_CURVE('',#23571,#23567,#19462,.T.);
#30016=EDGE_CURVE('',#23572,#23471,#4945,.T.);
#30017=EDGE_CURVE('',#23572,#23573,#19463,.T.);
#30018=EDGE_CURVE('',#23573,#23574,#4946,.T.);
#30019=EDGE_CURVE('',#23574,#23154,#4947,.T.);
#30020=EDGE_CURVE('',#23143,#23153,#4948,.T.);
#30021=EDGE_CURVE('',#23142,#23575,#4949,.T.);
#30022=EDGE_CURVE('',#23472,#23575,#4950,.T.);
#30023=EDGE_CURVE('',#23576,#23469,#4951,.T.);
#30024=EDGE_CURVE('',#23576,#23572,#19464,.T.);
#30025=EDGE_CURVE('',#23577,#23467,#4952,.T.);
#30026=EDGE_CURVE('',#23577,#23578,#19465,.T.);
#30027=EDGE_CURVE('',#23578,#23579,#4953,.T.);
#30028=EDGE_CURVE('',#23579,#23158,#4954,.T.);
#30029=EDGE_CURVE('',#23139,#23157,#4955,.T.);
#30030=EDGE_CURVE('',#23138,#23580,#4956,.T.);
#30031=EDGE_CURVE('',#23468,#23580,#4957,.T.);
#30032=EDGE_CURVE('',#23581,#23465,#4958,.T.);
#30033=EDGE_CURVE('',#23581,#23577,#19466,.T.);
#30034=EDGE_CURVE('',#23582,#23463,#4959,.T.);
#30035=EDGE_CURVE('',#23582,#23583,#19467,.T.);
#30036=EDGE_CURVE('',#23583,#23584,#4960,.T.);
#30037=EDGE_CURVE('',#23584,#23162,#4961,.T.);
#30038=EDGE_CURVE('',#23135,#23161,#4962,.T.);
#30039=EDGE_CURVE('',#23134,#23585,#4963,.T.);
#30040=EDGE_CURVE('',#23464,#23585,#4964,.T.);
#30041=EDGE_CURVE('',#23586,#23461,#4965,.T.);
#30042=EDGE_CURVE('',#23586,#23582,#19468,.T.);
#30043=EDGE_CURVE('',#23587,#23459,#4966,.T.);
#30044=EDGE_CURVE('',#23587,#23588,#19469,.T.);
#30045=EDGE_CURVE('',#23588,#23589,#4967,.T.);
#30046=EDGE_CURVE('',#23589,#23166,#4968,.T.);
#30047=EDGE_CURVE('',#23131,#23165,#4969,.T.);
#30048=EDGE_CURVE('',#23130,#23590,#4970,.T.);
#30049=EDGE_CURVE('',#23460,#23590,#4971,.T.);
#30050=EDGE_CURVE('',#23591,#23457,#4972,.T.);
#30051=EDGE_CURVE('',#23591,#23587,#19470,.T.);
#30052=EDGE_CURVE('',#23592,#23455,#4973,.T.);
#30053=EDGE_CURVE('',#23592,#23593,#19471,.T.);
#30054=EDGE_CURVE('',#23593,#23594,#4974,.T.);
#30055=EDGE_CURVE('',#23594,#23170,#4975,.T.);
#30056=EDGE_CURVE('',#23127,#23169,#4976,.T.);
#30057=EDGE_CURVE('',#23126,#23595,#4977,.T.);
#30058=EDGE_CURVE('',#23456,#23595,#4978,.T.);
#30059=EDGE_CURVE('',#23596,#23453,#4979,.T.);
#30060=EDGE_CURVE('',#23596,#23592,#19472,.T.);
#30061=EDGE_CURVE('',#23597,#23451,#4980,.T.);
#30062=EDGE_CURVE('',#23597,#23598,#19473,.T.);
#30063=EDGE_CURVE('',#23598,#23599,#4981,.T.);
#30064=EDGE_CURVE('',#23599,#23174,#4982,.T.);
#30065=EDGE_CURVE('',#23123,#23173,#4983,.T.);
#30066=EDGE_CURVE('',#23122,#23600,#4984,.T.);
#30067=EDGE_CURVE('',#23452,#23600,#4985,.T.);
#30068=EDGE_CURVE('',#23601,#23449,#4986,.T.);
#30069=EDGE_CURVE('',#23601,#23597,#19474,.T.);
#30070=EDGE_CURVE('',#23602,#23447,#4987,.T.);
#30071=EDGE_CURVE('',#23602,#23603,#19475,.T.);
#30072=EDGE_CURVE('',#23603,#23604,#4988,.T.);
#30073=EDGE_CURVE('',#23604,#23178,#4989,.T.);
#30074=EDGE_CURVE('',#23119,#23177,#4990,.T.);
#30075=EDGE_CURVE('',#23118,#23605,#4991,.T.);
#30076=EDGE_CURVE('',#23448,#23605,#4992,.T.);
#30077=EDGE_CURVE('',#23606,#23445,#4993,.T.);
#30078=EDGE_CURVE('',#23606,#23602,#19476,.T.);
#30079=EDGE_CURVE('',#23607,#23443,#4994,.T.);
#30080=EDGE_CURVE('',#23607,#23608,#19477,.T.);
#30081=EDGE_CURVE('',#23608,#23609,#4995,.T.);
#30082=EDGE_CURVE('',#23609,#23182,#4996,.T.);
#30083=EDGE_CURVE('',#23115,#23181,#4997,.T.);
#30084=EDGE_CURVE('',#23114,#23610,#4998,.T.);
#30085=EDGE_CURVE('',#23444,#23610,#4999,.T.);
#30086=EDGE_CURVE('',#23611,#23441,#5000,.T.);
#30087=EDGE_CURVE('',#23611,#23607,#19478,.T.);
#30088=EDGE_CURVE('',#23612,#23439,#5001,.T.);
#30089=EDGE_CURVE('',#23612,#23613,#19479,.T.);
#30090=EDGE_CURVE('',#23613,#23614,#5002,.T.);
#30091=EDGE_CURVE('',#23614,#23186,#5003,.T.);
#30092=EDGE_CURVE('',#23111,#23185,#5004,.T.);
#30093=EDGE_CURVE('',#23110,#23615,#5005,.T.);
#30094=EDGE_CURVE('',#23440,#23615,#5006,.T.);
#30095=EDGE_CURVE('',#23616,#23437,#5007,.T.);
#30096=EDGE_CURVE('',#23616,#23612,#19480,.T.);
#30097=EDGE_CURVE('',#23617,#23435,#5008,.T.);
#30098=EDGE_CURVE('',#23617,#23618,#19481,.T.);
#30099=EDGE_CURVE('',#23618,#23619,#5009,.T.);
#30100=EDGE_CURVE('',#23619,#23190,#5010,.T.);
#30101=EDGE_CURVE('',#23107,#23189,#5011,.T.);
#30102=EDGE_CURVE('',#23106,#23620,#5012,.T.);
#30103=EDGE_CURVE('',#23436,#23620,#5013,.T.);
#30104=EDGE_CURVE('',#23621,#23433,#5014,.T.);
#30105=EDGE_CURVE('',#23621,#23617,#19482,.T.);
#30106=EDGE_CURVE('',#23622,#23431,#5015,.T.);
#30107=EDGE_CURVE('',#23622,#23623,#19483,.T.);
#30108=EDGE_CURVE('',#23623,#23624,#5016,.T.);
#30109=EDGE_CURVE('',#23624,#23194,#5017,.T.);
#30110=EDGE_CURVE('',#23103,#23193,#5018,.T.);
#30111=EDGE_CURVE('',#23102,#23625,#5019,.T.);
#30112=EDGE_CURVE('',#23432,#23625,#5020,.T.);
#30113=EDGE_CURVE('',#23626,#23429,#5021,.T.);
#30114=EDGE_CURVE('',#23626,#23622,#19484,.T.);
#30115=EDGE_CURVE('',#23627,#23427,#5022,.T.);
#30116=EDGE_CURVE('',#23627,#23628,#19485,.T.);
#30117=EDGE_CURVE('',#23628,#23629,#5023,.T.);
#30118=EDGE_CURVE('',#23629,#23339,#5024,.T.);
#30119=EDGE_CURVE('',#23292,#23338,#5025,.T.);
#30120=EDGE_CURVE('',#23291,#23630,#5026,.T.);
#30121=EDGE_CURVE('',#23428,#23630,#5027,.T.);
#30122=EDGE_CURVE('',#23631,#23425,#5028,.T.);
#30123=EDGE_CURVE('',#23631,#23627,#19486,.T.);
#30124=EDGE_CURVE('',#23632,#23423,#5029,.T.);
#30125=EDGE_CURVE('',#23632,#23633,#19487,.T.);
#30126=EDGE_CURVE('',#23633,#23634,#5030,.T.);
#30127=EDGE_CURVE('',#23634,#23343,#5031,.T.);
#30128=EDGE_CURVE('',#23288,#23342,#5032,.T.);
#30129=EDGE_CURVE('',#23287,#23635,#5033,.T.);
#30130=EDGE_CURVE('',#23424,#23635,#5034,.T.);
#30131=EDGE_CURVE('',#23636,#23421,#5035,.T.);
#30132=EDGE_CURVE('',#23636,#23632,#19488,.T.);
#30133=EDGE_CURVE('',#23637,#23419,#5036,.T.);
#30134=EDGE_CURVE('',#23637,#23638,#19489,.T.);
#30135=EDGE_CURVE('',#23638,#23639,#5037,.T.);
#30136=EDGE_CURVE('',#23639,#23347,#5038,.T.);
#30137=EDGE_CURVE('',#23284,#23346,#5039,.T.);
#30138=EDGE_CURVE('',#23283,#23640,#5040,.T.);
#30139=EDGE_CURVE('',#23420,#23640,#5041,.T.);
#30140=EDGE_CURVE('',#23641,#23417,#5042,.T.);
#30141=EDGE_CURVE('',#23641,#23637,#19490,.T.);
#30142=EDGE_CURVE('',#23642,#23415,#5043,.T.);
#30143=EDGE_CURVE('',#23642,#23643,#19491,.T.);
#30144=EDGE_CURVE('',#23643,#23644,#5044,.T.);
#30145=EDGE_CURVE('',#23644,#23351,#5045,.T.);
#30146=EDGE_CURVE('',#23280,#23350,#5046,.T.);
#30147=EDGE_CURVE('',#23279,#23645,#5047,.T.);
#30148=EDGE_CURVE('',#23416,#23645,#5048,.T.);
#30149=EDGE_CURVE('',#23646,#23413,#5049,.T.);
#30150=EDGE_CURVE('',#23646,#23642,#19492,.T.);
#30151=EDGE_CURVE('',#23647,#23411,#5050,.T.);
#30152=EDGE_CURVE('',#23647,#23648,#19493,.T.);
#30153=EDGE_CURVE('',#23648,#23649,#5051,.T.);
#30154=EDGE_CURVE('',#23649,#23355,#5052,.T.);
#30155=EDGE_CURVE('',#23276,#23354,#5053,.T.);
#30156=EDGE_CURVE('',#23275,#23650,#5054,.T.);
#30157=EDGE_CURVE('',#23412,#23650,#5055,.T.);
#30158=EDGE_CURVE('',#23651,#23409,#5056,.T.);
#30159=EDGE_CURVE('',#23651,#23647,#19494,.T.);
#30160=EDGE_CURVE('',#23652,#23407,#5057,.T.);
#30161=EDGE_CURVE('',#23652,#23653,#19495,.T.);
#30162=EDGE_CURVE('',#23653,#23654,#5058,.T.);
#30163=EDGE_CURVE('',#23654,#23359,#5059,.T.);
#30164=EDGE_CURVE('',#23272,#23358,#5060,.T.);
#30165=EDGE_CURVE('',#23271,#23655,#5061,.T.);
#30166=EDGE_CURVE('',#23408,#23655,#5062,.T.);
#30167=EDGE_CURVE('',#23656,#23405,#5063,.T.);
#30168=EDGE_CURVE('',#23656,#23652,#19496,.T.);
#30169=EDGE_CURVE('',#23657,#23403,#5064,.T.);
#30170=EDGE_CURVE('',#23657,#23658,#19497,.T.);
#30171=EDGE_CURVE('',#23658,#23659,#5065,.T.);
#30172=EDGE_CURVE('',#23659,#23363,#5066,.T.);
#30173=EDGE_CURVE('',#23268,#23362,#5067,.T.);
#30174=EDGE_CURVE('',#23267,#23660,#5068,.T.);
#30175=EDGE_CURVE('',#23404,#23660,#5069,.T.);
#30176=EDGE_CURVE('',#23661,#23401,#5070,.T.);
#30177=EDGE_CURVE('',#23661,#23657,#19498,.T.);
#30178=EDGE_CURVE('',#23662,#23399,#5071,.T.);
#30179=EDGE_CURVE('',#23662,#23663,#19499,.T.);
#30180=EDGE_CURVE('',#23663,#23664,#5072,.T.);
#30181=EDGE_CURVE('',#23664,#23367,#5073,.T.);
#30182=EDGE_CURVE('',#23264,#23366,#5074,.T.);
#30183=EDGE_CURVE('',#23263,#23665,#5075,.T.);
#30184=EDGE_CURVE('',#23400,#23665,#5076,.T.);
#30185=EDGE_CURVE('',#23666,#23397,#5077,.T.);
#30186=EDGE_CURVE('',#23666,#23662,#19500,.T.);
#30187=EDGE_CURVE('',#23667,#23395,#5078,.T.);
#30188=EDGE_CURVE('',#23667,#23668,#19501,.T.);
#30189=EDGE_CURVE('',#23668,#23669,#5079,.T.);
#30190=EDGE_CURVE('',#23669,#23371,#5080,.T.);
#30191=EDGE_CURVE('',#23260,#23370,#5081,.T.);
#30192=EDGE_CURVE('',#23259,#23670,#5082,.T.);
#30193=EDGE_CURVE('',#23396,#23670,#5083,.T.);
#30194=EDGE_CURVE('',#23671,#23393,#5084,.T.);
#30195=EDGE_CURVE('',#23671,#23667,#19502,.T.);
#30196=EDGE_CURVE('',#23672,#23391,#5085,.T.);
#30197=EDGE_CURVE('',#23672,#23673,#19503,.T.);
#30198=EDGE_CURVE('',#23673,#23674,#5086,.T.);
#30199=EDGE_CURVE('',#23674,#23375,#5087,.T.);
#30200=EDGE_CURVE('',#23256,#23374,#5088,.T.);
#30201=EDGE_CURVE('',#23255,#23675,#5089,.T.);
#30202=EDGE_CURVE('',#23392,#23675,#5090,.T.);
#30203=EDGE_CURVE('',#23676,#23389,#5091,.T.);
#30204=EDGE_CURVE('',#23676,#23672,#19504,.T.);
#30205=EDGE_CURVE('',#23677,#23387,#5092,.T.);
#30206=EDGE_CURVE('',#23677,#23678,#19505,.T.);
#30207=EDGE_CURVE('',#23678,#23679,#5093,.T.);
#30208=EDGE_CURVE('',#23679,#23379,#5094,.T.);
#30209=EDGE_CURVE('',#23252,#23378,#5095,.T.);
#30210=EDGE_CURVE('',#23251,#23680,#5096,.T.);
#30211=EDGE_CURVE('',#23388,#23680,#5097,.T.);
#30212=EDGE_CURVE('',#23681,#23385,#5098,.T.);
#30213=EDGE_CURVE('',#23681,#23677,#19506,.T.);
#30214=EDGE_CURVE('',#23682,#23681,#19507,.T.);
#30215=EDGE_CURVE('',#23678,#23682,#19855,.T.);
#30216=EDGE_CURVE('',#23683,#23676,#19508,.T.);
#30217=EDGE_CURVE('',#23673,#23683,#19856,.T.);
#30218=EDGE_CURVE('',#23684,#23671,#19509,.T.);
#30219=EDGE_CURVE('',#23668,#23684,#19857,.T.);
#30220=EDGE_CURVE('',#23685,#23666,#19510,.T.);
#30221=EDGE_CURVE('',#23663,#23685,#19858,.T.);
#30222=EDGE_CURVE('',#23686,#23661,#19511,.T.);
#30223=EDGE_CURVE('',#23658,#23686,#19859,.T.);
#30224=EDGE_CURVE('',#23687,#23656,#19512,.T.);
#30225=EDGE_CURVE('',#23653,#23687,#19860,.T.);
#30226=EDGE_CURVE('',#23688,#23651,#19513,.T.);
#30227=EDGE_CURVE('',#23648,#23688,#19861,.T.);
#30228=EDGE_CURVE('',#23689,#23646,#19514,.T.);
#30229=EDGE_CURVE('',#23643,#23689,#19862,.T.);
#30230=EDGE_CURVE('',#23690,#23641,#19515,.T.);
#30231=EDGE_CURVE('',#23638,#23690,#19863,.T.);
#30232=EDGE_CURVE('',#23691,#23636,#19516,.T.);
#30233=EDGE_CURVE('',#23633,#23691,#19864,.T.);
#30234=EDGE_CURVE('',#23692,#23631,#19517,.T.);
#30235=EDGE_CURVE('',#23628,#23692,#19865,.T.);
#30236=EDGE_CURVE('',#23693,#23626,#19518,.T.);
#30237=EDGE_CURVE('',#23623,#23693,#19866,.T.);
#30238=EDGE_CURVE('',#23694,#23621,#19519,.T.);
#30239=EDGE_CURVE('',#23618,#23694,#19867,.T.);
#30240=EDGE_CURVE('',#23695,#23616,#19520,.T.);
#30241=EDGE_CURVE('',#23613,#23695,#19868,.T.);
#30242=EDGE_CURVE('',#23696,#23611,#19521,.T.);
#30243=EDGE_CURVE('',#23608,#23696,#19869,.T.);
#30244=EDGE_CURVE('',#23697,#23606,#19522,.T.);
#30245=EDGE_CURVE('',#23603,#23697,#19870,.T.);
#30246=EDGE_CURVE('',#23698,#23601,#19523,.T.);
#30247=EDGE_CURVE('',#23598,#23698,#19871,.T.);
#30248=EDGE_CURVE('',#23699,#23596,#19524,.T.);
#30249=EDGE_CURVE('',#23593,#23699,#19872,.T.);
#30250=EDGE_CURVE('',#23700,#23591,#19525,.T.);
#30251=EDGE_CURVE('',#23588,#23700,#19873,.T.);
#30252=EDGE_CURVE('',#23701,#23586,#19526,.T.);
#30253=EDGE_CURVE('',#23583,#23701,#19874,.T.);
#30254=EDGE_CURVE('',#23702,#23581,#19527,.T.);
#30255=EDGE_CURVE('',#23578,#23702,#19875,.T.);
#30256=EDGE_CURVE('',#23703,#23576,#19528,.T.);
#30257=EDGE_CURVE('',#23573,#23703,#19876,.T.);
#30258=EDGE_CURVE('',#23704,#23571,#19529,.T.);
#30259=EDGE_CURVE('',#23568,#23704,#19877,.T.);
#30260=EDGE_CURVE('',#23705,#23566,#19530,.T.);
#30261=EDGE_CURVE('',#23563,#23705,#19878,.T.);
#30262=EDGE_CURVE('',#23706,#23561,#19531,.T.);
#30263=EDGE_CURVE('',#23558,#23706,#19879,.T.);
#30264=EDGE_CURVE('',#23707,#23556,#19532,.T.);
#30265=EDGE_CURVE('',#23553,#23707,#19880,.T.);
#30266=EDGE_CURVE('',#23708,#23551,#19533,.T.);
#30267=EDGE_CURVE('',#23548,#23708,#19881,.T.);
#30268=EDGE_CURVE('',#23709,#23546,#19534,.T.);
#30269=EDGE_CURVE('',#23543,#23709,#19882,.T.);
#30270=EDGE_CURVE('',#23710,#23541,#19535,.T.);
#30271=EDGE_CURVE('',#23538,#23710,#19883,.T.);
#30272=EDGE_CURVE('',#23711,#23536,#19536,.T.);
#30273=EDGE_CURVE('',#23533,#23711,#19884,.T.);
#30274=EDGE_CURVE('',#23712,#23531,#19537,.T.);
#30275=EDGE_CURVE('',#23528,#23712,#19885,.T.);
#30276=EDGE_CURVE('',#23713,#23526,#19538,.T.);
#30277=EDGE_CURVE('',#23523,#23713,#19886,.T.);
#30278=EDGE_CURVE('',#23714,#23521,#19539,.T.);
#30279=EDGE_CURVE('',#23518,#23714,#19887,.T.);
#30280=EDGE_CURVE('',#23715,#23514,#5099,.T.);
#30281=EDGE_CURVE('',#23333,#23715,#5100,.T.);
#30282=EDGE_CURVE('',#23202,#23332,#5101,.T.);
#30283=EDGE_CURVE('',#23716,#23201,#5102,.T.);
#30284=EDGE_CURVE('',#23716,#23714,#5103,.T.);
#30285=EDGE_CURVE('',#23717,#23510,#5104,.T.);
#30286=EDGE_CURVE('',#23329,#23717,#5105,.T.);
#30287=EDGE_CURVE('',#23206,#23328,#5106,.T.);
#30288=EDGE_CURVE('',#23718,#23205,#5107,.T.);
#30289=EDGE_CURVE('',#23718,#23713,#5108,.T.);
#30290=EDGE_CURVE('',#23719,#23506,#5109,.T.);
#30291=EDGE_CURVE('',#23325,#23719,#5110,.T.);
#30292=EDGE_CURVE('',#23210,#23324,#5111,.T.);
#30293=EDGE_CURVE('',#23720,#23209,#5112,.T.);
#30294=EDGE_CURVE('',#23720,#23712,#5113,.T.);
#30295=EDGE_CURVE('',#23721,#23502,#5114,.T.);
#30296=EDGE_CURVE('',#23321,#23721,#5115,.T.);
#30297=EDGE_CURVE('',#23214,#23320,#5116,.T.);
#30298=EDGE_CURVE('',#23722,#23213,#5117,.T.);
#30299=EDGE_CURVE('',#23722,#23711,#5118,.T.);
#30300=EDGE_CURVE('',#23723,#23498,#5119,.T.);
#30301=EDGE_CURVE('',#23317,#23723,#5120,.T.);
#30302=EDGE_CURVE('',#23218,#23316,#5121,.T.);
#30303=EDGE_CURVE('',#23724,#23217,#5122,.T.);
#30304=EDGE_CURVE('',#23724,#23710,#5123,.T.);
#30305=EDGE_CURVE('',#23725,#23494,#5124,.T.);
#30306=EDGE_CURVE('',#23313,#23725,#5125,.T.);
#30307=EDGE_CURVE('',#23222,#23312,#5126,.T.);
#30308=EDGE_CURVE('',#23726,#23221,#5127,.T.);
#30309=EDGE_CURVE('',#23726,#23709,#5128,.T.);
#30310=EDGE_CURVE('',#23727,#23490,#5129,.T.);
#30311=EDGE_CURVE('',#23309,#23727,#5130,.T.);
#30312=EDGE_CURVE('',#23226,#23308,#5131,.T.);
#30313=EDGE_CURVE('',#23728,#23225,#5132,.T.);
#30314=EDGE_CURVE('',#23728,#23708,#5133,.T.);
#30315=EDGE_CURVE('',#23729,#23486,#5134,.T.);
#30316=EDGE_CURVE('',#23305,#23729,#5135,.T.);
#30317=EDGE_CURVE('',#23230,#23304,#5136,.T.);
#30318=EDGE_CURVE('',#23730,#23229,#5137,.T.);
#30319=EDGE_CURVE('',#23730,#23707,#5138,.T.);
#30320=EDGE_CURVE('',#23731,#23482,#5139,.T.);
#30321=EDGE_CURVE('',#23301,#23731,#5140,.T.);
#30322=EDGE_CURVE('',#23234,#23300,#5141,.T.);
#30323=EDGE_CURVE('',#23732,#23233,#5142,.T.);
#30324=EDGE_CURVE('',#23732,#23706,#5143,.T.);
#30325=EDGE_CURVE('',#23733,#23478,#5144,.T.);
#30326=EDGE_CURVE('',#23297,#23733,#5145,.T.);
#30327=EDGE_CURVE('',#23238,#23296,#5146,.T.);
#30328=EDGE_CURVE('',#23734,#23237,#5147,.T.);
#30329=EDGE_CURVE('',#23734,#23705,#5148,.T.);
#30330=EDGE_CURVE('',#23735,#23474,#5149,.T.);
#30331=EDGE_CURVE('',#23293,#23735,#5150,.T.);
#30332=EDGE_CURVE('',#23736,#23241,#5151,.T.);
#30333=EDGE_CURVE('',#23736,#23704,#5152,.T.);
#30334=EDGE_CURVE('',#23737,#23470,#5153,.T.);
#30335=EDGE_CURVE('',#23141,#23737,#5154,.T.);
#30336=EDGE_CURVE('',#23156,#23140,#5155,.T.);
#30337=EDGE_CURVE('',#23738,#23155,#5156,.T.);
#30338=EDGE_CURVE('',#23738,#23703,#5157,.T.);
#30339=EDGE_CURVE('',#23739,#23466,#5158,.T.);
#30340=EDGE_CURVE('',#23137,#23739,#5159,.T.);
#30341=EDGE_CURVE('',#23160,#23136,#5160,.T.);
#30342=EDGE_CURVE('',#23740,#23159,#5161,.T.);
#30343=EDGE_CURVE('',#23740,#23702,#5162,.T.);
#30344=EDGE_CURVE('',#23741,#23462,#5163,.T.);
#30345=EDGE_CURVE('',#23133,#23741,#5164,.T.);
#30346=EDGE_CURVE('',#23164,#23132,#5165,.T.);
#30347=EDGE_CURVE('',#23742,#23163,#5166,.T.);
#30348=EDGE_CURVE('',#23742,#23701,#5167,.T.);
#30349=EDGE_CURVE('',#23743,#23458,#5168,.T.);
#30350=EDGE_CURVE('',#23129,#23743,#5169,.T.);
#30351=EDGE_CURVE('',#23168,#23128,#5170,.T.);
#30352=EDGE_CURVE('',#23744,#23167,#5171,.T.);
#30353=EDGE_CURVE('',#23744,#23700,#5172,.T.);
#30354=EDGE_CURVE('',#23745,#23454,#5173,.T.);
#30355=EDGE_CURVE('',#23125,#23745,#5174,.T.);
#30356=EDGE_CURVE('',#23172,#23124,#5175,.T.);
#30357=EDGE_CURVE('',#23746,#23171,#5176,.T.);
#30358=EDGE_CURVE('',#23746,#23699,#5177,.T.);
#30359=EDGE_CURVE('',#23747,#23450,#5178,.T.);
#30360=EDGE_CURVE('',#23121,#23747,#5179,.T.);
#30361=EDGE_CURVE('',#23176,#23120,#5180,.T.);
#30362=EDGE_CURVE('',#23748,#23175,#5181,.T.);
#30363=EDGE_CURVE('',#23748,#23698,#5182,.T.);
#30364=EDGE_CURVE('',#23749,#23446,#5183,.T.);
#30365=EDGE_CURVE('',#23117,#23749,#5184,.T.);
#30366=EDGE_CURVE('',#23180,#23116,#5185,.T.);
#30367=EDGE_CURVE('',#23750,#23179,#5186,.T.);
#30368=EDGE_CURVE('',#23750,#23697,#5187,.T.);
#30369=EDGE_CURVE('',#23751,#23442,#5188,.T.);
#30370=EDGE_CURVE('',#23113,#23751,#5189,.T.);
#30371=EDGE_CURVE('',#23184,#23112,#5190,.T.);
#30372=EDGE_CURVE('',#23752,#23183,#5191,.T.);
#30373=EDGE_CURVE('',#23752,#23696,#5192,.T.);
#30374=EDGE_CURVE('',#23753,#23438,#5193,.T.);
#30375=EDGE_CURVE('',#23109,#23753,#5194,.T.);
#30376=EDGE_CURVE('',#23188,#23108,#5195,.T.);
#30377=EDGE_CURVE('',#23754,#23187,#5196,.T.);
#30378=EDGE_CURVE('',#23754,#23695,#5197,.T.);
#30379=EDGE_CURVE('',#23755,#23434,#5198,.T.);
#30380=EDGE_CURVE('',#23105,#23755,#5199,.T.);
#30381=EDGE_CURVE('',#23192,#23104,#5200,.T.);
#30382=EDGE_CURVE('',#23756,#23191,#5201,.T.);
#30383=EDGE_CURVE('',#23756,#23694,#5202,.T.);
#30384=EDGE_CURVE('',#23757,#23430,#5203,.T.);
#30385=EDGE_CURVE('',#23101,#23757,#5204,.T.);
#30386=EDGE_CURVE('',#23758,#23195,#5205,.T.);
#30387=EDGE_CURVE('',#23758,#23693,#5206,.T.);
#30388=EDGE_CURVE('',#23759,#23426,#5207,.T.);
#30389=EDGE_CURVE('',#23290,#23759,#5208,.T.);
#30390=EDGE_CURVE('',#23341,#23289,#5209,.T.);
#30391=EDGE_CURVE('',#23760,#23340,#5210,.T.);
#30392=EDGE_CURVE('',#23760,#23692,#5211,.T.);
#30393=EDGE_CURVE('',#23761,#23422,#5212,.T.);
#30394=EDGE_CURVE('',#23286,#23761,#5213,.T.);
#30395=EDGE_CURVE('',#23345,#23285,#5214,.T.);
#30396=EDGE_CURVE('',#23762,#23344,#5215,.T.);
#30397=EDGE_CURVE('',#23762,#23691,#5216,.T.);
#30398=EDGE_CURVE('',#23763,#23418,#5217,.T.);
#30399=EDGE_CURVE('',#23282,#23763,#5218,.T.);
#30400=EDGE_CURVE('',#23349,#23281,#5219,.T.);
#30401=EDGE_CURVE('',#23764,#23348,#5220,.T.);
#30402=EDGE_CURVE('',#23764,#23690,#5221,.T.);
#30403=EDGE_CURVE('',#23765,#23414,#5222,.T.);
#30404=EDGE_CURVE('',#23278,#23765,#5223,.T.);
#30405=EDGE_CURVE('',#23353,#23277,#5224,.T.);
#30406=EDGE_CURVE('',#23766,#23352,#5225,.T.);
#30407=EDGE_CURVE('',#23766,#23689,#5226,.T.);
#30408=EDGE_CURVE('',#23767,#23410,#5227,.T.);
#30409=EDGE_CURVE('',#23274,#23767,#5228,.T.);
#30410=EDGE_CURVE('',#23357,#23273,#5229,.T.);
#30411=EDGE_CURVE('',#23768,#23356,#5230,.T.);
#30412=EDGE_CURVE('',#23768,#23688,#5231,.T.);
#30413=EDGE_CURVE('',#23769,#23406,#5232,.T.);
#30414=EDGE_CURVE('',#23270,#23769,#5233,.T.);
#30415=EDGE_CURVE('',#23361,#23269,#5234,.T.);
#30416=EDGE_CURVE('',#23770,#23360,#5235,.T.);
#30417=EDGE_CURVE('',#23770,#23687,#5236,.T.);
#30418=EDGE_CURVE('',#23771,#23402,#5237,.T.);
#30419=EDGE_CURVE('',#23266,#23771,#5238,.T.);
#30420=EDGE_CURVE('',#23365,#23265,#5239,.T.);
#30421=EDGE_CURVE('',#23772,#23364,#5240,.T.);
#30422=EDGE_CURVE('',#23772,#23686,#5241,.T.);
#30423=EDGE_CURVE('',#23773,#23398,#5242,.T.);
#30424=EDGE_CURVE('',#23262,#23773,#5243,.T.);
#30425=EDGE_CURVE('',#23369,#23261,#5244,.T.);
#30426=EDGE_CURVE('',#23774,#23368,#5245,.T.);
#30427=EDGE_CURVE('',#23774,#23685,#5246,.T.);
#30428=EDGE_CURVE('',#23775,#23394,#5247,.T.);
#30429=EDGE_CURVE('',#23258,#23775,#5248,.T.);
#30430=EDGE_CURVE('',#23373,#23257,#5249,.T.);
#30431=EDGE_CURVE('',#23776,#23372,#5250,.T.);
#30432=EDGE_CURVE('',#23776,#23684,#5251,.T.);
#30433=EDGE_CURVE('',#23777,#23390,#5252,.T.);
#30434=EDGE_CURVE('',#23254,#23777,#5253,.T.);
#30435=EDGE_CURVE('',#23377,#23253,#5254,.T.);
#30436=EDGE_CURVE('',#23778,#23376,#5255,.T.);
#30437=EDGE_CURVE('',#23778,#23683,#5256,.T.);
#30438=EDGE_CURVE('',#23779,#23386,#5257,.T.);
#30439=EDGE_CURVE('',#23250,#23779,#5258,.T.);
#30440=EDGE_CURVE('',#23780,#23380,#5259,.T.);
#30441=EDGE_CURVE('',#23780,#23682,#5260,.T.);
#30442=EDGE_CURVE('',#23519,#23716,#5261,.T.);
#30443=EDGE_CURVE('',#23520,#23715,#5262,.T.);
#30444=EDGE_CURVE('',#23524,#23718,#5263,.T.);
#30445=EDGE_CURVE('',#23525,#23717,#5264,.T.);
#30446=EDGE_CURVE('',#23529,#23720,#5265,.T.);
#30447=EDGE_CURVE('',#23530,#23719,#5266,.T.);
#30448=EDGE_CURVE('',#23534,#23722,#5267,.T.);
#30449=EDGE_CURVE('',#23535,#23721,#5268,.T.);
#30450=EDGE_CURVE('',#23539,#23724,#5269,.T.);
#30451=EDGE_CURVE('',#23540,#23723,#5270,.T.);
#30452=EDGE_CURVE('',#23544,#23726,#5271,.T.);
#30453=EDGE_CURVE('',#23545,#23725,#5272,.T.);
#30454=EDGE_CURVE('',#23549,#23728,#5273,.T.);
#30455=EDGE_CURVE('',#23550,#23727,#5274,.T.);
#30456=EDGE_CURVE('',#23554,#23730,#5275,.T.);
#30457=EDGE_CURVE('',#23555,#23729,#5276,.T.);
#30458=EDGE_CURVE('',#23559,#23732,#5277,.T.);
#30459=EDGE_CURVE('',#23560,#23731,#5278,.T.);
#30460=EDGE_CURVE('',#23564,#23734,#5279,.T.);
#30461=EDGE_CURVE('',#23565,#23733,#5280,.T.);
#30462=EDGE_CURVE('',#23569,#23736,#5281,.T.);
#30463=EDGE_CURVE('',#23570,#23735,#5282,.T.);
#30464=EDGE_CURVE('',#23574,#23738,#5283,.T.);
#30465=EDGE_CURVE('',#23575,#23737,#5284,.T.);
#30466=EDGE_CURVE('',#23579,#23740,#5285,.T.);
#30467=EDGE_CURVE('',#23580,#23739,#5286,.T.);
#30468=EDGE_CURVE('',#23584,#23742,#5287,.T.);
#30469=EDGE_CURVE('',#23585,#23741,#5288,.T.);
#30470=EDGE_CURVE('',#23589,#23744,#5289,.T.);
#30471=EDGE_CURVE('',#23590,#23743,#5290,.T.);
#30472=EDGE_CURVE('',#23594,#23746,#5291,.T.);
#30473=EDGE_CURVE('',#23595,#23745,#5292,.T.);
#30474=EDGE_CURVE('',#23599,#23748,#5293,.T.);
#30475=EDGE_CURVE('',#23600,#23747,#5294,.T.);
#30476=EDGE_CURVE('',#23604,#23750,#5295,.T.);
#30477=EDGE_CURVE('',#23605,#23749,#5296,.T.);
#30478=EDGE_CURVE('',#23609,#23752,#5297,.T.);
#30479=EDGE_CURVE('',#23610,#23751,#5298,.T.);
#30480=EDGE_CURVE('',#23614,#23754,#5299,.T.);
#30481=EDGE_CURVE('',#23615,#23753,#5300,.T.);
#30482=EDGE_CURVE('',#23619,#23756,#5301,.T.);
#30483=EDGE_CURVE('',#23620,#23755,#5302,.T.);
#30484=EDGE_CURVE('',#23624,#23758,#5303,.T.);
#30485=EDGE_CURVE('',#23625,#23757,#5304,.T.);
#30486=EDGE_CURVE('',#23629,#23760,#5305,.T.);
#30487=EDGE_CURVE('',#23630,#23759,#5306,.T.);
#30488=EDGE_CURVE('',#23634,#23762,#5307,.T.);
#30489=EDGE_CURVE('',#23635,#23761,#5308,.T.);
#30490=EDGE_CURVE('',#23639,#23764,#5309,.T.);
#30491=EDGE_CURVE('',#23640,#23763,#5310,.T.);
#30492=EDGE_CURVE('',#23644,#23766,#5311,.T.);
#30493=EDGE_CURVE('',#23645,#23765,#5312,.T.);
#30494=EDGE_CURVE('',#23649,#23768,#5313,.T.);
#30495=EDGE_CURVE('',#23650,#23767,#5314,.T.);
#30496=EDGE_CURVE('',#23654,#23770,#5315,.T.);
#30497=EDGE_CURVE('',#23655,#23769,#5316,.T.);
#30498=EDGE_CURVE('',#23659,#23772,#5317,.T.);
#30499=EDGE_CURVE('',#23660,#23771,#5318,.T.);
#30500=EDGE_CURVE('',#23664,#23774,#5319,.T.);
#30501=EDGE_CURVE('',#23665,#23773,#5320,.T.);
#30502=EDGE_CURVE('',#23669,#23776,#5321,.T.);
#30503=EDGE_CURVE('',#23670,#23775,#5322,.T.);
#30504=EDGE_CURVE('',#23674,#23778,#5323,.T.);
#30505=EDGE_CURVE('',#23675,#23777,#5324,.T.);
#30506=EDGE_CURVE('',#23679,#23780,#5325,.T.);
#30507=EDGE_CURVE('',#23680,#23779,#5326,.T.);
#30508=EDGE_CURVE('',#23781,#23782,#19888,.T.);
#30509=EDGE_CURVE('',#23782,#23783,#19889,.T.);
#30510=EDGE_CURVE('',#23783,#23783,#19890,.T.);
#30511=EDGE_CURVE('',#23782,#23781,#19891,.T.);
#30512=EDGE_CURVE('',#23784,#23784,#19892,.T.);
#30513=EDGE_CURVE('',#23785,#23785,#19893,.T.);
#30514=EDGE_CURVE('',#23785,#23781,#5327,.T.);
#30515=EDGE_CURVE('',#23786,#23786,#19894,.T.);
#30516=EDGE_CURVE('',#23786,#23787,#19895,.T.);
#30517=EDGE_CURVE('',#23787,#23788,#19896,.T.);
#30518=EDGE_CURVE('',#23788,#23787,#19897,.T.);
#30519=EDGE_CURVE('',#23789,#23789,#19898,.T.);
#30520=EDGE_CURVE('',#23788,#23152,#5328,.T.);
#30521=EDGE_CURVE('',#23784,#23790,#19899,.T.);
#30522=EDGE_CURVE('',#23790,#23791,#19900,.T.);
#30523=EDGE_CURVE('',#23791,#23790,#19901,.T.);
#30524=EDGE_CURVE('',#23792,#23792,#19902,.T.);
#30525=EDGE_CURVE('',#23792,#23791,#5329,.T.);
#30526=EDGE_CURVE('',#23793,#23794,#19903,.T.);
#30527=EDGE_CURVE('',#23794,#23789,#19904,.T.);
#30528=EDGE_CURVE('',#23794,#23793,#19905,.T.);
#30529=EDGE_CURVE('',#23793,#23795,#5330,.T.);
#30530=EDGE_CURVE('',#23795,#23795,#19906,.T.);
#30531=EDGE_CURVE('',#23796,#23796,#19907,.T.);
#30532=EDGE_CURVE('',#23796,#23797,#5331,.T.);
#30533=EDGE_CURVE('',#23797,#23797,#19908,.T.);
#30534=EDGE_CURVE('',#23797,#23798,#5332,.T.);
#30535=EDGE_CURVE('',#23798,#23798,#19909,.T.);
#30536=EDGE_CURVE('',#23799,#23799,#19910,.T.);
#30537=EDGE_CURVE('',#23799,#23796,#5333,.T.);
#30538=EDGE_CURVE('',#23800,#23800,#19911,.T.);
#30539=EDGE_CURVE('',#23800,#23801,#5334,.T.);
#30540=EDGE_CURVE('',#23801,#23801,#19912,.T.);
#30541=EDGE_CURVE('',#23802,#23802,#19913,.T.);
#30542=EDGE_CURVE('',#23803,#23803,#19914,.T.);
#30543=EDGE_CURVE('',#23804,#23804,#19915,.T.);
#30544=EDGE_CURVE('',#23805,#23805,#19916,.T.);
#30545=EDGE_CURVE('',#23806,#23806,#19917,.T.);
#30546=EDGE_CURVE('',#23807,#23807,#19918,.T.);
#30547=EDGE_CURVE('',#23808,#23808,#19919,.T.);
#30548=EDGE_CURVE('',#23809,#23809,#19920,.T.);
#30549=EDGE_CURVE('',#23809,#23801,#5335,.T.);
#30550=EDGE_CURVE('',#23803,#23810,#5336,.T.);
#30551=EDGE_CURVE('',#23810,#23810,#19921,.T.);
#30552=EDGE_CURVE('',#23811,#23811,#19922,.T.);
#30553=EDGE_CURVE('',#23811,#23810,#5337,.T.);
#30554=EDGE_CURVE('',#23812,#23812,#19923,.T.);
#30555=EDGE_CURVE('',#23812,#23813,#5338,.T.);
#30556=EDGE_CURVE('',#23813,#23813,#19924,.T.);
#30557=EDGE_CURVE('',#23814,#23814,#19925,.T.);
#30558=EDGE_CURVE('',#23814,#23815,#5339,.T.);
#30559=EDGE_CURVE('',#23815,#23815,#19926,.T.);
#30560=EDGE_CURVE('',#23816,#23816,#19927,.T.);
#30561=EDGE_CURVE('',#23816,#23817,#5340,.T.);
#30562=EDGE_CURVE('',#23817,#23817,#19928,.T.);
#30563=EDGE_CURVE('',#23818,#23818,#19929,.T.);
#30564=EDGE_CURVE('',#23818,#23819,#5341,.T.);
#30565=EDGE_CURVE('',#23819,#23819,#19930,.T.);
#30566=EDGE_CURVE('',#23820,#23820,#19931,.T.);
#30567=EDGE_CURVE('',#23820,#23804,#5342,.T.);
#30568=EDGE_CURVE('',#23821,#23821,#19932,.T.);
#30569=EDGE_CURVE('',#23821,#23805,#5343,.T.);
#30570=EDGE_CURVE('',#23822,#23822,#19933,.T.);
#30571=EDGE_CURVE('',#23822,#23806,#5344,.T.);
#30572=EDGE_CURVE('',#23823,#23823,#19934,.T.);
#30573=EDGE_CURVE('',#23823,#23807,#5345,.T.);
#30574=EDGE_CURVE('',#23824,#23825,#5346,.T.);
#30575=EDGE_CURVE('',#23825,#23825,#19935,.T.);
#30576=EDGE_CURVE('',#23825,#23826,#5347,.T.);
#30577=EDGE_CURVE('',#23826,#23826,#19936,.T.);
#30578=EDGE_CURVE('',#23826,#23827,#5348,.T.);
#30579=EDGE_CURVE('',#23827,#23827,#19937,.T.);
#30580=EDGE_CURVE('',#23808,#23828,#19938,.T.);
#30581=EDGE_CURVE('',#23828,#23829,#19939,.T.);
#30582=EDGE_CURVE('',#23829,#23828,#19940,.T.);
#30583=EDGE_CURVE('',#23830,#23830,#19941,.T.);
#30584=EDGE_CURVE('',#23830,#23829,#5349,.T.);
#30585=EDGE_CURVE('',#23831,#23831,#19942,.T.);
#30586=EDGE_CURVE('',#23832,#23832,#19943,.T.);
#30587=EDGE_CURVE('',#23832,#23831,#5350,.T.);
#30588=EDGE_CURVE('',#23833,#23833,#19944,.T.);
#30589=EDGE_CURVE('',#23833,#23832,#5351,.T.);
#30590=EDGE_CURVE('',#23834,#23834,#19945,.T.);
#30591=EDGE_CURVE('',#23835,#23835,#19946,.T.);
#30592=EDGE_CURVE('',#23835,#23834,#5352,.T.);
#30593=EDGE_CURVE('',#23836,#23836,#19947,.T.);
#30594=EDGE_CURVE('',#23836,#23835,#5353,.T.);
#30595=EDGE_CURVE('',#23802,#23836,#5354,.T.);
#30596=EDGE_CURVE('',#23837,#23837,#19948,.T.);
#30597=EDGE_CURVE('',#23838,#23838,#19949,.T.);
#30598=EDGE_CURVE('',#23838,#23837,#5355,.T.);
#30599=EDGE_CURVE('',#23839,#23839,#19950,.T.);
#30600=EDGE_CURVE('',#23839,#23838,#5356,.T.);
#30601=EDGE_CURVE('',#23840,#23841,#5357,.T.);
#30602=EDGE_CURVE('',#23840,#23842,#5358,.T.);
#30603=EDGE_CURVE('',#23842,#23843,#5359,.T.);
#30604=EDGE_CURVE('',#23841,#23843,#5360,.T.);
#30605=EDGE_CURVE('',#23844,#23840,#5361,.T.);
#30606=EDGE_CURVE('',#23844,#23845,#5362,.T.);
#30607=EDGE_CURVE('',#23845,#23842,#5363,.T.);
#30608=EDGE_CURVE('',#23846,#23844,#5364,.T.);
#30609=EDGE_CURVE('',#23846,#23847,#5365,.T.);
#30610=EDGE_CURVE('',#23847,#23845,#5366,.T.);
#30611=EDGE_CURVE('',#23848,#23846,#5367,.T.);
#30612=EDGE_CURVE('',#23848,#23849,#5368,.T.);
#30613=EDGE_CURVE('',#23849,#23847,#5369,.T.);
#30614=EDGE_CURVE('',#23850,#23848,#5370,.T.);
#30615=EDGE_CURVE('',#23850,#23851,#5371,.T.);
#30616=EDGE_CURVE('',#23851,#23849,#5372,.T.);
#30617=EDGE_CURVE('',#23852,#23850,#5373,.T.);
#30618=EDGE_CURVE('',#23852,#23853,#5374,.T.);
#30619=EDGE_CURVE('',#23853,#23851,#5375,.T.);
#30620=EDGE_CURVE('',#23854,#23852,#5376,.T.);
#30621=EDGE_CURVE('',#23854,#23855,#5377,.T.);
#30622=EDGE_CURVE('',#23855,#23853,#5378,.T.);
#30623=EDGE_CURVE('',#23856,#23854,#5379,.T.);
#30624=EDGE_CURVE('',#23856,#23857,#5380,.T.);
#30625=EDGE_CURVE('',#23857,#23855,#5381,.T.);
#30626=EDGE_CURVE('',#23858,#23856,#5382,.T.);
#30627=EDGE_CURVE('',#23858,#23859,#5383,.T.);
#30628=EDGE_CURVE('',#23859,#23857,#5384,.T.);
#30629=EDGE_CURVE('',#23860,#23858,#5385,.T.);
#30630=EDGE_CURVE('',#23860,#23861,#5386,.T.);
#30631=EDGE_CURVE('',#23861,#23859,#5387,.T.);
#30632=EDGE_CURVE('',#23862,#23860,#5388,.T.);
#30633=EDGE_CURVE('',#23862,#23863,#5389,.T.);
#30634=EDGE_CURVE('',#23863,#23861,#5390,.T.);
#30635=EDGE_CURVE('',#23841,#23862,#5391,.T.);
#30636=EDGE_CURVE('',#23843,#23863,#5392,.T.);
#30637=EDGE_CURVE('',#23864,#23865,#5393,.T.);
#30638=EDGE_CURVE('',#23864,#23866,#5394,.T.);
#30639=EDGE_CURVE('',#23866,#23867,#5395,.T.);
#30640=EDGE_CURVE('',#23865,#23867,#5396,.T.);
#30641=EDGE_CURVE('',#23868,#23864,#5397,.T.);
#30642=EDGE_CURVE('',#23868,#23869,#5398,.T.);
#30643=EDGE_CURVE('',#23869,#23866,#5399,.T.);
#30644=EDGE_CURVE('',#23870,#23868,#5400,.T.);
#30645=EDGE_CURVE('',#23870,#23871,#5401,.T.);
#30646=EDGE_CURVE('',#23871,#23869,#5402,.T.);
#30647=EDGE_CURVE('',#23865,#23870,#5403,.T.);
#30648=EDGE_CURVE('',#23867,#23871,#5404,.T.);
#30649=EDGE_CURVE('',#23872,#23873,#147,.T.);
#30650=EDGE_CURVE('',#23872,#23874,#5405,.T.);
#30651=EDGE_CURVE('',#23874,#23875,#148,.T.);
#30652=EDGE_CURVE('',#23873,#23875,#5406,.T.);
#30653=EDGE_CURVE('',#23876,#23872,#149,.T.);
#30654=EDGE_CURVE('',#23876,#23877,#5407,.T.);
#30655=EDGE_CURVE('',#23877,#23874,#150,.T.);
#30656=EDGE_CURVE('',#23878,#23876,#151,.T.);
#30657=EDGE_CURVE('',#23878,#23879,#5408,.T.);
#30658=EDGE_CURVE('',#23879,#23877,#152,.T.);
#30659=EDGE_CURVE('',#23880,#23878,#153,.T.);
#30660=EDGE_CURVE('',#23880,#23881,#5409,.T.);
#30661=EDGE_CURVE('',#23881,#23879,#154,.T.);
#30662=EDGE_CURVE('',#23882,#23880,#155,.T.);
#30663=EDGE_CURVE('',#23882,#23883,#5410,.T.);
#30664=EDGE_CURVE('',#23883,#23881,#156,.T.);
#30665=EDGE_CURVE('',#23884,#23882,#157,.T.);
#30666=EDGE_CURVE('',#23884,#23885,#5411,.T.);
#30667=EDGE_CURVE('',#23885,#23883,#158,.T.);
#30668=EDGE_CURVE('',#23886,#23884,#159,.T.);
#30669=EDGE_CURVE('',#23886,#23887,#5412,.T.);
#30670=EDGE_CURVE('',#23887,#23885,#160,.T.);
#30671=EDGE_CURVE('',#23888,#23886,#161,.T.);
#30672=EDGE_CURVE('',#23888,#23889,#5413,.T.);
#30673=EDGE_CURVE('',#23889,#23887,#162,.T.);
#30674=EDGE_CURVE('',#23890,#23888,#163,.T.);
#30675=EDGE_CURVE('',#23890,#23891,#5414,.T.);
#30676=EDGE_CURVE('',#23891,#23889,#164,.T.);
#30677=EDGE_CURVE('',#23892,#23890,#165,.T.);
#30678=EDGE_CURVE('',#23892,#23893,#5415,.T.);
#30679=EDGE_CURVE('',#23893,#23891,#166,.T.);
#30680=EDGE_CURVE('',#23894,#23892,#167,.T.);
#30681=EDGE_CURVE('',#23894,#23895,#5416,.T.);
#30682=EDGE_CURVE('',#23895,#23893,#168,.T.);
#30683=EDGE_CURVE('',#23896,#23894,#169,.T.);
#30684=EDGE_CURVE('',#23896,#23897,#5417,.T.);
#30685=EDGE_CURVE('',#23897,#23895,#170,.T.);
#30686=EDGE_CURVE('',#23898,#23896,#171,.T.);
#30687=EDGE_CURVE('',#23898,#23899,#5418,.T.);
#30688=EDGE_CURVE('',#23899,#23897,#172,.T.);
#30689=EDGE_CURVE('',#23900,#23898,#5419,.T.);
#30690=EDGE_CURVE('',#23900,#23901,#5420,.T.);
#30691=EDGE_CURVE('',#23901,#23899,#5421,.T.);
#30692=EDGE_CURVE('',#23902,#23900,#173,.T.);
#30693=EDGE_CURVE('',#23902,#23903,#5422,.T.);
#30694=EDGE_CURVE('',#23903,#23901,#174,.T.);
#30695=EDGE_CURVE('',#23904,#23902,#175,.T.);
#30696=EDGE_CURVE('',#23904,#23905,#5423,.T.);
#30697=EDGE_CURVE('',#23905,#23903,#176,.T.);
#30698=EDGE_CURVE('',#23906,#23904,#177,.T.);
#30699=EDGE_CURVE('',#23906,#23907,#5424,.T.);
#30700=EDGE_CURVE('',#23907,#23905,#178,.T.);
#30701=EDGE_CURVE('',#23908,#23906,#179,.T.);
#30702=EDGE_CURVE('',#23908,#23909,#5425,.T.);
#30703=EDGE_CURVE('',#23909,#23907,#180,.T.);
#30704=EDGE_CURVE('',#23910,#23908,#181,.T.);
#30705=EDGE_CURVE('',#23910,#23911,#5426,.T.);
#30706=EDGE_CURVE('',#23911,#23909,#182,.T.);
#30707=EDGE_CURVE('',#23912,#23910,#183,.T.);
#30708=EDGE_CURVE('',#23912,#23913,#5427,.T.);
#30709=EDGE_CURVE('',#23913,#23911,#184,.T.);
#30710=EDGE_CURVE('',#23914,#23912,#185,.T.);
#30711=EDGE_CURVE('',#23914,#23915,#5428,.T.);
#30712=EDGE_CURVE('',#23915,#23913,#186,.T.);
#30713=EDGE_CURVE('',#23916,#23914,#187,.T.);
#30714=EDGE_CURVE('',#23916,#23917,#5429,.T.);
#30715=EDGE_CURVE('',#23917,#23915,#188,.T.);
#30716=EDGE_CURVE('',#23918,#23916,#189,.T.);
#30717=EDGE_CURVE('',#23918,#23919,#5430,.T.);
#30718=EDGE_CURVE('',#23919,#23917,#190,.T.);
#30719=EDGE_CURVE('',#23920,#23918,#191,.T.);
#30720=EDGE_CURVE('',#23920,#23921,#5431,.T.);
#30721=EDGE_CURVE('',#23921,#23919,#192,.T.);
#30722=EDGE_CURVE('',#23922,#23920,#193,.T.);
#30723=EDGE_CURVE('',#23922,#23923,#5432,.T.);
#30724=EDGE_CURVE('',#23923,#23921,#194,.T.);
#30725=EDGE_CURVE('',#23924,#23922,#195,.T.);
#30726=EDGE_CURVE('',#23924,#23925,#5433,.T.);
#30727=EDGE_CURVE('',#23925,#23923,#196,.T.);
#30728=EDGE_CURVE('',#23926,#23924,#197,.T.);
#30729=EDGE_CURVE('',#23926,#23927,#5434,.T.);
#30730=EDGE_CURVE('',#23927,#23925,#198,.T.);
#30731=EDGE_CURVE('',#23928,#23926,#199,.T.);
#30732=EDGE_CURVE('',#23928,#23929,#5435,.T.);
#30733=EDGE_CURVE('',#23929,#23927,#200,.T.);
#30734=EDGE_CURVE('',#23930,#23928,#201,.T.);
#30735=EDGE_CURVE('',#23930,#23931,#5436,.T.);
#30736=EDGE_CURVE('',#23931,#23929,#202,.T.);
#30737=EDGE_CURVE('',#23932,#23930,#203,.T.);
#30738=EDGE_CURVE('',#23932,#23933,#5437,.T.);
#30739=EDGE_CURVE('',#23933,#23931,#204,.T.);
#30740=EDGE_CURVE('',#23934,#23932,#205,.T.);
#30741=EDGE_CURVE('',#23934,#23935,#5438,.T.);
#30742=EDGE_CURVE('',#23935,#23933,#206,.T.);
#30743=EDGE_CURVE('',#23936,#23934,#207,.T.);
#30744=EDGE_CURVE('',#23936,#23937,#5439,.T.);
#30745=EDGE_CURVE('',#23937,#23935,#208,.T.);
#30746=EDGE_CURVE('',#23938,#23936,#5440,.T.);
#30747=EDGE_CURVE('',#23938,#23939,#5441,.T.);
#30748=EDGE_CURVE('',#23939,#23937,#5442,.T.);
#30749=EDGE_CURVE('',#23940,#23938,#209,.T.);
#30750=EDGE_CURVE('',#23940,#23941,#5443,.T.);
#30751=EDGE_CURVE('',#23941,#23939,#210,.T.);
#30752=EDGE_CURVE('',#23873,#23940,#211,.T.);
#30753=EDGE_CURVE('',#23875,#23941,#212,.T.);
#30754=EDGE_CURVE('',#23942,#23943,#213,.T.);
#30755=EDGE_CURVE('',#23942,#23944,#5444,.T.);
#30756=EDGE_CURVE('',#23944,#23945,#214,.T.);
#30757=EDGE_CURVE('',#23943,#23945,#5445,.T.);
#30758=EDGE_CURVE('',#23946,#23942,#215,.T.);
#30759=EDGE_CURVE('',#23946,#23947,#5446,.T.);
#30760=EDGE_CURVE('',#23947,#23944,#216,.T.);
#30761=EDGE_CURVE('',#23948,#23946,#217,.T.);
#30762=EDGE_CURVE('',#23948,#23949,#5447,.T.);
#30763=EDGE_CURVE('',#23949,#23947,#218,.T.);
#30764=EDGE_CURVE('',#23950,#23948,#219,.T.);
#30765=EDGE_CURVE('',#23950,#23951,#5448,.T.);
#30766=EDGE_CURVE('',#23951,#23949,#220,.T.);
#30767=EDGE_CURVE('',#23952,#23950,#221,.T.);
#30768=EDGE_CURVE('',#23952,#23953,#5449,.T.);
#30769=EDGE_CURVE('',#23953,#23951,#222,.T.);
#30770=EDGE_CURVE('',#23954,#23952,#223,.T.);
#30771=EDGE_CURVE('',#23954,#23955,#5450,.T.);
#30772=EDGE_CURVE('',#23955,#23953,#224,.T.);
#30773=EDGE_CURVE('',#23956,#23954,#225,.T.);
#30774=EDGE_CURVE('',#23956,#23957,#5451,.T.);
#30775=EDGE_CURVE('',#23957,#23955,#226,.T.);
#30776=EDGE_CURVE('',#23958,#23956,#227,.T.);
#30777=EDGE_CURVE('',#23958,#23959,#5452,.T.);
#30778=EDGE_CURVE('',#23959,#23957,#228,.T.);
#30779=EDGE_CURVE('',#23960,#23958,#5453,.T.);
#30780=EDGE_CURVE('',#23960,#23961,#5454,.T.);
#30781=EDGE_CURVE('',#23961,#23959,#5455,.T.);
#30782=EDGE_CURVE('',#23962,#23960,#229,.T.);
#30783=EDGE_CURVE('',#23962,#23963,#5456,.T.);
#30784=EDGE_CURVE('',#23963,#23961,#230,.T.);
#30785=EDGE_CURVE('',#23964,#23962,#231,.T.);
#30786=EDGE_CURVE('',#23964,#23965,#5457,.T.);
#30787=EDGE_CURVE('',#23965,#23963,#232,.T.);
#30788=EDGE_CURVE('',#23966,#23964,#233,.T.);
#30789=EDGE_CURVE('',#23966,#23967,#5458,.T.);
#30790=EDGE_CURVE('',#23967,#23965,#234,.T.);
#30791=EDGE_CURVE('',#23968,#23966,#235,.T.);
#30792=EDGE_CURVE('',#23968,#23969,#5459,.T.);
#30793=EDGE_CURVE('',#23969,#23967,#236,.T.);
#30794=EDGE_CURVE('',#23970,#23968,#237,.T.);
#30795=EDGE_CURVE('',#23970,#23971,#5460,.T.);
#30796=EDGE_CURVE('',#23971,#23969,#238,.T.);
#30797=EDGE_CURVE('',#23972,#23970,#239,.T.);
#30798=EDGE_CURVE('',#23972,#23973,#5461,.T.);
#30799=EDGE_CURVE('',#23973,#23971,#240,.T.);
#30800=EDGE_CURVE('',#23974,#23972,#241,.T.);
#30801=EDGE_CURVE('',#23974,#23975,#5462,.T.);
#30802=EDGE_CURVE('',#23975,#23973,#242,.T.);
#30803=EDGE_CURVE('',#23976,#23974,#243,.T.);
#30804=EDGE_CURVE('',#23976,#23977,#5463,.T.);
#30805=EDGE_CURVE('',#23977,#23975,#244,.T.);
#30806=EDGE_CURVE('',#23978,#23976,#245,.T.);
#30807=EDGE_CURVE('',#23978,#23979,#5464,.T.);
#30808=EDGE_CURVE('',#23979,#23977,#246,.T.);
#30809=EDGE_CURVE('',#23980,#23978,#247,.T.);
#30810=EDGE_CURVE('',#23980,#23981,#5465,.T.);
#30811=EDGE_CURVE('',#23981,#23979,#248,.T.);
#30812=EDGE_CURVE('',#23982,#23980,#5466,.T.);
#30813=EDGE_CURVE('',#23982,#23983,#5467,.T.);
#30814=EDGE_CURVE('',#23983,#23981,#5468,.T.);
#30815=EDGE_CURVE('',#23984,#23982,#249,.T.);
#30816=EDGE_CURVE('',#23984,#23985,#5469,.T.);
#30817=EDGE_CURVE('',#23985,#23983,#250,.T.);
#30818=EDGE_CURVE('',#23943,#23984,#251,.T.);
#30819=EDGE_CURVE('',#23945,#23985,#252,.T.);
#30820=EDGE_CURVE('',#23986,#23987,#5470,.T.);
#30821=EDGE_CURVE('',#23986,#23988,#5471,.T.);
#30822=EDGE_CURVE('',#23988,#23989,#5472,.T.);
#30823=EDGE_CURVE('',#23987,#23989,#5473,.T.);
#30824=EDGE_CURVE('',#23990,#23986,#5474,.T.);
#30825=EDGE_CURVE('',#23990,#23991,#5475,.T.);
#30826=EDGE_CURVE('',#23991,#23988,#5476,.T.);
#30827=EDGE_CURVE('',#23992,#23990,#5477,.T.);
#30828=EDGE_CURVE('',#23992,#23993,#5478,.T.);
#30829=EDGE_CURVE('',#23993,#23991,#5479,.T.);
#30830=EDGE_CURVE('',#23994,#23992,#5480,.T.);
#30831=EDGE_CURVE('',#23994,#23995,#5481,.T.);
#30832=EDGE_CURVE('',#23995,#23993,#5482,.T.);
#30833=EDGE_CURVE('',#23996,#23994,#5483,.T.);
#30834=EDGE_CURVE('',#23996,#23997,#5484,.T.);
#30835=EDGE_CURVE('',#23997,#23995,#5485,.T.);
#30836=EDGE_CURVE('',#23987,#23996,#5486,.T.);
#30837=EDGE_CURVE('',#23989,#23997,#5487,.T.);
#30838=EDGE_CURVE('',#23998,#23999,#5488,.T.);
#30839=EDGE_CURVE('',#23998,#24000,#5489,.T.);
#30840=EDGE_CURVE('',#24000,#24001,#5490,.T.);
#30841=EDGE_CURVE('',#23999,#24001,#5491,.T.);
#30842=EDGE_CURVE('',#24002,#23998,#5492,.T.);
#30843=EDGE_CURVE('',#24002,#24003,#5493,.T.);
#30844=EDGE_CURVE('',#24003,#24000,#5494,.T.);
#30845=EDGE_CURVE('',#24004,#24002,#5495,.T.);
#30846=EDGE_CURVE('',#24004,#24005,#5496,.T.);
#30847=EDGE_CURVE('',#24005,#24003,#5497,.T.);
#30848=EDGE_CURVE('',#24006,#24004,#5498,.T.);
#30849=EDGE_CURVE('',#24006,#24007,#5499,.T.);
#30850=EDGE_CURVE('',#24007,#24005,#5500,.T.);
#30851=EDGE_CURVE('',#24008,#24006,#5501,.T.);
#30852=EDGE_CURVE('',#24008,#24009,#5502,.T.);
#30853=EDGE_CURVE('',#24009,#24007,#5503,.T.);
#30854=EDGE_CURVE('',#24010,#24008,#5504,.T.);
#30855=EDGE_CURVE('',#24010,#24011,#5505,.T.);
#30856=EDGE_CURVE('',#24011,#24009,#5506,.T.);
#30857=EDGE_CURVE('',#24012,#24010,#5507,.T.);
#30858=EDGE_CURVE('',#24012,#24013,#5508,.T.);
#30859=EDGE_CURVE('',#24013,#24011,#5509,.T.);
#30860=EDGE_CURVE('',#23999,#24012,#5510,.T.);
#30861=EDGE_CURVE('',#24001,#24013,#5511,.T.);
#30862=EDGE_CURVE('',#24014,#24015,#253,.T.);
#30863=EDGE_CURVE('',#24014,#24016,#5512,.T.);
#30864=EDGE_CURVE('',#24016,#24017,#254,.T.);
#30865=EDGE_CURVE('',#24015,#24017,#5513,.T.);
#30866=EDGE_CURVE('',#24018,#24014,#255,.T.);
#30867=EDGE_CURVE('',#24018,#24019,#5514,.T.);
#30868=EDGE_CURVE('',#24019,#24016,#256,.T.);
#30869=EDGE_CURVE('',#24020,#24018,#257,.T.);
#30870=EDGE_CURVE('',#24020,#24021,#5515,.T.);
#30871=EDGE_CURVE('',#24021,#24019,#258,.T.);
#30872=EDGE_CURVE('',#24022,#24020,#259,.T.);
#30873=EDGE_CURVE('',#24022,#24023,#5516,.T.);
#30874=EDGE_CURVE('',#24023,#24021,#260,.T.);
#30875=EDGE_CURVE('',#24024,#24022,#5517,.T.);
#30876=EDGE_CURVE('',#24024,#24025,#5518,.T.);
#30877=EDGE_CURVE('',#24025,#24023,#5519,.T.);
#30878=EDGE_CURVE('',#24026,#24024,#5520,.T.);
#30879=EDGE_CURVE('',#24026,#24027,#5521,.T.);
#30880=EDGE_CURVE('',#24027,#24025,#5522,.T.);
#30881=EDGE_CURVE('',#24028,#24026,#5523,.T.);
#30882=EDGE_CURVE('',#24028,#24029,#5524,.T.);
#30883=EDGE_CURVE('',#24029,#24027,#5525,.T.);
#30884=EDGE_CURVE('',#24030,#24028,#261,.T.);
#30885=EDGE_CURVE('',#24030,#24031,#5526,.T.);
#30886=EDGE_CURVE('',#24031,#24029,#262,.T.);
#30887=EDGE_CURVE('',#24032,#24030,#263,.T.);
#30888=EDGE_CURVE('',#24032,#24033,#5527,.T.);
#30889=EDGE_CURVE('',#24033,#24031,#264,.T.);
#30890=EDGE_CURVE('',#24034,#24032,#265,.T.);
#30891=EDGE_CURVE('',#24034,#24035,#5528,.T.);
#30892=EDGE_CURVE('',#24035,#24033,#266,.T.);
#30893=EDGE_CURVE('',#24036,#24034,#267,.T.);
#30894=EDGE_CURVE('',#24036,#24037,#5529,.T.);
#30895=EDGE_CURVE('',#24037,#24035,#268,.T.);
#30896=EDGE_CURVE('',#24038,#24036,#269,.T.);
#30897=EDGE_CURVE('',#24038,#24039,#5530,.T.);
#30898=EDGE_CURVE('',#24039,#24037,#270,.T.);
#30899=EDGE_CURVE('',#24040,#24038,#271,.T.);
#30900=EDGE_CURVE('',#24040,#24041,#5531,.T.);
#30901=EDGE_CURVE('',#24041,#24039,#272,.T.);
#30902=EDGE_CURVE('',#24042,#24040,#5532,.T.);
#30903=EDGE_CURVE('',#24042,#24043,#5533,.T.);
#30904=EDGE_CURVE('',#24043,#24041,#5534,.T.);
#30905=EDGE_CURVE('',#24044,#24042,#5535,.T.);
#30906=EDGE_CURVE('',#24044,#24045,#5536,.T.);
#30907=EDGE_CURVE('',#24045,#24043,#5537,.T.);
#30908=EDGE_CURVE('',#24046,#24044,#5538,.T.);
#30909=EDGE_CURVE('',#24046,#24047,#5539,.T.);
#30910=EDGE_CURVE('',#24047,#24045,#5540,.T.);
#30911=EDGE_CURVE('',#24015,#24046,#273,.T.);
#30912=EDGE_CURVE('',#24017,#24047,#274,.T.);
#30913=EDGE_CURVE('',#24048,#24049,#5541,.T.);
#30914=EDGE_CURVE('',#24048,#24050,#5542,.T.);
#30915=EDGE_CURVE('',#24050,#24051,#5543,.T.);
#30916=EDGE_CURVE('',#24049,#24051,#5544,.T.);
#30917=EDGE_CURVE('',#24052,#24048,#275,.T.);
#30918=EDGE_CURVE('',#24052,#24053,#5545,.T.);
#30919=EDGE_CURVE('',#24053,#24050,#276,.T.);
#30920=EDGE_CURVE('',#24054,#24052,#277,.T.);
#30921=EDGE_CURVE('',#24054,#24055,#5546,.T.);
#30922=EDGE_CURVE('',#24055,#24053,#278,.T.);
#30923=EDGE_CURVE('',#24056,#24054,#279,.T.);
#30924=EDGE_CURVE('',#24056,#24057,#5547,.T.);
#30925=EDGE_CURVE('',#24057,#24055,#280,.T.);
#30926=EDGE_CURVE('',#24058,#24056,#281,.T.);
#30927=EDGE_CURVE('',#24058,#24059,#5548,.T.);
#30928=EDGE_CURVE('',#24059,#24057,#282,.T.);
#30929=EDGE_CURVE('',#24060,#24058,#5549,.T.);
#30930=EDGE_CURVE('',#24060,#24061,#5550,.T.);
#30931=EDGE_CURVE('',#24061,#24059,#5551,.T.);
#30932=EDGE_CURVE('',#24062,#24060,#5552,.T.);
#30933=EDGE_CURVE('',#24062,#24063,#5553,.T.);
#30934=EDGE_CURVE('',#24063,#24061,#5554,.T.);
#30935=EDGE_CURVE('',#24064,#24062,#5555,.T.);
#30936=EDGE_CURVE('',#24064,#24065,#5556,.T.);
#30937=EDGE_CURVE('',#24065,#24063,#5557,.T.);
#30938=EDGE_CURVE('',#24066,#24064,#283,.T.);
#30939=EDGE_CURVE('',#24066,#24067,#5558,.T.);
#30940=EDGE_CURVE('',#24067,#24065,#284,.T.);
#30941=EDGE_CURVE('',#24068,#24066,#285,.T.);
#30942=EDGE_CURVE('',#24068,#24069,#5559,.T.);
#30943=EDGE_CURVE('',#24069,#24067,#286,.T.);
#30944=EDGE_CURVE('',#24070,#24068,#287,.T.);
#30945=EDGE_CURVE('',#24070,#24071,#5560,.T.);
#30946=EDGE_CURVE('',#24071,#24069,#288,.T.);
#30947=EDGE_CURVE('',#24072,#24070,#289,.T.);
#30948=EDGE_CURVE('',#24072,#24073,#5561,.T.);
#30949=EDGE_CURVE('',#24073,#24071,#290,.T.);
#30950=EDGE_CURVE('',#24074,#24072,#291,.T.);
#30951=EDGE_CURVE('',#24074,#24075,#5562,.T.);
#30952=EDGE_CURVE('',#24075,#24073,#292,.T.);
#30953=EDGE_CURVE('',#24076,#24074,#293,.T.);
#30954=EDGE_CURVE('',#24076,#24077,#5563,.T.);
#30955=EDGE_CURVE('',#24077,#24075,#294,.T.);
#30956=EDGE_CURVE('',#24078,#24076,#295,.T.);
#30957=EDGE_CURVE('',#24078,#24079,#5564,.T.);
#30958=EDGE_CURVE('',#24079,#24077,#296,.T.);
#30959=EDGE_CURVE('',#24080,#24078,#5565,.T.);
#30960=EDGE_CURVE('',#24080,#24081,#5566,.T.);
#30961=EDGE_CURVE('',#24081,#24079,#5567,.T.);
#30962=EDGE_CURVE('',#24082,#24080,#5568,.T.);
#30963=EDGE_CURVE('',#24082,#24083,#5569,.T.);
#30964=EDGE_CURVE('',#24083,#24081,#5570,.T.);
#30965=EDGE_CURVE('',#24084,#24082,#5571,.T.);
#30966=EDGE_CURVE('',#24084,#24085,#5572,.T.);
#30967=EDGE_CURVE('',#24085,#24083,#5573,.T.);
#30968=EDGE_CURVE('',#24049,#24084,#5574,.T.);
#30969=EDGE_CURVE('',#24051,#24085,#5575,.T.);
#30970=EDGE_CURVE('',#24086,#24087,#5576,.T.);
#30971=EDGE_CURVE('',#24086,#24088,#5577,.T.);
#30972=EDGE_CURVE('',#24088,#24089,#5578,.T.);
#30973=EDGE_CURVE('',#24087,#24089,#5579,.T.);
#30974=EDGE_CURVE('',#24090,#24086,#5580,.T.);
#30975=EDGE_CURVE('',#24090,#24091,#5581,.T.);
#30976=EDGE_CURVE('',#24091,#24088,#5582,.T.);
#30977=EDGE_CURVE('',#24092,#24090,#5583,.T.);
#30978=EDGE_CURVE('',#24092,#24093,#5584,.T.);
#30979=EDGE_CURVE('',#24093,#24091,#5585,.T.);
#30980=EDGE_CURVE('',#24094,#24092,#5586,.T.);
#30981=EDGE_CURVE('',#24094,#24095,#5587,.T.);
#30982=EDGE_CURVE('',#24095,#24093,#5588,.T.);
#30983=EDGE_CURVE('',#24096,#24094,#5589,.T.);
#30984=EDGE_CURVE('',#24096,#24097,#5590,.T.);
#30985=EDGE_CURVE('',#24097,#24095,#5591,.T.);
#30986=EDGE_CURVE('',#24098,#24096,#5592,.T.);
#30987=EDGE_CURVE('',#24098,#24099,#5593,.T.);
#30988=EDGE_CURVE('',#24099,#24097,#5594,.T.);
#30989=EDGE_CURVE('',#24100,#24098,#5595,.T.);
#30990=EDGE_CURVE('',#24100,#24101,#5596,.T.);
#30991=EDGE_CURVE('',#24101,#24099,#5597,.T.);
#30992=EDGE_CURVE('',#24087,#24100,#5598,.T.);
#30993=EDGE_CURVE('',#24089,#24101,#5599,.T.);
#30994=EDGE_CURVE('',#24102,#24103,#297,.T.);
#30995=EDGE_CURVE('',#24102,#24104,#5600,.T.);
#30996=EDGE_CURVE('',#24104,#24105,#298,.T.);
#30997=EDGE_CURVE('',#24103,#24105,#5601,.T.);
#30998=EDGE_CURVE('',#24106,#24102,#299,.T.);
#30999=EDGE_CURVE('',#24106,#24107,#5602,.T.);
#31000=EDGE_CURVE('',#24107,#24104,#300,.T.);
#31001=EDGE_CURVE('',#24108,#24106,#5603,.T.);
#31002=EDGE_CURVE('',#24108,#24109,#5604,.T.);
#31003=EDGE_CURVE('',#24109,#24107,#5605,.T.);
#31004=EDGE_CURVE('',#24110,#24108,#301,.T.);
#31005=EDGE_CURVE('',#24110,#24111,#5606,.T.);
#31006=EDGE_CURVE('',#24111,#24109,#302,.T.);
#31007=EDGE_CURVE('',#24112,#24110,#303,.T.);
#31008=EDGE_CURVE('',#24112,#24113,#5607,.T.);
#31009=EDGE_CURVE('',#24113,#24111,#304,.T.);
#31010=EDGE_CURVE('',#24114,#24112,#5608,.T.);
#31011=EDGE_CURVE('',#24114,#24115,#5609,.T.);
#31012=EDGE_CURVE('',#24115,#24113,#5610,.T.);
#31013=EDGE_CURVE('',#24116,#24114,#5611,.T.);
#31014=EDGE_CURVE('',#24116,#24117,#5612,.T.);
#31015=EDGE_CURVE('',#24117,#24115,#5613,.T.);
#31016=EDGE_CURVE('',#24118,#24116,#5614,.T.);
#31017=EDGE_CURVE('',#24118,#24119,#5615,.T.);
#31018=EDGE_CURVE('',#24119,#24117,#5616,.T.);
#31019=EDGE_CURVE('',#24103,#24118,#5617,.T.);
#31020=EDGE_CURVE('',#24105,#24119,#5618,.T.);
#31021=EDGE_CURVE('',#24120,#24121,#305,.T.);
#31022=EDGE_CURVE('',#24120,#24122,#5619,.T.);
#31023=EDGE_CURVE('',#24122,#24123,#306,.T.);
#31024=EDGE_CURVE('',#24121,#24123,#5620,.T.);
#31025=EDGE_CURVE('',#24124,#24120,#307,.T.);
#31026=EDGE_CURVE('',#24124,#24125,#5621,.T.);
#31027=EDGE_CURVE('',#24125,#24122,#308,.T.);
#31028=EDGE_CURVE('',#24126,#24124,#309,.T.);
#31029=EDGE_CURVE('',#24126,#24127,#5622,.T.);
#31030=EDGE_CURVE('',#24127,#24125,#310,.T.);
#31031=EDGE_CURVE('',#24128,#24126,#311,.T.);
#31032=EDGE_CURVE('',#24128,#24129,#5623,.T.);
#31033=EDGE_CURVE('',#24129,#24127,#312,.T.);
#31034=EDGE_CURVE('',#24130,#24128,#313,.T.);
#31035=EDGE_CURVE('',#24130,#24131,#5624,.T.);
#31036=EDGE_CURVE('',#24131,#24129,#314,.T.);
#31037=EDGE_CURVE('',#24132,#24130,#315,.T.);
#31038=EDGE_CURVE('',#24132,#24133,#5625,.T.);
#31039=EDGE_CURVE('',#24133,#24131,#316,.T.);
#31040=EDGE_CURVE('',#24134,#24132,#317,.T.);
#31041=EDGE_CURVE('',#24134,#24135,#5626,.T.);
#31042=EDGE_CURVE('',#24135,#24133,#318,.T.);
#31043=EDGE_CURVE('',#24136,#24134,#319,.T.);
#31044=EDGE_CURVE('',#24136,#24137,#5627,.T.);
#31045=EDGE_CURVE('',#24137,#24135,#320,.T.);
#31046=EDGE_CURVE('',#24138,#24136,#321,.T.);
#31047=EDGE_CURVE('',#24138,#24139,#5628,.T.);
#31048=EDGE_CURVE('',#24139,#24137,#322,.T.);
#31049=EDGE_CURVE('',#24140,#24138,#323,.T.);
#31050=EDGE_CURVE('',#24140,#24141,#5629,.T.);
#31051=EDGE_CURVE('',#24141,#24139,#324,.T.);
#31052=EDGE_CURVE('',#24142,#24140,#325,.T.);
#31053=EDGE_CURVE('',#24142,#24143,#5630,.T.);
#31054=EDGE_CURVE('',#24143,#24141,#326,.T.);
#31055=EDGE_CURVE('',#24121,#24142,#327,.T.);
#31056=EDGE_CURVE('',#24123,#24143,#328,.T.);
#31057=EDGE_CURVE('',#24144,#24145,#329,.T.);
#31058=EDGE_CURVE('',#24144,#24146,#5631,.T.);
#31059=EDGE_CURVE('',#24146,#24147,#330,.T.);
#31060=EDGE_CURVE('',#24145,#24147,#5632,.T.);
#31061=EDGE_CURVE('',#24148,#24144,#331,.T.);
#31062=EDGE_CURVE('',#24148,#24149,#5633,.T.);
#31063=EDGE_CURVE('',#24149,#24146,#332,.T.);
#31064=EDGE_CURVE('',#24150,#24148,#5634,.T.);
#31065=EDGE_CURVE('',#24150,#24151,#5635,.T.);
#31066=EDGE_CURVE('',#24151,#24149,#5636,.T.);
#31067=EDGE_CURVE('',#24152,#24150,#333,.T.);
#31068=EDGE_CURVE('',#24152,#24153,#5637,.T.);
#31069=EDGE_CURVE('',#24153,#24151,#334,.T.);
#31070=EDGE_CURVE('',#24154,#24152,#335,.T.);
#31071=EDGE_CURVE('',#24154,#24155,#5638,.T.);
#31072=EDGE_CURVE('',#24155,#24153,#336,.T.);
#31073=EDGE_CURVE('',#24156,#24154,#5639,.T.);
#31074=EDGE_CURVE('',#24156,#24157,#5640,.T.);
#31075=EDGE_CURVE('',#24157,#24155,#5641,.T.);
#31076=EDGE_CURVE('',#24158,#24156,#5642,.T.);
#31077=EDGE_CURVE('',#24158,#24159,#5643,.T.);
#31078=EDGE_CURVE('',#24159,#24157,#5644,.T.);
#31079=EDGE_CURVE('',#24160,#24158,#5645,.T.);
#31080=EDGE_CURVE('',#24160,#24161,#5646,.T.);
#31081=EDGE_CURVE('',#24161,#24159,#5647,.T.);
#31082=EDGE_CURVE('',#24145,#24160,#5648,.T.);
#31083=EDGE_CURVE('',#24147,#24161,#5649,.T.);
#31084=EDGE_CURVE('',#24162,#24163,#5650,.T.);
#31085=EDGE_CURVE('',#24162,#24164,#5651,.T.);
#31086=EDGE_CURVE('',#24164,#24165,#5652,.T.);
#31087=EDGE_CURVE('',#24163,#24165,#5653,.T.);
#31088=EDGE_CURVE('',#24166,#24162,#5654,.T.);
#31089=EDGE_CURVE('',#24166,#24167,#5655,.T.);
#31090=EDGE_CURVE('',#24167,#24164,#5656,.T.);
#31091=EDGE_CURVE('',#24168,#24166,#5657,.T.);
#31092=EDGE_CURVE('',#24168,#24169,#5658,.T.);
#31093=EDGE_CURVE('',#24169,#24167,#5659,.T.);
#31094=EDGE_CURVE('',#24163,#24168,#5660,.T.);
#31095=EDGE_CURVE('',#24165,#24169,#5661,.T.);
#31096=EDGE_CURVE('',#24170,#24171,#337,.T.);
#31097=EDGE_CURVE('',#24170,#24172,#5662,.T.);
#31098=EDGE_CURVE('',#24172,#24173,#338,.T.);
#31099=EDGE_CURVE('',#24171,#24173,#5663,.T.);
#31100=EDGE_CURVE('',#24174,#24170,#339,.T.);
#31101=EDGE_CURVE('',#24174,#24175,#5664,.T.);
#31102=EDGE_CURVE('',#24175,#24172,#340,.T.);
#31103=EDGE_CURVE('',#24176,#24174,#341,.T.);
#31104=EDGE_CURVE('',#24176,#24177,#5665,.T.);
#31105=EDGE_CURVE('',#24177,#24175,#342,.T.);
#31106=EDGE_CURVE('',#24178,#24176,#343,.T.);
#31107=EDGE_CURVE('',#24178,#24179,#5666,.T.);
#31108=EDGE_CURVE('',#24179,#24177,#344,.T.);
#31109=EDGE_CURVE('',#24180,#24178,#345,.T.);
#31110=EDGE_CURVE('',#24180,#24181,#5667,.T.);
#31111=EDGE_CURVE('',#24181,#24179,#346,.T.);
#31112=EDGE_CURVE('',#24182,#24180,#5668,.T.);
#31113=EDGE_CURVE('',#24182,#24183,#5669,.T.);
#31114=EDGE_CURVE('',#24183,#24181,#5670,.T.);
#31115=EDGE_CURVE('',#24184,#24182,#5671,.T.);
#31116=EDGE_CURVE('',#24184,#24185,#5672,.T.);
#31117=EDGE_CURVE('',#24185,#24183,#5673,.T.);
#31118=EDGE_CURVE('',#24186,#24184,#5674,.T.);
#31119=EDGE_CURVE('',#24186,#24187,#5675,.T.);
#31120=EDGE_CURVE('',#24187,#24185,#5676,.T.);
#31121=EDGE_CURVE('',#24188,#24186,#5677,.T.);
#31122=EDGE_CURVE('',#24188,#24189,#5678,.T.);
#31123=EDGE_CURVE('',#24189,#24187,#5679,.T.);
#31124=EDGE_CURVE('',#24190,#24188,#5680,.T.);
#31125=EDGE_CURVE('',#24190,#24191,#5681,.T.);
#31126=EDGE_CURVE('',#24191,#24189,#5682,.T.);
#31127=EDGE_CURVE('',#24192,#24190,#5683,.T.);
#31128=EDGE_CURVE('',#24192,#24193,#5684,.T.);
#31129=EDGE_CURVE('',#24193,#24191,#5685,.T.);
#31130=EDGE_CURVE('',#24194,#24192,#347,.T.);
#31131=EDGE_CURVE('',#24194,#24195,#5686,.T.);
#31132=EDGE_CURVE('',#24195,#24193,#348,.T.);
#31133=EDGE_CURVE('',#24196,#24194,#349,.T.);
#31134=EDGE_CURVE('',#24196,#24197,#5687,.T.);
#31135=EDGE_CURVE('',#24197,#24195,#350,.T.);
#31136=EDGE_CURVE('',#24198,#24196,#351,.T.);
#31137=EDGE_CURVE('',#24198,#24199,#5688,.T.);
#31138=EDGE_CURVE('',#24199,#24197,#352,.T.);
#31139=EDGE_CURVE('',#24200,#24198,#353,.T.);
#31140=EDGE_CURVE('',#24200,#24201,#5689,.T.);
#31141=EDGE_CURVE('',#24201,#24199,#354,.T.);
#31142=EDGE_CURVE('',#24202,#24200,#355,.T.);
#31143=EDGE_CURVE('',#24202,#24203,#5690,.T.);
#31144=EDGE_CURVE('',#24203,#24201,#356,.T.);
#31145=EDGE_CURVE('',#24204,#24202,#357,.T.);
#31146=EDGE_CURVE('',#24204,#24205,#5691,.T.);
#31147=EDGE_CURVE('',#24205,#24203,#358,.T.);
#31148=EDGE_CURVE('',#24206,#24204,#359,.T.);
#31149=EDGE_CURVE('',#24206,#24207,#5692,.T.);
#31150=EDGE_CURVE('',#24207,#24205,#360,.T.);
#31151=EDGE_CURVE('',#24208,#24206,#361,.T.);
#31152=EDGE_CURVE('',#24208,#24209,#5693,.T.);
#31153=EDGE_CURVE('',#24209,#24207,#362,.T.);
#31154=EDGE_CURVE('',#24210,#24208,#5694,.T.);
#31155=EDGE_CURVE('',#24210,#24211,#5695,.T.);
#31156=EDGE_CURVE('',#24211,#24209,#5696,.T.);
#31157=EDGE_CURVE('',#24212,#24210,#363,.T.);
#31158=EDGE_CURVE('',#24212,#24213,#5697,.T.);
#31159=EDGE_CURVE('',#24213,#24211,#364,.T.);
#31160=EDGE_CURVE('',#24171,#24212,#365,.T.);
#31161=EDGE_CURVE('',#24173,#24213,#366,.T.);
#31162=EDGE_CURVE('',#24214,#24215,#367,.T.);
#31163=EDGE_CURVE('',#24214,#24216,#5698,.T.);
#31164=EDGE_CURVE('',#24216,#24217,#368,.T.);
#31165=EDGE_CURVE('',#24215,#24217,#5699,.T.);
#31166=EDGE_CURVE('',#24218,#24214,#369,.T.);
#31167=EDGE_CURVE('',#24218,#24219,#5700,.T.);
#31168=EDGE_CURVE('',#24219,#24216,#370,.T.);
#31169=EDGE_CURVE('',#24220,#24218,#371,.T.);
#31170=EDGE_CURVE('',#24220,#24221,#5701,.T.);
#31171=EDGE_CURVE('',#24221,#24219,#372,.T.);
#31172=EDGE_CURVE('',#24222,#24220,#373,.T.);
#31173=EDGE_CURVE('',#24222,#24223,#5702,.T.);
#31174=EDGE_CURVE('',#24223,#24221,#374,.T.);
#31175=EDGE_CURVE('',#24224,#24222,#375,.T.);
#31176=EDGE_CURVE('',#24224,#24225,#5703,.T.);
#31177=EDGE_CURVE('',#24225,#24223,#376,.T.);
#31178=EDGE_CURVE('',#24226,#24224,#377,.T.);
#31179=EDGE_CURVE('',#24226,#24227,#5704,.T.);
#31180=EDGE_CURVE('',#24227,#24225,#378,.T.);
#31181=EDGE_CURVE('',#24228,#24226,#379,.T.);
#31182=EDGE_CURVE('',#24228,#24229,#5705,.T.);
#31183=EDGE_CURVE('',#24229,#24227,#380,.T.);
#31184=EDGE_CURVE('',#24230,#24228,#381,.T.);
#31185=EDGE_CURVE('',#24230,#24231,#5706,.T.);
#31186=EDGE_CURVE('',#24231,#24229,#382,.T.);
#31187=EDGE_CURVE('',#24232,#24230,#383,.T.);
#31188=EDGE_CURVE('',#24232,#24233,#5707,.T.);
#31189=EDGE_CURVE('',#24233,#24231,#384,.T.);
#31190=EDGE_CURVE('',#24234,#24232,#385,.T.);
#31191=EDGE_CURVE('',#24234,#24235,#5708,.T.);
#31192=EDGE_CURVE('',#24235,#24233,#386,.T.);
#31193=EDGE_CURVE('',#24215,#24234,#387,.T.);
#31194=EDGE_CURVE('',#24217,#24235,#388,.T.);
#31195=EDGE_CURVE('',#24236,#24237,#389,.T.);
#31196=EDGE_CURVE('',#24236,#24238,#5709,.T.);
#31197=EDGE_CURVE('',#24238,#24239,#390,.T.);
#31198=EDGE_CURVE('',#24237,#24239,#5710,.T.);
#31199=EDGE_CURVE('',#24240,#24236,#391,.T.);
#31200=EDGE_CURVE('',#24240,#24241,#5711,.T.);
#31201=EDGE_CURVE('',#24241,#24238,#392,.T.);
#31202=EDGE_CURVE('',#24242,#24240,#393,.T.);
#31203=EDGE_CURVE('',#24242,#24243,#5712,.T.);
#31204=EDGE_CURVE('',#24243,#24241,#394,.T.);
#31205=EDGE_CURVE('',#24244,#24242,#395,.T.);
#31206=EDGE_CURVE('',#24244,#24245,#5713,.T.);
#31207=EDGE_CURVE('',#24245,#24243,#396,.T.);
#31208=EDGE_CURVE('',#24246,#24244,#397,.T.);
#31209=EDGE_CURVE('',#24246,#24247,#5714,.T.);
#31210=EDGE_CURVE('',#24247,#24245,#398,.T.);
#31211=EDGE_CURVE('',#24248,#24246,#399,.T.);
#31212=EDGE_CURVE('',#24248,#24249,#5715,.T.);
#31213=EDGE_CURVE('',#24249,#24247,#400,.T.);
#31214=EDGE_CURVE('',#24250,#24248,#401,.T.);
#31215=EDGE_CURVE('',#24250,#24251,#5716,.T.);
#31216=EDGE_CURVE('',#24251,#24249,#402,.T.);
#31217=EDGE_CURVE('',#24252,#24250,#403,.T.);
#31218=EDGE_CURVE('',#24252,#24253,#5717,.T.);
#31219=EDGE_CURVE('',#24253,#24251,#404,.T.);
#31220=EDGE_CURVE('',#24254,#24252,#405,.T.);
#31221=EDGE_CURVE('',#24254,#24255,#5718,.T.);
#31222=EDGE_CURVE('',#24255,#24253,#406,.T.);
#31223=EDGE_CURVE('',#24256,#24254,#407,.T.);
#31224=EDGE_CURVE('',#24256,#24257,#5719,.T.);
#31225=EDGE_CURVE('',#24257,#24255,#408,.T.);
#31226=EDGE_CURVE('',#24258,#24256,#409,.T.);
#31227=EDGE_CURVE('',#24258,#24259,#5720,.T.);
#31228=EDGE_CURVE('',#24259,#24257,#410,.T.);
#31229=EDGE_CURVE('',#24260,#24258,#5721,.T.);
#31230=EDGE_CURVE('',#24260,#24261,#5722,.T.);
#31231=EDGE_CURVE('',#24261,#24259,#5723,.T.);
#31232=EDGE_CURVE('',#24262,#24260,#411,.T.);
#31233=EDGE_CURVE('',#24262,#24263,#5724,.T.);
#31234=EDGE_CURVE('',#24263,#24261,#412,.T.);
#31235=EDGE_CURVE('',#24264,#24262,#413,.T.);
#31236=EDGE_CURVE('',#24264,#24265,#5725,.T.);
#31237=EDGE_CURVE('',#24265,#24263,#414,.T.);
#31238=EDGE_CURVE('',#24237,#24264,#415,.T.);
#31239=EDGE_CURVE('',#24239,#24265,#416,.T.);
#31240=EDGE_CURVE('',#24266,#24267,#5726,.T.);
#31241=EDGE_CURVE('',#24266,#24268,#5727,.T.);
#31242=EDGE_CURVE('',#24268,#24269,#5728,.T.);
#31243=EDGE_CURVE('',#24267,#24269,#5729,.T.);
#31244=EDGE_CURVE('',#24270,#24266,#5730,.T.);
#31245=EDGE_CURVE('',#24270,#24271,#5731,.T.);
#31246=EDGE_CURVE('',#24271,#24268,#5732,.T.);
#31247=EDGE_CURVE('',#24272,#24270,#5733,.T.);
#31248=EDGE_CURVE('',#24272,#24273,#5734,.T.);
#31249=EDGE_CURVE('',#24273,#24271,#5735,.T.);
#31250=EDGE_CURVE('',#24274,#24272,#5736,.T.);
#31251=EDGE_CURVE('',#24274,#24275,#5737,.T.);
#31252=EDGE_CURVE('',#24275,#24273,#5738,.T.);
#31253=EDGE_CURVE('',#24276,#24274,#5739,.T.);
#31254=EDGE_CURVE('',#24276,#24277,#5740,.T.);
#31255=EDGE_CURVE('',#24277,#24275,#5741,.T.);
#31256=EDGE_CURVE('',#24278,#24276,#5742,.T.);
#31257=EDGE_CURVE('',#24278,#24279,#5743,.T.);
#31258=EDGE_CURVE('',#24279,#24277,#5744,.T.);
#31259=EDGE_CURVE('',#24280,#24278,#5745,.T.);
#31260=EDGE_CURVE('',#24280,#24281,#5746,.T.);
#31261=EDGE_CURVE('',#24281,#24279,#5747,.T.);
#31262=EDGE_CURVE('',#24282,#24280,#5748,.T.);
#31263=EDGE_CURVE('',#24282,#24283,#5749,.T.);
#31264=EDGE_CURVE('',#24283,#24281,#5750,.T.);
#31265=EDGE_CURVE('',#24284,#24282,#5751,.T.);
#31266=EDGE_CURVE('',#24284,#24285,#5752,.T.);
#31267=EDGE_CURVE('',#24285,#24283,#5753,.T.);
#31268=EDGE_CURVE('',#24286,#24284,#5754,.T.);
#31269=EDGE_CURVE('',#24286,#24287,#5755,.T.);
#31270=EDGE_CURVE('',#24287,#24285,#5756,.T.);
#31271=EDGE_CURVE('',#24288,#24286,#5757,.T.);
#31272=EDGE_CURVE('',#24288,#24289,#5758,.T.);
#31273=EDGE_CURVE('',#24289,#24287,#5759,.T.);
#31274=EDGE_CURVE('',#24267,#24288,#5760,.T.);
#31275=EDGE_CURVE('',#24269,#24289,#5761,.T.);
#31276=EDGE_CURVE('',#24290,#24291,#5762,.T.);
#31277=EDGE_CURVE('',#24290,#24292,#5763,.T.);
#31278=EDGE_CURVE('',#24292,#24293,#5764,.T.);
#31279=EDGE_CURVE('',#24291,#24293,#5765,.T.);
#31280=EDGE_CURVE('',#24294,#24290,#5766,.T.);
#31281=EDGE_CURVE('',#24294,#24295,#5767,.T.);
#31282=EDGE_CURVE('',#24295,#24292,#5768,.T.);
#31283=EDGE_CURVE('',#24296,#24294,#5769,.T.);
#31284=EDGE_CURVE('',#24296,#24297,#5770,.T.);
#31285=EDGE_CURVE('',#24297,#24295,#5771,.T.);
#31286=EDGE_CURVE('',#24291,#24296,#5772,.T.);
#31287=EDGE_CURVE('',#24293,#24297,#5773,.T.);
#31288=EDGE_CURVE('',#24298,#24299,#417,.T.);
#31289=EDGE_CURVE('',#24298,#24300,#5774,.T.);
#31290=EDGE_CURVE('',#24300,#24301,#418,.T.);
#31291=EDGE_CURVE('',#24299,#24301,#5775,.T.);
#31292=EDGE_CURVE('',#24302,#24298,#419,.T.);
#31293=EDGE_CURVE('',#24302,#24303,#5776,.T.);
#31294=EDGE_CURVE('',#24303,#24300,#420,.T.);
#31295=EDGE_CURVE('',#24304,#24302,#421,.T.);
#31296=EDGE_CURVE('',#24304,#24305,#5777,.T.);
#31297=EDGE_CURVE('',#24305,#24303,#422,.T.);
#31298=EDGE_CURVE('',#24306,#24304,#423,.T.);
#31299=EDGE_CURVE('',#24306,#24307,#5778,.T.);
#31300=EDGE_CURVE('',#24307,#24305,#424,.T.);
#31301=EDGE_CURVE('',#24308,#24306,#425,.T.);
#31302=EDGE_CURVE('',#24308,#24309,#5779,.T.);
#31303=EDGE_CURVE('',#24309,#24307,#426,.T.);
#31304=EDGE_CURVE('',#24310,#24308,#427,.T.);
#31305=EDGE_CURVE('',#24310,#24311,#5780,.T.);
#31306=EDGE_CURVE('',#24311,#24309,#428,.T.);
#31307=EDGE_CURVE('',#24312,#24310,#429,.T.);
#31308=EDGE_CURVE('',#24312,#24313,#5781,.T.);
#31309=EDGE_CURVE('',#24313,#24311,#430,.T.);
#31310=EDGE_CURVE('',#24314,#24312,#431,.T.);
#31311=EDGE_CURVE('',#24314,#24315,#5782,.T.);
#31312=EDGE_CURVE('',#24315,#24313,#432,.T.);
#31313=EDGE_CURVE('',#24316,#24314,#433,.T.);
#31314=EDGE_CURVE('',#24316,#24317,#5783,.T.);
#31315=EDGE_CURVE('',#24317,#24315,#434,.T.);
#31316=EDGE_CURVE('',#24318,#24316,#435,.T.);
#31317=EDGE_CURVE('',#24318,#24319,#5784,.T.);
#31318=EDGE_CURVE('',#24319,#24317,#436,.T.);
#31319=EDGE_CURVE('',#24299,#24318,#437,.T.);
#31320=EDGE_CURVE('',#24301,#24319,#438,.T.);
#31321=EDGE_CURVE('',#24320,#24321,#5785,.T.);
#31322=EDGE_CURVE('',#24320,#24322,#5786,.T.);
#31323=EDGE_CURVE('',#24322,#24323,#5787,.T.);
#31324=EDGE_CURVE('',#24321,#24323,#5788,.T.);
#31325=EDGE_CURVE('',#24324,#24320,#5789,.T.);
#31326=EDGE_CURVE('',#24324,#24325,#5790,.T.);
#31327=EDGE_CURVE('',#24325,#24322,#5791,.T.);
#31328=EDGE_CURVE('',#24326,#24324,#5792,.T.);
#31329=EDGE_CURVE('',#24326,#24327,#5793,.T.);
#31330=EDGE_CURVE('',#24327,#24325,#5794,.T.);
#31331=EDGE_CURVE('',#24328,#24326,#5795,.T.);
#31332=EDGE_CURVE('',#24328,#24329,#5796,.T.);
#31333=EDGE_CURVE('',#24329,#24327,#5797,.T.);
#31334=EDGE_CURVE('',#24330,#24328,#5798,.T.);
#31335=EDGE_CURVE('',#24330,#24331,#5799,.T.);
#31336=EDGE_CURVE('',#24331,#24329,#5800,.T.);
#31337=EDGE_CURVE('',#24332,#24330,#5801,.T.);
#31338=EDGE_CURVE('',#24332,#24333,#5802,.T.);
#31339=EDGE_CURVE('',#24333,#24331,#5803,.T.);
#31340=EDGE_CURVE('',#24334,#24332,#5804,.T.);
#31341=EDGE_CURVE('',#24334,#24335,#5805,.T.);
#31342=EDGE_CURVE('',#24335,#24333,#5806,.T.);
#31343=EDGE_CURVE('',#24336,#24334,#5807,.T.);
#31344=EDGE_CURVE('',#24336,#24337,#5808,.T.);
#31345=EDGE_CURVE('',#24337,#24335,#5809,.T.);
#31346=EDGE_CURVE('',#24338,#24336,#5810,.T.);
#31347=EDGE_CURVE('',#24338,#24339,#5811,.T.);
#31348=EDGE_CURVE('',#24339,#24337,#5812,.T.);
#31349=EDGE_CURVE('',#24340,#24338,#5813,.T.);
#31350=EDGE_CURVE('',#24340,#24341,#5814,.T.);
#31351=EDGE_CURVE('',#24341,#24339,#5815,.T.);
#31352=EDGE_CURVE('',#24342,#24340,#5816,.T.);
#31353=EDGE_CURVE('',#24342,#24343,#5817,.T.);
#31354=EDGE_CURVE('',#24343,#24341,#5818,.T.);
#31355=EDGE_CURVE('',#24321,#24342,#5819,.T.);
#31356=EDGE_CURVE('',#24323,#24343,#5820,.T.);
#31357=EDGE_CURVE('',#24344,#24345,#5821,.T.);
#31358=EDGE_CURVE('',#24344,#24346,#5822,.T.);
#31359=EDGE_CURVE('',#24346,#24347,#5823,.T.);
#31360=EDGE_CURVE('',#24345,#24347,#5824,.T.);
#31361=EDGE_CURVE('',#24348,#24344,#5825,.T.);
#31362=EDGE_CURVE('',#24348,#24349,#5826,.T.);
#31363=EDGE_CURVE('',#24349,#24346,#5827,.T.);
#31364=EDGE_CURVE('',#24350,#24348,#5828,.T.);
#31365=EDGE_CURVE('',#24350,#24351,#5829,.T.);
#31366=EDGE_CURVE('',#24351,#24349,#5830,.T.);
#31367=EDGE_CURVE('',#24352,#24350,#5831,.T.);
#31368=EDGE_CURVE('',#24352,#24353,#5832,.T.);
#31369=EDGE_CURVE('',#24353,#24351,#5833,.T.);
#31370=EDGE_CURVE('',#24354,#24352,#5834,.T.);
#31371=EDGE_CURVE('',#24354,#24355,#5835,.T.);
#31372=EDGE_CURVE('',#24355,#24353,#5836,.T.);
#31373=EDGE_CURVE('',#24345,#24354,#5837,.T.);
#31374=EDGE_CURVE('',#24347,#24355,#5838,.T.);
#31375=EDGE_CURVE('',#24356,#24357,#439,.T.);
#31376=EDGE_CURVE('',#24356,#24358,#5839,.T.);
#31377=EDGE_CURVE('',#24358,#24359,#440,.T.);
#31378=EDGE_CURVE('',#24357,#24359,#5840,.T.);
#31379=EDGE_CURVE('',#24360,#24356,#441,.T.);
#31380=EDGE_CURVE('',#24360,#24361,#5841,.T.);
#31381=EDGE_CURVE('',#24361,#24358,#442,.T.);
#31382=EDGE_CURVE('',#24362,#24360,#443,.T.);
#31383=EDGE_CURVE('',#24362,#24363,#5842,.T.);
#31384=EDGE_CURVE('',#24363,#24361,#444,.T.);
#31385=EDGE_CURVE('',#24364,#24362,#445,.T.);
#31386=EDGE_CURVE('',#24364,#24365,#5843,.T.);
#31387=EDGE_CURVE('',#24365,#24363,#446,.T.);
#31388=EDGE_CURVE('',#24366,#24364,#447,.T.);
#31389=EDGE_CURVE('',#24366,#24367,#5844,.T.);
#31390=EDGE_CURVE('',#24367,#24365,#448,.T.);
#31391=EDGE_CURVE('',#24368,#24366,#449,.T.);
#31392=EDGE_CURVE('',#24368,#24369,#5845,.T.);
#31393=EDGE_CURVE('',#24369,#24367,#450,.T.);
#31394=EDGE_CURVE('',#24370,#24368,#451,.T.);
#31395=EDGE_CURVE('',#24370,#24371,#5846,.T.);
#31396=EDGE_CURVE('',#24371,#24369,#452,.T.);
#31397=EDGE_CURVE('',#24372,#24370,#453,.T.);
#31398=EDGE_CURVE('',#24372,#24373,#5847,.T.);
#31399=EDGE_CURVE('',#24373,#24371,#454,.T.);
#31400=EDGE_CURVE('',#24374,#24372,#5848,.T.);
#31401=EDGE_CURVE('',#24374,#24375,#5849,.T.);
#31402=EDGE_CURVE('',#24375,#24373,#5850,.T.);
#31403=EDGE_CURVE('',#24376,#24374,#5851,.T.);
#31404=EDGE_CURVE('',#24376,#24377,#5852,.T.);
#31405=EDGE_CURVE('',#24377,#24375,#5853,.T.);
#31406=EDGE_CURVE('',#24378,#24376,#5854,.T.);
#31407=EDGE_CURVE('',#24378,#24379,#5855,.T.);
#31408=EDGE_CURVE('',#24379,#24377,#5856,.T.);
#31409=EDGE_CURVE('',#24357,#24378,#455,.T.);
#31410=EDGE_CURVE('',#24359,#24379,#456,.T.);
#31411=EDGE_CURVE('',#24380,#24381,#5857,.T.);
#31412=EDGE_CURVE('',#24380,#24382,#5858,.T.);
#31413=EDGE_CURVE('',#24382,#24383,#5859,.T.);
#31414=EDGE_CURVE('',#24381,#24383,#5860,.T.);
#31415=EDGE_CURVE('',#24384,#24380,#457,.T.);
#31416=EDGE_CURVE('',#24384,#24385,#5861,.T.);
#31417=EDGE_CURVE('',#24385,#24382,#458,.T.);
#31418=EDGE_CURVE('',#24386,#24384,#459,.T.);
#31419=EDGE_CURVE('',#24386,#24387,#5862,.T.);
#31420=EDGE_CURVE('',#24387,#24385,#460,.T.);
#31421=EDGE_CURVE('',#24388,#24386,#461,.T.);
#31422=EDGE_CURVE('',#24388,#24389,#5863,.T.);
#31423=EDGE_CURVE('',#24389,#24387,#462,.T.);
#31424=EDGE_CURVE('',#24390,#24388,#463,.T.);
#31425=EDGE_CURVE('',#24390,#24391,#5864,.T.);
#31426=EDGE_CURVE('',#24391,#24389,#464,.T.);
#31427=EDGE_CURVE('',#24392,#24390,#5865,.T.);
#31428=EDGE_CURVE('',#24392,#24393,#5866,.T.);
#31429=EDGE_CURVE('',#24393,#24391,#5867,.T.);
#31430=EDGE_CURVE('',#24394,#24392,#5868,.T.);
#31431=EDGE_CURVE('',#24394,#24395,#5869,.T.);
#31432=EDGE_CURVE('',#24395,#24393,#5870,.T.);
#31433=EDGE_CURVE('',#24396,#24394,#5871,.T.);
#31434=EDGE_CURVE('',#24396,#24397,#5872,.T.);
#31435=EDGE_CURVE('',#24397,#24395,#5873,.T.);
#31436=EDGE_CURVE('',#24398,#24396,#465,.T.);
#31437=EDGE_CURVE('',#24398,#24399,#5874,.T.);
#31438=EDGE_CURVE('',#24399,#24397,#466,.T.);
#31439=EDGE_CURVE('',#24400,#24398,#467,.T.);
#31440=EDGE_CURVE('',#24400,#24401,#5875,.T.);
#31441=EDGE_CURVE('',#24401,#24399,#468,.T.);
#31442=EDGE_CURVE('',#24402,#24400,#469,.T.);
#31443=EDGE_CURVE('',#24402,#24403,#5876,.T.);
#31444=EDGE_CURVE('',#24403,#24401,#470,.T.);
#31445=EDGE_CURVE('',#24404,#24402,#471,.T.);
#31446=EDGE_CURVE('',#24404,#24405,#5877,.T.);
#31447=EDGE_CURVE('',#24405,#24403,#472,.T.);
#31448=EDGE_CURVE('',#24406,#24404,#473,.T.);
#31449=EDGE_CURVE('',#24406,#24407,#5878,.T.);
#31450=EDGE_CURVE('',#24407,#24405,#474,.T.);
#31451=EDGE_CURVE('',#24408,#24406,#475,.T.);
#31452=EDGE_CURVE('',#24408,#24409,#5879,.T.);
#31453=EDGE_CURVE('',#24409,#24407,#476,.T.);
#31454=EDGE_CURVE('',#24410,#24408,#477,.T.);
#31455=EDGE_CURVE('',#24410,#24411,#5880,.T.);
#31456=EDGE_CURVE('',#24411,#24409,#478,.T.);
#31457=EDGE_CURVE('',#24412,#24410,#5881,.T.);
#31458=EDGE_CURVE('',#24412,#24413,#5882,.T.);
#31459=EDGE_CURVE('',#24413,#24411,#5883,.T.);
#31460=EDGE_CURVE('',#24414,#24412,#5884,.T.);
#31461=EDGE_CURVE('',#24414,#24415,#5885,.T.);
#31462=EDGE_CURVE('',#24415,#24413,#5886,.T.);
#31463=EDGE_CURVE('',#24416,#24414,#5887,.T.);
#31464=EDGE_CURVE('',#24416,#24417,#5888,.T.);
#31465=EDGE_CURVE('',#24417,#24415,#5889,.T.);
#31466=EDGE_CURVE('',#24381,#24416,#5890,.T.);
#31467=EDGE_CURVE('',#24383,#24417,#5891,.T.);
#31468=EDGE_CURVE('',#24418,#24419,#5892,.T.);
#31469=EDGE_CURVE('',#24420,#24418,#5893,.T.);
#31470=EDGE_CURVE('',#24421,#24420,#5894,.T.);
#31471=EDGE_CURVE('',#24421,#24419,#5895,.T.);
#31472=EDGE_CURVE('',#24419,#24422,#5896,.T.);
#31473=EDGE_CURVE('',#24423,#24421,#5897,.T.);
#31474=EDGE_CURVE('',#24423,#24422,#5898,.T.);
#31475=EDGE_CURVE('',#24422,#24424,#5899,.T.);
#31476=EDGE_CURVE('',#24425,#24423,#5900,.T.);
#31477=EDGE_CURVE('',#24425,#24424,#5901,.T.);
#31478=EDGE_CURVE('',#24424,#24418,#5902,.T.);
#31479=EDGE_CURVE('',#24420,#24425,#5903,.T.);
#31480=EDGE_CURVE('',#24426,#24426,#19951,.T.);
#31481=EDGE_CURVE('',#24426,#24427,#5904,.T.);
#31482=EDGE_CURVE('',#24427,#24427,#19952,.T.);
#31483=EDGE_CURVE('',#24428,#24428,#19953,.T.);
#31484=EDGE_CURVE('',#24428,#24427,#5905,.T.);
#31485=EDGE_CURVE('',#24429,#24430,#5906,.T.);
#31486=EDGE_CURVE('',#24431,#24429,#19954,.T.);
#31487=EDGE_CURVE('',#24432,#24431,#5907,.T.);
#31488=EDGE_CURVE('',#24433,#24432,#19955,.T.);
#31489=EDGE_CURVE('',#24434,#24433,#5908,.T.);
#31490=EDGE_CURVE('',#24435,#24434,#19956,.T.);
#31491=EDGE_CURVE('',#24436,#24435,#5909,.T.);
#31492=EDGE_CURVE('',#24430,#24436,#19957,.T.);
#31493=EDGE_CURVE('',#24437,#24437,#19958,.T.);
#31494=EDGE_CURVE('',#24438,#24438,#19959,.T.);
#31495=EDGE_CURVE('',#24439,#24439,#19960,.T.);
#31496=EDGE_CURVE('',#24440,#24440,#19961,.T.);
#31497=EDGE_CURVE('',#24441,#24441,#19962,.T.);
#31498=EDGE_CURVE('',#24442,#24442,#19963,.T.);
#31499=EDGE_CURVE('',#24443,#24443,#19964,.T.);
#31500=EDGE_CURVE('',#24444,#24444,#19965,.T.);
#31501=EDGE_CURVE('',#24445,#24445,#19966,.T.);
#31502=EDGE_CURVE('',#24446,#24446,#19967,.T.);
#31503=EDGE_CURVE('',#24447,#24447,#19968,.T.);
#31504=EDGE_CURVE('',#24447,#24428,#5910,.T.);
#31505=EDGE_CURVE('',#24448,#24449,#19969,.T.);
#31506=EDGE_CURVE('',#24450,#24448,#5911,.T.);
#31507=EDGE_CURVE('',#24451,#24450,#19970,.T.);
#31508=EDGE_CURVE('',#24452,#24451,#5912,.T.);
#31509=EDGE_CURVE('',#24453,#24452,#19971,.T.);
#31510=EDGE_CURVE('',#24454,#24453,#5913,.T.);
#31511=EDGE_CURVE('',#24455,#24454,#19972,.T.);
#31512=EDGE_CURVE('',#24449,#24455,#5914,.T.);
#31513=EDGE_CURVE('',#24456,#24456,#19973,.T.);
#31514=EDGE_CURVE('',#24457,#24457,#19974,.T.);
#31515=EDGE_CURVE('',#24458,#24458,#19975,.T.);
#31516=EDGE_CURVE('',#24446,#24459,#5915,.T.);
#31517=EDGE_CURVE('',#24459,#24459,#19976,.T.);
#31518=EDGE_CURVE('',#24460,#24460,#19977,.T.);
#31519=EDGE_CURVE('',#24460,#24459,#5916,.T.);
#31520=EDGE_CURVE('',#24456,#24460,#5917,.T.);
#31521=EDGE_CURVE('',#24437,#24461,#5918,.T.);
#31522=EDGE_CURVE('',#24461,#24461,#19978,.T.);
#31523=EDGE_CURVE('',#24462,#24462,#19979,.T.);
#31524=EDGE_CURVE('',#24462,#24461,#5919,.T.);
#31525=EDGE_CURVE('',#24458,#24462,#5920,.T.);
#31526=EDGE_CURVE('',#24445,#24463,#5921,.T.);
#31527=EDGE_CURVE('',#24463,#24463,#19980,.T.);
#31528=EDGE_CURVE('',#24464,#24464,#19981,.T.);
#31529=EDGE_CURVE('',#24464,#24463,#5922,.T.);
#31530=EDGE_CURVE('',#24457,#24464,#5923,.T.);
#31531=EDGE_CURVE('',#24465,#24465,#19982,.T.);
#31532=EDGE_CURVE('',#24465,#24466,#5924,.T.);
#31533=EDGE_CURVE('',#24444,#24465,#5925,.T.);
#31534=EDGE_CURVE('',#24467,#24467,#19983,.T.);
#31535=EDGE_CURVE('',#24467,#24468,#5926,.T.);
#31536=EDGE_CURVE('',#24443,#24467,#5927,.T.);
#31537=EDGE_CURVE('',#24469,#24469,#19984,.T.);
#31538=EDGE_CURVE('',#24469,#24470,#5928,.T.);
#31539=EDGE_CURVE('',#24438,#24471,#5929,.T.);
#31540=EDGE_CURVE('',#24471,#24471,#19985,.T.);
#31541=EDGE_CURVE('',#24471,#24469,#5930,.T.);
#31542=EDGE_CURVE('',#24472,#24472,#19986,.T.);
#31543=EDGE_CURVE('',#24472,#24473,#5931,.T.);
#31544=EDGE_CURVE('',#24439,#24474,#5932,.T.);
#31545=EDGE_CURVE('',#24474,#24474,#19987,.T.);
#31546=EDGE_CURVE('',#24474,#24472,#5933,.T.);
#31547=EDGE_CURVE('',#24475,#24475,#19988,.T.);
#31548=EDGE_CURVE('',#24475,#24476,#5934,.T.);
#31549=EDGE_CURVE('',#24440,#24477,#5935,.T.);
#31550=EDGE_CURVE('',#24477,#24477,#19989,.T.);
#31551=EDGE_CURVE('',#24477,#24475,#5936,.T.);
#31552=EDGE_CURVE('',#24478,#24478,#19990,.T.);
#31553=EDGE_CURVE('',#24478,#24479,#5937,.T.);
#31554=EDGE_CURVE('',#24441,#24480,#5938,.T.);
#31555=EDGE_CURVE('',#24480,#24480,#19991,.T.);
#31556=EDGE_CURVE('',#24480,#24478,#5939,.T.);
#31557=EDGE_CURVE('',#24481,#24481,#19992,.T.);
#31558=EDGE_CURVE('',#24481,#24442,#5940,.T.);
#31559=EDGE_CURVE('',#24449,#24482,#5941,.T.);
#31560=EDGE_CURVE('',#24482,#24483,#19993,.T.);
#31561=EDGE_CURVE('',#24483,#24448,#5942,.T.);
#31562=EDGE_CURVE('',#24455,#24484,#5943,.T.);
#31563=EDGE_CURVE('',#24484,#24482,#5944,.T.);
#31564=EDGE_CURVE('',#24454,#24485,#5945,.T.);
#31565=EDGE_CURVE('',#24485,#24484,#19994,.T.);
#31566=EDGE_CURVE('',#24453,#24486,#5946,.T.);
#31567=EDGE_CURVE('',#24486,#24485,#5947,.T.);
#31568=EDGE_CURVE('',#24452,#24487,#5948,.T.);
#31569=EDGE_CURVE('',#24487,#24486,#19995,.T.);
#31570=EDGE_CURVE('',#24451,#24488,#5949,.T.);
#31571=EDGE_CURVE('',#24488,#24487,#5950,.T.);
#31572=EDGE_CURVE('',#24450,#24489,#5951,.T.);
#31573=EDGE_CURVE('',#24489,#24488,#19996,.T.);
#31574=EDGE_CURVE('',#24483,#24489,#5952,.T.);
#31575=EDGE_CURVE('',#24488,#24490,#5953,.T.);
#31576=EDGE_CURVE('',#24491,#24490,#5954,.T.);
#31577=EDGE_CURVE('',#24487,#24491,#5955,.T.);
#31578=EDGE_CURVE('',#24489,#24492,#5956,.T.);
#31579=EDGE_CURVE('',#24490,#24492,#19997,.T.);
#31580=EDGE_CURVE('',#24483,#24493,#5957,.T.);
#31581=EDGE_CURVE('',#24492,#24493,#5958,.T.);
#31582=EDGE_CURVE('',#24482,#24494,#5959,.T.);
#31583=EDGE_CURVE('',#24493,#24494,#19998,.T.);
#31584=EDGE_CURVE('',#24490,#24429,#5960,.T.);
#31585=EDGE_CURVE('',#24430,#24491,#5961,.T.);
#31586=EDGE_CURVE('',#24492,#24431,#5962,.T.);
#31587=EDGE_CURVE('',#24493,#24432,#5963,.T.);
#31588=EDGE_CURVE('',#24494,#24433,#5964,.T.);
#31589=EDGE_CURVE('',#24495,#24434,#5965,.T.);
#31590=EDGE_CURVE('',#24494,#24495,#5966,.T.);
#31591=EDGE_CURVE('',#24496,#24435,#5967,.T.);
#31592=EDGE_CURVE('',#24495,#24496,#19999,.T.);
#31593=EDGE_CURVE('',#24497,#24436,#5968,.T.);
#31594=EDGE_CURVE('',#24496,#24497,#5969,.T.);
#31595=EDGE_CURVE('',#24497,#24491,#20000,.T.);
#31596=EDGE_CURVE('',#24486,#24497,#5970,.T.);
#31597=EDGE_CURVE('',#24485,#24496,#5971,.T.);
#31598=EDGE_CURVE('',#24484,#24495,#5972,.T.);
#31599=EDGE_CURVE('',#24498,#24498,#20001,.T.);
#31600=EDGE_CURVE('',#24498,#24499,#5973,.T.);
#31601=EDGE_CURVE('',#24499,#24499,#20002,.T.);
#31602=EDGE_CURVE('',#24499,#24500,#5974,.T.);
#31603=EDGE_CURVE('',#24500,#24500,#20003,.T.);
#31604=EDGE_CURVE('',#24501,#24501,#20004,.T.);
#31605=EDGE_CURVE('',#24502,#24502,#20005,.T.);
#31606=EDGE_CURVE('',#24502,#24501,#5975,.T.);
#31607=EDGE_CURVE('',#24503,#24503,#20006,.T.);
#31608=EDGE_CURVE('',#24503,#24502,#5976,.T.);
#31609=EDGE_CURVE('',#24504,#24504,#20007,.T.);
#31610=EDGE_CURVE('',#24504,#24503,#5977,.T.);
#31611=EDGE_CURVE('',#24505,#24505,#20008,.T.);
#31612=EDGE_CURVE('',#24505,#24498,#5978,.T.);
#31613=EDGE_CURVE('',#24506,#24507,#5979,.T.);
#31614=EDGE_CURVE('',#24506,#24508,#479,.T.);
#31615=EDGE_CURVE('',#24508,#24509,#20009,.T.);
#31616=EDGE_CURVE('',#24509,#24507,#480,.T.);
#31617=EDGE_CURVE('',#24510,#24511,#5980,.T.);
#31618=EDGE_CURVE('',#24510,#24506,#481,.T.);
#31619=EDGE_CURVE('',#24507,#24511,#482,.T.);
#31620=EDGE_CURVE('',#24512,#24513,#5981,.T.);
#31621=EDGE_CURVE('',#24512,#24510,#483,.T.);
#31622=EDGE_CURVE('',#24511,#24513,#484,.T.);
#31623=EDGE_CURVE('',#24514,#24515,#5982,.T.);
#31624=EDGE_CURVE('',#24514,#24512,#485,.T.);
#31625=EDGE_CURVE('',#24513,#24515,#486,.T.);
#31626=EDGE_CURVE('',#24516,#24517,#5983,.T.);
#31627=EDGE_CURVE('',#24516,#24514,#487,.T.);
#31628=EDGE_CURVE('',#24515,#24517,#488,.T.);
#31629=EDGE_CURVE('',#24518,#24519,#5984,.T.);
#31630=EDGE_CURVE('',#24518,#24516,#489,.T.);
#31631=EDGE_CURVE('',#24517,#24519,#490,.T.);
#31632=EDGE_CURVE('',#24520,#24521,#5985,.T.);
#31633=EDGE_CURVE('',#24520,#24518,#491,.T.);
#31634=EDGE_CURVE('',#24519,#24521,#492,.T.);
#31635=EDGE_CURVE('',#24522,#24523,#5986,.T.);
#31636=EDGE_CURVE('',#24522,#24520,#493,.T.);
#31637=EDGE_CURVE('',#24521,#24523,#494,.T.);
#31638=EDGE_CURVE('',#24524,#24525,#5987,.T.);
#31639=EDGE_CURVE('',#24524,#24522,#495,.T.);
#31640=EDGE_CURVE('',#24523,#24525,#496,.T.);
#31641=EDGE_CURVE('',#24526,#24527,#5988,.T.);
#31642=EDGE_CURVE('',#24526,#24524,#497,.T.);
#31643=EDGE_CURVE('',#24525,#24527,#498,.T.);
#31644=EDGE_CURVE('',#24528,#24529,#5989,.T.);
#31645=EDGE_CURVE('',#24528,#24526,#499,.T.);
#31646=EDGE_CURVE('',#24527,#24529,#500,.T.);
#31647=EDGE_CURVE('',#24530,#24531,#5990,.T.);
#31648=EDGE_CURVE('',#24530,#24528,#501,.T.);
#31649=EDGE_CURVE('',#24529,#24531,#502,.T.);
#31650=EDGE_CURVE('',#24532,#24533,#5991,.T.);
#31651=EDGE_CURVE('',#24532,#24530,#503,.T.);
#31652=EDGE_CURVE('',#24531,#24533,#504,.T.);
#31653=EDGE_CURVE('',#24534,#24535,#5992,.T.);
#31654=EDGE_CURVE('',#24534,#24532,#505,.T.);
#31655=EDGE_CURVE('',#24533,#24535,#506,.T.);
#31656=EDGE_CURVE('',#24536,#24537,#5993,.T.);
#31657=EDGE_CURVE('',#24536,#24534,#507,.T.);
#31658=EDGE_CURVE('',#24535,#24537,#508,.T.);
#31659=EDGE_CURVE('',#24538,#24539,#5994,.T.);
#31660=EDGE_CURVE('',#24538,#24536,#509,.T.);
#31661=EDGE_CURVE('',#24537,#24539,#510,.T.);
#31662=EDGE_CURVE('',#24540,#24541,#5995,.T.);
#31663=EDGE_CURVE('',#24540,#24542,#511,.T.);
#31664=EDGE_CURVE('',#24541,#24542,#20010,.T.);
#31665=EDGE_CURVE('',#24543,#24544,#5996,.T.);
#31666=EDGE_CURVE('',#24543,#24540,#512,.T.);
#31667=EDGE_CURVE('',#24545,#24541,#20011,.T.);
#31668=EDGE_CURVE('',#24544,#24545,#513,.T.);
#31669=EDGE_CURVE('',#24546,#24547,#5997,.T.);
#31670=EDGE_CURVE('',#24546,#24543,#514,.T.);
#31671=EDGE_CURVE('',#24547,#24544,#515,.T.);
#31672=EDGE_CURVE('',#24548,#24549,#5998,.T.);
#31673=EDGE_CURVE('',#24548,#24546,#516,.T.);
#31674=EDGE_CURVE('',#24549,#24547,#517,.T.);
#31675=EDGE_CURVE('',#24550,#24551,#5999,.T.);
#31676=EDGE_CURVE('',#24550,#24548,#518,.T.);
#31677=EDGE_CURVE('',#24551,#24549,#519,.T.);
#31678=EDGE_CURVE('',#24552,#24553,#6000,.T.);
#31679=EDGE_CURVE('',#24552,#24550,#520,.T.);
#31680=EDGE_CURVE('',#24553,#24551,#521,.T.);
#31681=EDGE_CURVE('',#24554,#24555,#6001,.T.);
#31682=EDGE_CURVE('',#24554,#24552,#522,.T.);
#31683=EDGE_CURVE('',#24555,#24553,#523,.T.);
#31684=EDGE_CURVE('',#24556,#24557,#6002,.T.);
#31685=EDGE_CURVE('',#24556,#24554,#524,.T.);
#31686=EDGE_CURVE('',#24557,#24555,#525,.T.);
#31687=EDGE_CURVE('',#24558,#24559,#6003,.T.);
#31688=EDGE_CURVE('',#24558,#24556,#526,.T.);
#31689=EDGE_CURVE('',#24559,#24557,#527,.T.);
#31690=EDGE_CURVE('',#24560,#24561,#6004,.T.);
#31691=EDGE_CURVE('',#24560,#24558,#528,.T.);
#31692=EDGE_CURVE('',#24561,#24559,#529,.T.);
#31693=EDGE_CURVE('',#24562,#24563,#6005,.T.);
#31694=EDGE_CURVE('',#24562,#24560,#530,.T.);
#31695=EDGE_CURVE('',#24563,#24561,#531,.T.);
#31696=EDGE_CURVE('',#24564,#24565,#6006,.T.);
#31697=EDGE_CURVE('',#24564,#24562,#532,.T.);
#31698=EDGE_CURVE('',#24565,#24563,#533,.T.);
#31699=EDGE_CURVE('',#24566,#24567,#6007,.T.);
#31700=EDGE_CURVE('',#24566,#24564,#534,.T.);
#31701=EDGE_CURVE('',#24567,#24565,#535,.T.);
#31702=EDGE_CURVE('',#24568,#24569,#6008,.T.);
#31703=EDGE_CURVE('',#24568,#24566,#536,.T.);
#31704=EDGE_CURVE('',#24569,#24567,#537,.T.);
#31705=EDGE_CURVE('',#24570,#24571,#6009,.T.);
#31706=EDGE_CURVE('',#24570,#24568,#538,.T.);
#31707=EDGE_CURVE('',#24571,#24569,#539,.T.);
#31708=EDGE_CURVE('',#24572,#24573,#6010,.T.);
#31709=EDGE_CURVE('',#24572,#24570,#540,.T.);
#31710=EDGE_CURVE('',#24573,#24571,#541,.T.);
#31711=EDGE_CURVE('',#24542,#24574,#542,.T.);
#31712=EDGE_CURVE('',#24575,#24574,#20012,.T.);
#31713=EDGE_CURVE('',#24576,#24575,#20013,.T.);
#31714=EDGE_CURVE('',#24576,#24545,#543,.T.);
#31715=EDGE_CURVE('',#24539,#24576,#544,.T.);
#31716=EDGE_CURVE('',#24577,#24509,#545,.T.);
#31717=EDGE_CURVE('',#24577,#24573,#546,.T.);
#31718=EDGE_CURVE('',#24509,#24578,#20014,.T.);
#31719=EDGE_CURVE('',#24578,#24508,#20015,.T.);
#31720=EDGE_CURVE('',#24508,#24579,#547,.T.);
#31721=EDGE_CURVE('',#24579,#24577,#20016,.T.);
#31722=EDGE_CURVE('',#24579,#24572,#548,.T.);
#31723=EDGE_CURVE('',#24574,#24538,#549,.T.);
#31724=EDGE_CURVE('',#24575,#24580,#20017,.T.);
#31725=EDGE_CURVE('',#24580,#24580,#20018,.T.);
#31726=EDGE_CURVE('',#24574,#24576,#20019,.T.);
#31727=EDGE_CURVE('',#24581,#24581,#20020,.T.);
#31728=EDGE_CURVE('',#24582,#24583,#6011,.T.);
#31729=EDGE_CURVE('',#24582,#24584,#6012,.T.);
#31730=EDGE_CURVE('',#24584,#24585,#6013,.T.);
#31731=EDGE_CURVE('',#24585,#24583,#6014,.T.);
#31732=EDGE_CURVE('',#24583,#24586,#20021,.T.);
#31733=EDGE_CURVE('',#24586,#24585,#6015,.T.);
#31734=EDGE_CURVE('',#24586,#24587,#6016,.T.);
#31735=EDGE_CURVE('',#24584,#24587,#6017,.T.);
#31736=EDGE_CURVE('',#24587,#24582,#20022,.T.);
#31737=EDGE_CURVE('',#24588,#24589,#6018,.T.);
#31738=EDGE_CURVE('',#24588,#24590,#6019,.T.);
#31739=EDGE_CURVE('',#24590,#24591,#6020,.T.);
#31740=EDGE_CURVE('',#24591,#24589,#6021,.T.);
#31741=EDGE_CURVE('',#24589,#24592,#20023,.T.);
#31742=EDGE_CURVE('',#24592,#24591,#6022,.T.);
#31743=EDGE_CURVE('',#24592,#24593,#6023,.T.);
#31744=EDGE_CURVE('',#24590,#24593,#6024,.T.);
#31745=EDGE_CURVE('',#24593,#24588,#20024,.T.);
#31746=EDGE_CURVE('',#24594,#24595,#6025,.T.);
#31747=EDGE_CURVE('',#24594,#24596,#6026,.T.);
#31748=EDGE_CURVE('',#24596,#24597,#6027,.T.);
#31749=EDGE_CURVE('',#24597,#24595,#6028,.T.);
#31750=EDGE_CURVE('',#24595,#24598,#20025,.T.);
#31751=EDGE_CURVE('',#24598,#24597,#6029,.T.);
#31752=EDGE_CURVE('',#24598,#24599,#6030,.T.);
#31753=EDGE_CURVE('',#24596,#24599,#6031,.T.);
#31754=EDGE_CURVE('',#24599,#24594,#20026,.T.);
#31755=EDGE_CURVE('',#24600,#24601,#6032,.T.);
#31756=EDGE_CURVE('',#24600,#24602,#6033,.T.);
#31757=EDGE_CURVE('',#24602,#24603,#6034,.T.);
#31758=EDGE_CURVE('',#24603,#24601,#6035,.T.);
#31759=EDGE_CURVE('',#24601,#24604,#20027,.T.);
#31760=EDGE_CURVE('',#24604,#24603,#6036,.T.);
#31761=EDGE_CURVE('',#24604,#24605,#6037,.T.);
#31762=EDGE_CURVE('',#24602,#24605,#6038,.T.);
#31763=EDGE_CURVE('',#24605,#24600,#20028,.T.);
#31764=EDGE_CURVE('',#24606,#24607,#6039,.T.);
#31765=EDGE_CURVE('',#24606,#24608,#6040,.T.);
#31766=EDGE_CURVE('',#24608,#24609,#6041,.T.);
#31767=EDGE_CURVE('',#24609,#24607,#6042,.T.);
#31768=EDGE_CURVE('',#24607,#24610,#20029,.T.);
#31769=EDGE_CURVE('',#24610,#24609,#6043,.T.);
#31770=EDGE_CURVE('',#24610,#24611,#6044,.T.);
#31771=EDGE_CURVE('',#24608,#24611,#6045,.T.);
#31772=EDGE_CURVE('',#24611,#24606,#20030,.T.);
#31773=EDGE_CURVE('',#24612,#24613,#6046,.T.);
#31774=EDGE_CURVE('',#24612,#24614,#6047,.T.);
#31775=EDGE_CURVE('',#24614,#24615,#6048,.T.);
#31776=EDGE_CURVE('',#24615,#24613,#6049,.T.);
#31777=EDGE_CURVE('',#24613,#24616,#20031,.T.);
#31778=EDGE_CURVE('',#24616,#24615,#6050,.T.);
#31779=EDGE_CURVE('',#24616,#24617,#6051,.T.);
#31780=EDGE_CURVE('',#24614,#24617,#6052,.T.);
#31781=EDGE_CURVE('',#24617,#24612,#20032,.T.);
#31782=EDGE_CURVE('',#24618,#24619,#6053,.T.);
#31783=EDGE_CURVE('',#24618,#24620,#6054,.T.);
#31784=EDGE_CURVE('',#24620,#24621,#6055,.T.);
#31785=EDGE_CURVE('',#24621,#24619,#6056,.T.);
#31786=EDGE_CURVE('',#24619,#24622,#20033,.T.);
#31787=EDGE_CURVE('',#24622,#24621,#6057,.T.);
#31788=EDGE_CURVE('',#24622,#24623,#6058,.T.);
#31789=EDGE_CURVE('',#24620,#24623,#6059,.T.);
#31790=EDGE_CURVE('',#24623,#24618,#20034,.T.);
#31791=EDGE_CURVE('',#24624,#24625,#6060,.T.);
#31792=EDGE_CURVE('',#24624,#24626,#6061,.T.);
#31793=EDGE_CURVE('',#24626,#24627,#6062,.T.);
#31794=EDGE_CURVE('',#24627,#24625,#6063,.T.);
#31795=EDGE_CURVE('',#24625,#24628,#20035,.T.);
#31796=EDGE_CURVE('',#24628,#24627,#6064,.T.);
#31797=EDGE_CURVE('',#24628,#24629,#6065,.T.);
#31798=EDGE_CURVE('',#24626,#24629,#6066,.T.);
#31799=EDGE_CURVE('',#24629,#24624,#20036,.T.);
#31800=EDGE_CURVE('',#24630,#24631,#6067,.T.);
#31801=EDGE_CURVE('',#24630,#24632,#6068,.T.);
#31802=EDGE_CURVE('',#24632,#24633,#6069,.T.);
#31803=EDGE_CURVE('',#24633,#24631,#6070,.T.);
#31804=EDGE_CURVE('',#24631,#24634,#20037,.T.);
#31805=EDGE_CURVE('',#24634,#24633,#6071,.T.);
#31806=EDGE_CURVE('',#24634,#24635,#6072,.T.);
#31807=EDGE_CURVE('',#24632,#24635,#6073,.T.);
#31808=EDGE_CURVE('',#24635,#24630,#20038,.T.);
#31809=EDGE_CURVE('',#24636,#24637,#6074,.T.);
#31810=EDGE_CURVE('',#24636,#24638,#6075,.T.);
#31811=EDGE_CURVE('',#24638,#24639,#6076,.T.);
#31812=EDGE_CURVE('',#24639,#24637,#6077,.T.);
#31813=EDGE_CURVE('',#24637,#24640,#20039,.T.);
#31814=EDGE_CURVE('',#24640,#24639,#6078,.T.);
#31815=EDGE_CURVE('',#24640,#24641,#6079,.T.);
#31816=EDGE_CURVE('',#24638,#24641,#6080,.T.);
#31817=EDGE_CURVE('',#24641,#24636,#20040,.T.);
#31818=EDGE_CURVE('',#24642,#24643,#6081,.T.);
#31819=EDGE_CURVE('',#24642,#24644,#6082,.T.);
#31820=EDGE_CURVE('',#24644,#24645,#6083,.T.);
#31821=EDGE_CURVE('',#24645,#24643,#6084,.T.);
#31822=EDGE_CURVE('',#24643,#24646,#20041,.T.);
#31823=EDGE_CURVE('',#24646,#24645,#6085,.T.);
#31824=EDGE_CURVE('',#24646,#24647,#6086,.T.);
#31825=EDGE_CURVE('',#24644,#24647,#6087,.T.);
#31826=EDGE_CURVE('',#24647,#24642,#20042,.T.);
#31827=EDGE_CURVE('',#24648,#24649,#6088,.T.);
#31828=EDGE_CURVE('',#24648,#24650,#6089,.T.);
#31829=EDGE_CURVE('',#24650,#24651,#6090,.T.);
#31830=EDGE_CURVE('',#24651,#24649,#6091,.T.);
#31831=EDGE_CURVE('',#24649,#24652,#20043,.T.);
#31832=EDGE_CURVE('',#24652,#24651,#6092,.T.);
#31833=EDGE_CURVE('',#24652,#24653,#6093,.T.);
#31834=EDGE_CURVE('',#24650,#24653,#6094,.T.);
#31835=EDGE_CURVE('',#24653,#24648,#20044,.T.);
#31836=EDGE_CURVE('',#24654,#24655,#6095,.T.);
#31837=EDGE_CURVE('',#24654,#24656,#6096,.T.);
#31838=EDGE_CURVE('',#24656,#24657,#6097,.T.);
#31839=EDGE_CURVE('',#24657,#24655,#6098,.T.);
#31840=EDGE_CURVE('',#24655,#24658,#20045,.T.);
#31841=EDGE_CURVE('',#24658,#24657,#6099,.T.);
#31842=EDGE_CURVE('',#24658,#24659,#6100,.T.);
#31843=EDGE_CURVE('',#24656,#24659,#6101,.T.);
#31844=EDGE_CURVE('',#24659,#24654,#20046,.T.);
#31845=EDGE_CURVE('',#24660,#24661,#6102,.T.);
#31846=EDGE_CURVE('',#24660,#24662,#6103,.T.);
#31847=EDGE_CURVE('',#24662,#24663,#6104,.T.);
#31848=EDGE_CURVE('',#24663,#24661,#6105,.T.);
#31849=EDGE_CURVE('',#24661,#24664,#20047,.T.);
#31850=EDGE_CURVE('',#24664,#24663,#6106,.T.);
#31851=EDGE_CURVE('',#24664,#24665,#6107,.T.);
#31852=EDGE_CURVE('',#24662,#24665,#6108,.T.);
#31853=EDGE_CURVE('',#24665,#24660,#20048,.T.);
#31854=EDGE_CURVE('',#24666,#24667,#6109,.T.);
#31855=EDGE_CURVE('',#24666,#24668,#6110,.T.);
#31856=EDGE_CURVE('',#24668,#24669,#6111,.T.);
#31857=EDGE_CURVE('',#24669,#24667,#6112,.T.);
#31858=EDGE_CURVE('',#24667,#24670,#20049,.T.);
#31859=EDGE_CURVE('',#24670,#24669,#6113,.T.);
#31860=EDGE_CURVE('',#24670,#24671,#6114,.T.);
#31861=EDGE_CURVE('',#24668,#24671,#6115,.T.);
#31862=EDGE_CURVE('',#24671,#24666,#20050,.T.);
#31863=EDGE_CURVE('',#24672,#24673,#6116,.T.);
#31864=EDGE_CURVE('',#24672,#24674,#6117,.T.);
#31865=EDGE_CURVE('',#24674,#24675,#6118,.T.);
#31866=EDGE_CURVE('',#24675,#24673,#6119,.T.);
#31867=EDGE_CURVE('',#24673,#24676,#20051,.T.);
#31868=EDGE_CURVE('',#24676,#24675,#6120,.T.);
#31869=EDGE_CURVE('',#24676,#24677,#6121,.T.);
#31870=EDGE_CURVE('',#24674,#24677,#6122,.T.);
#31871=EDGE_CURVE('',#24677,#24672,#20052,.T.);
#31872=EDGE_CURVE('',#24678,#24679,#6123,.T.);
#31873=EDGE_CURVE('',#24678,#24680,#6124,.T.);
#31874=EDGE_CURVE('',#24680,#24681,#6125,.T.);
#31875=EDGE_CURVE('',#24681,#24679,#6126,.T.);
#31876=EDGE_CURVE('',#24679,#24682,#20053,.T.);
#31877=EDGE_CURVE('',#24682,#24681,#6127,.T.);
#31878=EDGE_CURVE('',#24682,#24683,#6128,.T.);
#31879=EDGE_CURVE('',#24680,#24683,#6129,.T.);
#31880=EDGE_CURVE('',#24683,#24678,#20054,.T.);
#31881=EDGE_CURVE('',#24684,#24685,#6130,.T.);
#31882=EDGE_CURVE('',#24684,#24686,#6131,.T.);
#31883=EDGE_CURVE('',#24686,#24687,#6132,.T.);
#31884=EDGE_CURVE('',#24687,#24685,#6133,.T.);
#31885=EDGE_CURVE('',#24685,#24688,#20055,.T.);
#31886=EDGE_CURVE('',#24689,#24687,#6134,.T.);
#31887=EDGE_CURVE('',#24688,#24689,#20056,.T.);
#31888=EDGE_CURVE('',#24689,#24690,#6135,.T.);
#31889=EDGE_CURVE('',#24686,#24690,#6136,.T.);
#31890=EDGE_CURVE('',#24690,#24691,#20057,.T.);
#31891=EDGE_CURVE('',#24691,#24684,#20058,.T.);
#31892=EDGE_CURVE('',#24692,#24693,#6137,.T.);
#31893=EDGE_CURVE('',#24692,#24694,#6138,.T.);
#31894=EDGE_CURVE('',#24694,#24695,#6139,.T.);
#31895=EDGE_CURVE('',#24695,#24693,#6140,.T.);
#31896=EDGE_CURVE('',#24693,#24696,#20059,.T.);
#31897=EDGE_CURVE('',#24696,#24695,#6141,.T.);
#31898=EDGE_CURVE('',#24696,#24697,#6142,.T.);
#31899=EDGE_CURVE('',#24694,#24697,#6143,.T.);
#31900=EDGE_CURVE('',#24697,#24692,#20060,.T.);
#31901=EDGE_CURVE('',#24698,#24699,#6144,.T.);
#31902=EDGE_CURVE('',#24698,#24700,#6145,.T.);
#31903=EDGE_CURVE('',#24700,#24701,#6146,.T.);
#31904=EDGE_CURVE('',#24701,#24699,#6147,.T.);
#31905=EDGE_CURVE('',#24699,#24702,#20061,.T.);
#31906=EDGE_CURVE('',#24702,#24701,#6148,.T.);
#31907=EDGE_CURVE('',#24702,#24703,#6149,.T.);
#31908=EDGE_CURVE('',#24700,#24703,#6150,.T.);
#31909=EDGE_CURVE('',#24703,#24698,#20062,.T.);
#31910=EDGE_CURVE('',#24704,#24705,#6151,.T.);
#31911=EDGE_CURVE('',#24704,#24706,#6152,.T.);
#31912=EDGE_CURVE('',#24706,#24707,#6153,.T.);
#31913=EDGE_CURVE('',#24707,#24705,#6154,.T.);
#31914=EDGE_CURVE('',#24705,#24708,#20063,.T.);
#31915=EDGE_CURVE('',#24708,#24707,#6155,.T.);
#31916=EDGE_CURVE('',#24708,#24709,#6156,.T.);
#31917=EDGE_CURVE('',#24706,#24709,#6157,.T.);
#31918=EDGE_CURVE('',#24709,#24704,#20064,.T.);
#31919=EDGE_CURVE('',#24710,#24711,#6158,.T.);
#31920=EDGE_CURVE('',#24710,#24712,#6159,.T.);
#31921=EDGE_CURVE('',#24712,#24713,#6160,.T.);
#31922=EDGE_CURVE('',#24713,#24711,#6161,.T.);
#31923=EDGE_CURVE('',#24711,#24714,#20065,.T.);
#31924=EDGE_CURVE('',#24714,#24713,#6162,.T.);
#31925=EDGE_CURVE('',#24714,#24715,#6163,.T.);
#31926=EDGE_CURVE('',#24712,#24715,#6164,.T.);
#31927=EDGE_CURVE('',#24715,#24710,#20066,.T.);
#31928=EDGE_CURVE('',#24716,#24717,#6165,.T.);
#31929=EDGE_CURVE('',#24716,#24718,#6166,.T.);
#31930=EDGE_CURVE('',#24718,#24719,#6167,.T.);
#31931=EDGE_CURVE('',#24719,#24717,#6168,.T.);
#31932=EDGE_CURVE('',#24717,#24720,#20067,.T.);
#31933=EDGE_CURVE('',#24720,#24719,#6169,.T.);
#31934=EDGE_CURVE('',#24720,#24721,#6170,.T.);
#31935=EDGE_CURVE('',#24718,#24721,#6171,.T.);
#31936=EDGE_CURVE('',#24721,#24716,#20068,.T.);
#31937=EDGE_CURVE('',#24722,#24723,#6172,.T.);
#31938=EDGE_CURVE('',#24722,#24724,#6173,.T.);
#31939=EDGE_CURVE('',#24724,#24725,#6174,.T.);
#31940=EDGE_CURVE('',#24725,#24723,#6175,.T.);
#31941=EDGE_CURVE('',#24723,#24726,#20069,.T.);
#31942=EDGE_CURVE('',#24726,#24725,#6176,.T.);
#31943=EDGE_CURVE('',#24726,#24727,#6177,.T.);
#31944=EDGE_CURVE('',#24724,#24727,#6178,.T.);
#31945=EDGE_CURVE('',#24727,#24722,#20070,.T.);
#31946=EDGE_CURVE('',#24728,#24729,#6179,.T.);
#31947=EDGE_CURVE('',#24728,#24730,#6180,.T.);
#31948=EDGE_CURVE('',#24730,#24731,#6181,.T.);
#31949=EDGE_CURVE('',#24731,#24729,#6182,.T.);
#31950=EDGE_CURVE('',#24729,#24732,#20071,.T.);
#31951=EDGE_CURVE('',#24732,#24731,#6183,.T.);
#31952=EDGE_CURVE('',#24732,#24733,#6184,.T.);
#31953=EDGE_CURVE('',#24730,#24733,#6185,.T.);
#31954=EDGE_CURVE('',#24733,#24728,#20072,.T.);
#31955=EDGE_CURVE('',#24734,#24735,#6186,.T.);
#31956=EDGE_CURVE('',#24734,#24736,#6187,.T.);
#31957=EDGE_CURVE('',#24736,#24737,#6188,.T.);
#31958=EDGE_CURVE('',#24737,#24735,#6189,.T.);
#31959=EDGE_CURVE('',#24735,#24738,#20073,.T.);
#31960=EDGE_CURVE('',#24738,#24737,#6190,.T.);
#31961=EDGE_CURVE('',#24738,#24739,#6191,.T.);
#31962=EDGE_CURVE('',#24736,#24739,#6192,.T.);
#31963=EDGE_CURVE('',#24739,#24734,#20074,.T.);
#31964=EDGE_CURVE('',#24740,#24741,#6193,.T.);
#31965=EDGE_CURVE('',#24740,#24742,#6194,.T.);
#31966=EDGE_CURVE('',#24742,#24743,#6195,.T.);
#31967=EDGE_CURVE('',#24743,#24741,#6196,.T.);
#31968=EDGE_CURVE('',#24741,#24744,#20075,.T.);
#31969=EDGE_CURVE('',#24744,#24743,#6197,.T.);
#31970=EDGE_CURVE('',#24744,#24745,#6198,.T.);
#31971=EDGE_CURVE('',#24742,#24745,#6199,.T.);
#31972=EDGE_CURVE('',#24745,#24740,#20076,.T.);
#31973=EDGE_CURVE('',#24746,#24747,#6200,.T.);
#31974=EDGE_CURVE('',#24746,#24748,#6201,.T.);
#31975=EDGE_CURVE('',#24748,#24749,#6202,.T.);
#31976=EDGE_CURVE('',#24749,#24747,#6203,.T.);
#31977=EDGE_CURVE('',#24747,#24750,#20077,.T.);
#31978=EDGE_CURVE('',#24750,#24749,#6204,.T.);
#31979=EDGE_CURVE('',#24750,#24751,#6205,.T.);
#31980=EDGE_CURVE('',#24748,#24751,#6206,.T.);
#31981=EDGE_CURVE('',#24751,#24746,#20078,.T.);
#31982=EDGE_CURVE('',#24752,#24753,#6207,.T.);
#31983=EDGE_CURVE('',#24752,#24754,#6208,.T.);
#31984=EDGE_CURVE('',#24754,#24755,#6209,.T.);
#31985=EDGE_CURVE('',#24755,#24753,#6210,.T.);
#31986=EDGE_CURVE('',#24753,#24756,#20079,.T.);
#31987=EDGE_CURVE('',#24756,#24755,#6211,.T.);
#31988=EDGE_CURVE('',#24756,#24757,#6212,.T.);
#31989=EDGE_CURVE('',#24754,#24757,#6213,.T.);
#31990=EDGE_CURVE('',#24757,#24752,#20080,.T.);
#31991=EDGE_CURVE('',#24758,#24759,#6214,.T.);
#31992=EDGE_CURVE('',#24758,#24760,#6215,.T.);
#31993=EDGE_CURVE('',#24760,#24761,#6216,.T.);
#31994=EDGE_CURVE('',#24761,#24759,#6217,.T.);
#31995=EDGE_CURVE('',#24759,#24762,#20081,.T.);
#31996=EDGE_CURVE('',#24762,#24761,#6218,.T.);
#31997=EDGE_CURVE('',#24762,#24763,#6219,.T.);
#31998=EDGE_CURVE('',#24760,#24763,#6220,.T.);
#31999=EDGE_CURVE('',#24763,#24758,#20082,.T.);
#32000=EDGE_CURVE('',#24764,#24765,#6221,.T.);
#32001=EDGE_CURVE('',#24764,#24766,#6222,.T.);
#32002=EDGE_CURVE('',#24766,#24767,#6223,.T.);
#32003=EDGE_CURVE('',#24767,#24765,#6224,.T.);
#32004=EDGE_CURVE('',#24765,#24768,#20083,.T.);
#32005=EDGE_CURVE('',#24768,#24767,#6225,.T.);
#32006=EDGE_CURVE('',#24768,#24769,#6226,.T.);
#32007=EDGE_CURVE('',#24766,#24769,#6227,.T.);
#32008=EDGE_CURVE('',#24769,#24764,#20084,.T.);
#32009=EDGE_CURVE('',#24770,#24771,#6228,.T.);
#32010=EDGE_CURVE('',#24770,#24772,#6229,.T.);
#32011=EDGE_CURVE('',#24772,#24773,#6230,.T.);
#32012=EDGE_CURVE('',#24773,#24771,#6231,.T.);
#32013=EDGE_CURVE('',#24771,#24774,#20085,.T.);
#32014=EDGE_CURVE('',#24774,#24773,#6232,.T.);
#32015=EDGE_CURVE('',#24774,#24775,#6233,.T.);
#32016=EDGE_CURVE('',#24772,#24775,#6234,.T.);
#32017=EDGE_CURVE('',#24775,#24770,#20086,.T.);
#32018=EDGE_CURVE('',#24776,#24777,#6235,.T.);
#32019=EDGE_CURVE('',#24776,#24778,#6236,.T.);
#32020=EDGE_CURVE('',#24778,#24779,#6237,.T.);
#32021=EDGE_CURVE('',#24779,#24777,#6238,.T.);
#32022=EDGE_CURVE('',#24777,#24780,#20087,.T.);
#32023=EDGE_CURVE('',#24780,#24779,#6239,.T.);
#32024=EDGE_CURVE('',#24780,#24781,#6240,.T.);
#32025=EDGE_CURVE('',#24778,#24781,#6241,.T.);
#32026=EDGE_CURVE('',#24781,#24776,#20088,.T.);
#32027=EDGE_CURVE('',#24782,#24783,#6242,.T.);
#32028=EDGE_CURVE('',#24782,#24784,#6243,.T.);
#32029=EDGE_CURVE('',#24784,#24785,#6244,.T.);
#32030=EDGE_CURVE('',#24785,#24783,#6245,.T.);
#32031=EDGE_CURVE('',#24783,#24786,#20089,.T.);
#32032=EDGE_CURVE('',#24786,#24785,#6246,.T.);
#32033=EDGE_CURVE('',#24786,#24787,#6247,.T.);
#32034=EDGE_CURVE('',#24784,#24787,#6248,.T.);
#32035=EDGE_CURVE('',#24787,#24782,#20090,.T.);
#32036=EDGE_CURVE('',#24788,#24789,#6249,.T.);
#32037=EDGE_CURVE('',#24788,#24790,#6250,.T.);
#32038=EDGE_CURVE('',#24790,#24791,#6251,.T.);
#32039=EDGE_CURVE('',#24791,#24789,#6252,.T.);
#32040=EDGE_CURVE('',#24789,#24792,#20091,.T.);
#32041=EDGE_CURVE('',#24792,#24791,#6253,.T.);
#32042=EDGE_CURVE('',#24792,#24793,#6254,.T.);
#32043=EDGE_CURVE('',#24790,#24793,#6255,.T.);
#32044=EDGE_CURVE('',#24793,#24788,#20092,.T.);
#32045=EDGE_CURVE('',#24794,#24795,#20093,.T.);
#32046=EDGE_CURVE('',#24796,#24794,#6256,.T.);
#32047=EDGE_CURVE('',#24795,#24796,#6257,.T.);
#32048=EDGE_CURVE('',#24797,#24794,#6258,.T.);
#32049=EDGE_CURVE('',#24797,#24798,#6259,.T.);
#32050=EDGE_CURVE('',#24798,#24796,#6260,.T.);
#32051=EDGE_CURVE('',#24795,#24799,#6261,.T.);
#32052=EDGE_CURVE('',#24798,#24799,#6262,.T.);
#32053=EDGE_CURVE('',#24799,#24797,#20094,.T.);
#32054=EDGE_CURVE('',#24800,#24801,#6263,.T.);
#32055=EDGE_CURVE('',#24801,#24801,#20095,.T.);
#32056=EDGE_CURVE('',#24802,#24803,#6264,.T.);
#32057=EDGE_CURVE('',#24804,#24802,#6265,.T.);
#32058=EDGE_CURVE('',#24805,#24804,#6266,.T.);
#32059=EDGE_CURVE('',#24805,#24803,#6267,.T.);
#32060=EDGE_CURVE('',#24803,#24806,#6268,.T.);
#32061=EDGE_CURVE('',#24807,#24805,#6269,.T.);
#32062=EDGE_CURVE('',#24807,#24806,#6270,.T.);
#32063=EDGE_CURVE('',#24806,#24808,#6271,.T.);
#32064=EDGE_CURVE('',#24809,#24807,#6272,.T.);
#32065=EDGE_CURVE('',#24809,#24808,#6273,.T.);
#32066=EDGE_CURVE('',#24808,#24810,#6274,.T.);
#32067=EDGE_CURVE('',#24811,#24809,#6275,.T.);
#32068=EDGE_CURVE('',#24811,#24810,#6276,.T.);
#32069=EDGE_CURVE('',#24810,#24812,#6277,.T.);
#32070=EDGE_CURVE('',#24813,#24811,#6278,.T.);
#32071=EDGE_CURVE('',#24813,#24812,#6279,.T.);
#32072=EDGE_CURVE('',#24812,#24802,#6280,.T.);
#32073=EDGE_CURVE('',#24804,#24813,#6281,.T.);
#32074=EDGE_CURVE('',#24814,#24814,#20096,.T.);
#32075=EDGE_CURVE('',#24578,#24814,#6282,.T.);
#32076=EDGE_CURVE('',#24592,#24583,#20097,.T.);
#32077=EDGE_CURVE('',#24598,#24589,#20098,.T.);
#32078=EDGE_CURVE('',#24604,#24595,#20099,.T.);
#32079=EDGE_CURVE('',#24610,#24601,#20100,.T.);
#32080=EDGE_CURVE('',#24616,#24607,#20101,.T.);
#32081=EDGE_CURVE('',#24622,#24613,#20102,.T.);
#32082=EDGE_CURVE('',#24628,#24619,#20103,.T.);
#32083=EDGE_CURVE('',#24634,#24625,#20104,.T.);
#32084=EDGE_CURVE('',#24640,#24631,#20105,.T.);
#32085=EDGE_CURVE('',#24646,#24637,#20106,.T.);
#32086=EDGE_CURVE('',#24652,#24643,#20107,.T.);
#32087=EDGE_CURVE('',#24658,#24649,#20108,.T.);
#32088=EDGE_CURVE('',#24664,#24655,#20109,.T.);
#32089=EDGE_CURVE('',#24670,#24661,#20110,.T.);
#32090=EDGE_CURVE('',#24676,#24667,#20111,.T.);
#32091=EDGE_CURVE('',#24682,#24673,#20112,.T.);
#32092=EDGE_CURVE('',#24689,#24679,#20113,.T.);
#32093=EDGE_CURVE('',#24691,#24581,#6283,.T.);
#32094=EDGE_CURVE('',#24696,#24685,#20114,.T.);
#32095=EDGE_CURVE('',#24702,#24693,#20115,.T.);
#32096=EDGE_CURVE('',#24708,#24699,#20116,.T.);
#32097=EDGE_CURVE('',#24714,#24705,#20117,.T.);
#32098=EDGE_CURVE('',#24720,#24711,#20118,.T.);
#32099=EDGE_CURVE('',#24726,#24717,#20119,.T.);
#32100=EDGE_CURVE('',#24732,#24723,#20120,.T.);
#32101=EDGE_CURVE('',#24738,#24729,#20121,.T.);
#32102=EDGE_CURVE('',#24744,#24735,#20122,.T.);
#32103=EDGE_CURVE('',#24750,#24741,#20123,.T.);
#32104=EDGE_CURVE('',#24756,#24747,#20124,.T.);
#32105=EDGE_CURVE('',#24762,#24753,#20125,.T.);
#32106=EDGE_CURVE('',#24768,#24759,#20126,.T.);
#32107=EDGE_CURVE('',#24774,#24765,#20127,.T.);
#32108=EDGE_CURVE('',#24780,#24771,#20128,.T.);
#32109=EDGE_CURVE('',#24786,#24777,#20129,.T.);
#32110=EDGE_CURVE('',#24792,#24783,#20130,.T.);
#32111=EDGE_CURVE('',#24795,#24789,#20131,.T.);
#32112=EDGE_CURVE('',#24586,#24794,#20132,.T.);
#32113=EDGE_CURVE('',#24815,#24815,#20133,.T.);
#32114=EDGE_CURVE('',#24815,#24688,#6284,.T.);
#32115=EDGE_CURVE('',#24816,#24816,#20134,.T.);
#32116=EDGE_CURVE('',#24816,#24817,#6285,.T.);
#32117=EDGE_CURVE('',#24817,#24817,#20135,.T.);
#32118=EDGE_CURVE('',#24818,#24818,#20136,.T.);
#32119=EDGE_CURVE('',#24818,#24816,#6286,.T.);
#32120=EDGE_CURVE('',#24819,#24819,#20137,.T.);
#32121=EDGE_CURVE('',#24819,#24818,#6287,.T.);
#32122=EDGE_CURVE('',#24820,#24820,#20138,.T.);
#32123=EDGE_CURVE('',#24820,#24821,#6288,.T.);
#32124=EDGE_CURVE('',#24821,#24821,#20139,.T.);
#32125=EDGE_CURVE('',#24821,#24822,#6289,.T.);
#32126=EDGE_CURVE('',#24822,#24822,#20140,.T.);
#32127=EDGE_CURVE('',#24822,#24823,#6290,.T.);
#32128=EDGE_CURVE('',#24823,#24823,#20141,.T.);
#32129=EDGE_CURVE('',#24824,#24825,#6291,.T.);
#32130=EDGE_CURVE('',#24826,#24824,#20142,.T.);
#32131=EDGE_CURVE('',#24826,#24827,#2152,.T.);
#32132=EDGE_CURVE('',#24825,#24827,#20143,.T.);
#32133=EDGE_CURVE('',#24828,#24829,#6292,.T.);
#32134=EDGE_CURVE('',#24830,#24828,#20144,.T.);
#32135=EDGE_CURVE('',#24830,#24831,#2153,.T.);
#32136=EDGE_CURVE('',#24829,#24831,#20145,.T.);
#32137=EDGE_CURVE('',#24832,#24826,#19540,.T.);
#32138=EDGE_CURVE('',#24833,#24832,#6293,.T.);
#32139=EDGE_CURVE('',#24834,#24833,#19541,.T.);
#32140=EDGE_CURVE('',#24835,#24834,#2154,.T.);
#32141=EDGE_CURVE('',#24836,#24835,#19542,.T.);
#32142=EDGE_CURVE('',#24837,#24836,#6294,.T.);
#32143=EDGE_CURVE('',#24827,#24837,#19543,.T.);
#32144=EDGE_CURVE('',#24838,#24839,#19544,.T.);
#32145=EDGE_CURVE('',#24840,#24838,#2155,.T.);
#32146=EDGE_CURVE('',#24841,#24840,#19545,.T.);
#32147=EDGE_CURVE('',#24842,#24841,#6295,.T.);
#32148=EDGE_CURVE('',#24831,#24842,#19546,.T.);
#32149=EDGE_CURVE('',#24843,#24830,#19547,.T.);
#32150=EDGE_CURVE('',#24839,#24843,#6296,.T.);
#32151=EDGE_CURVE('',#24835,#24829,#20146,.T.);
#32152=EDGE_CURVE('',#24842,#24836,#20147,.T.);
#32153=EDGE_CURVE('',#24828,#24834,#20148,.T.);
#32154=EDGE_CURVE('',#24833,#24843,#20149,.T.);
#32155=EDGE_CURVE('',#24839,#24832,#20150,.T.);
#32156=EDGE_CURVE('',#24824,#24838,#20151,.T.);
#32157=EDGE_CURVE('',#24840,#24825,#20152,.T.);
#32158=EDGE_CURVE('',#24837,#24841,#20153,.T.);
#32159=EDGE_CURVE('',#24844,#24845,#6297,.T.);
#32160=EDGE_CURVE('',#24844,#24846,#550,.T.);
#32161=EDGE_CURVE('',#24846,#24847,#20154,.T.);
#32162=EDGE_CURVE('',#24847,#24845,#551,.T.);
#32163=EDGE_CURVE('',#24848,#24849,#6298,.T.);
#32164=EDGE_CURVE('',#24848,#24844,#552,.T.);
#32165=EDGE_CURVE('',#24845,#24849,#553,.T.);
#32166=EDGE_CURVE('',#24850,#24851,#6299,.T.);
#32167=EDGE_CURVE('',#24850,#24848,#554,.T.);
#32168=EDGE_CURVE('',#24849,#24851,#555,.T.);
#32169=EDGE_CURVE('',#24852,#24853,#6300,.T.);
#32170=EDGE_CURVE('',#24852,#24850,#556,.T.);
#32171=EDGE_CURVE('',#24851,#24853,#557,.T.);
#32172=EDGE_CURVE('',#24854,#24855,#6301,.T.);
#32173=EDGE_CURVE('',#24854,#24852,#558,.T.);
#32174=EDGE_CURVE('',#24853,#24855,#559,.T.);
#32175=EDGE_CURVE('',#24856,#24857,#6302,.T.);
#32176=EDGE_CURVE('',#24856,#24854,#560,.T.);
#32177=EDGE_CURVE('',#24855,#24857,#561,.T.);
#32178=EDGE_CURVE('',#24858,#24859,#6303,.T.);
#32179=EDGE_CURVE('',#24858,#24856,#562,.T.);
#32180=EDGE_CURVE('',#24857,#24859,#563,.T.);
#32181=EDGE_CURVE('',#24860,#24861,#6304,.T.);
#32182=EDGE_CURVE('',#24860,#24858,#564,.T.);
#32183=EDGE_CURVE('',#24859,#24861,#565,.T.);
#32184=EDGE_CURVE('',#24862,#24863,#6305,.T.);
#32185=EDGE_CURVE('',#24862,#24860,#566,.T.);
#32186=EDGE_CURVE('',#24861,#24863,#567,.T.);
#32187=EDGE_CURVE('',#24864,#24865,#6306,.T.);
#32188=EDGE_CURVE('',#24864,#24862,#568,.T.);
#32189=EDGE_CURVE('',#24863,#24865,#569,.T.);
#32190=EDGE_CURVE('',#24866,#24867,#6307,.T.);
#32191=EDGE_CURVE('',#24866,#24864,#570,.T.);
#32192=EDGE_CURVE('',#24865,#24867,#571,.T.);
#32193=EDGE_CURVE('',#24868,#24869,#6308,.T.);
#32194=EDGE_CURVE('',#24868,#24866,#572,.T.);
#32195=EDGE_CURVE('',#24867,#24869,#573,.T.);
#32196=EDGE_CURVE('',#24870,#24871,#6309,.T.);
#32197=EDGE_CURVE('',#24870,#24868,#574,.T.);
#32198=EDGE_CURVE('',#24869,#24871,#575,.T.);
#32199=EDGE_CURVE('',#24872,#24873,#6310,.T.);
#32200=EDGE_CURVE('',#24872,#24870,#576,.T.);
#32201=EDGE_CURVE('',#24871,#24873,#577,.T.);
#32202=EDGE_CURVE('',#24874,#24875,#6311,.T.);
#32203=EDGE_CURVE('',#24874,#24872,#578,.T.);
#32204=EDGE_CURVE('',#24873,#24875,#579,.T.);
#32205=EDGE_CURVE('',#24876,#24877,#6312,.T.);
#32206=EDGE_CURVE('',#24878,#24876,#20155,.T.);
#32207=EDGE_CURVE('',#24878,#24874,#580,.T.);
#32208=EDGE_CURVE('',#24875,#24877,#581,.T.);
#32209=EDGE_CURVE('',#24879,#24880,#6313,.T.);
#32210=EDGE_CURVE('',#24879,#24881,#582,.T.);
#32211=EDGE_CURVE('',#24882,#24881,#20156,.T.);
#32212=EDGE_CURVE('',#24880,#24882,#583,.T.);
#32213=EDGE_CURVE('',#24883,#24884,#6314,.T.);
#32214=EDGE_CURVE('',#24883,#24879,#584,.T.);
#32215=EDGE_CURVE('',#24884,#24880,#585,.T.);
#32216=EDGE_CURVE('',#24885,#24886,#6315,.T.);
#32217=EDGE_CURVE('',#24885,#24883,#586,.T.);
#32218=EDGE_CURVE('',#24886,#24884,#587,.T.);
#32219=EDGE_CURVE('',#24887,#24888,#6316,.T.);
#32220=EDGE_CURVE('',#24887,#24885,#588,.T.);
#32221=EDGE_CURVE('',#24888,#24886,#589,.T.);
#32222=EDGE_CURVE('',#24889,#24890,#6317,.T.);
#32223=EDGE_CURVE('',#24889,#24887,#590,.T.);
#32224=EDGE_CURVE('',#24890,#24888,#591,.T.);
#32225=EDGE_CURVE('',#24891,#24892,#6318,.T.);
#32226=EDGE_CURVE('',#24891,#24889,#592,.T.);
#32227=EDGE_CURVE('',#24892,#24890,#593,.T.);
#32228=EDGE_CURVE('',#24893,#24894,#6319,.T.);
#32229=EDGE_CURVE('',#24893,#24891,#594,.T.);
#32230=EDGE_CURVE('',#24894,#24892,#595,.T.);
#32231=EDGE_CURVE('',#24895,#24896,#6320,.T.);
#32232=EDGE_CURVE('',#24895,#24893,#596,.T.);
#32233=EDGE_CURVE('',#24896,#24894,#597,.T.);
#32234=EDGE_CURVE('',#24897,#24898,#6321,.T.);
#32235=EDGE_CURVE('',#24897,#24895,#598,.T.);
#32236=EDGE_CURVE('',#24898,#24896,#599,.T.);
#32237=EDGE_CURVE('',#24899,#24900,#6322,.T.);
#32238=EDGE_CURVE('',#24899,#24897,#600,.T.);
#32239=EDGE_CURVE('',#24900,#24898,#601,.T.);
#32240=EDGE_CURVE('',#24901,#24902,#6323,.T.);
#32241=EDGE_CURVE('',#24901,#24899,#602,.T.);
#32242=EDGE_CURVE('',#24902,#24900,#603,.T.);
#32243=EDGE_CURVE('',#24903,#24904,#6324,.T.);
#32244=EDGE_CURVE('',#24903,#24901,#604,.T.);
#32245=EDGE_CURVE('',#24904,#24902,#605,.T.);
#32246=EDGE_CURVE('',#24905,#24906,#6325,.T.);
#32247=EDGE_CURVE('',#24905,#24903,#606,.T.);
#32248=EDGE_CURVE('',#24906,#24904,#607,.T.);
#32249=EDGE_CURVE('',#24907,#24908,#6326,.T.);
#32250=EDGE_CURVE('',#24907,#24905,#608,.T.);
#32251=EDGE_CURVE('',#24908,#24906,#609,.T.);
#32252=EDGE_CURVE('',#24909,#24910,#6327,.T.);
#32253=EDGE_CURVE('',#24909,#24907,#610,.T.);
#32254=EDGE_CURVE('',#24910,#24908,#611,.T.);
#32255=EDGE_CURVE('',#24881,#24878,#612,.T.);
#32256=EDGE_CURVE('',#24911,#24878,#20157,.T.);
#32257=EDGE_CURVE('',#24912,#24911,#20158,.T.);
#32258=EDGE_CURVE('',#24912,#24882,#613,.T.);
#32259=EDGE_CURVE('',#24877,#24912,#614,.T.);
#32260=EDGE_CURVE('',#24913,#24847,#615,.T.);
#32261=EDGE_CURVE('',#24913,#24910,#616,.T.);
#32262=EDGE_CURVE('',#24847,#24914,#20159,.T.);
#32263=EDGE_CURVE('',#24914,#24846,#20160,.T.);
#32264=EDGE_CURVE('',#24846,#24915,#617,.T.);
#32265=EDGE_CURVE('',#24915,#24913,#20161,.T.);
#32266=EDGE_CURVE('',#24915,#24909,#618,.T.);
#32267=EDGE_CURVE('',#24876,#24912,#20162,.T.);
#32268=EDGE_CURVE('',#24911,#24916,#20163,.T.);
#32269=EDGE_CURVE('',#24916,#24916,#20164,.T.);
#32270=EDGE_CURVE('',#24917,#24917,#20165,.T.);
#32271=EDGE_CURVE('',#24918,#24919,#6328,.T.);
#32272=EDGE_CURVE('',#24918,#24920,#6329,.T.);
#32273=EDGE_CURVE('',#24920,#24921,#6330,.T.);
#32274=EDGE_CURVE('',#24921,#24919,#6331,.T.);
#32275=EDGE_CURVE('',#24919,#24922,#20166,.T.);
#32276=EDGE_CURVE('',#24922,#24921,#6332,.T.);
#32277=EDGE_CURVE('',#24922,#24923,#6333,.T.);
#32278=EDGE_CURVE('',#24920,#24923,#6334,.T.);
#32279=EDGE_CURVE('',#24923,#24918,#20167,.T.);
#32280=EDGE_CURVE('',#24924,#24925,#6335,.T.);
#32281=EDGE_CURVE('',#24924,#24926,#6336,.T.);
#32282=EDGE_CURVE('',#24926,#24927,#6337,.T.);
#32283=EDGE_CURVE('',#24927,#24925,#6338,.T.);
#32284=EDGE_CURVE('',#24925,#24928,#20168,.T.);
#32285=EDGE_CURVE('',#24928,#24927,#6339,.T.);
#32286=EDGE_CURVE('',#24928,#24929,#6340,.T.);
#32287=EDGE_CURVE('',#24926,#24929,#6341,.T.);
#32288=EDGE_CURVE('',#24929,#24924,#20169,.T.);
#32289=EDGE_CURVE('',#24930,#24931,#6342,.T.);
#32290=EDGE_CURVE('',#24930,#24932,#6343,.T.);
#32291=EDGE_CURVE('',#24932,#24933,#6344,.T.);
#32292=EDGE_CURVE('',#24933,#24931,#6345,.T.);
#32293=EDGE_CURVE('',#24931,#24934,#20170,.T.);
#32294=EDGE_CURVE('',#24934,#24933,#6346,.T.);
#32295=EDGE_CURVE('',#24934,#24935,#6347,.T.);
#32296=EDGE_CURVE('',#24932,#24935,#6348,.T.);
#32297=EDGE_CURVE('',#24935,#24930,#20171,.T.);
#32298=EDGE_CURVE('',#24936,#24937,#6349,.T.);
#32299=EDGE_CURVE('',#24936,#24938,#6350,.T.);
#32300=EDGE_CURVE('',#24938,#24939,#6351,.T.);
#32301=EDGE_CURVE('',#24939,#24937,#6352,.T.);
#32302=EDGE_CURVE('',#24937,#24940,#20172,.T.);
#32303=EDGE_CURVE('',#24940,#24939,#6353,.T.);
#32304=EDGE_CURVE('',#24940,#24941,#6354,.T.);
#32305=EDGE_CURVE('',#24938,#24941,#6355,.T.);
#32306=EDGE_CURVE('',#24941,#24936,#20173,.T.);
#32307=EDGE_CURVE('',#24942,#24943,#6356,.T.);
#32308=EDGE_CURVE('',#24942,#24944,#6357,.T.);
#32309=EDGE_CURVE('',#24944,#24945,#6358,.T.);
#32310=EDGE_CURVE('',#24945,#24943,#6359,.T.);
#32311=EDGE_CURVE('',#24943,#24946,#20174,.T.);
#32312=EDGE_CURVE('',#24946,#24945,#6360,.T.);
#32313=EDGE_CURVE('',#24946,#24947,#6361,.T.);
#32314=EDGE_CURVE('',#24944,#24947,#6362,.T.);
#32315=EDGE_CURVE('',#24947,#24942,#20175,.T.);
#32316=EDGE_CURVE('',#24948,#24949,#6363,.T.);
#32317=EDGE_CURVE('',#24948,#24950,#6364,.T.);
#32318=EDGE_CURVE('',#24950,#24951,#6365,.T.);
#32319=EDGE_CURVE('',#24951,#24949,#6366,.T.);
#32320=EDGE_CURVE('',#24949,#24952,#20176,.T.);
#32321=EDGE_CURVE('',#24952,#24951,#6367,.T.);
#32322=EDGE_CURVE('',#24952,#24953,#6368,.T.);
#32323=EDGE_CURVE('',#24950,#24953,#6369,.T.);
#32324=EDGE_CURVE('',#24953,#24948,#20177,.T.);
#32325=EDGE_CURVE('',#24954,#24955,#6370,.T.);
#32326=EDGE_CURVE('',#24954,#24956,#6371,.T.);
#32327=EDGE_CURVE('',#24956,#24957,#6372,.T.);
#32328=EDGE_CURVE('',#24957,#24955,#6373,.T.);
#32329=EDGE_CURVE('',#24955,#24958,#20178,.T.);
#32330=EDGE_CURVE('',#24958,#24957,#6374,.T.);
#32331=EDGE_CURVE('',#24958,#24959,#6375,.T.);
#32332=EDGE_CURVE('',#24956,#24959,#6376,.T.);
#32333=EDGE_CURVE('',#24959,#24954,#20179,.T.);
#32334=EDGE_CURVE('',#24960,#24961,#6377,.T.);
#32335=EDGE_CURVE('',#24960,#24962,#6378,.T.);
#32336=EDGE_CURVE('',#24962,#24963,#6379,.T.);
#32337=EDGE_CURVE('',#24963,#24961,#6380,.T.);
#32338=EDGE_CURVE('',#24961,#24964,#20180,.T.);
#32339=EDGE_CURVE('',#24964,#24963,#6381,.T.);
#32340=EDGE_CURVE('',#24964,#24965,#6382,.T.);
#32341=EDGE_CURVE('',#24962,#24965,#6383,.T.);
#32342=EDGE_CURVE('',#24965,#24960,#20181,.T.);
#32343=EDGE_CURVE('',#24966,#24967,#6384,.T.);
#32344=EDGE_CURVE('',#24966,#24968,#6385,.T.);
#32345=EDGE_CURVE('',#24968,#24969,#6386,.T.);
#32346=EDGE_CURVE('',#24969,#24967,#6387,.T.);
#32347=EDGE_CURVE('',#24967,#24970,#20182,.T.);
#32348=EDGE_CURVE('',#24970,#24969,#6388,.T.);
#32349=EDGE_CURVE('',#24970,#24971,#6389,.T.);
#32350=EDGE_CURVE('',#24968,#24971,#6390,.T.);
#32351=EDGE_CURVE('',#24971,#24966,#20183,.T.);
#32352=EDGE_CURVE('',#24972,#24973,#6391,.T.);
#32353=EDGE_CURVE('',#24972,#24974,#6392,.T.);
#32354=EDGE_CURVE('',#24974,#24975,#6393,.T.);
#32355=EDGE_CURVE('',#24975,#24973,#6394,.T.);
#32356=EDGE_CURVE('',#24973,#24976,#20184,.T.);
#32357=EDGE_CURVE('',#24976,#24975,#6395,.T.);
#32358=EDGE_CURVE('',#24976,#24977,#6396,.T.);
#32359=EDGE_CURVE('',#24974,#24977,#6397,.T.);
#32360=EDGE_CURVE('',#24977,#24972,#20185,.T.);
#32361=EDGE_CURVE('',#24978,#24979,#6398,.T.);
#32362=EDGE_CURVE('',#24978,#24980,#6399,.T.);
#32363=EDGE_CURVE('',#24980,#24981,#6400,.T.);
#32364=EDGE_CURVE('',#24981,#24979,#6401,.T.);
#32365=EDGE_CURVE('',#24979,#24982,#20186,.T.);
#32366=EDGE_CURVE('',#24982,#24981,#6402,.T.);
#32367=EDGE_CURVE('',#24982,#24983,#6403,.T.);
#32368=EDGE_CURVE('',#24980,#24983,#6404,.T.);
#32369=EDGE_CURVE('',#24983,#24978,#20187,.T.);
#32370=EDGE_CURVE('',#24984,#24985,#6405,.T.);
#32371=EDGE_CURVE('',#24984,#24986,#6406,.T.);
#32372=EDGE_CURVE('',#24986,#24987,#6407,.T.);
#32373=EDGE_CURVE('',#24987,#24985,#6408,.T.);
#32374=EDGE_CURVE('',#24985,#24988,#20188,.T.);
#32375=EDGE_CURVE('',#24988,#24987,#6409,.T.);
#32376=EDGE_CURVE('',#24988,#24989,#6410,.T.);
#32377=EDGE_CURVE('',#24986,#24989,#6411,.T.);
#32378=EDGE_CURVE('',#24989,#24984,#20189,.T.);
#32379=EDGE_CURVE('',#24990,#24991,#6412,.T.);
#32380=EDGE_CURVE('',#24990,#24992,#6413,.T.);
#32381=EDGE_CURVE('',#24992,#24993,#6414,.T.);
#32382=EDGE_CURVE('',#24993,#24991,#6415,.T.);
#32383=EDGE_CURVE('',#24991,#24994,#20190,.T.);
#32384=EDGE_CURVE('',#24994,#24993,#6416,.T.);
#32385=EDGE_CURVE('',#24994,#24995,#6417,.T.);
#32386=EDGE_CURVE('',#24992,#24995,#6418,.T.);
#32387=EDGE_CURVE('',#24995,#24990,#20191,.T.);
#32388=EDGE_CURVE('',#24996,#24997,#6419,.T.);
#32389=EDGE_CURVE('',#24996,#24998,#6420,.T.);
#32390=EDGE_CURVE('',#24998,#24999,#6421,.T.);
#32391=EDGE_CURVE('',#24999,#24997,#6422,.T.);
#32392=EDGE_CURVE('',#24997,#25000,#20192,.T.);
#32393=EDGE_CURVE('',#25000,#24999,#6423,.T.);
#32394=EDGE_CURVE('',#25000,#25001,#6424,.T.);
#32395=EDGE_CURVE('',#24998,#25001,#6425,.T.);
#32396=EDGE_CURVE('',#25001,#24996,#20193,.T.);
#32397=EDGE_CURVE('',#25002,#25003,#6426,.T.);
#32398=EDGE_CURVE('',#25002,#25004,#6427,.T.);
#32399=EDGE_CURVE('',#25004,#25005,#6428,.T.);
#32400=EDGE_CURVE('',#25005,#25003,#6429,.T.);
#32401=EDGE_CURVE('',#25003,#25006,#20194,.T.);
#32402=EDGE_CURVE('',#25006,#25005,#6430,.T.);
#32403=EDGE_CURVE('',#25006,#25007,#6431,.T.);
#32404=EDGE_CURVE('',#25004,#25007,#6432,.T.);
#32405=EDGE_CURVE('',#25007,#25002,#20195,.T.);
#32406=EDGE_CURVE('',#25008,#25009,#6433,.T.);
#32407=EDGE_CURVE('',#25008,#25010,#6434,.T.);
#32408=EDGE_CURVE('',#25010,#25011,#6435,.T.);
#32409=EDGE_CURVE('',#25011,#25009,#6436,.T.);
#32410=EDGE_CURVE('',#25009,#25012,#20196,.T.);
#32411=EDGE_CURVE('',#25012,#25011,#6437,.T.);
#32412=EDGE_CURVE('',#25012,#25013,#6438,.T.);
#32413=EDGE_CURVE('',#25010,#25013,#6439,.T.);
#32414=EDGE_CURVE('',#25013,#25008,#20197,.T.);
#32415=EDGE_CURVE('',#25014,#25015,#6440,.T.);
#32416=EDGE_CURVE('',#25014,#25016,#6441,.T.);
#32417=EDGE_CURVE('',#25016,#25017,#6442,.T.);
#32418=EDGE_CURVE('',#25017,#25015,#6443,.T.);
#32419=EDGE_CURVE('',#25015,#25018,#20198,.T.);
#32420=EDGE_CURVE('',#25018,#25017,#6444,.T.);
#32421=EDGE_CURVE('',#25018,#25019,#6445,.T.);
#32422=EDGE_CURVE('',#25016,#25019,#6446,.T.);
#32423=EDGE_CURVE('',#25019,#25014,#20199,.T.);
#32424=EDGE_CURVE('',#25020,#25021,#6447,.T.);
#32425=EDGE_CURVE('',#25020,#25022,#6448,.T.);
#32426=EDGE_CURVE('',#25022,#25023,#6449,.T.);
#32427=EDGE_CURVE('',#25023,#25021,#6450,.T.);
#32428=EDGE_CURVE('',#25021,#25024,#20200,.T.);
#32429=EDGE_CURVE('',#25025,#25023,#6451,.T.);
#32430=EDGE_CURVE('',#25024,#25025,#20201,.T.);
#32431=EDGE_CURVE('',#25025,#25026,#6452,.T.);
#32432=EDGE_CURVE('',#25022,#25026,#6453,.T.);
#32433=EDGE_CURVE('',#25026,#25027,#20202,.T.);
#32434=EDGE_CURVE('',#25027,#25020,#20203,.T.);
#32435=EDGE_CURVE('',#25028,#25029,#6454,.T.);
#32436=EDGE_CURVE('',#25028,#25030,#6455,.T.);
#32437=EDGE_CURVE('',#25030,#25031,#6456,.T.);
#32438=EDGE_CURVE('',#25031,#25029,#6457,.T.);
#32439=EDGE_CURVE('',#25029,#25032,#20204,.T.);
#32440=EDGE_CURVE('',#25032,#25031,#6458,.T.);
#32441=EDGE_CURVE('',#25032,#25033,#6459,.T.);
#32442=EDGE_CURVE('',#25030,#25033,#6460,.T.);
#32443=EDGE_CURVE('',#25033,#25028,#20205,.T.);
#32444=EDGE_CURVE('',#25034,#25035,#6461,.T.);
#32445=EDGE_CURVE('',#25034,#25036,#6462,.T.);
#32446=EDGE_CURVE('',#25036,#25037,#6463,.T.);
#32447=EDGE_CURVE('',#25037,#25035,#6464,.T.);
#32448=EDGE_CURVE('',#25035,#25038,#20206,.T.);
#32449=EDGE_CURVE('',#25038,#25037,#6465,.T.);
#32450=EDGE_CURVE('',#25038,#25039,#6466,.T.);
#32451=EDGE_CURVE('',#25036,#25039,#6467,.T.);
#32452=EDGE_CURVE('',#25039,#25034,#20207,.T.);
#32453=EDGE_CURVE('',#25040,#25041,#6468,.T.);
#32454=EDGE_CURVE('',#25040,#25042,#6469,.T.);
#32455=EDGE_CURVE('',#25042,#25043,#6470,.T.);
#32456=EDGE_CURVE('',#25043,#25041,#6471,.T.);
#32457=EDGE_CURVE('',#25041,#25044,#20208,.T.);
#32458=EDGE_CURVE('',#25044,#25043,#6472,.T.);
#32459=EDGE_CURVE('',#25044,#25045,#6473,.T.);
#32460=EDGE_CURVE('',#25042,#25045,#6474,.T.);
#32461=EDGE_CURVE('',#25045,#25040,#20209,.T.);
#32462=EDGE_CURVE('',#25046,#25047,#6475,.T.);
#32463=EDGE_CURVE('',#25046,#25048,#6476,.T.);
#32464=EDGE_CURVE('',#25048,#25049,#6477,.T.);
#32465=EDGE_CURVE('',#25049,#25047,#6478,.T.);
#32466=EDGE_CURVE('',#25047,#25050,#20210,.T.);
#32467=EDGE_CURVE('',#25050,#25049,#6479,.T.);
#32468=EDGE_CURVE('',#25050,#25051,#6480,.T.);
#32469=EDGE_CURVE('',#25048,#25051,#6481,.T.);
#32470=EDGE_CURVE('',#25051,#25046,#20211,.T.);
#32471=EDGE_CURVE('',#25052,#25053,#6482,.T.);
#32472=EDGE_CURVE('',#25052,#25054,#6483,.T.);
#32473=EDGE_CURVE('',#25054,#25055,#6484,.T.);
#32474=EDGE_CURVE('',#25055,#25053,#6485,.T.);
#32475=EDGE_CURVE('',#25053,#25056,#20212,.T.);
#32476=EDGE_CURVE('',#25056,#25055,#6486,.T.);
#32477=EDGE_CURVE('',#25056,#25057,#6487,.T.);
#32478=EDGE_CURVE('',#25054,#25057,#6488,.T.);
#32479=EDGE_CURVE('',#25057,#25052,#20213,.T.);
#32480=EDGE_CURVE('',#25058,#25059,#6489,.T.);
#32481=EDGE_CURVE('',#25058,#25060,#6490,.T.);
#32482=EDGE_CURVE('',#25060,#25061,#6491,.T.);
#32483=EDGE_CURVE('',#25061,#25059,#6492,.T.);
#32484=EDGE_CURVE('',#25059,#25062,#20214,.T.);
#32485=EDGE_CURVE('',#25062,#25061,#6493,.T.);
#32486=EDGE_CURVE('',#25062,#25063,#6494,.T.);
#32487=EDGE_CURVE('',#25060,#25063,#6495,.T.);
#32488=EDGE_CURVE('',#25063,#25058,#20215,.T.);
#32489=EDGE_CURVE('',#25064,#25065,#6496,.T.);
#32490=EDGE_CURVE('',#25064,#25066,#6497,.T.);
#32491=EDGE_CURVE('',#25066,#25067,#6498,.T.);
#32492=EDGE_CURVE('',#25067,#25065,#6499,.T.);
#32493=EDGE_CURVE('',#25065,#25068,#20216,.T.);
#32494=EDGE_CURVE('',#25068,#25067,#6500,.T.);
#32495=EDGE_CURVE('',#25068,#25069,#6501,.T.);
#32496=EDGE_CURVE('',#25066,#25069,#6502,.T.);
#32497=EDGE_CURVE('',#25069,#25064,#20217,.T.);
#32498=EDGE_CURVE('',#25070,#25071,#6503,.T.);
#32499=EDGE_CURVE('',#25070,#25072,#6504,.T.);
#32500=EDGE_CURVE('',#25072,#25073,#6505,.T.);
#32501=EDGE_CURVE('',#25073,#25071,#6506,.T.);
#32502=EDGE_CURVE('',#25071,#25074,#20218,.T.);
#32503=EDGE_CURVE('',#25074,#25073,#6507,.T.);
#32504=EDGE_CURVE('',#25074,#25075,#6508,.T.);
#32505=EDGE_CURVE('',#25072,#25075,#6509,.T.);
#32506=EDGE_CURVE('',#25075,#25070,#20219,.T.);
#32507=EDGE_CURVE('',#25076,#25077,#6510,.T.);
#32508=EDGE_CURVE('',#25076,#25078,#6511,.T.);
#32509=EDGE_CURVE('',#25078,#25079,#6512,.T.);
#32510=EDGE_CURVE('',#25079,#25077,#6513,.T.);
#32511=EDGE_CURVE('',#25077,#25080,#20220,.T.);
#32512=EDGE_CURVE('',#25080,#25079,#6514,.T.);
#32513=EDGE_CURVE('',#25080,#25081,#6515,.T.);
#32514=EDGE_CURVE('',#25078,#25081,#6516,.T.);
#32515=EDGE_CURVE('',#25081,#25076,#20221,.T.);
#32516=EDGE_CURVE('',#25082,#25083,#6517,.T.);
#32517=EDGE_CURVE('',#25082,#25084,#6518,.T.);
#32518=EDGE_CURVE('',#25084,#25085,#6519,.T.);
#32519=EDGE_CURVE('',#25085,#25083,#6520,.T.);
#32520=EDGE_CURVE('',#25083,#25086,#20222,.T.);
#32521=EDGE_CURVE('',#25086,#25085,#6521,.T.);
#32522=EDGE_CURVE('',#25086,#25087,#6522,.T.);
#32523=EDGE_CURVE('',#25084,#25087,#6523,.T.);
#32524=EDGE_CURVE('',#25087,#25082,#20223,.T.);
#32525=EDGE_CURVE('',#25088,#25089,#6524,.T.);
#32526=EDGE_CURVE('',#25088,#25090,#6525,.T.);
#32527=EDGE_CURVE('',#25090,#25091,#6526,.T.);
#32528=EDGE_CURVE('',#25091,#25089,#6527,.T.);
#32529=EDGE_CURVE('',#25089,#25092,#20224,.T.);
#32530=EDGE_CURVE('',#25092,#25091,#6528,.T.);
#32531=EDGE_CURVE('',#25092,#25093,#6529,.T.);
#32532=EDGE_CURVE('',#25090,#25093,#6530,.T.);
#32533=EDGE_CURVE('',#25093,#25088,#20225,.T.);
#32534=EDGE_CURVE('',#25094,#25095,#6531,.T.);
#32535=EDGE_CURVE('',#25094,#25096,#6532,.T.);
#32536=EDGE_CURVE('',#25096,#25097,#6533,.T.);
#32537=EDGE_CURVE('',#25097,#25095,#6534,.T.);
#32538=EDGE_CURVE('',#25095,#25098,#20226,.T.);
#32539=EDGE_CURVE('',#25098,#25097,#6535,.T.);
#32540=EDGE_CURVE('',#25098,#25099,#6536,.T.);
#32541=EDGE_CURVE('',#25096,#25099,#6537,.T.);
#32542=EDGE_CURVE('',#25099,#25094,#20227,.T.);
#32543=EDGE_CURVE('',#25100,#25101,#6538,.T.);
#32544=EDGE_CURVE('',#25100,#25102,#6539,.T.);
#32545=EDGE_CURVE('',#25102,#25103,#6540,.T.);
#32546=EDGE_CURVE('',#25103,#25101,#6541,.T.);
#32547=EDGE_CURVE('',#25101,#25104,#20228,.T.);
#32548=EDGE_CURVE('',#25104,#25103,#6542,.T.);
#32549=EDGE_CURVE('',#25104,#25105,#6543,.T.);
#32550=EDGE_CURVE('',#25102,#25105,#6544,.T.);
#32551=EDGE_CURVE('',#25105,#25100,#20229,.T.);
#32552=EDGE_CURVE('',#25106,#25107,#6545,.T.);
#32553=EDGE_CURVE('',#25106,#25108,#6546,.T.);
#32554=EDGE_CURVE('',#25108,#25109,#6547,.T.);
#32555=EDGE_CURVE('',#25109,#25107,#6548,.T.);
#32556=EDGE_CURVE('',#25107,#25110,#20230,.T.);
#32557=EDGE_CURVE('',#25110,#25109,#6549,.T.);
#32558=EDGE_CURVE('',#25110,#25111,#6550,.T.);
#32559=EDGE_CURVE('',#25108,#25111,#6551,.T.);
#32560=EDGE_CURVE('',#25111,#25106,#20231,.T.);
#32561=EDGE_CURVE('',#25112,#25113,#6552,.T.);
#32562=EDGE_CURVE('',#25112,#25114,#6553,.T.);
#32563=EDGE_CURVE('',#25114,#25115,#6554,.T.);
#32564=EDGE_CURVE('',#25115,#25113,#6555,.T.);
#32565=EDGE_CURVE('',#25113,#25116,#20232,.T.);
#32566=EDGE_CURVE('',#25116,#25115,#6556,.T.);
#32567=EDGE_CURVE('',#25116,#25117,#6557,.T.);
#32568=EDGE_CURVE('',#25114,#25117,#6558,.T.);
#32569=EDGE_CURVE('',#25117,#25112,#20233,.T.);
#32570=EDGE_CURVE('',#25118,#25119,#6559,.T.);
#32571=EDGE_CURVE('',#25118,#25120,#6560,.T.);
#32572=EDGE_CURVE('',#25120,#25121,#6561,.T.);
#32573=EDGE_CURVE('',#25121,#25119,#6562,.T.);
#32574=EDGE_CURVE('',#25119,#25122,#20234,.T.);
#32575=EDGE_CURVE('',#25122,#25121,#6563,.T.);
#32576=EDGE_CURVE('',#25122,#25123,#6564,.T.);
#32577=EDGE_CURVE('',#25120,#25123,#6565,.T.);
#32578=EDGE_CURVE('',#25123,#25118,#20235,.T.);
#32579=EDGE_CURVE('',#25124,#25125,#6566,.T.);
#32580=EDGE_CURVE('',#25124,#25126,#6567,.T.);
#32581=EDGE_CURVE('',#25126,#25127,#6568,.T.);
#32582=EDGE_CURVE('',#25127,#25125,#6569,.T.);
#32583=EDGE_CURVE('',#25125,#25128,#20236,.T.);
#32584=EDGE_CURVE('',#25128,#25127,#6570,.T.);
#32585=EDGE_CURVE('',#25128,#25129,#6571,.T.);
#32586=EDGE_CURVE('',#25126,#25129,#6572,.T.);
#32587=EDGE_CURVE('',#25129,#25124,#20237,.T.);
#32588=EDGE_CURVE('',#25130,#25131,#20238,.T.);
#32589=EDGE_CURVE('',#25132,#25130,#6573,.T.);
#32590=EDGE_CURVE('',#25131,#25132,#6574,.T.);
#32591=EDGE_CURVE('',#25133,#25130,#6575,.T.);
#32592=EDGE_CURVE('',#25133,#25134,#6576,.T.);
#32593=EDGE_CURVE('',#25134,#25132,#6577,.T.);
#32594=EDGE_CURVE('',#25131,#25135,#6578,.T.);
#32595=EDGE_CURVE('',#25134,#25135,#6579,.T.);
#32596=EDGE_CURVE('',#25135,#25133,#20239,.T.);
#32597=EDGE_CURVE('',#25136,#25137,#6580,.T.);
#32598=EDGE_CURVE('',#25137,#25137,#20240,.T.);
#32599=EDGE_CURVE('',#25138,#25139,#6581,.T.);
#32600=EDGE_CURVE('',#25140,#25138,#6582,.T.);
#32601=EDGE_CURVE('',#25141,#25140,#6583,.T.);
#32602=EDGE_CURVE('',#25141,#25139,#6584,.T.);
#32603=EDGE_CURVE('',#25139,#25142,#6585,.T.);
#32604=EDGE_CURVE('',#25143,#25141,#6586,.T.);
#32605=EDGE_CURVE('',#25143,#25142,#6587,.T.);
#32606=EDGE_CURVE('',#25142,#25144,#6588,.T.);
#32607=EDGE_CURVE('',#25145,#25143,#6589,.T.);
#32608=EDGE_CURVE('',#25145,#25144,#6590,.T.);
#32609=EDGE_CURVE('',#25144,#25146,#6591,.T.);
#32610=EDGE_CURVE('',#25147,#25145,#6592,.T.);
#32611=EDGE_CURVE('',#25147,#25146,#6593,.T.);
#32612=EDGE_CURVE('',#25146,#25148,#6594,.T.);
#32613=EDGE_CURVE('',#25149,#25147,#6595,.T.);
#32614=EDGE_CURVE('',#25149,#25148,#6596,.T.);
#32615=EDGE_CURVE('',#25148,#25138,#6597,.T.);
#32616=EDGE_CURVE('',#25140,#25149,#6598,.T.);
#32617=EDGE_CURVE('',#25150,#25150,#20241,.T.);
#32618=EDGE_CURVE('',#24914,#25150,#6599,.T.);
#32619=EDGE_CURVE('',#24928,#24919,#20242,.T.);
#32620=EDGE_CURVE('',#24934,#24925,#20243,.T.);
#32621=EDGE_CURVE('',#24940,#24931,#20244,.T.);
#32622=EDGE_CURVE('',#24946,#24937,#20245,.T.);
#32623=EDGE_CURVE('',#24952,#24943,#20246,.T.);
#32624=EDGE_CURVE('',#24958,#24949,#20247,.T.);
#32625=EDGE_CURVE('',#24964,#24955,#20248,.T.);
#32626=EDGE_CURVE('',#24970,#24961,#20249,.T.);
#32627=EDGE_CURVE('',#24976,#24967,#20250,.T.);
#32628=EDGE_CURVE('',#24982,#24973,#20251,.T.);
#32629=EDGE_CURVE('',#24988,#24979,#20252,.T.);
#32630=EDGE_CURVE('',#24994,#24985,#20253,.T.);
#32631=EDGE_CURVE('',#25000,#24991,#20254,.T.);
#32632=EDGE_CURVE('',#25006,#24997,#20255,.T.);
#32633=EDGE_CURVE('',#25012,#25003,#20256,.T.);
#32634=EDGE_CURVE('',#25018,#25009,#20257,.T.);
#32635=EDGE_CURVE('',#25025,#25015,#20258,.T.);
#32636=EDGE_CURVE('',#25027,#24917,#6600,.T.);
#32637=EDGE_CURVE('',#25032,#25021,#20259,.T.);
#32638=EDGE_CURVE('',#25038,#25029,#20260,.T.);
#32639=EDGE_CURVE('',#25044,#25035,#20261,.T.);
#32640=EDGE_CURVE('',#25050,#25041,#20262,.T.);
#32641=EDGE_CURVE('',#25056,#25047,#20263,.T.);
#32642=EDGE_CURVE('',#25062,#25053,#20264,.T.);
#32643=EDGE_CURVE('',#25068,#25059,#20265,.T.);
#32644=EDGE_CURVE('',#25074,#25065,#20266,.T.);
#32645=EDGE_CURVE('',#25080,#25071,#20267,.T.);
#32646=EDGE_CURVE('',#25086,#25077,#20268,.T.);
#32647=EDGE_CURVE('',#25092,#25083,#20269,.T.);
#32648=EDGE_CURVE('',#25098,#25089,#20270,.T.);
#32649=EDGE_CURVE('',#25104,#25095,#20271,.T.);
#32650=EDGE_CURVE('',#25110,#25101,#20272,.T.);
#32651=EDGE_CURVE('',#25116,#25107,#20273,.T.);
#32652=EDGE_CURVE('',#25122,#25113,#20274,.T.);
#32653=EDGE_CURVE('',#25128,#25119,#20275,.T.);
#32654=EDGE_CURVE('',#25131,#25125,#20276,.T.);
#32655=EDGE_CURVE('',#24922,#25130,#20277,.T.);
#32656=EDGE_CURVE('',#25151,#25151,#20278,.T.);
#32657=EDGE_CURVE('',#25151,#25024,#6601,.T.);
#32658=EDGE_CURVE('',#25152,#25152,#20279,.T.);
#32659=EDGE_CURVE('',#25152,#25153,#20280,.T.);
#32660=EDGE_CURVE('',#25153,#25154,#20281,.T.);
#32661=EDGE_CURVE('',#25154,#25153,#20282,.T.);
#32662=EDGE_CURVE('',#25154,#25155,#6602,.T.);
#32663=EDGE_CURVE('',#25155,#25155,#20283,.T.);
#32664=EDGE_CURVE('',#25156,#25156,#20284,.T.);
#32665=EDGE_CURVE('',#25157,#25157,#20285,.T.);
#32666=EDGE_CURVE('',#25157,#25156,#6603,.T.);
#32667=EDGE_CURVE('',#25155,#25157,#6604,.T.);
#32668=EDGE_CURVE('',#25158,#25159,#6605,.T.);
#32669=EDGE_CURVE('',#25158,#25160,#619,.T.);
#32670=EDGE_CURVE('',#25160,#25161,#20286,.T.);
#32671=EDGE_CURVE('',#25161,#25159,#620,.T.);
#32672=EDGE_CURVE('',#25162,#25163,#6606,.T.);
#32673=EDGE_CURVE('',#25162,#25158,#621,.T.);
#32674=EDGE_CURVE('',#25159,#25163,#622,.T.);
#32675=EDGE_CURVE('',#25164,#25165,#6607,.T.);
#32676=EDGE_CURVE('',#25164,#25162,#623,.T.);
#32677=EDGE_CURVE('',#25163,#25165,#624,.T.);
#32678=EDGE_CURVE('',#25166,#25167,#6608,.T.);
#32679=EDGE_CURVE('',#25166,#25164,#625,.T.);
#32680=EDGE_CURVE('',#25165,#25167,#626,.T.);
#32681=EDGE_CURVE('',#25168,#25169,#6609,.T.);
#32682=EDGE_CURVE('',#25168,#25166,#627,.T.);
#32683=EDGE_CURVE('',#25167,#25169,#628,.T.);
#32684=EDGE_CURVE('',#25170,#25171,#6610,.T.);
#32685=EDGE_CURVE('',#25170,#25168,#629,.T.);
#32686=EDGE_CURVE('',#25169,#25171,#630,.T.);
#32687=EDGE_CURVE('',#25172,#25173,#6611,.T.);
#32688=EDGE_CURVE('',#25172,#25170,#631,.T.);
#32689=EDGE_CURVE('',#25171,#25173,#632,.T.);
#32690=EDGE_CURVE('',#25174,#25175,#6612,.T.);
#32691=EDGE_CURVE('',#25174,#25172,#633,.T.);
#32692=EDGE_CURVE('',#25173,#25175,#634,.T.);
#32693=EDGE_CURVE('',#25176,#25177,#6613,.T.);
#32694=EDGE_CURVE('',#25176,#25174,#635,.T.);
#32695=EDGE_CURVE('',#25175,#25177,#636,.T.);
#32696=EDGE_CURVE('',#25178,#25179,#6614,.T.);
#32697=EDGE_CURVE('',#25178,#25176,#637,.T.);
#32698=EDGE_CURVE('',#25177,#25179,#638,.T.);
#32699=EDGE_CURVE('',#25180,#25181,#6615,.T.);
#32700=EDGE_CURVE('',#25180,#25178,#639,.T.);
#32701=EDGE_CURVE('',#25179,#25181,#640,.T.);
#32702=EDGE_CURVE('',#25182,#25183,#6616,.T.);
#32703=EDGE_CURVE('',#25182,#25180,#641,.T.);
#32704=EDGE_CURVE('',#25181,#25183,#642,.T.);
#32705=EDGE_CURVE('',#25184,#25185,#6617,.T.);
#32706=EDGE_CURVE('',#25184,#25182,#643,.T.);
#32707=EDGE_CURVE('',#25183,#25185,#644,.T.);
#32708=EDGE_CURVE('',#25186,#25187,#6618,.T.);
#32709=EDGE_CURVE('',#25186,#25184,#645,.T.);
#32710=EDGE_CURVE('',#25185,#25187,#646,.T.);
#32711=EDGE_CURVE('',#25188,#25189,#6619,.T.);
#32712=EDGE_CURVE('',#25188,#25186,#647,.T.);
#32713=EDGE_CURVE('',#25187,#25189,#648,.T.);
#32714=EDGE_CURVE('',#25190,#25191,#6620,.T.);
#32715=EDGE_CURVE('',#25190,#25188,#649,.T.);
#32716=EDGE_CURVE('',#25189,#25191,#650,.T.);
#32717=EDGE_CURVE('',#25192,#25193,#6621,.T.);
#32718=EDGE_CURVE('',#25192,#25190,#651,.T.);
#32719=EDGE_CURVE('',#25191,#25193,#652,.T.);
#32720=EDGE_CURVE('',#25194,#25195,#6622,.T.);
#32721=EDGE_CURVE('',#25194,#25192,#653,.T.);
#32722=EDGE_CURVE('',#25193,#25195,#654,.T.);
#32723=EDGE_CURVE('',#25196,#25197,#6623,.T.);
#32724=EDGE_CURVE('',#25196,#25194,#655,.T.);
#32725=EDGE_CURVE('',#25195,#25197,#656,.T.);
#32726=EDGE_CURVE('',#25198,#25199,#6624,.T.);
#32727=EDGE_CURVE('',#25198,#25196,#657,.T.);
#32728=EDGE_CURVE('',#25197,#25199,#658,.T.);
#32729=EDGE_CURVE('',#25200,#25201,#6625,.T.);
#32730=EDGE_CURVE('',#25200,#25198,#659,.T.);
#32731=EDGE_CURVE('',#25199,#25201,#660,.T.);
#32732=EDGE_CURVE('',#25202,#25203,#6626,.T.);
#32733=EDGE_CURVE('',#25202,#25200,#661,.T.);
#32734=EDGE_CURVE('',#25201,#25203,#662,.T.);
#32735=EDGE_CURVE('',#25204,#25205,#6627,.T.);
#32736=EDGE_CURVE('',#25204,#25202,#663,.T.);
#32737=EDGE_CURVE('',#25203,#25205,#664,.T.);
#32738=EDGE_CURVE('',#25206,#25207,#6628,.T.);
#32739=EDGE_CURVE('',#25206,#25208,#665,.T.);
#32740=EDGE_CURVE('',#25209,#25208,#20287,.T.);
#32741=EDGE_CURVE('',#25207,#25209,#666,.T.);
#32742=EDGE_CURVE('',#25210,#25211,#6629,.T.);
#32743=EDGE_CURVE('',#25210,#25206,#667,.T.);
#32744=EDGE_CURVE('',#25211,#25207,#668,.T.);
#32745=EDGE_CURVE('',#25212,#25213,#6630,.T.);
#32746=EDGE_CURVE('',#25212,#25210,#669,.T.);
#32747=EDGE_CURVE('',#25213,#25211,#670,.T.);
#32748=EDGE_CURVE('',#25214,#25215,#6631,.T.);
#32749=EDGE_CURVE('',#25214,#25212,#671,.T.);
#32750=EDGE_CURVE('',#25215,#25213,#672,.T.);
#32751=EDGE_CURVE('',#25216,#25217,#6632,.T.);
#32752=EDGE_CURVE('',#25216,#25214,#673,.T.);
#32753=EDGE_CURVE('',#25217,#25215,#674,.T.);
#32754=EDGE_CURVE('',#25218,#25219,#6633,.T.);
#32755=EDGE_CURVE('',#25218,#25216,#675,.T.);
#32756=EDGE_CURVE('',#25219,#25217,#676,.T.);
#32757=EDGE_CURVE('',#25220,#25221,#6634,.T.);
#32758=EDGE_CURVE('',#25220,#25218,#677,.T.);
#32759=EDGE_CURVE('',#25221,#25219,#678,.T.);
#32760=EDGE_CURVE('',#25222,#25223,#6635,.T.);
#32761=EDGE_CURVE('',#25222,#25220,#679,.T.);
#32762=EDGE_CURVE('',#25223,#25221,#680,.T.);
#32763=EDGE_CURVE('',#25224,#25225,#6636,.T.);
#32764=EDGE_CURVE('',#25224,#25222,#681,.T.);
#32765=EDGE_CURVE('',#25225,#25223,#682,.T.);
#32766=EDGE_CURVE('',#25226,#25227,#6637,.T.);
#32767=EDGE_CURVE('',#25226,#25224,#683,.T.);
#32768=EDGE_CURVE('',#25227,#25225,#684,.T.);
#32769=EDGE_CURVE('',#25228,#25229,#6638,.T.);
#32770=EDGE_CURVE('',#25228,#25226,#685,.T.);
#32771=EDGE_CURVE('',#25229,#25227,#686,.T.);
#32772=EDGE_CURVE('',#25230,#25231,#6639,.T.);
#32773=EDGE_CURVE('',#25230,#25228,#687,.T.);
#32774=EDGE_CURVE('',#25231,#25229,#688,.T.);
#32775=EDGE_CURVE('',#25232,#25233,#6640,.T.);
#32776=EDGE_CURVE('',#25232,#25230,#689,.T.);
#32777=EDGE_CURVE('',#25233,#25231,#690,.T.);
#32778=EDGE_CURVE('',#25234,#25235,#6641,.T.);
#32779=EDGE_CURVE('',#25234,#25232,#691,.T.);
#32780=EDGE_CURVE('',#25235,#25233,#692,.T.);
#32781=EDGE_CURVE('',#25236,#25237,#6642,.T.);
#32782=EDGE_CURVE('',#25236,#25234,#693,.T.);
#32783=EDGE_CURVE('',#25237,#25235,#694,.T.);
#32784=EDGE_CURVE('',#25238,#25239,#6643,.T.);
#32785=EDGE_CURVE('',#25238,#25236,#695,.T.);
#32786=EDGE_CURVE('',#25239,#25237,#696,.T.);
#32787=EDGE_CURVE('',#25240,#25241,#6644,.T.);
#32788=EDGE_CURVE('',#25240,#25238,#697,.T.);
#32789=EDGE_CURVE('',#25241,#25239,#698,.T.);
#32790=EDGE_CURVE('',#25242,#25243,#6645,.T.);
#32791=EDGE_CURVE('',#25242,#25240,#699,.T.);
#32792=EDGE_CURVE('',#25243,#25241,#700,.T.);
#32793=EDGE_CURVE('',#25244,#25245,#6646,.T.);
#32794=EDGE_CURVE('',#25244,#25242,#701,.T.);
#32795=EDGE_CURVE('',#25245,#25243,#702,.T.);
#32796=EDGE_CURVE('',#25246,#25247,#6647,.T.);
#32797=EDGE_CURVE('',#25246,#25244,#703,.T.);
#32798=EDGE_CURVE('',#25247,#25245,#704,.T.);
#32799=EDGE_CURVE('',#25248,#25249,#6648,.T.);
#32800=EDGE_CURVE('',#25248,#25246,#705,.T.);
#32801=EDGE_CURVE('',#25249,#25247,#706,.T.);
#32802=EDGE_CURVE('',#25250,#25251,#6649,.T.);
#32803=EDGE_CURVE('',#25250,#25248,#707,.T.);
#32804=EDGE_CURVE('',#25251,#25249,#708,.T.);
#32805=EDGE_CURVE('',#25252,#25253,#6650,.T.);
#32806=EDGE_CURVE('',#25252,#25250,#709,.T.);
#32807=EDGE_CURVE('',#25253,#25251,#710,.T.);
#32808=EDGE_CURVE('',#25208,#25254,#711,.T.);
#32809=EDGE_CURVE('',#25255,#25254,#20288,.T.);
#32810=EDGE_CURVE('',#25256,#25255,#20289,.T.);
#32811=EDGE_CURVE('',#25256,#25209,#712,.T.);
#32812=EDGE_CURVE('',#25205,#25256,#713,.T.);
#32813=EDGE_CURVE('',#25257,#25161,#714,.T.);
#32814=EDGE_CURVE('',#25257,#25253,#715,.T.);
#32815=EDGE_CURVE('',#25161,#25258,#20290,.T.);
#32816=EDGE_CURVE('',#25258,#25160,#20291,.T.);
#32817=EDGE_CURVE('',#25160,#25259,#716,.T.);
#32818=EDGE_CURVE('',#25259,#25257,#20292,.T.);
#32819=EDGE_CURVE('',#25259,#25252,#717,.T.);
#32820=EDGE_CURVE('',#25254,#25204,#718,.T.);
#32821=EDGE_CURVE('',#25255,#25260,#20293,.T.);
#32822=EDGE_CURVE('',#25260,#25260,#20294,.T.);
#32823=EDGE_CURVE('',#25254,#25256,#20295,.T.);
#32824=EDGE_CURVE('',#25261,#25261,#20296,.T.);
#32825=EDGE_CURVE('',#25262,#25263,#19548,.T.);
#32826=EDGE_CURVE('',#25264,#25262,#19549,.T.);
#32827=EDGE_CURVE('',#25265,#25264,#19550,.T.);
#32828=EDGE_CURVE('',#25266,#25265,#19551,.T.);
#32829=EDGE_CURVE('',#25267,#25266,#19552,.T.);
#32830=EDGE_CURVE('',#25267,#25268,#6651,.T.);
#32831=EDGE_CURVE('',#25268,#25268,#20297,.T.);
#32832=EDGE_CURVE('',#25263,#25267,#19553,.T.);
#32833=EDGE_CURVE('',#25269,#25265,#6652,.T.);
#32834=EDGE_CURVE('',#25269,#25270,#6653,.T.);
#32835=EDGE_CURVE('',#25270,#25266,#6654,.T.);
#32836=EDGE_CURVE('',#25271,#25264,#6655,.T.);
#32837=EDGE_CURVE('',#25271,#25269,#6656,.T.);
#32838=EDGE_CURVE('',#25272,#25262,#6657,.T.);
#32839=EDGE_CURVE('',#25272,#25271,#6658,.T.);
#32840=EDGE_CURVE('',#25273,#25273,#20298,.T.);
#32841=EDGE_CURVE('',#25273,#25261,#6659,.T.);
#32842=EDGE_CURVE('',#25274,#25274,#20299,.T.);
#32843=EDGE_CURVE('',#25258,#25274,#6660,.T.);
#32844=EDGE_CURVE('',#25275,#25263,#6661,.T.);
#32845=EDGE_CURVE('',#25275,#25272,#6662,.T.);
#32846=EDGE_CURVE('',#25276,#25267,#6663,.T.);
#32847=EDGE_CURVE('',#25276,#25275,#6664,.T.);
#32848=EDGE_CURVE('',#25270,#25276,#6665,.T.);
#32849=EDGE_CURVE('',#25277,#25277,#20300,.T.);
#32850=EDGE_CURVE('',#25277,#25278,#6666,.T.);
#32851=EDGE_CURVE('',#25278,#25278,#20301,.T.);
#32852=EDGE_CURVE('',#25279,#25279,#20302,.T.);
#32853=EDGE_CURVE('',#25279,#25277,#6667,.T.);
#32854=EDGE_CURVE('',#25280,#25280,#20303,.T.);
#32855=EDGE_CURVE('',#25280,#25279,#6668,.T.);
#32856=EDGE_CURVE('',#25281,#25281,#20304,.T.);
#32857=EDGE_CURVE('',#25281,#25282,#6669,.T.);
#32858=EDGE_CURVE('',#25282,#25282,#20305,.T.);
#32859=EDGE_CURVE('',#25282,#25283,#6670,.T.);
#32860=EDGE_CURVE('',#25283,#25283,#20306,.T.);
#32861=EDGE_CURVE('',#25283,#25284,#6671,.T.);
#32862=EDGE_CURVE('',#25284,#25284,#20307,.T.);
#32863=EDGE_CURVE('',#25285,#25286,#6672,.T.);
#32864=EDGE_CURVE('',#25287,#25285,#20308,.T.);
#32865=EDGE_CURVE('',#25287,#25288,#2156,.T.);
#32866=EDGE_CURVE('',#25286,#25288,#20309,.T.);
#32867=EDGE_CURVE('',#25289,#25290,#19554,.T.);
#32868=EDGE_CURVE('',#25291,#25289,#6673,.T.);
#32869=EDGE_CURVE('',#25292,#25291,#19555,.T.);
#32870=EDGE_CURVE('',#25293,#25292,#2157,.T.);
#32871=EDGE_CURVE('',#25294,#25293,#19556,.T.);
#32872=EDGE_CURVE('',#25295,#25294,#6674,.T.);
#32873=EDGE_CURVE('',#25296,#25295,#19557,.T.);
#32874=EDGE_CURVE('',#25290,#25296,#2158,.T.);
#32875=EDGE_CURVE('',#25297,#25298,#19558,.T.);
#32876=EDGE_CURVE('',#25299,#25297,#2159,.T.);
#32877=EDGE_CURVE('',#25300,#25299,#19559,.T.);
#32878=EDGE_CURVE('',#25301,#25300,#6675,.T.);
#32879=EDGE_CURVE('',#25288,#25301,#19560,.T.);
#32880=EDGE_CURVE('',#25302,#25287,#19561,.T.);
#32881=EDGE_CURVE('',#25298,#25302,#6676,.T.);
#32882=EDGE_CURVE('',#25293,#25286,#20310,.T.);
#32883=EDGE_CURVE('',#25301,#25294,#20311,.T.);
#32884=EDGE_CURVE('',#25285,#25292,#20312,.T.);
#32885=EDGE_CURVE('',#25291,#25302,#20313,.T.);
#32886=EDGE_CURVE('',#25298,#25289,#20314,.T.);
#32887=EDGE_CURVE('',#25290,#25297,#20315,.T.);
#32888=EDGE_CURVE('',#25299,#25296,#20316,.T.);
#32889=EDGE_CURVE('',#25295,#25300,#20317,.T.);
#32890=EDGE_CURVE('',#25303,#25303,#20318,.T.);
#32891=EDGE_CURVE('',#25303,#25304,#6677,.T.);
#32892=EDGE_CURVE('',#25304,#25304,#20319,.T.);
#32893=EDGE_CURVE('',#25304,#25305,#6678,.T.);
#32894=EDGE_CURVE('',#25305,#25305,#20320,.T.);
#32895=EDGE_CURVE('',#25305,#25306,#6679,.T.);
#32896=EDGE_CURVE('',#25306,#25306,#20321,.T.);
#32897=EDGE_CURVE('',#25307,#25307,#20322,.T.);
#32898=EDGE_CURVE('',#25307,#25308,#6680,.T.);
#32899=EDGE_CURVE('',#25309,#25308,#19562,.T.);
#32900=EDGE_CURVE('',#25310,#25309,#19563,.T.);
#32901=EDGE_CURVE('',#25311,#25310,#19564,.T.);
#32902=EDGE_CURVE('',#25312,#25311,#19565,.T.);
#32903=EDGE_CURVE('',#25313,#25312,#19566,.T.);
#32904=EDGE_CURVE('',#25308,#25313,#19567,.T.);
#32905=EDGE_CURVE('',#25312,#25314,#6681,.T.);
#32906=EDGE_CURVE('',#25314,#25315,#19568,.T.);
#32907=EDGE_CURVE('',#25313,#25315,#6682,.T.);
#32908=EDGE_CURVE('',#25311,#25316,#6683,.T.);
#32909=EDGE_CURVE('',#25316,#25314,#19569,.T.);
#32910=EDGE_CURVE('',#25310,#25317,#6684,.T.);
#32911=EDGE_CURVE('',#25317,#25316,#19570,.T.);
#32912=EDGE_CURVE('',#25318,#25317,#19571,.T.);
#32913=EDGE_CURVE('',#25319,#25318,#19572,.T.);
#32914=EDGE_CURVE('',#25319,#25320,#6685,.T.);
#32915=EDGE_CURVE('',#25320,#25320,#20323,.T.);
#32916=EDGE_CURVE('',#25315,#25319,#19573,.T.);
#32917=EDGE_CURVE('',#25309,#25318,#6686,.T.);
#32918=EDGE_CURVE('',#25308,#25319,#6687,.T.);
#32919=ORIENTED_EDGE('',*,*,#25321,.F.);
#32920=ORIENTED_EDGE('',*,*,#25322,.F.);
#32921=ORIENTED_EDGE('',*,*,#25323,.F.);
#32922=ORIENTED_EDGE('',*,*,#25324,.F.);
#32923=ORIENTED_EDGE('',*,*,#25325,.F.);
#32924=ORIENTED_EDGE('',*,*,#25326,.F.);
#32925=ORIENTED_EDGE('',*,*,#25327,.F.);
#32926=ORIENTED_EDGE('',*,*,#25328,.F.);
#32927=ORIENTED_EDGE('',*,*,#25329,.F.);
#32928=ORIENTED_EDGE('',*,*,#25330,.F.);
#32929=ORIENTED_EDGE('',*,*,#25331,.F.);
#32930=ORIENTED_EDGE('',*,*,#25332,.F.);
#32931=ORIENTED_EDGE('',*,*,#25333,.F.);
#32932=ORIENTED_EDGE('',*,*,#25334,.F.);
#32933=ORIENTED_EDGE('',*,*,#25335,.F.);
#32934=ORIENTED_EDGE('',*,*,#25336,.F.);
#32935=ORIENTED_EDGE('',*,*,#25337,.F.);
#32936=ORIENTED_EDGE('',*,*,#25338,.F.);
#32937=ORIENTED_EDGE('',*,*,#25339,.F.);
#32938=ORIENTED_EDGE('',*,*,#25340,.F.);
#32939=ORIENTED_EDGE('',*,*,#25341,.F.);
#32940=ORIENTED_EDGE('',*,*,#25342,.F.);
#32941=ORIENTED_EDGE('',*,*,#25343,.F.);
#32942=ORIENTED_EDGE('',*,*,#25344,.F.);
#32943=ORIENTED_EDGE('',*,*,#25345,.F.);
#32944=ORIENTED_EDGE('',*,*,#25346,.F.);
#32945=ORIENTED_EDGE('',*,*,#25347,.F.);
#32946=ORIENTED_EDGE('',*,*,#25348,.F.);
#32947=ORIENTED_EDGE('',*,*,#25349,.F.);
#32948=ORIENTED_EDGE('',*,*,#25350,.F.);
#32949=ORIENTED_EDGE('',*,*,#25351,.F.);
#32950=ORIENTED_EDGE('',*,*,#25352,.F.);
#32951=ORIENTED_EDGE('',*,*,#25353,.F.);
#32952=ORIENTED_EDGE('',*,*,#25354,.F.);
#32953=ORIENTED_EDGE('',*,*,#25355,.F.);
#32954=ORIENTED_EDGE('',*,*,#25356,.F.);
#32955=ORIENTED_EDGE('',*,*,#25357,.F.);
#32956=ORIENTED_EDGE('',*,*,#25358,.F.);
#32957=ORIENTED_EDGE('',*,*,#25359,.F.);
#32958=ORIENTED_EDGE('',*,*,#25360,.F.);
#32959=ORIENTED_EDGE('',*,*,#25361,.F.);
#32960=ORIENTED_EDGE('',*,*,#25362,.F.);
#32961=ORIENTED_EDGE('',*,*,#25363,.F.);
#32962=ORIENTED_EDGE('',*,*,#25364,.F.);
#32963=ORIENTED_EDGE('',*,*,#25365,.F.);
#32964=ORIENTED_EDGE('',*,*,#25366,.F.);
#32965=ORIENTED_EDGE('',*,*,#25367,.F.);
#32966=ORIENTED_EDGE('',*,*,#25368,.F.);
#32967=ORIENTED_EDGE('',*,*,#25369,.F.);
#32968=ORIENTED_EDGE('',*,*,#25370,.F.);
#32969=ORIENTED_EDGE('',*,*,#25371,.F.);
#32970=ORIENTED_EDGE('',*,*,#25372,.F.);
#32971=ORIENTED_EDGE('',*,*,#25373,.F.);
#32972=ORIENTED_EDGE('',*,*,#25374,.F.);
#32973=ORIENTED_EDGE('',*,*,#25375,.F.);
#32974=ORIENTED_EDGE('',*,*,#25376,.F.);
#32975=ORIENTED_EDGE('',*,*,#25377,.F.);
#32976=ORIENTED_EDGE('',*,*,#25378,.F.);
#32977=ORIENTED_EDGE('',*,*,#25379,.F.);
#32978=ORIENTED_EDGE('',*,*,#25380,.F.);
#32979=ORIENTED_EDGE('',*,*,#25381,.F.);
#32980=ORIENTED_EDGE('',*,*,#25382,.F.);
#32981=ORIENTED_EDGE('',*,*,#25383,.F.);
#32982=ORIENTED_EDGE('',*,*,#25384,.F.);
#32983=ORIENTED_EDGE('',*,*,#25385,.F.);
#32984=ORIENTED_EDGE('',*,*,#25386,.F.);
#32985=ORIENTED_EDGE('',*,*,#25387,.F.);
#32986=ORIENTED_EDGE('',*,*,#25388,.F.);
#32987=ORIENTED_EDGE('',*,*,#25389,.F.);
#32988=ORIENTED_EDGE('',*,*,#25390,.F.);
#32989=ORIENTED_EDGE('',*,*,#25391,.F.);
#32990=ORIENTED_EDGE('',*,*,#25392,.F.);
#32991=ORIENTED_EDGE('',*,*,#25393,.F.);
#32992=ORIENTED_EDGE('',*,*,#25394,.F.);
#32993=ORIENTED_EDGE('',*,*,#25395,.F.);
#32994=ORIENTED_EDGE('',*,*,#25396,.F.);
#32995=ORIENTED_EDGE('',*,*,#25397,.F.);
#32996=ORIENTED_EDGE('',*,*,#25398,.F.);
#32997=ORIENTED_EDGE('',*,*,#25399,.F.);
#32998=ORIENTED_EDGE('',*,*,#25400,.F.);
#32999=ORIENTED_EDGE('',*,*,#25401,.F.);
#33000=ORIENTED_EDGE('',*,*,#25402,.F.);
#33001=ORIENTED_EDGE('',*,*,#25403,.F.);
#33002=ORIENTED_EDGE('',*,*,#25404,.F.);
#33003=ORIENTED_EDGE('',*,*,#25405,.F.);
#33004=ORIENTED_EDGE('',*,*,#25406,.F.);
#33005=ORIENTED_EDGE('',*,*,#25407,.F.);
#33006=ORIENTED_EDGE('',*,*,#25408,.F.);
#33007=ORIENTED_EDGE('',*,*,#25409,.F.);
#33008=ORIENTED_EDGE('',*,*,#25410,.F.);
#33009=ORIENTED_EDGE('',*,*,#25411,.F.);
#33010=ORIENTED_EDGE('',*,*,#25412,.F.);
#33011=ORIENTED_EDGE('',*,*,#25413,.F.);
#33012=ORIENTED_EDGE('',*,*,#25414,.F.);
#33013=ORIENTED_EDGE('',*,*,#25415,.F.);
#33014=ORIENTED_EDGE('',*,*,#25416,.F.);
#33015=ORIENTED_EDGE('',*,*,#25417,.F.);
#33016=ORIENTED_EDGE('',*,*,#25418,.F.);
#33017=ORIENTED_EDGE('',*,*,#25419,.F.);
#33018=ORIENTED_EDGE('',*,*,#25420,.F.);
#33019=ORIENTED_EDGE('',*,*,#25421,.F.);
#33020=ORIENTED_EDGE('',*,*,#25422,.F.);
#33021=ORIENTED_EDGE('',*,*,#25423,.F.);
#33022=ORIENTED_EDGE('',*,*,#25424,.F.);
#33023=ORIENTED_EDGE('',*,*,#25425,.F.);
#33024=ORIENTED_EDGE('',*,*,#25426,.F.);
#33025=ORIENTED_EDGE('',*,*,#25427,.F.);
#33026=ORIENTED_EDGE('',*,*,#25428,.F.);
#33027=ORIENTED_EDGE('',*,*,#25429,.F.);
#33028=ORIENTED_EDGE('',*,*,#25430,.F.);
#33029=ORIENTED_EDGE('',*,*,#25431,.F.);
#33030=ORIENTED_EDGE('',*,*,#25432,.F.);
#33031=ORIENTED_EDGE('',*,*,#25433,.F.);
#33032=ORIENTED_EDGE('',*,*,#25434,.F.);
#33033=ORIENTED_EDGE('',*,*,#25435,.F.);
#33034=ORIENTED_EDGE('',*,*,#25436,.F.);
#33035=ORIENTED_EDGE('',*,*,#25437,.F.);
#33036=ORIENTED_EDGE('',*,*,#25438,.F.);
#33037=ORIENTED_EDGE('',*,*,#25439,.F.);
#33038=ORIENTED_EDGE('',*,*,#25440,.F.);
#33039=ORIENTED_EDGE('',*,*,#25441,.F.);
#33040=ORIENTED_EDGE('',*,*,#25442,.F.);
#33041=ORIENTED_EDGE('',*,*,#25443,.F.);
#33042=ORIENTED_EDGE('',*,*,#25444,.F.);
#33043=ORIENTED_EDGE('',*,*,#25445,.F.);
#33044=ORIENTED_EDGE('',*,*,#25446,.F.);
#33045=ORIENTED_EDGE('',*,*,#25447,.F.);
#33046=ORIENTED_EDGE('',*,*,#25448,.F.);
#33047=ORIENTED_EDGE('',*,*,#25449,.F.);
#33048=ORIENTED_EDGE('',*,*,#25450,.F.);
#33049=ORIENTED_EDGE('',*,*,#25451,.F.);
#33050=ORIENTED_EDGE('',*,*,#25452,.F.);
#33051=ORIENTED_EDGE('',*,*,#25453,.F.);
#33052=ORIENTED_EDGE('',*,*,#25454,.F.);
#33053=ORIENTED_EDGE('',*,*,#25455,.F.);
#33054=ORIENTED_EDGE('',*,*,#25456,.F.);
#33055=ORIENTED_EDGE('',*,*,#25457,.F.);
#33056=ORIENTED_EDGE('',*,*,#25458,.F.);
#33057=ORIENTED_EDGE('',*,*,#25459,.F.);
#33058=ORIENTED_EDGE('',*,*,#25460,.F.);
#33059=ORIENTED_EDGE('',*,*,#25461,.F.);
#33060=ORIENTED_EDGE('',*,*,#25462,.F.);
#33061=ORIENTED_EDGE('',*,*,#25463,.F.);
#33062=ORIENTED_EDGE('',*,*,#25464,.F.);
#33063=ORIENTED_EDGE('',*,*,#25463,.T.);
#33064=ORIENTED_EDGE('',*,*,#25465,.F.);
#33065=ORIENTED_EDGE('',*,*,#25466,.F.);
#33066=ORIENTED_EDGE('',*,*,#25467,.F.);
#33067=ORIENTED_EDGE('',*,*,#25468,.F.);
#33068=ORIENTED_EDGE('',*,*,#25469,.F.);
#33069=ORIENTED_EDGE('',*,*,#25470,.F.);
#33070=ORIENTED_EDGE('',*,*,#25471,.F.);
#33071=ORIENTED_EDGE('',*,*,#25472,.F.);
#33072=ORIENTED_EDGE('',*,*,#25473,.F.);
#33073=ORIENTED_EDGE('',*,*,#25474,.F.);
#33074=ORIENTED_EDGE('',*,*,#25475,.F.);
#33075=ORIENTED_EDGE('',*,*,#25476,.F.);
#33076=ORIENTED_EDGE('',*,*,#25477,.F.);
#33077=ORIENTED_EDGE('',*,*,#25478,.F.);
#33078=ORIENTED_EDGE('',*,*,#25479,.F.);
#33079=ORIENTED_EDGE('',*,*,#25480,.T.);
#33080=ORIENTED_EDGE('',*,*,#25481,.F.);
#33081=ORIENTED_EDGE('',*,*,#25482,.F.);
#33082=ORIENTED_EDGE('',*,*,#25483,.F.);
#33083=ORIENTED_EDGE('',*,*,#25484,.F.);
#33084=ORIENTED_EDGE('',*,*,#25485,.F.);
#33085=ORIENTED_EDGE('',*,*,#25486,.F.);
#33086=ORIENTED_EDGE('',*,*,#25487,.F.);
#33087=ORIENTED_EDGE('',*,*,#25488,.F.);
#33088=ORIENTED_EDGE('',*,*,#25489,.F.);
#33089=ORIENTED_EDGE('',*,*,#25490,.F.);
#33090=ORIENTED_EDGE('',*,*,#25491,.F.);
#33091=ORIENTED_EDGE('',*,*,#25492,.F.);
#33092=ORIENTED_EDGE('',*,*,#25493,.F.);
#33093=ORIENTED_EDGE('',*,*,#25494,.F.);
#33094=ORIENTED_EDGE('',*,*,#25495,.F.);
#33095=ORIENTED_EDGE('',*,*,#25462,.T.);
#33096=ORIENTED_EDGE('',*,*,#25496,.T.);
#33097=ORIENTED_EDGE('',*,*,#25497,.T.);
#33098=ORIENTED_EDGE('',*,*,#25498,.F.);
#33099=ORIENTED_EDGE('',*,*,#25499,.F.);
#33100=ORIENTED_EDGE('',*,*,#25500,.F.);
#33101=ORIENTED_EDGE('',*,*,#25465,.T.);
#33102=ORIENTED_EDGE('',*,*,#25459,.T.);
#33103=ORIENTED_EDGE('',*,*,#25501,.F.);
#33104=ORIENTED_EDGE('',*,*,#25502,.F.);
#33105=ORIENTED_EDGE('',*,*,#25503,.F.);
#33106=ORIENTED_EDGE('',*,*,#25504,.F.);
#33107=ORIENTED_EDGE('',*,*,#25505,.F.);
#33108=ORIENTED_EDGE('',*,*,#25506,.F.);
#33109=ORIENTED_EDGE('',*,*,#25507,.F.);
#33110=ORIENTED_EDGE('',*,*,#25508,.F.);
#33111=ORIENTED_EDGE('',*,*,#25509,.F.);
#33112=ORIENTED_EDGE('',*,*,#25510,.F.);
#33113=ORIENTED_EDGE('',*,*,#25511,.F.);
#33114=ORIENTED_EDGE('',*,*,#25512,.F.);
#33115=ORIENTED_EDGE('',*,*,#25513,.F.);
#33116=ORIENTED_EDGE('',*,*,#25514,.F.);
#33117=ORIENTED_EDGE('',*,*,#25515,.F.);
#33118=ORIENTED_EDGE('',*,*,#25516,.T.);
#33119=ORIENTED_EDGE('',*,*,#25517,.F.);
#33120=ORIENTED_EDGE('',*,*,#25518,.F.);
#33121=ORIENTED_EDGE('',*,*,#25519,.F.);
#33122=ORIENTED_EDGE('',*,*,#25520,.F.);
#33123=ORIENTED_EDGE('',*,*,#25521,.F.);
#33124=ORIENTED_EDGE('',*,*,#25522,.F.);
#33125=ORIENTED_EDGE('',*,*,#25523,.F.);
#33126=ORIENTED_EDGE('',*,*,#25524,.F.);
#33127=ORIENTED_EDGE('',*,*,#25525,.F.);
#33128=ORIENTED_EDGE('',*,*,#25526,.F.);
#33129=ORIENTED_EDGE('',*,*,#25527,.F.);
#33130=ORIENTED_EDGE('',*,*,#25528,.F.);
#33131=ORIENTED_EDGE('',*,*,#25529,.F.);
#33132=ORIENTED_EDGE('',*,*,#25530,.F.);
#33133=ORIENTED_EDGE('',*,*,#25531,.F.);
#33134=ORIENTED_EDGE('',*,*,#25458,.T.);
#33135=ORIENTED_EDGE('',*,*,#25532,.T.);
#33136=ORIENTED_EDGE('',*,*,#25533,.T.);
#33137=ORIENTED_EDGE('',*,*,#25534,.F.);
#33138=ORIENTED_EDGE('',*,*,#25535,.F.);
#33139=ORIENTED_EDGE('',*,*,#25536,.F.);
#33140=ORIENTED_EDGE('',*,*,#25501,.T.);
#33141=ORIENTED_EDGE('',*,*,#25455,.T.);
#33142=ORIENTED_EDGE('',*,*,#25537,.F.);
#33143=ORIENTED_EDGE('',*,*,#25538,.F.);
#33144=ORIENTED_EDGE('',*,*,#25539,.F.);
#33145=ORIENTED_EDGE('',*,*,#25540,.F.);
#33146=ORIENTED_EDGE('',*,*,#25541,.F.);
#33147=ORIENTED_EDGE('',*,*,#25542,.F.);
#33148=ORIENTED_EDGE('',*,*,#25543,.F.);
#33149=ORIENTED_EDGE('',*,*,#25544,.F.);
#33150=ORIENTED_EDGE('',*,*,#25545,.F.);
#33151=ORIENTED_EDGE('',*,*,#25546,.F.);
#33152=ORIENTED_EDGE('',*,*,#25547,.F.);
#33153=ORIENTED_EDGE('',*,*,#25548,.F.);
#33154=ORIENTED_EDGE('',*,*,#25549,.F.);
#33155=ORIENTED_EDGE('',*,*,#25550,.F.);
#33156=ORIENTED_EDGE('',*,*,#25551,.F.);
#33157=ORIENTED_EDGE('',*,*,#25552,.T.);
#33158=ORIENTED_EDGE('',*,*,#25553,.F.);
#33159=ORIENTED_EDGE('',*,*,#25554,.F.);
#33160=ORIENTED_EDGE('',*,*,#25555,.F.);
#33161=ORIENTED_EDGE('',*,*,#25556,.F.);
#33162=ORIENTED_EDGE('',*,*,#25557,.F.);
#33163=ORIENTED_EDGE('',*,*,#25558,.F.);
#33164=ORIENTED_EDGE('',*,*,#25559,.F.);
#33165=ORIENTED_EDGE('',*,*,#25560,.F.);
#33166=ORIENTED_EDGE('',*,*,#25561,.F.);
#33167=ORIENTED_EDGE('',*,*,#25562,.F.);
#33168=ORIENTED_EDGE('',*,*,#25563,.F.);
#33169=ORIENTED_EDGE('',*,*,#25564,.F.);
#33170=ORIENTED_EDGE('',*,*,#25565,.F.);
#33171=ORIENTED_EDGE('',*,*,#25566,.F.);
#33172=ORIENTED_EDGE('',*,*,#25567,.F.);
#33173=ORIENTED_EDGE('',*,*,#25454,.T.);
#33174=ORIENTED_EDGE('',*,*,#25568,.T.);
#33175=ORIENTED_EDGE('',*,*,#25569,.T.);
#33176=ORIENTED_EDGE('',*,*,#25570,.F.);
#33177=ORIENTED_EDGE('',*,*,#25571,.F.);
#33178=ORIENTED_EDGE('',*,*,#25572,.F.);
#33179=ORIENTED_EDGE('',*,*,#25537,.T.);
#33180=ORIENTED_EDGE('',*,*,#25451,.T.);
#33181=ORIENTED_EDGE('',*,*,#25573,.F.);
#33182=ORIENTED_EDGE('',*,*,#25574,.F.);
#33183=ORIENTED_EDGE('',*,*,#25575,.F.);
#33184=ORIENTED_EDGE('',*,*,#25576,.F.);
#33185=ORIENTED_EDGE('',*,*,#25577,.F.);
#33186=ORIENTED_EDGE('',*,*,#25578,.F.);
#33187=ORIENTED_EDGE('',*,*,#25579,.F.);
#33188=ORIENTED_EDGE('',*,*,#25580,.F.);
#33189=ORIENTED_EDGE('',*,*,#25581,.F.);
#33190=ORIENTED_EDGE('',*,*,#25582,.F.);
#33191=ORIENTED_EDGE('',*,*,#25583,.F.);
#33192=ORIENTED_EDGE('',*,*,#25584,.F.);
#33193=ORIENTED_EDGE('',*,*,#25585,.F.);
#33194=ORIENTED_EDGE('',*,*,#25586,.F.);
#33195=ORIENTED_EDGE('',*,*,#25587,.F.);
#33196=ORIENTED_EDGE('',*,*,#25588,.T.);
#33197=ORIENTED_EDGE('',*,*,#25589,.F.);
#33198=ORIENTED_EDGE('',*,*,#25590,.F.);
#33199=ORIENTED_EDGE('',*,*,#25591,.F.);
#33200=ORIENTED_EDGE('',*,*,#25592,.F.);
#33201=ORIENTED_EDGE('',*,*,#25593,.F.);
#33202=ORIENTED_EDGE('',*,*,#25594,.F.);
#33203=ORIENTED_EDGE('',*,*,#25595,.F.);
#33204=ORIENTED_EDGE('',*,*,#25596,.F.);
#33205=ORIENTED_EDGE('',*,*,#25597,.F.);
#33206=ORIENTED_EDGE('',*,*,#25598,.F.);
#33207=ORIENTED_EDGE('',*,*,#25599,.F.);
#33208=ORIENTED_EDGE('',*,*,#25600,.F.);
#33209=ORIENTED_EDGE('',*,*,#25601,.F.);
#33210=ORIENTED_EDGE('',*,*,#25602,.F.);
#33211=ORIENTED_EDGE('',*,*,#25603,.F.);
#33212=ORIENTED_EDGE('',*,*,#25450,.T.);
#33213=ORIENTED_EDGE('',*,*,#25604,.T.);
#33214=ORIENTED_EDGE('',*,*,#25605,.T.);
#33215=ORIENTED_EDGE('',*,*,#25606,.F.);
#33216=ORIENTED_EDGE('',*,*,#25607,.F.);
#33217=ORIENTED_EDGE('',*,*,#25608,.F.);
#33218=ORIENTED_EDGE('',*,*,#25573,.T.);
#33219=ORIENTED_EDGE('',*,*,#25447,.T.);
#33220=ORIENTED_EDGE('',*,*,#25609,.F.);
#33221=ORIENTED_EDGE('',*,*,#25610,.F.);
#33222=ORIENTED_EDGE('',*,*,#25611,.F.);
#33223=ORIENTED_EDGE('',*,*,#25612,.F.);
#33224=ORIENTED_EDGE('',*,*,#25613,.F.);
#33225=ORIENTED_EDGE('',*,*,#25614,.F.);
#33226=ORIENTED_EDGE('',*,*,#25615,.F.);
#33227=ORIENTED_EDGE('',*,*,#25616,.F.);
#33228=ORIENTED_EDGE('',*,*,#25617,.F.);
#33229=ORIENTED_EDGE('',*,*,#25618,.F.);
#33230=ORIENTED_EDGE('',*,*,#25619,.F.);
#33231=ORIENTED_EDGE('',*,*,#25620,.F.);
#33232=ORIENTED_EDGE('',*,*,#25621,.F.);
#33233=ORIENTED_EDGE('',*,*,#25622,.F.);
#33234=ORIENTED_EDGE('',*,*,#25623,.F.);
#33235=ORIENTED_EDGE('',*,*,#25624,.T.);
#33236=ORIENTED_EDGE('',*,*,#25625,.F.);
#33237=ORIENTED_EDGE('',*,*,#25626,.F.);
#33238=ORIENTED_EDGE('',*,*,#25627,.F.);
#33239=ORIENTED_EDGE('',*,*,#25628,.F.);
#33240=ORIENTED_EDGE('',*,*,#25629,.F.);
#33241=ORIENTED_EDGE('',*,*,#25630,.F.);
#33242=ORIENTED_EDGE('',*,*,#25631,.F.);
#33243=ORIENTED_EDGE('',*,*,#25632,.F.);
#33244=ORIENTED_EDGE('',*,*,#25633,.F.);
#33245=ORIENTED_EDGE('',*,*,#25634,.F.);
#33246=ORIENTED_EDGE('',*,*,#25635,.F.);
#33247=ORIENTED_EDGE('',*,*,#25636,.F.);
#33248=ORIENTED_EDGE('',*,*,#25637,.F.);
#33249=ORIENTED_EDGE('',*,*,#25638,.F.);
#33250=ORIENTED_EDGE('',*,*,#25639,.F.);
#33251=ORIENTED_EDGE('',*,*,#25446,.T.);
#33252=ORIENTED_EDGE('',*,*,#25640,.T.);
#33253=ORIENTED_EDGE('',*,*,#25641,.T.);
#33254=ORIENTED_EDGE('',*,*,#25642,.F.);
#33255=ORIENTED_EDGE('',*,*,#25643,.F.);
#33256=ORIENTED_EDGE('',*,*,#25644,.F.);
#33257=ORIENTED_EDGE('',*,*,#25609,.T.);
#33258=ORIENTED_EDGE('',*,*,#25443,.T.);
#33259=ORIENTED_EDGE('',*,*,#25645,.F.);
#33260=ORIENTED_EDGE('',*,*,#25646,.F.);
#33261=ORIENTED_EDGE('',*,*,#25647,.F.);
#33262=ORIENTED_EDGE('',*,*,#25648,.F.);
#33263=ORIENTED_EDGE('',*,*,#25649,.F.);
#33264=ORIENTED_EDGE('',*,*,#25650,.F.);
#33265=ORIENTED_EDGE('',*,*,#25651,.F.);
#33266=ORIENTED_EDGE('',*,*,#25652,.F.);
#33267=ORIENTED_EDGE('',*,*,#25653,.F.);
#33268=ORIENTED_EDGE('',*,*,#25654,.F.);
#33269=ORIENTED_EDGE('',*,*,#25655,.F.);
#33270=ORIENTED_EDGE('',*,*,#25656,.F.);
#33271=ORIENTED_EDGE('',*,*,#25657,.F.);
#33272=ORIENTED_EDGE('',*,*,#25658,.F.);
#33273=ORIENTED_EDGE('',*,*,#25659,.F.);
#33274=ORIENTED_EDGE('',*,*,#25660,.T.);
#33275=ORIENTED_EDGE('',*,*,#25661,.F.);
#33276=ORIENTED_EDGE('',*,*,#25662,.F.);
#33277=ORIENTED_EDGE('',*,*,#25663,.F.);
#33278=ORIENTED_EDGE('',*,*,#25664,.F.);
#33279=ORIENTED_EDGE('',*,*,#25665,.F.);
#33280=ORIENTED_EDGE('',*,*,#25666,.F.);
#33281=ORIENTED_EDGE('',*,*,#25667,.F.);
#33282=ORIENTED_EDGE('',*,*,#25668,.F.);
#33283=ORIENTED_EDGE('',*,*,#25669,.F.);
#33284=ORIENTED_EDGE('',*,*,#25670,.F.);
#33285=ORIENTED_EDGE('',*,*,#25671,.F.);
#33286=ORIENTED_EDGE('',*,*,#25672,.F.);
#33287=ORIENTED_EDGE('',*,*,#25673,.F.);
#33288=ORIENTED_EDGE('',*,*,#25674,.F.);
#33289=ORIENTED_EDGE('',*,*,#25675,.F.);
#33290=ORIENTED_EDGE('',*,*,#25442,.T.);
#33291=ORIENTED_EDGE('',*,*,#25676,.T.);
#33292=ORIENTED_EDGE('',*,*,#25677,.T.);
#33293=ORIENTED_EDGE('',*,*,#25678,.F.);
#33294=ORIENTED_EDGE('',*,*,#25679,.F.);
#33295=ORIENTED_EDGE('',*,*,#25680,.F.);
#33296=ORIENTED_EDGE('',*,*,#25645,.T.);
#33297=ORIENTED_EDGE('',*,*,#25439,.T.);
#33298=ORIENTED_EDGE('',*,*,#25681,.F.);
#33299=ORIENTED_EDGE('',*,*,#25682,.F.);
#33300=ORIENTED_EDGE('',*,*,#25683,.F.);
#33301=ORIENTED_EDGE('',*,*,#25684,.F.);
#33302=ORIENTED_EDGE('',*,*,#25685,.F.);
#33303=ORIENTED_EDGE('',*,*,#25686,.F.);
#33304=ORIENTED_EDGE('',*,*,#25687,.F.);
#33305=ORIENTED_EDGE('',*,*,#25688,.F.);
#33306=ORIENTED_EDGE('',*,*,#25689,.F.);
#33307=ORIENTED_EDGE('',*,*,#25690,.F.);
#33308=ORIENTED_EDGE('',*,*,#25691,.F.);
#33309=ORIENTED_EDGE('',*,*,#25692,.F.);
#33310=ORIENTED_EDGE('',*,*,#25693,.F.);
#33311=ORIENTED_EDGE('',*,*,#25694,.F.);
#33312=ORIENTED_EDGE('',*,*,#25695,.F.);
#33313=ORIENTED_EDGE('',*,*,#25696,.T.);
#33314=ORIENTED_EDGE('',*,*,#25697,.F.);
#33315=ORIENTED_EDGE('',*,*,#25698,.F.);
#33316=ORIENTED_EDGE('',*,*,#25699,.F.);
#33317=ORIENTED_EDGE('',*,*,#25700,.F.);
#33318=ORIENTED_EDGE('',*,*,#25701,.F.);
#33319=ORIENTED_EDGE('',*,*,#25702,.F.);
#33320=ORIENTED_EDGE('',*,*,#25703,.F.);
#33321=ORIENTED_EDGE('',*,*,#25704,.F.);
#33322=ORIENTED_EDGE('',*,*,#25705,.F.);
#33323=ORIENTED_EDGE('',*,*,#25706,.F.);
#33324=ORIENTED_EDGE('',*,*,#25707,.F.);
#33325=ORIENTED_EDGE('',*,*,#25708,.F.);
#33326=ORIENTED_EDGE('',*,*,#25709,.F.);
#33327=ORIENTED_EDGE('',*,*,#25710,.F.);
#33328=ORIENTED_EDGE('',*,*,#25711,.F.);
#33329=ORIENTED_EDGE('',*,*,#25438,.T.);
#33330=ORIENTED_EDGE('',*,*,#25712,.T.);
#33331=ORIENTED_EDGE('',*,*,#25713,.T.);
#33332=ORIENTED_EDGE('',*,*,#25714,.F.);
#33333=ORIENTED_EDGE('',*,*,#25715,.F.);
#33334=ORIENTED_EDGE('',*,*,#25716,.F.);
#33335=ORIENTED_EDGE('',*,*,#25681,.T.);
#33336=ORIENTED_EDGE('',*,*,#25435,.T.);
#33337=ORIENTED_EDGE('',*,*,#25717,.F.);
#33338=ORIENTED_EDGE('',*,*,#25718,.F.);
#33339=ORIENTED_EDGE('',*,*,#25719,.F.);
#33340=ORIENTED_EDGE('',*,*,#25720,.F.);
#33341=ORIENTED_EDGE('',*,*,#25721,.F.);
#33342=ORIENTED_EDGE('',*,*,#25722,.F.);
#33343=ORIENTED_EDGE('',*,*,#25723,.F.);
#33344=ORIENTED_EDGE('',*,*,#25724,.F.);
#33345=ORIENTED_EDGE('',*,*,#25725,.F.);
#33346=ORIENTED_EDGE('',*,*,#25726,.F.);
#33347=ORIENTED_EDGE('',*,*,#25727,.F.);
#33348=ORIENTED_EDGE('',*,*,#25728,.F.);
#33349=ORIENTED_EDGE('',*,*,#25729,.F.);
#33350=ORIENTED_EDGE('',*,*,#25730,.F.);
#33351=ORIENTED_EDGE('',*,*,#25731,.F.);
#33352=ORIENTED_EDGE('',*,*,#25732,.T.);
#33353=ORIENTED_EDGE('',*,*,#25733,.F.);
#33354=ORIENTED_EDGE('',*,*,#25734,.F.);
#33355=ORIENTED_EDGE('',*,*,#25735,.F.);
#33356=ORIENTED_EDGE('',*,*,#25736,.F.);
#33357=ORIENTED_EDGE('',*,*,#25737,.F.);
#33358=ORIENTED_EDGE('',*,*,#25738,.F.);
#33359=ORIENTED_EDGE('',*,*,#25739,.F.);
#33360=ORIENTED_EDGE('',*,*,#25740,.F.);
#33361=ORIENTED_EDGE('',*,*,#25741,.F.);
#33362=ORIENTED_EDGE('',*,*,#25742,.F.);
#33363=ORIENTED_EDGE('',*,*,#25743,.F.);
#33364=ORIENTED_EDGE('',*,*,#25744,.F.);
#33365=ORIENTED_EDGE('',*,*,#25745,.F.);
#33366=ORIENTED_EDGE('',*,*,#25746,.F.);
#33367=ORIENTED_EDGE('',*,*,#25747,.F.);
#33368=ORIENTED_EDGE('',*,*,#25434,.T.);
#33369=ORIENTED_EDGE('',*,*,#25748,.T.);
#33370=ORIENTED_EDGE('',*,*,#25749,.T.);
#33371=ORIENTED_EDGE('',*,*,#25750,.F.);
#33372=ORIENTED_EDGE('',*,*,#25751,.F.);
#33373=ORIENTED_EDGE('',*,*,#25752,.F.);
#33374=ORIENTED_EDGE('',*,*,#25717,.T.);
#33375=ORIENTED_EDGE('',*,*,#25431,.T.);
#33376=ORIENTED_EDGE('',*,*,#25753,.F.);
#33377=ORIENTED_EDGE('',*,*,#25754,.F.);
#33378=ORIENTED_EDGE('',*,*,#25755,.F.);
#33379=ORIENTED_EDGE('',*,*,#25756,.F.);
#33380=ORIENTED_EDGE('',*,*,#25757,.F.);
#33381=ORIENTED_EDGE('',*,*,#25758,.F.);
#33382=ORIENTED_EDGE('',*,*,#25759,.F.);
#33383=ORIENTED_EDGE('',*,*,#25760,.F.);
#33384=ORIENTED_EDGE('',*,*,#25761,.F.);
#33385=ORIENTED_EDGE('',*,*,#25762,.F.);
#33386=ORIENTED_EDGE('',*,*,#25763,.F.);
#33387=ORIENTED_EDGE('',*,*,#25764,.F.);
#33388=ORIENTED_EDGE('',*,*,#25765,.F.);
#33389=ORIENTED_EDGE('',*,*,#25766,.F.);
#33390=ORIENTED_EDGE('',*,*,#25767,.F.);
#33391=ORIENTED_EDGE('',*,*,#25768,.T.);
#33392=ORIENTED_EDGE('',*,*,#25769,.F.);
#33393=ORIENTED_EDGE('',*,*,#25770,.F.);
#33394=ORIENTED_EDGE('',*,*,#25771,.F.);
#33395=ORIENTED_EDGE('',*,*,#25772,.F.);
#33396=ORIENTED_EDGE('',*,*,#25773,.F.);
#33397=ORIENTED_EDGE('',*,*,#25774,.F.);
#33398=ORIENTED_EDGE('',*,*,#25775,.F.);
#33399=ORIENTED_EDGE('',*,*,#25776,.F.);
#33400=ORIENTED_EDGE('',*,*,#25777,.F.);
#33401=ORIENTED_EDGE('',*,*,#25778,.F.);
#33402=ORIENTED_EDGE('',*,*,#25779,.F.);
#33403=ORIENTED_EDGE('',*,*,#25780,.F.);
#33404=ORIENTED_EDGE('',*,*,#25781,.F.);
#33405=ORIENTED_EDGE('',*,*,#25782,.F.);
#33406=ORIENTED_EDGE('',*,*,#25783,.F.);
#33407=ORIENTED_EDGE('',*,*,#25430,.T.);
#33408=ORIENTED_EDGE('',*,*,#25784,.T.);
#33409=ORIENTED_EDGE('',*,*,#25785,.T.);
#33410=ORIENTED_EDGE('',*,*,#25786,.F.);
#33411=ORIENTED_EDGE('',*,*,#25787,.F.);
#33412=ORIENTED_EDGE('',*,*,#25788,.F.);
#33413=ORIENTED_EDGE('',*,*,#25753,.T.);
#33414=ORIENTED_EDGE('',*,*,#25427,.T.);
#33415=ORIENTED_EDGE('',*,*,#25789,.F.);
#33416=ORIENTED_EDGE('',*,*,#25790,.F.);
#33417=ORIENTED_EDGE('',*,*,#25791,.F.);
#33418=ORIENTED_EDGE('',*,*,#25792,.F.);
#33419=ORIENTED_EDGE('',*,*,#25793,.F.);
#33420=ORIENTED_EDGE('',*,*,#25794,.F.);
#33421=ORIENTED_EDGE('',*,*,#25795,.F.);
#33422=ORIENTED_EDGE('',*,*,#25796,.F.);
#33423=ORIENTED_EDGE('',*,*,#25797,.F.);
#33424=ORIENTED_EDGE('',*,*,#25798,.F.);
#33425=ORIENTED_EDGE('',*,*,#25799,.F.);
#33426=ORIENTED_EDGE('',*,*,#25800,.F.);
#33427=ORIENTED_EDGE('',*,*,#25801,.F.);
#33428=ORIENTED_EDGE('',*,*,#25802,.F.);
#33429=ORIENTED_EDGE('',*,*,#25803,.F.);
#33430=ORIENTED_EDGE('',*,*,#25804,.T.);
#33431=ORIENTED_EDGE('',*,*,#25805,.F.);
#33432=ORIENTED_EDGE('',*,*,#25806,.F.);
#33433=ORIENTED_EDGE('',*,*,#25807,.F.);
#33434=ORIENTED_EDGE('',*,*,#25808,.F.);
#33435=ORIENTED_EDGE('',*,*,#25809,.F.);
#33436=ORIENTED_EDGE('',*,*,#25810,.F.);
#33437=ORIENTED_EDGE('',*,*,#25811,.F.);
#33438=ORIENTED_EDGE('',*,*,#25812,.F.);
#33439=ORIENTED_EDGE('',*,*,#25813,.F.);
#33440=ORIENTED_EDGE('',*,*,#25814,.F.);
#33441=ORIENTED_EDGE('',*,*,#25815,.F.);
#33442=ORIENTED_EDGE('',*,*,#25816,.F.);
#33443=ORIENTED_EDGE('',*,*,#25817,.F.);
#33444=ORIENTED_EDGE('',*,*,#25818,.F.);
#33445=ORIENTED_EDGE('',*,*,#25819,.F.);
#33446=ORIENTED_EDGE('',*,*,#25426,.T.);
#33447=ORIENTED_EDGE('',*,*,#25820,.T.);
#33448=ORIENTED_EDGE('',*,*,#25821,.T.);
#33449=ORIENTED_EDGE('',*,*,#25822,.F.);
#33450=ORIENTED_EDGE('',*,*,#25823,.F.);
#33451=ORIENTED_EDGE('',*,*,#25824,.F.);
#33452=ORIENTED_EDGE('',*,*,#25789,.T.);
#33453=ORIENTED_EDGE('',*,*,#25423,.T.);
#33454=ORIENTED_EDGE('',*,*,#25825,.F.);
#33455=ORIENTED_EDGE('',*,*,#25826,.F.);
#33456=ORIENTED_EDGE('',*,*,#25827,.F.);
#33457=ORIENTED_EDGE('',*,*,#25828,.F.);
#33458=ORIENTED_EDGE('',*,*,#25829,.F.);
#33459=ORIENTED_EDGE('',*,*,#25830,.F.);
#33460=ORIENTED_EDGE('',*,*,#25831,.F.);
#33461=ORIENTED_EDGE('',*,*,#25832,.F.);
#33462=ORIENTED_EDGE('',*,*,#25833,.F.);
#33463=ORIENTED_EDGE('',*,*,#25834,.F.);
#33464=ORIENTED_EDGE('',*,*,#25835,.F.);
#33465=ORIENTED_EDGE('',*,*,#25836,.F.);
#33466=ORIENTED_EDGE('',*,*,#25837,.F.);
#33467=ORIENTED_EDGE('',*,*,#25838,.F.);
#33468=ORIENTED_EDGE('',*,*,#25839,.F.);
#33469=ORIENTED_EDGE('',*,*,#25840,.T.);
#33470=ORIENTED_EDGE('',*,*,#25841,.F.);
#33471=ORIENTED_EDGE('',*,*,#25842,.F.);
#33472=ORIENTED_EDGE('',*,*,#25843,.F.);
#33473=ORIENTED_EDGE('',*,*,#25844,.F.);
#33474=ORIENTED_EDGE('',*,*,#25845,.F.);
#33475=ORIENTED_EDGE('',*,*,#25846,.F.);
#33476=ORIENTED_EDGE('',*,*,#25847,.F.);
#33477=ORIENTED_EDGE('',*,*,#25848,.F.);
#33478=ORIENTED_EDGE('',*,*,#25849,.F.);
#33479=ORIENTED_EDGE('',*,*,#25850,.F.);
#33480=ORIENTED_EDGE('',*,*,#25851,.F.);
#33481=ORIENTED_EDGE('',*,*,#25852,.F.);
#33482=ORIENTED_EDGE('',*,*,#25853,.F.);
#33483=ORIENTED_EDGE('',*,*,#25854,.F.);
#33484=ORIENTED_EDGE('',*,*,#25855,.F.);
#33485=ORIENTED_EDGE('',*,*,#25422,.T.);
#33486=ORIENTED_EDGE('',*,*,#25856,.T.);
#33487=ORIENTED_EDGE('',*,*,#25857,.T.);
#33488=ORIENTED_EDGE('',*,*,#25858,.F.);
#33489=ORIENTED_EDGE('',*,*,#25859,.F.);
#33490=ORIENTED_EDGE('',*,*,#25860,.F.);
#33491=ORIENTED_EDGE('',*,*,#25825,.T.);
#33492=ORIENTED_EDGE('',*,*,#25419,.T.);
#33493=ORIENTED_EDGE('',*,*,#25861,.F.);
#33494=ORIENTED_EDGE('',*,*,#25862,.F.);
#33495=ORIENTED_EDGE('',*,*,#25863,.F.);
#33496=ORIENTED_EDGE('',*,*,#25864,.F.);
#33497=ORIENTED_EDGE('',*,*,#25865,.F.);
#33498=ORIENTED_EDGE('',*,*,#25866,.F.);
#33499=ORIENTED_EDGE('',*,*,#25867,.F.);
#33500=ORIENTED_EDGE('',*,*,#25868,.F.);
#33501=ORIENTED_EDGE('',*,*,#25869,.F.);
#33502=ORIENTED_EDGE('',*,*,#25870,.F.);
#33503=ORIENTED_EDGE('',*,*,#25871,.F.);
#33504=ORIENTED_EDGE('',*,*,#25872,.F.);
#33505=ORIENTED_EDGE('',*,*,#25873,.F.);
#33506=ORIENTED_EDGE('',*,*,#25874,.F.);
#33507=ORIENTED_EDGE('',*,*,#25875,.F.);
#33508=ORIENTED_EDGE('',*,*,#25876,.T.);
#33509=ORIENTED_EDGE('',*,*,#25877,.F.);
#33510=ORIENTED_EDGE('',*,*,#25878,.F.);
#33511=ORIENTED_EDGE('',*,*,#25879,.F.);
#33512=ORIENTED_EDGE('',*,*,#25880,.F.);
#33513=ORIENTED_EDGE('',*,*,#25881,.F.);
#33514=ORIENTED_EDGE('',*,*,#25882,.F.);
#33515=ORIENTED_EDGE('',*,*,#25883,.F.);
#33516=ORIENTED_EDGE('',*,*,#25884,.F.);
#33517=ORIENTED_EDGE('',*,*,#25885,.F.);
#33518=ORIENTED_EDGE('',*,*,#25886,.F.);
#33519=ORIENTED_EDGE('',*,*,#25887,.F.);
#33520=ORIENTED_EDGE('',*,*,#25888,.F.);
#33521=ORIENTED_EDGE('',*,*,#25889,.F.);
#33522=ORIENTED_EDGE('',*,*,#25890,.F.);
#33523=ORIENTED_EDGE('',*,*,#25891,.F.);
#33524=ORIENTED_EDGE('',*,*,#25418,.T.);
#33525=ORIENTED_EDGE('',*,*,#25892,.T.);
#33526=ORIENTED_EDGE('',*,*,#25893,.T.);
#33527=ORIENTED_EDGE('',*,*,#25894,.F.);
#33528=ORIENTED_EDGE('',*,*,#25895,.F.);
#33529=ORIENTED_EDGE('',*,*,#25896,.F.);
#33530=ORIENTED_EDGE('',*,*,#25861,.T.);
#33531=ORIENTED_EDGE('',*,*,#25415,.T.);
#33532=ORIENTED_EDGE('',*,*,#25897,.F.);
#33533=ORIENTED_EDGE('',*,*,#25898,.F.);
#33534=ORIENTED_EDGE('',*,*,#25899,.F.);
#33535=ORIENTED_EDGE('',*,*,#25900,.F.);
#33536=ORIENTED_EDGE('',*,*,#25901,.F.);
#33537=ORIENTED_EDGE('',*,*,#25902,.F.);
#33538=ORIENTED_EDGE('',*,*,#25903,.F.);
#33539=ORIENTED_EDGE('',*,*,#25904,.F.);
#33540=ORIENTED_EDGE('',*,*,#25905,.F.);
#33541=ORIENTED_EDGE('',*,*,#25906,.F.);
#33542=ORIENTED_EDGE('',*,*,#25907,.F.);
#33543=ORIENTED_EDGE('',*,*,#25908,.F.);
#33544=ORIENTED_EDGE('',*,*,#25909,.F.);
#33545=ORIENTED_EDGE('',*,*,#25910,.F.);
#33546=ORIENTED_EDGE('',*,*,#25911,.F.);
#33547=ORIENTED_EDGE('',*,*,#25912,.T.);
#33548=ORIENTED_EDGE('',*,*,#25913,.F.);
#33549=ORIENTED_EDGE('',*,*,#25914,.F.);
#33550=ORIENTED_EDGE('',*,*,#25915,.F.);
#33551=ORIENTED_EDGE('',*,*,#25916,.F.);
#33552=ORIENTED_EDGE('',*,*,#25917,.F.);
#33553=ORIENTED_EDGE('',*,*,#25918,.F.);
#33554=ORIENTED_EDGE('',*,*,#25919,.F.);
#33555=ORIENTED_EDGE('',*,*,#25920,.F.);
#33556=ORIENTED_EDGE('',*,*,#25921,.F.);
#33557=ORIENTED_EDGE('',*,*,#25922,.F.);
#33558=ORIENTED_EDGE('',*,*,#25923,.F.);
#33559=ORIENTED_EDGE('',*,*,#25924,.F.);
#33560=ORIENTED_EDGE('',*,*,#25925,.F.);
#33561=ORIENTED_EDGE('',*,*,#25926,.F.);
#33562=ORIENTED_EDGE('',*,*,#25927,.F.);
#33563=ORIENTED_EDGE('',*,*,#25414,.T.);
#33564=ORIENTED_EDGE('',*,*,#25928,.T.);
#33565=ORIENTED_EDGE('',*,*,#25929,.T.);
#33566=ORIENTED_EDGE('',*,*,#25930,.F.);
#33567=ORIENTED_EDGE('',*,*,#25931,.F.);
#33568=ORIENTED_EDGE('',*,*,#25932,.F.);
#33569=ORIENTED_EDGE('',*,*,#25897,.T.);
#33570=ORIENTED_EDGE('',*,*,#25411,.T.);
#33571=ORIENTED_EDGE('',*,*,#25933,.F.);
#33572=ORIENTED_EDGE('',*,*,#25934,.F.);
#33573=ORIENTED_EDGE('',*,*,#25935,.F.);
#33574=ORIENTED_EDGE('',*,*,#25936,.F.);
#33575=ORIENTED_EDGE('',*,*,#25937,.F.);
#33576=ORIENTED_EDGE('',*,*,#25938,.F.);
#33577=ORIENTED_EDGE('',*,*,#25939,.F.);
#33578=ORIENTED_EDGE('',*,*,#25940,.F.);
#33579=ORIENTED_EDGE('',*,*,#25941,.F.);
#33580=ORIENTED_EDGE('',*,*,#25942,.F.);
#33581=ORIENTED_EDGE('',*,*,#25943,.F.);
#33582=ORIENTED_EDGE('',*,*,#25944,.F.);
#33583=ORIENTED_EDGE('',*,*,#25945,.F.);
#33584=ORIENTED_EDGE('',*,*,#25946,.F.);
#33585=ORIENTED_EDGE('',*,*,#25947,.F.);
#33586=ORIENTED_EDGE('',*,*,#25948,.T.);
#33587=ORIENTED_EDGE('',*,*,#25949,.F.);
#33588=ORIENTED_EDGE('',*,*,#25950,.F.);
#33589=ORIENTED_EDGE('',*,*,#25951,.F.);
#33590=ORIENTED_EDGE('',*,*,#25952,.F.);
#33591=ORIENTED_EDGE('',*,*,#25953,.F.);
#33592=ORIENTED_EDGE('',*,*,#25954,.F.);
#33593=ORIENTED_EDGE('',*,*,#25955,.F.);
#33594=ORIENTED_EDGE('',*,*,#25956,.F.);
#33595=ORIENTED_EDGE('',*,*,#25957,.F.);
#33596=ORIENTED_EDGE('',*,*,#25958,.F.);
#33597=ORIENTED_EDGE('',*,*,#25959,.F.);
#33598=ORIENTED_EDGE('',*,*,#25960,.F.);
#33599=ORIENTED_EDGE('',*,*,#25961,.F.);
#33600=ORIENTED_EDGE('',*,*,#25962,.F.);
#33601=ORIENTED_EDGE('',*,*,#25963,.F.);
#33602=ORIENTED_EDGE('',*,*,#25410,.T.);
#33603=ORIENTED_EDGE('',*,*,#25964,.T.);
#33604=ORIENTED_EDGE('',*,*,#25965,.T.);
#33605=ORIENTED_EDGE('',*,*,#25966,.F.);
#33606=ORIENTED_EDGE('',*,*,#25967,.F.);
#33607=ORIENTED_EDGE('',*,*,#25968,.F.);
#33608=ORIENTED_EDGE('',*,*,#25933,.T.);
#33609=ORIENTED_EDGE('',*,*,#25407,.T.);
#33610=ORIENTED_EDGE('',*,*,#25969,.F.);
#33611=ORIENTED_EDGE('',*,*,#25970,.F.);
#33612=ORIENTED_EDGE('',*,*,#25971,.F.);
#33613=ORIENTED_EDGE('',*,*,#25972,.F.);
#33614=ORIENTED_EDGE('',*,*,#25973,.F.);
#33615=ORIENTED_EDGE('',*,*,#25974,.F.);
#33616=ORIENTED_EDGE('',*,*,#25975,.F.);
#33617=ORIENTED_EDGE('',*,*,#25976,.F.);
#33618=ORIENTED_EDGE('',*,*,#25977,.F.);
#33619=ORIENTED_EDGE('',*,*,#25978,.F.);
#33620=ORIENTED_EDGE('',*,*,#25979,.F.);
#33621=ORIENTED_EDGE('',*,*,#25980,.F.);
#33622=ORIENTED_EDGE('',*,*,#25981,.F.);
#33623=ORIENTED_EDGE('',*,*,#25982,.F.);
#33624=ORIENTED_EDGE('',*,*,#25983,.F.);
#33625=ORIENTED_EDGE('',*,*,#25984,.T.);
#33626=ORIENTED_EDGE('',*,*,#25985,.F.);
#33627=ORIENTED_EDGE('',*,*,#25986,.F.);
#33628=ORIENTED_EDGE('',*,*,#25987,.F.);
#33629=ORIENTED_EDGE('',*,*,#25988,.F.);
#33630=ORIENTED_EDGE('',*,*,#25989,.F.);
#33631=ORIENTED_EDGE('',*,*,#25990,.F.);
#33632=ORIENTED_EDGE('',*,*,#25991,.F.);
#33633=ORIENTED_EDGE('',*,*,#25992,.F.);
#33634=ORIENTED_EDGE('',*,*,#25993,.F.);
#33635=ORIENTED_EDGE('',*,*,#25994,.F.);
#33636=ORIENTED_EDGE('',*,*,#25995,.F.);
#33637=ORIENTED_EDGE('',*,*,#25996,.F.);
#33638=ORIENTED_EDGE('',*,*,#25997,.F.);
#33639=ORIENTED_EDGE('',*,*,#25998,.F.);
#33640=ORIENTED_EDGE('',*,*,#25999,.F.);
#33641=ORIENTED_EDGE('',*,*,#25406,.T.);
#33642=ORIENTED_EDGE('',*,*,#26000,.T.);
#33643=ORIENTED_EDGE('',*,*,#26001,.T.);
#33644=ORIENTED_EDGE('',*,*,#26002,.F.);
#33645=ORIENTED_EDGE('',*,*,#26003,.F.);
#33646=ORIENTED_EDGE('',*,*,#26004,.F.);
#33647=ORIENTED_EDGE('',*,*,#25969,.T.);
#33648=ORIENTED_EDGE('',*,*,#25403,.T.);
#33649=ORIENTED_EDGE('',*,*,#26005,.F.);
#33650=ORIENTED_EDGE('',*,*,#26006,.F.);
#33651=ORIENTED_EDGE('',*,*,#26007,.F.);
#33652=ORIENTED_EDGE('',*,*,#26008,.F.);
#33653=ORIENTED_EDGE('',*,*,#26009,.F.);
#33654=ORIENTED_EDGE('',*,*,#26010,.F.);
#33655=ORIENTED_EDGE('',*,*,#26011,.F.);
#33656=ORIENTED_EDGE('',*,*,#26012,.F.);
#33657=ORIENTED_EDGE('',*,*,#26013,.F.);
#33658=ORIENTED_EDGE('',*,*,#26014,.F.);
#33659=ORIENTED_EDGE('',*,*,#26015,.F.);
#33660=ORIENTED_EDGE('',*,*,#26016,.F.);
#33661=ORIENTED_EDGE('',*,*,#26017,.F.);
#33662=ORIENTED_EDGE('',*,*,#26018,.F.);
#33663=ORIENTED_EDGE('',*,*,#26019,.F.);
#33664=ORIENTED_EDGE('',*,*,#26020,.T.);
#33665=ORIENTED_EDGE('',*,*,#26021,.F.);
#33666=ORIENTED_EDGE('',*,*,#26022,.F.);
#33667=ORIENTED_EDGE('',*,*,#26023,.F.);
#33668=ORIENTED_EDGE('',*,*,#26024,.F.);
#33669=ORIENTED_EDGE('',*,*,#26025,.F.);
#33670=ORIENTED_EDGE('',*,*,#26026,.F.);
#33671=ORIENTED_EDGE('',*,*,#26027,.F.);
#33672=ORIENTED_EDGE('',*,*,#26028,.F.);
#33673=ORIENTED_EDGE('',*,*,#26029,.F.);
#33674=ORIENTED_EDGE('',*,*,#26030,.F.);
#33675=ORIENTED_EDGE('',*,*,#26031,.F.);
#33676=ORIENTED_EDGE('',*,*,#26032,.F.);
#33677=ORIENTED_EDGE('',*,*,#26033,.F.);
#33678=ORIENTED_EDGE('',*,*,#26034,.F.);
#33679=ORIENTED_EDGE('',*,*,#26035,.F.);
#33680=ORIENTED_EDGE('',*,*,#25402,.T.);
#33681=ORIENTED_EDGE('',*,*,#26036,.T.);
#33682=ORIENTED_EDGE('',*,*,#26037,.T.);
#33683=ORIENTED_EDGE('',*,*,#26038,.F.);
#33684=ORIENTED_EDGE('',*,*,#26039,.F.);
#33685=ORIENTED_EDGE('',*,*,#26040,.F.);
#33686=ORIENTED_EDGE('',*,*,#26005,.T.);
#33687=ORIENTED_EDGE('',*,*,#25399,.T.);
#33688=ORIENTED_EDGE('',*,*,#26041,.F.);
#33689=ORIENTED_EDGE('',*,*,#26042,.F.);
#33690=ORIENTED_EDGE('',*,*,#26043,.F.);
#33691=ORIENTED_EDGE('',*,*,#26044,.F.);
#33692=ORIENTED_EDGE('',*,*,#26045,.F.);
#33693=ORIENTED_EDGE('',*,*,#26046,.F.);
#33694=ORIENTED_EDGE('',*,*,#26047,.F.);
#33695=ORIENTED_EDGE('',*,*,#26048,.F.);
#33696=ORIENTED_EDGE('',*,*,#26049,.F.);
#33697=ORIENTED_EDGE('',*,*,#26050,.F.);
#33698=ORIENTED_EDGE('',*,*,#26051,.F.);
#33699=ORIENTED_EDGE('',*,*,#26052,.F.);
#33700=ORIENTED_EDGE('',*,*,#26053,.F.);
#33701=ORIENTED_EDGE('',*,*,#26054,.F.);
#33702=ORIENTED_EDGE('',*,*,#26055,.F.);
#33703=ORIENTED_EDGE('',*,*,#26056,.T.);
#33704=ORIENTED_EDGE('',*,*,#26057,.F.);
#33705=ORIENTED_EDGE('',*,*,#26058,.F.);
#33706=ORIENTED_EDGE('',*,*,#26059,.F.);
#33707=ORIENTED_EDGE('',*,*,#26060,.F.);
#33708=ORIENTED_EDGE('',*,*,#26061,.F.);
#33709=ORIENTED_EDGE('',*,*,#26062,.F.);
#33710=ORIENTED_EDGE('',*,*,#26063,.F.);
#33711=ORIENTED_EDGE('',*,*,#26064,.F.);
#33712=ORIENTED_EDGE('',*,*,#26065,.F.);
#33713=ORIENTED_EDGE('',*,*,#26066,.F.);
#33714=ORIENTED_EDGE('',*,*,#26067,.F.);
#33715=ORIENTED_EDGE('',*,*,#26068,.F.);
#33716=ORIENTED_EDGE('',*,*,#26069,.F.);
#33717=ORIENTED_EDGE('',*,*,#26070,.F.);
#33718=ORIENTED_EDGE('',*,*,#26071,.F.);
#33719=ORIENTED_EDGE('',*,*,#25398,.T.);
#33720=ORIENTED_EDGE('',*,*,#26072,.T.);
#33721=ORIENTED_EDGE('',*,*,#26073,.T.);
#33722=ORIENTED_EDGE('',*,*,#26074,.F.);
#33723=ORIENTED_EDGE('',*,*,#26075,.F.);
#33724=ORIENTED_EDGE('',*,*,#26076,.F.);
#33725=ORIENTED_EDGE('',*,*,#26041,.T.);
#33726=ORIENTED_EDGE('',*,*,#25395,.T.);
#33727=ORIENTED_EDGE('',*,*,#26077,.F.);
#33728=ORIENTED_EDGE('',*,*,#26078,.F.);
#33729=ORIENTED_EDGE('',*,*,#26079,.F.);
#33730=ORIENTED_EDGE('',*,*,#26080,.F.);
#33731=ORIENTED_EDGE('',*,*,#26081,.F.);
#33732=ORIENTED_EDGE('',*,*,#26082,.F.);
#33733=ORIENTED_EDGE('',*,*,#26083,.F.);
#33734=ORIENTED_EDGE('',*,*,#26084,.F.);
#33735=ORIENTED_EDGE('',*,*,#26085,.F.);
#33736=ORIENTED_EDGE('',*,*,#26086,.F.);
#33737=ORIENTED_EDGE('',*,*,#26087,.F.);
#33738=ORIENTED_EDGE('',*,*,#26088,.F.);
#33739=ORIENTED_EDGE('',*,*,#26089,.F.);
#33740=ORIENTED_EDGE('',*,*,#26090,.F.);
#33741=ORIENTED_EDGE('',*,*,#26091,.F.);
#33742=ORIENTED_EDGE('',*,*,#26092,.T.);
#33743=ORIENTED_EDGE('',*,*,#26093,.F.);
#33744=ORIENTED_EDGE('',*,*,#26094,.F.);
#33745=ORIENTED_EDGE('',*,*,#26095,.F.);
#33746=ORIENTED_EDGE('',*,*,#26096,.F.);
#33747=ORIENTED_EDGE('',*,*,#26097,.F.);
#33748=ORIENTED_EDGE('',*,*,#26098,.F.);
#33749=ORIENTED_EDGE('',*,*,#26099,.F.);
#33750=ORIENTED_EDGE('',*,*,#26100,.F.);
#33751=ORIENTED_EDGE('',*,*,#26101,.F.);
#33752=ORIENTED_EDGE('',*,*,#26102,.F.);
#33753=ORIENTED_EDGE('',*,*,#26103,.F.);
#33754=ORIENTED_EDGE('',*,*,#26104,.F.);
#33755=ORIENTED_EDGE('',*,*,#26105,.F.);
#33756=ORIENTED_EDGE('',*,*,#26106,.F.);
#33757=ORIENTED_EDGE('',*,*,#26107,.F.);
#33758=ORIENTED_EDGE('',*,*,#25394,.T.);
#33759=ORIENTED_EDGE('',*,*,#26108,.T.);
#33760=ORIENTED_EDGE('',*,*,#26109,.T.);
#33761=ORIENTED_EDGE('',*,*,#26110,.F.);
#33762=ORIENTED_EDGE('',*,*,#26111,.F.);
#33763=ORIENTED_EDGE('',*,*,#26112,.F.);
#33764=ORIENTED_EDGE('',*,*,#26077,.T.);
#33765=ORIENTED_EDGE('',*,*,#25391,.T.);
#33766=ORIENTED_EDGE('',*,*,#26113,.F.);
#33767=ORIENTED_EDGE('',*,*,#26114,.F.);
#33768=ORIENTED_EDGE('',*,*,#26115,.F.);
#33769=ORIENTED_EDGE('',*,*,#26116,.F.);
#33770=ORIENTED_EDGE('',*,*,#26117,.F.);
#33771=ORIENTED_EDGE('',*,*,#26118,.F.);
#33772=ORIENTED_EDGE('',*,*,#26119,.F.);
#33773=ORIENTED_EDGE('',*,*,#26120,.F.);
#33774=ORIENTED_EDGE('',*,*,#26121,.F.);
#33775=ORIENTED_EDGE('',*,*,#26122,.F.);
#33776=ORIENTED_EDGE('',*,*,#26123,.F.);
#33777=ORIENTED_EDGE('',*,*,#26124,.F.);
#33778=ORIENTED_EDGE('',*,*,#26125,.F.);
#33779=ORIENTED_EDGE('',*,*,#26126,.F.);
#33780=ORIENTED_EDGE('',*,*,#26127,.F.);
#33781=ORIENTED_EDGE('',*,*,#26128,.T.);
#33782=ORIENTED_EDGE('',*,*,#26129,.F.);
#33783=ORIENTED_EDGE('',*,*,#26130,.F.);
#33784=ORIENTED_EDGE('',*,*,#26131,.F.);
#33785=ORIENTED_EDGE('',*,*,#26132,.F.);
#33786=ORIENTED_EDGE('',*,*,#26133,.F.);
#33787=ORIENTED_EDGE('',*,*,#26134,.F.);
#33788=ORIENTED_EDGE('',*,*,#26135,.F.);
#33789=ORIENTED_EDGE('',*,*,#26136,.F.);
#33790=ORIENTED_EDGE('',*,*,#26137,.F.);
#33791=ORIENTED_EDGE('',*,*,#26138,.F.);
#33792=ORIENTED_EDGE('',*,*,#26139,.F.);
#33793=ORIENTED_EDGE('',*,*,#26140,.F.);
#33794=ORIENTED_EDGE('',*,*,#26141,.F.);
#33795=ORIENTED_EDGE('',*,*,#26142,.F.);
#33796=ORIENTED_EDGE('',*,*,#26143,.F.);
#33797=ORIENTED_EDGE('',*,*,#25390,.T.);
#33798=ORIENTED_EDGE('',*,*,#26144,.T.);
#33799=ORIENTED_EDGE('',*,*,#26145,.T.);
#33800=ORIENTED_EDGE('',*,*,#26146,.F.);
#33801=ORIENTED_EDGE('',*,*,#26147,.F.);
#33802=ORIENTED_EDGE('',*,*,#26148,.F.);
#33803=ORIENTED_EDGE('',*,*,#26113,.T.);
#33804=ORIENTED_EDGE('',*,*,#25387,.T.);
#33805=ORIENTED_EDGE('',*,*,#26149,.F.);
#33806=ORIENTED_EDGE('',*,*,#26150,.F.);
#33807=ORIENTED_EDGE('',*,*,#26151,.F.);
#33808=ORIENTED_EDGE('',*,*,#26152,.F.);
#33809=ORIENTED_EDGE('',*,*,#26153,.F.);
#33810=ORIENTED_EDGE('',*,*,#26154,.F.);
#33811=ORIENTED_EDGE('',*,*,#26155,.F.);
#33812=ORIENTED_EDGE('',*,*,#26156,.F.);
#33813=ORIENTED_EDGE('',*,*,#26157,.F.);
#33814=ORIENTED_EDGE('',*,*,#26158,.F.);
#33815=ORIENTED_EDGE('',*,*,#26159,.F.);
#33816=ORIENTED_EDGE('',*,*,#26160,.F.);
#33817=ORIENTED_EDGE('',*,*,#26161,.F.);
#33818=ORIENTED_EDGE('',*,*,#26162,.F.);
#33819=ORIENTED_EDGE('',*,*,#26163,.F.);
#33820=ORIENTED_EDGE('',*,*,#26164,.T.);
#33821=ORIENTED_EDGE('',*,*,#26165,.F.);
#33822=ORIENTED_EDGE('',*,*,#26166,.F.);
#33823=ORIENTED_EDGE('',*,*,#26167,.F.);
#33824=ORIENTED_EDGE('',*,*,#26168,.F.);
#33825=ORIENTED_EDGE('',*,*,#26169,.F.);
#33826=ORIENTED_EDGE('',*,*,#26170,.F.);
#33827=ORIENTED_EDGE('',*,*,#26171,.F.);
#33828=ORIENTED_EDGE('',*,*,#26172,.F.);
#33829=ORIENTED_EDGE('',*,*,#26173,.F.);
#33830=ORIENTED_EDGE('',*,*,#26174,.F.);
#33831=ORIENTED_EDGE('',*,*,#26175,.F.);
#33832=ORIENTED_EDGE('',*,*,#26176,.F.);
#33833=ORIENTED_EDGE('',*,*,#26177,.F.);
#33834=ORIENTED_EDGE('',*,*,#26178,.F.);
#33835=ORIENTED_EDGE('',*,*,#26179,.F.);
#33836=ORIENTED_EDGE('',*,*,#25386,.T.);
#33837=ORIENTED_EDGE('',*,*,#26180,.T.);
#33838=ORIENTED_EDGE('',*,*,#26181,.T.);
#33839=ORIENTED_EDGE('',*,*,#26182,.F.);
#33840=ORIENTED_EDGE('',*,*,#26183,.F.);
#33841=ORIENTED_EDGE('',*,*,#26184,.F.);
#33842=ORIENTED_EDGE('',*,*,#26149,.T.);
#33843=ORIENTED_EDGE('',*,*,#25383,.T.);
#33844=ORIENTED_EDGE('',*,*,#26185,.F.);
#33845=ORIENTED_EDGE('',*,*,#26186,.F.);
#33846=ORIENTED_EDGE('',*,*,#26187,.F.);
#33847=ORIENTED_EDGE('',*,*,#26188,.F.);
#33848=ORIENTED_EDGE('',*,*,#26189,.F.);
#33849=ORIENTED_EDGE('',*,*,#26190,.F.);
#33850=ORIENTED_EDGE('',*,*,#26191,.F.);
#33851=ORIENTED_EDGE('',*,*,#26192,.F.);
#33852=ORIENTED_EDGE('',*,*,#26193,.F.);
#33853=ORIENTED_EDGE('',*,*,#26194,.F.);
#33854=ORIENTED_EDGE('',*,*,#26195,.F.);
#33855=ORIENTED_EDGE('',*,*,#26196,.F.);
#33856=ORIENTED_EDGE('',*,*,#26197,.F.);
#33857=ORIENTED_EDGE('',*,*,#26198,.F.);
#33858=ORIENTED_EDGE('',*,*,#26199,.F.);
#33859=ORIENTED_EDGE('',*,*,#26200,.T.);
#33860=ORIENTED_EDGE('',*,*,#26201,.F.);
#33861=ORIENTED_EDGE('',*,*,#26202,.F.);
#33862=ORIENTED_EDGE('',*,*,#26203,.F.);
#33863=ORIENTED_EDGE('',*,*,#26204,.F.);
#33864=ORIENTED_EDGE('',*,*,#26205,.F.);
#33865=ORIENTED_EDGE('',*,*,#26206,.F.);
#33866=ORIENTED_EDGE('',*,*,#26207,.F.);
#33867=ORIENTED_EDGE('',*,*,#26208,.F.);
#33868=ORIENTED_EDGE('',*,*,#26209,.F.);
#33869=ORIENTED_EDGE('',*,*,#26210,.F.);
#33870=ORIENTED_EDGE('',*,*,#26211,.F.);
#33871=ORIENTED_EDGE('',*,*,#26212,.F.);
#33872=ORIENTED_EDGE('',*,*,#26213,.F.);
#33873=ORIENTED_EDGE('',*,*,#26214,.F.);
#33874=ORIENTED_EDGE('',*,*,#26215,.F.);
#33875=ORIENTED_EDGE('',*,*,#25382,.T.);
#33876=ORIENTED_EDGE('',*,*,#26216,.T.);
#33877=ORIENTED_EDGE('',*,*,#26217,.T.);
#33878=ORIENTED_EDGE('',*,*,#26218,.F.);
#33879=ORIENTED_EDGE('',*,*,#26219,.F.);
#33880=ORIENTED_EDGE('',*,*,#26220,.F.);
#33881=ORIENTED_EDGE('',*,*,#26185,.T.);
#33882=ORIENTED_EDGE('',*,*,#25379,.T.);
#33883=ORIENTED_EDGE('',*,*,#26221,.F.);
#33884=ORIENTED_EDGE('',*,*,#26222,.F.);
#33885=ORIENTED_EDGE('',*,*,#26223,.F.);
#33886=ORIENTED_EDGE('',*,*,#26224,.F.);
#33887=ORIENTED_EDGE('',*,*,#26225,.F.);
#33888=ORIENTED_EDGE('',*,*,#26226,.F.);
#33889=ORIENTED_EDGE('',*,*,#26227,.F.);
#33890=ORIENTED_EDGE('',*,*,#26228,.F.);
#33891=ORIENTED_EDGE('',*,*,#26229,.F.);
#33892=ORIENTED_EDGE('',*,*,#26230,.F.);
#33893=ORIENTED_EDGE('',*,*,#26231,.F.);
#33894=ORIENTED_EDGE('',*,*,#26232,.F.);
#33895=ORIENTED_EDGE('',*,*,#26233,.F.);
#33896=ORIENTED_EDGE('',*,*,#26234,.F.);
#33897=ORIENTED_EDGE('',*,*,#26235,.F.);
#33898=ORIENTED_EDGE('',*,*,#26236,.T.);
#33899=ORIENTED_EDGE('',*,*,#26237,.F.);
#33900=ORIENTED_EDGE('',*,*,#26238,.F.);
#33901=ORIENTED_EDGE('',*,*,#26239,.F.);
#33902=ORIENTED_EDGE('',*,*,#26240,.F.);
#33903=ORIENTED_EDGE('',*,*,#26241,.F.);
#33904=ORIENTED_EDGE('',*,*,#26242,.F.);
#33905=ORIENTED_EDGE('',*,*,#26243,.F.);
#33906=ORIENTED_EDGE('',*,*,#26244,.F.);
#33907=ORIENTED_EDGE('',*,*,#26245,.F.);
#33908=ORIENTED_EDGE('',*,*,#26246,.F.);
#33909=ORIENTED_EDGE('',*,*,#26247,.F.);
#33910=ORIENTED_EDGE('',*,*,#26248,.F.);
#33911=ORIENTED_EDGE('',*,*,#26249,.F.);
#33912=ORIENTED_EDGE('',*,*,#26250,.F.);
#33913=ORIENTED_EDGE('',*,*,#26251,.F.);
#33914=ORIENTED_EDGE('',*,*,#25378,.T.);
#33915=ORIENTED_EDGE('',*,*,#26252,.T.);
#33916=ORIENTED_EDGE('',*,*,#26253,.T.);
#33917=ORIENTED_EDGE('',*,*,#26254,.F.);
#33918=ORIENTED_EDGE('',*,*,#26255,.F.);
#33919=ORIENTED_EDGE('',*,*,#26256,.F.);
#33920=ORIENTED_EDGE('',*,*,#26221,.T.);
#33921=ORIENTED_EDGE('',*,*,#25375,.T.);
#33922=ORIENTED_EDGE('',*,*,#26257,.F.);
#33923=ORIENTED_EDGE('',*,*,#26258,.F.);
#33924=ORIENTED_EDGE('',*,*,#26259,.F.);
#33925=ORIENTED_EDGE('',*,*,#26260,.F.);
#33926=ORIENTED_EDGE('',*,*,#26261,.F.);
#33927=ORIENTED_EDGE('',*,*,#26262,.F.);
#33928=ORIENTED_EDGE('',*,*,#26263,.F.);
#33929=ORIENTED_EDGE('',*,*,#26264,.F.);
#33930=ORIENTED_EDGE('',*,*,#26265,.F.);
#33931=ORIENTED_EDGE('',*,*,#26266,.F.);
#33932=ORIENTED_EDGE('',*,*,#26267,.F.);
#33933=ORIENTED_EDGE('',*,*,#26268,.F.);
#33934=ORIENTED_EDGE('',*,*,#26269,.F.);
#33935=ORIENTED_EDGE('',*,*,#26270,.F.);
#33936=ORIENTED_EDGE('',*,*,#26271,.F.);
#33937=ORIENTED_EDGE('',*,*,#26272,.T.);
#33938=ORIENTED_EDGE('',*,*,#26273,.F.);
#33939=ORIENTED_EDGE('',*,*,#26274,.F.);
#33940=ORIENTED_EDGE('',*,*,#26275,.F.);
#33941=ORIENTED_EDGE('',*,*,#26276,.F.);
#33942=ORIENTED_EDGE('',*,*,#26277,.F.);
#33943=ORIENTED_EDGE('',*,*,#26278,.F.);
#33944=ORIENTED_EDGE('',*,*,#26279,.F.);
#33945=ORIENTED_EDGE('',*,*,#26280,.F.);
#33946=ORIENTED_EDGE('',*,*,#26281,.F.);
#33947=ORIENTED_EDGE('',*,*,#26282,.F.);
#33948=ORIENTED_EDGE('',*,*,#26283,.F.);
#33949=ORIENTED_EDGE('',*,*,#26284,.F.);
#33950=ORIENTED_EDGE('',*,*,#26285,.F.);
#33951=ORIENTED_EDGE('',*,*,#26286,.F.);
#33952=ORIENTED_EDGE('',*,*,#26287,.F.);
#33953=ORIENTED_EDGE('',*,*,#25374,.T.);
#33954=ORIENTED_EDGE('',*,*,#26288,.T.);
#33955=ORIENTED_EDGE('',*,*,#26289,.T.);
#33956=ORIENTED_EDGE('',*,*,#26290,.F.);
#33957=ORIENTED_EDGE('',*,*,#26291,.F.);
#33958=ORIENTED_EDGE('',*,*,#26292,.F.);
#33959=ORIENTED_EDGE('',*,*,#26257,.T.);
#33960=ORIENTED_EDGE('',*,*,#25371,.T.);
#33961=ORIENTED_EDGE('',*,*,#26293,.F.);
#33962=ORIENTED_EDGE('',*,*,#26294,.F.);
#33963=ORIENTED_EDGE('',*,*,#26295,.F.);
#33964=ORIENTED_EDGE('',*,*,#26296,.F.);
#33965=ORIENTED_EDGE('',*,*,#26297,.F.);
#33966=ORIENTED_EDGE('',*,*,#26298,.F.);
#33967=ORIENTED_EDGE('',*,*,#26299,.F.);
#33968=ORIENTED_EDGE('',*,*,#26300,.F.);
#33969=ORIENTED_EDGE('',*,*,#26301,.F.);
#33970=ORIENTED_EDGE('',*,*,#26302,.F.);
#33971=ORIENTED_EDGE('',*,*,#26303,.F.);
#33972=ORIENTED_EDGE('',*,*,#26304,.F.);
#33973=ORIENTED_EDGE('',*,*,#26305,.F.);
#33974=ORIENTED_EDGE('',*,*,#26306,.F.);
#33975=ORIENTED_EDGE('',*,*,#26307,.F.);
#33976=ORIENTED_EDGE('',*,*,#26308,.T.);
#33977=ORIENTED_EDGE('',*,*,#26309,.F.);
#33978=ORIENTED_EDGE('',*,*,#26310,.F.);
#33979=ORIENTED_EDGE('',*,*,#26311,.F.);
#33980=ORIENTED_EDGE('',*,*,#26312,.F.);
#33981=ORIENTED_EDGE('',*,*,#26313,.F.);
#33982=ORIENTED_EDGE('',*,*,#26314,.F.);
#33983=ORIENTED_EDGE('',*,*,#26315,.F.);
#33984=ORIENTED_EDGE('',*,*,#26316,.F.);
#33985=ORIENTED_EDGE('',*,*,#26317,.F.);
#33986=ORIENTED_EDGE('',*,*,#26318,.F.);
#33987=ORIENTED_EDGE('',*,*,#26319,.F.);
#33988=ORIENTED_EDGE('',*,*,#26320,.F.);
#33989=ORIENTED_EDGE('',*,*,#26321,.F.);
#33990=ORIENTED_EDGE('',*,*,#26322,.F.);
#33991=ORIENTED_EDGE('',*,*,#26323,.F.);
#33992=ORIENTED_EDGE('',*,*,#25370,.T.);
#33993=ORIENTED_EDGE('',*,*,#26324,.T.);
#33994=ORIENTED_EDGE('',*,*,#26325,.T.);
#33995=ORIENTED_EDGE('',*,*,#26326,.F.);
#33996=ORIENTED_EDGE('',*,*,#26327,.F.);
#33997=ORIENTED_EDGE('',*,*,#26328,.F.);
#33998=ORIENTED_EDGE('',*,*,#26293,.T.);
#33999=ORIENTED_EDGE('',*,*,#25367,.T.);
#34000=ORIENTED_EDGE('',*,*,#26329,.F.);
#34001=ORIENTED_EDGE('',*,*,#26330,.F.);
#34002=ORIENTED_EDGE('',*,*,#26331,.F.);
#34003=ORIENTED_EDGE('',*,*,#26332,.F.);
#34004=ORIENTED_EDGE('',*,*,#26333,.F.);
#34005=ORIENTED_EDGE('',*,*,#26334,.F.);
#34006=ORIENTED_EDGE('',*,*,#26335,.F.);
#34007=ORIENTED_EDGE('',*,*,#26336,.F.);
#34008=ORIENTED_EDGE('',*,*,#26337,.F.);
#34009=ORIENTED_EDGE('',*,*,#26338,.F.);
#34010=ORIENTED_EDGE('',*,*,#26339,.F.);
#34011=ORIENTED_EDGE('',*,*,#26340,.F.);
#34012=ORIENTED_EDGE('',*,*,#26341,.F.);
#34013=ORIENTED_EDGE('',*,*,#26342,.F.);
#34014=ORIENTED_EDGE('',*,*,#26343,.F.);
#34015=ORIENTED_EDGE('',*,*,#26344,.T.);
#34016=ORIENTED_EDGE('',*,*,#26345,.F.);
#34017=ORIENTED_EDGE('',*,*,#26346,.F.);
#34018=ORIENTED_EDGE('',*,*,#26347,.F.);
#34019=ORIENTED_EDGE('',*,*,#26348,.F.);
#34020=ORIENTED_EDGE('',*,*,#26349,.F.);
#34021=ORIENTED_EDGE('',*,*,#26350,.F.);
#34022=ORIENTED_EDGE('',*,*,#26351,.F.);
#34023=ORIENTED_EDGE('',*,*,#26352,.F.);
#34024=ORIENTED_EDGE('',*,*,#26353,.F.);
#34025=ORIENTED_EDGE('',*,*,#26354,.F.);
#34026=ORIENTED_EDGE('',*,*,#26355,.F.);
#34027=ORIENTED_EDGE('',*,*,#26356,.F.);
#34028=ORIENTED_EDGE('',*,*,#26357,.F.);
#34029=ORIENTED_EDGE('',*,*,#26358,.F.);
#34030=ORIENTED_EDGE('',*,*,#26359,.F.);
#34031=ORIENTED_EDGE('',*,*,#25366,.T.);
#34032=ORIENTED_EDGE('',*,*,#26360,.T.);
#34033=ORIENTED_EDGE('',*,*,#26361,.T.);
#34034=ORIENTED_EDGE('',*,*,#26362,.F.);
#34035=ORIENTED_EDGE('',*,*,#26363,.F.);
#34036=ORIENTED_EDGE('',*,*,#26364,.F.);
#34037=ORIENTED_EDGE('',*,*,#26329,.T.);
#34038=ORIENTED_EDGE('',*,*,#25363,.T.);
#34039=ORIENTED_EDGE('',*,*,#26365,.F.);
#34040=ORIENTED_EDGE('',*,*,#26366,.F.);
#34041=ORIENTED_EDGE('',*,*,#26367,.F.);
#34042=ORIENTED_EDGE('',*,*,#26368,.F.);
#34043=ORIENTED_EDGE('',*,*,#26369,.F.);
#34044=ORIENTED_EDGE('',*,*,#26370,.F.);
#34045=ORIENTED_EDGE('',*,*,#26371,.F.);
#34046=ORIENTED_EDGE('',*,*,#26372,.F.);
#34047=ORIENTED_EDGE('',*,*,#26373,.F.);
#34048=ORIENTED_EDGE('',*,*,#26374,.F.);
#34049=ORIENTED_EDGE('',*,*,#26375,.F.);
#34050=ORIENTED_EDGE('',*,*,#26376,.F.);
#34051=ORIENTED_EDGE('',*,*,#26377,.F.);
#34052=ORIENTED_EDGE('',*,*,#26378,.F.);
#34053=ORIENTED_EDGE('',*,*,#26379,.F.);
#34054=ORIENTED_EDGE('',*,*,#26380,.T.);
#34055=ORIENTED_EDGE('',*,*,#26381,.F.);
#34056=ORIENTED_EDGE('',*,*,#26382,.F.);
#34057=ORIENTED_EDGE('',*,*,#26383,.F.);
#34058=ORIENTED_EDGE('',*,*,#26384,.F.);
#34059=ORIENTED_EDGE('',*,*,#26385,.F.);
#34060=ORIENTED_EDGE('',*,*,#26386,.F.);
#34061=ORIENTED_EDGE('',*,*,#26387,.F.);
#34062=ORIENTED_EDGE('',*,*,#26388,.F.);
#34063=ORIENTED_EDGE('',*,*,#26389,.F.);
#34064=ORIENTED_EDGE('',*,*,#26390,.F.);
#34065=ORIENTED_EDGE('',*,*,#26391,.F.);
#34066=ORIENTED_EDGE('',*,*,#26392,.F.);
#34067=ORIENTED_EDGE('',*,*,#26393,.F.);
#34068=ORIENTED_EDGE('',*,*,#26394,.F.);
#34069=ORIENTED_EDGE('',*,*,#26395,.F.);
#34070=ORIENTED_EDGE('',*,*,#25362,.T.);
#34071=ORIENTED_EDGE('',*,*,#26396,.T.);
#34072=ORIENTED_EDGE('',*,*,#26397,.T.);
#34073=ORIENTED_EDGE('',*,*,#26398,.F.);
#34074=ORIENTED_EDGE('',*,*,#26399,.F.);
#34075=ORIENTED_EDGE('',*,*,#26400,.F.);
#34076=ORIENTED_EDGE('',*,*,#26365,.T.);
#34077=ORIENTED_EDGE('',*,*,#25359,.T.);
#34078=ORIENTED_EDGE('',*,*,#26401,.F.);
#34079=ORIENTED_EDGE('',*,*,#26402,.F.);
#34080=ORIENTED_EDGE('',*,*,#26403,.F.);
#34081=ORIENTED_EDGE('',*,*,#26404,.F.);
#34082=ORIENTED_EDGE('',*,*,#26405,.F.);
#34083=ORIENTED_EDGE('',*,*,#26406,.F.);
#34084=ORIENTED_EDGE('',*,*,#26407,.F.);
#34085=ORIENTED_EDGE('',*,*,#26408,.F.);
#34086=ORIENTED_EDGE('',*,*,#26409,.F.);
#34087=ORIENTED_EDGE('',*,*,#26410,.F.);
#34088=ORIENTED_EDGE('',*,*,#26411,.F.);
#34089=ORIENTED_EDGE('',*,*,#26412,.F.);
#34090=ORIENTED_EDGE('',*,*,#26413,.F.);
#34091=ORIENTED_EDGE('',*,*,#26414,.F.);
#34092=ORIENTED_EDGE('',*,*,#26415,.F.);
#34093=ORIENTED_EDGE('',*,*,#26416,.T.);
#34094=ORIENTED_EDGE('',*,*,#26417,.F.);
#34095=ORIENTED_EDGE('',*,*,#26418,.F.);
#34096=ORIENTED_EDGE('',*,*,#26419,.F.);
#34097=ORIENTED_EDGE('',*,*,#26420,.F.);
#34098=ORIENTED_EDGE('',*,*,#26421,.F.);
#34099=ORIENTED_EDGE('',*,*,#26422,.F.);
#34100=ORIENTED_EDGE('',*,*,#26423,.F.);
#34101=ORIENTED_EDGE('',*,*,#26424,.F.);
#34102=ORIENTED_EDGE('',*,*,#26425,.F.);
#34103=ORIENTED_EDGE('',*,*,#26426,.F.);
#34104=ORIENTED_EDGE('',*,*,#26427,.F.);
#34105=ORIENTED_EDGE('',*,*,#26428,.F.);
#34106=ORIENTED_EDGE('',*,*,#26429,.F.);
#34107=ORIENTED_EDGE('',*,*,#26430,.F.);
#34108=ORIENTED_EDGE('',*,*,#26431,.F.);
#34109=ORIENTED_EDGE('',*,*,#25358,.T.);
#34110=ORIENTED_EDGE('',*,*,#26432,.T.);
#34111=ORIENTED_EDGE('',*,*,#26433,.T.);
#34112=ORIENTED_EDGE('',*,*,#26434,.F.);
#34113=ORIENTED_EDGE('',*,*,#26435,.F.);
#34114=ORIENTED_EDGE('',*,*,#26436,.F.);
#34115=ORIENTED_EDGE('',*,*,#26401,.T.);
#34116=ORIENTED_EDGE('',*,*,#25355,.T.);
#34117=ORIENTED_EDGE('',*,*,#26437,.F.);
#34118=ORIENTED_EDGE('',*,*,#26438,.F.);
#34119=ORIENTED_EDGE('',*,*,#26439,.F.);
#34120=ORIENTED_EDGE('',*,*,#26440,.F.);
#34121=ORIENTED_EDGE('',*,*,#26441,.F.);
#34122=ORIENTED_EDGE('',*,*,#26442,.F.);
#34123=ORIENTED_EDGE('',*,*,#26443,.F.);
#34124=ORIENTED_EDGE('',*,*,#26444,.F.);
#34125=ORIENTED_EDGE('',*,*,#26445,.F.);
#34126=ORIENTED_EDGE('',*,*,#26446,.F.);
#34127=ORIENTED_EDGE('',*,*,#26447,.F.);
#34128=ORIENTED_EDGE('',*,*,#26448,.F.);
#34129=ORIENTED_EDGE('',*,*,#26449,.F.);
#34130=ORIENTED_EDGE('',*,*,#26450,.F.);
#34131=ORIENTED_EDGE('',*,*,#26451,.F.);
#34132=ORIENTED_EDGE('',*,*,#26452,.T.);
#34133=ORIENTED_EDGE('',*,*,#26453,.F.);
#34134=ORIENTED_EDGE('',*,*,#26454,.F.);
#34135=ORIENTED_EDGE('',*,*,#26455,.F.);
#34136=ORIENTED_EDGE('',*,*,#26456,.F.);
#34137=ORIENTED_EDGE('',*,*,#26457,.F.);
#34138=ORIENTED_EDGE('',*,*,#26458,.F.);
#34139=ORIENTED_EDGE('',*,*,#26459,.F.);
#34140=ORIENTED_EDGE('',*,*,#26460,.F.);
#34141=ORIENTED_EDGE('',*,*,#26461,.F.);
#34142=ORIENTED_EDGE('',*,*,#26462,.F.);
#34143=ORIENTED_EDGE('',*,*,#26463,.F.);
#34144=ORIENTED_EDGE('',*,*,#26464,.F.);
#34145=ORIENTED_EDGE('',*,*,#26465,.F.);
#34146=ORIENTED_EDGE('',*,*,#26466,.F.);
#34147=ORIENTED_EDGE('',*,*,#26467,.F.);
#34148=ORIENTED_EDGE('',*,*,#25354,.T.);
#34149=ORIENTED_EDGE('',*,*,#26468,.T.);
#34150=ORIENTED_EDGE('',*,*,#26469,.T.);
#34151=ORIENTED_EDGE('',*,*,#26470,.F.);
#34152=ORIENTED_EDGE('',*,*,#26471,.F.);
#34153=ORIENTED_EDGE('',*,*,#26472,.F.);
#34154=ORIENTED_EDGE('',*,*,#26437,.T.);
#34155=ORIENTED_EDGE('',*,*,#25351,.T.);
#34156=ORIENTED_EDGE('',*,*,#26473,.F.);
#34157=ORIENTED_EDGE('',*,*,#26474,.F.);
#34158=ORIENTED_EDGE('',*,*,#26475,.F.);
#34159=ORIENTED_EDGE('',*,*,#26476,.F.);
#34160=ORIENTED_EDGE('',*,*,#26477,.F.);
#34161=ORIENTED_EDGE('',*,*,#26478,.F.);
#34162=ORIENTED_EDGE('',*,*,#26479,.F.);
#34163=ORIENTED_EDGE('',*,*,#26480,.F.);
#34164=ORIENTED_EDGE('',*,*,#26481,.F.);
#34165=ORIENTED_EDGE('',*,*,#26482,.F.);
#34166=ORIENTED_EDGE('',*,*,#26483,.F.);
#34167=ORIENTED_EDGE('',*,*,#26484,.F.);
#34168=ORIENTED_EDGE('',*,*,#26485,.F.);
#34169=ORIENTED_EDGE('',*,*,#26486,.F.);
#34170=ORIENTED_EDGE('',*,*,#26487,.F.);
#34171=ORIENTED_EDGE('',*,*,#26488,.T.);
#34172=ORIENTED_EDGE('',*,*,#26489,.F.);
#34173=ORIENTED_EDGE('',*,*,#26490,.F.);
#34174=ORIENTED_EDGE('',*,*,#26491,.F.);
#34175=ORIENTED_EDGE('',*,*,#26492,.F.);
#34176=ORIENTED_EDGE('',*,*,#26493,.F.);
#34177=ORIENTED_EDGE('',*,*,#26494,.F.);
#34178=ORIENTED_EDGE('',*,*,#26495,.F.);
#34179=ORIENTED_EDGE('',*,*,#26496,.F.);
#34180=ORIENTED_EDGE('',*,*,#26497,.F.);
#34181=ORIENTED_EDGE('',*,*,#26498,.F.);
#34182=ORIENTED_EDGE('',*,*,#26499,.F.);
#34183=ORIENTED_EDGE('',*,*,#26500,.F.);
#34184=ORIENTED_EDGE('',*,*,#26501,.F.);
#34185=ORIENTED_EDGE('',*,*,#26502,.F.);
#34186=ORIENTED_EDGE('',*,*,#26503,.F.);
#34187=ORIENTED_EDGE('',*,*,#25350,.T.);
#34188=ORIENTED_EDGE('',*,*,#26504,.T.);
#34189=ORIENTED_EDGE('',*,*,#26505,.T.);
#34190=ORIENTED_EDGE('',*,*,#26506,.F.);
#34191=ORIENTED_EDGE('',*,*,#26507,.F.);
#34192=ORIENTED_EDGE('',*,*,#26508,.F.);
#34193=ORIENTED_EDGE('',*,*,#26473,.T.);
#34194=ORIENTED_EDGE('',*,*,#25347,.T.);
#34195=ORIENTED_EDGE('',*,*,#26509,.F.);
#34196=ORIENTED_EDGE('',*,*,#26510,.F.);
#34197=ORIENTED_EDGE('',*,*,#26511,.F.);
#34198=ORIENTED_EDGE('',*,*,#26512,.F.);
#34199=ORIENTED_EDGE('',*,*,#26513,.F.);
#34200=ORIENTED_EDGE('',*,*,#26514,.F.);
#34201=ORIENTED_EDGE('',*,*,#26515,.F.);
#34202=ORIENTED_EDGE('',*,*,#26516,.F.);
#34203=ORIENTED_EDGE('',*,*,#26517,.F.);
#34204=ORIENTED_EDGE('',*,*,#26518,.F.);
#34205=ORIENTED_EDGE('',*,*,#26519,.F.);
#34206=ORIENTED_EDGE('',*,*,#26520,.F.);
#34207=ORIENTED_EDGE('',*,*,#26521,.F.);
#34208=ORIENTED_EDGE('',*,*,#26522,.F.);
#34209=ORIENTED_EDGE('',*,*,#26523,.F.);
#34210=ORIENTED_EDGE('',*,*,#26524,.T.);
#34211=ORIENTED_EDGE('',*,*,#26525,.F.);
#34212=ORIENTED_EDGE('',*,*,#26526,.F.);
#34213=ORIENTED_EDGE('',*,*,#26527,.F.);
#34214=ORIENTED_EDGE('',*,*,#26528,.F.);
#34215=ORIENTED_EDGE('',*,*,#26529,.F.);
#34216=ORIENTED_EDGE('',*,*,#26530,.F.);
#34217=ORIENTED_EDGE('',*,*,#26531,.F.);
#34218=ORIENTED_EDGE('',*,*,#26532,.F.);
#34219=ORIENTED_EDGE('',*,*,#26533,.F.);
#34220=ORIENTED_EDGE('',*,*,#26534,.F.);
#34221=ORIENTED_EDGE('',*,*,#26535,.F.);
#34222=ORIENTED_EDGE('',*,*,#26536,.F.);
#34223=ORIENTED_EDGE('',*,*,#26537,.F.);
#34224=ORIENTED_EDGE('',*,*,#26538,.F.);
#34225=ORIENTED_EDGE('',*,*,#26539,.F.);
#34226=ORIENTED_EDGE('',*,*,#25346,.T.);
#34227=ORIENTED_EDGE('',*,*,#26540,.T.);
#34228=ORIENTED_EDGE('',*,*,#26541,.T.);
#34229=ORIENTED_EDGE('',*,*,#26542,.F.);
#34230=ORIENTED_EDGE('',*,*,#26543,.F.);
#34231=ORIENTED_EDGE('',*,*,#26544,.F.);
#34232=ORIENTED_EDGE('',*,*,#26509,.T.);
#34233=ORIENTED_EDGE('',*,*,#25343,.T.);
#34234=ORIENTED_EDGE('',*,*,#26545,.F.);
#34235=ORIENTED_EDGE('',*,*,#26546,.F.);
#34236=ORIENTED_EDGE('',*,*,#26547,.F.);
#34237=ORIENTED_EDGE('',*,*,#26548,.F.);
#34238=ORIENTED_EDGE('',*,*,#26549,.F.);
#34239=ORIENTED_EDGE('',*,*,#26550,.F.);
#34240=ORIENTED_EDGE('',*,*,#26551,.F.);
#34241=ORIENTED_EDGE('',*,*,#26552,.F.);
#34242=ORIENTED_EDGE('',*,*,#26553,.F.);
#34243=ORIENTED_EDGE('',*,*,#26554,.F.);
#34244=ORIENTED_EDGE('',*,*,#26555,.F.);
#34245=ORIENTED_EDGE('',*,*,#26556,.F.);
#34246=ORIENTED_EDGE('',*,*,#26557,.F.);
#34247=ORIENTED_EDGE('',*,*,#26558,.F.);
#34248=ORIENTED_EDGE('',*,*,#26559,.F.);
#34249=ORIENTED_EDGE('',*,*,#26560,.T.);
#34250=ORIENTED_EDGE('',*,*,#26561,.F.);
#34251=ORIENTED_EDGE('',*,*,#26562,.F.);
#34252=ORIENTED_EDGE('',*,*,#26563,.F.);
#34253=ORIENTED_EDGE('',*,*,#26564,.F.);
#34254=ORIENTED_EDGE('',*,*,#26565,.F.);
#34255=ORIENTED_EDGE('',*,*,#26566,.F.);
#34256=ORIENTED_EDGE('',*,*,#26567,.F.);
#34257=ORIENTED_EDGE('',*,*,#26568,.F.);
#34258=ORIENTED_EDGE('',*,*,#26569,.F.);
#34259=ORIENTED_EDGE('',*,*,#26570,.F.);
#34260=ORIENTED_EDGE('',*,*,#26571,.F.);
#34261=ORIENTED_EDGE('',*,*,#26572,.F.);
#34262=ORIENTED_EDGE('',*,*,#26573,.F.);
#34263=ORIENTED_EDGE('',*,*,#26574,.F.);
#34264=ORIENTED_EDGE('',*,*,#26575,.F.);
#34265=ORIENTED_EDGE('',*,*,#25342,.T.);
#34266=ORIENTED_EDGE('',*,*,#26576,.T.);
#34267=ORIENTED_EDGE('',*,*,#26577,.T.);
#34268=ORIENTED_EDGE('',*,*,#26578,.F.);
#34269=ORIENTED_EDGE('',*,*,#26579,.F.);
#34270=ORIENTED_EDGE('',*,*,#26580,.F.);
#34271=ORIENTED_EDGE('',*,*,#26545,.T.);
#34272=ORIENTED_EDGE('',*,*,#25339,.T.);
#34273=ORIENTED_EDGE('',*,*,#26581,.F.);
#34274=ORIENTED_EDGE('',*,*,#26582,.F.);
#34275=ORIENTED_EDGE('',*,*,#26583,.F.);
#34276=ORIENTED_EDGE('',*,*,#26584,.F.);
#34277=ORIENTED_EDGE('',*,*,#26585,.F.);
#34278=ORIENTED_EDGE('',*,*,#26586,.F.);
#34279=ORIENTED_EDGE('',*,*,#26587,.F.);
#34280=ORIENTED_EDGE('',*,*,#26588,.F.);
#34281=ORIENTED_EDGE('',*,*,#26589,.F.);
#34282=ORIENTED_EDGE('',*,*,#26590,.F.);
#34283=ORIENTED_EDGE('',*,*,#26591,.F.);
#34284=ORIENTED_EDGE('',*,*,#26592,.F.);
#34285=ORIENTED_EDGE('',*,*,#26593,.F.);
#34286=ORIENTED_EDGE('',*,*,#26594,.F.);
#34287=ORIENTED_EDGE('',*,*,#26595,.F.);
#34288=ORIENTED_EDGE('',*,*,#26596,.T.);
#34289=ORIENTED_EDGE('',*,*,#26597,.F.);
#34290=ORIENTED_EDGE('',*,*,#26598,.F.);
#34291=ORIENTED_EDGE('',*,*,#26599,.F.);
#34292=ORIENTED_EDGE('',*,*,#26600,.F.);
#34293=ORIENTED_EDGE('',*,*,#26601,.F.);
#34294=ORIENTED_EDGE('',*,*,#26602,.F.);
#34295=ORIENTED_EDGE('',*,*,#26603,.F.);
#34296=ORIENTED_EDGE('',*,*,#26604,.F.);
#34297=ORIENTED_EDGE('',*,*,#26605,.F.);
#34298=ORIENTED_EDGE('',*,*,#26606,.F.);
#34299=ORIENTED_EDGE('',*,*,#26607,.F.);
#34300=ORIENTED_EDGE('',*,*,#26608,.F.);
#34301=ORIENTED_EDGE('',*,*,#26609,.F.);
#34302=ORIENTED_EDGE('',*,*,#26610,.F.);
#34303=ORIENTED_EDGE('',*,*,#26611,.F.);
#34304=ORIENTED_EDGE('',*,*,#25338,.T.);
#34305=ORIENTED_EDGE('',*,*,#26612,.T.);
#34306=ORIENTED_EDGE('',*,*,#26613,.T.);
#34307=ORIENTED_EDGE('',*,*,#26614,.F.);
#34308=ORIENTED_EDGE('',*,*,#26615,.F.);
#34309=ORIENTED_EDGE('',*,*,#26616,.F.);
#34310=ORIENTED_EDGE('',*,*,#26581,.T.);
#34311=ORIENTED_EDGE('',*,*,#25335,.T.);
#34312=ORIENTED_EDGE('',*,*,#26617,.F.);
#34313=ORIENTED_EDGE('',*,*,#26618,.F.);
#34314=ORIENTED_EDGE('',*,*,#26619,.F.);
#34315=ORIENTED_EDGE('',*,*,#26620,.F.);
#34316=ORIENTED_EDGE('',*,*,#26621,.F.);
#34317=ORIENTED_EDGE('',*,*,#26622,.F.);
#34318=ORIENTED_EDGE('',*,*,#26623,.F.);
#34319=ORIENTED_EDGE('',*,*,#26624,.F.);
#34320=ORIENTED_EDGE('',*,*,#26625,.F.);
#34321=ORIENTED_EDGE('',*,*,#26626,.F.);
#34322=ORIENTED_EDGE('',*,*,#26627,.F.);
#34323=ORIENTED_EDGE('',*,*,#26628,.F.);
#34324=ORIENTED_EDGE('',*,*,#26629,.F.);
#34325=ORIENTED_EDGE('',*,*,#26630,.F.);
#34326=ORIENTED_EDGE('',*,*,#26631,.F.);
#34327=ORIENTED_EDGE('',*,*,#26632,.T.);
#34328=ORIENTED_EDGE('',*,*,#26633,.F.);
#34329=ORIENTED_EDGE('',*,*,#26634,.F.);
#34330=ORIENTED_EDGE('',*,*,#26635,.F.);
#34331=ORIENTED_EDGE('',*,*,#26636,.F.);
#34332=ORIENTED_EDGE('',*,*,#26637,.F.);
#34333=ORIENTED_EDGE('',*,*,#26638,.F.);
#34334=ORIENTED_EDGE('',*,*,#26639,.F.);
#34335=ORIENTED_EDGE('',*,*,#26640,.F.);
#34336=ORIENTED_EDGE('',*,*,#26641,.F.);
#34337=ORIENTED_EDGE('',*,*,#26642,.F.);
#34338=ORIENTED_EDGE('',*,*,#26643,.F.);
#34339=ORIENTED_EDGE('',*,*,#26644,.F.);
#34340=ORIENTED_EDGE('',*,*,#26645,.F.);
#34341=ORIENTED_EDGE('',*,*,#26646,.F.);
#34342=ORIENTED_EDGE('',*,*,#26647,.F.);
#34343=ORIENTED_EDGE('',*,*,#25334,.T.);
#34344=ORIENTED_EDGE('',*,*,#26648,.T.);
#34345=ORIENTED_EDGE('',*,*,#26649,.T.);
#34346=ORIENTED_EDGE('',*,*,#26650,.F.);
#34347=ORIENTED_EDGE('',*,*,#26651,.F.);
#34348=ORIENTED_EDGE('',*,*,#26652,.F.);
#34349=ORIENTED_EDGE('',*,*,#26617,.T.);
#34350=ORIENTED_EDGE('',*,*,#25331,.T.);
#34351=ORIENTED_EDGE('',*,*,#26653,.F.);
#34352=ORIENTED_EDGE('',*,*,#26654,.F.);
#34353=ORIENTED_EDGE('',*,*,#26655,.F.);
#34354=ORIENTED_EDGE('',*,*,#26656,.F.);
#34355=ORIENTED_EDGE('',*,*,#26657,.F.);
#34356=ORIENTED_EDGE('',*,*,#26658,.F.);
#34357=ORIENTED_EDGE('',*,*,#26659,.F.);
#34358=ORIENTED_EDGE('',*,*,#26660,.F.);
#34359=ORIENTED_EDGE('',*,*,#26661,.F.);
#34360=ORIENTED_EDGE('',*,*,#26662,.F.);
#34361=ORIENTED_EDGE('',*,*,#26663,.F.);
#34362=ORIENTED_EDGE('',*,*,#26664,.F.);
#34363=ORIENTED_EDGE('',*,*,#26665,.F.);
#34364=ORIENTED_EDGE('',*,*,#26666,.F.);
#34365=ORIENTED_EDGE('',*,*,#26667,.F.);
#34366=ORIENTED_EDGE('',*,*,#26668,.T.);
#34367=ORIENTED_EDGE('',*,*,#26669,.F.);
#34368=ORIENTED_EDGE('',*,*,#26670,.F.);
#34369=ORIENTED_EDGE('',*,*,#26671,.F.);
#34370=ORIENTED_EDGE('',*,*,#26672,.F.);
#34371=ORIENTED_EDGE('',*,*,#26673,.F.);
#34372=ORIENTED_EDGE('',*,*,#26674,.F.);
#34373=ORIENTED_EDGE('',*,*,#26675,.F.);
#34374=ORIENTED_EDGE('',*,*,#26676,.F.);
#34375=ORIENTED_EDGE('',*,*,#26677,.F.);
#34376=ORIENTED_EDGE('',*,*,#26678,.F.);
#34377=ORIENTED_EDGE('',*,*,#26679,.F.);
#34378=ORIENTED_EDGE('',*,*,#26680,.F.);
#34379=ORIENTED_EDGE('',*,*,#26681,.F.);
#34380=ORIENTED_EDGE('',*,*,#26682,.F.);
#34381=ORIENTED_EDGE('',*,*,#26683,.F.);
#34382=ORIENTED_EDGE('',*,*,#25330,.T.);
#34383=ORIENTED_EDGE('',*,*,#26684,.T.);
#34384=ORIENTED_EDGE('',*,*,#26685,.T.);
#34385=ORIENTED_EDGE('',*,*,#26686,.F.);
#34386=ORIENTED_EDGE('',*,*,#26687,.F.);
#34387=ORIENTED_EDGE('',*,*,#26688,.F.);
#34388=ORIENTED_EDGE('',*,*,#26653,.T.);
#34389=ORIENTED_EDGE('',*,*,#25327,.T.);
#34390=ORIENTED_EDGE('',*,*,#26689,.F.);
#34391=ORIENTED_EDGE('',*,*,#26690,.F.);
#34392=ORIENTED_EDGE('',*,*,#26691,.F.);
#34393=ORIENTED_EDGE('',*,*,#26692,.F.);
#34394=ORIENTED_EDGE('',*,*,#26693,.F.);
#34395=ORIENTED_EDGE('',*,*,#26694,.F.);
#34396=ORIENTED_EDGE('',*,*,#26695,.F.);
#34397=ORIENTED_EDGE('',*,*,#26696,.F.);
#34398=ORIENTED_EDGE('',*,*,#26697,.F.);
#34399=ORIENTED_EDGE('',*,*,#26698,.F.);
#34400=ORIENTED_EDGE('',*,*,#26699,.F.);
#34401=ORIENTED_EDGE('',*,*,#26700,.F.);
#34402=ORIENTED_EDGE('',*,*,#26701,.F.);
#34403=ORIENTED_EDGE('',*,*,#26702,.F.);
#34404=ORIENTED_EDGE('',*,*,#26703,.F.);
#34405=ORIENTED_EDGE('',*,*,#26704,.T.);
#34406=ORIENTED_EDGE('',*,*,#26705,.F.);
#34407=ORIENTED_EDGE('',*,*,#26706,.F.);
#34408=ORIENTED_EDGE('',*,*,#26707,.F.);
#34409=ORIENTED_EDGE('',*,*,#26708,.F.);
#34410=ORIENTED_EDGE('',*,*,#26709,.F.);
#34411=ORIENTED_EDGE('',*,*,#26710,.F.);
#34412=ORIENTED_EDGE('',*,*,#26711,.F.);
#34413=ORIENTED_EDGE('',*,*,#26712,.F.);
#34414=ORIENTED_EDGE('',*,*,#26713,.F.);
#34415=ORIENTED_EDGE('',*,*,#26714,.F.);
#34416=ORIENTED_EDGE('',*,*,#26715,.F.);
#34417=ORIENTED_EDGE('',*,*,#26716,.F.);
#34418=ORIENTED_EDGE('',*,*,#26717,.F.);
#34419=ORIENTED_EDGE('',*,*,#26718,.F.);
#34420=ORIENTED_EDGE('',*,*,#26719,.F.);
#34421=ORIENTED_EDGE('',*,*,#25326,.T.);
#34422=ORIENTED_EDGE('',*,*,#26720,.T.);
#34423=ORIENTED_EDGE('',*,*,#26721,.T.);
#34424=ORIENTED_EDGE('',*,*,#26722,.F.);
#34425=ORIENTED_EDGE('',*,*,#26723,.F.);
#34426=ORIENTED_EDGE('',*,*,#26724,.F.);
#34427=ORIENTED_EDGE('',*,*,#26689,.T.);
#34428=ORIENTED_EDGE('',*,*,#25323,.T.);
#34429=ORIENTED_EDGE('',*,*,#26725,.F.);
#34430=ORIENTED_EDGE('',*,*,#26726,.F.);
#34431=ORIENTED_EDGE('',*,*,#26727,.F.);
#34432=ORIENTED_EDGE('',*,*,#26728,.F.);
#34433=ORIENTED_EDGE('',*,*,#26729,.F.);
#34434=ORIENTED_EDGE('',*,*,#26730,.F.);
#34435=ORIENTED_EDGE('',*,*,#26731,.F.);
#34436=ORIENTED_EDGE('',*,*,#26732,.F.);
#34437=ORIENTED_EDGE('',*,*,#26733,.F.);
#34438=ORIENTED_EDGE('',*,*,#26734,.F.);
#34439=ORIENTED_EDGE('',*,*,#26735,.F.);
#34440=ORIENTED_EDGE('',*,*,#26736,.F.);
#34441=ORIENTED_EDGE('',*,*,#26737,.F.);
#34442=ORIENTED_EDGE('',*,*,#26738,.F.);
#34443=ORIENTED_EDGE('',*,*,#26739,.F.);
#34444=ORIENTED_EDGE('',*,*,#26740,.T.);
#34445=ORIENTED_EDGE('',*,*,#26741,.F.);
#34446=ORIENTED_EDGE('',*,*,#26742,.F.);
#34447=ORIENTED_EDGE('',*,*,#26743,.F.);
#34448=ORIENTED_EDGE('',*,*,#26744,.F.);
#34449=ORIENTED_EDGE('',*,*,#26745,.F.);
#34450=ORIENTED_EDGE('',*,*,#26746,.F.);
#34451=ORIENTED_EDGE('',*,*,#26747,.F.);
#34452=ORIENTED_EDGE('',*,*,#26748,.F.);
#34453=ORIENTED_EDGE('',*,*,#26749,.F.);
#34454=ORIENTED_EDGE('',*,*,#26750,.F.);
#34455=ORIENTED_EDGE('',*,*,#26751,.F.);
#34456=ORIENTED_EDGE('',*,*,#26752,.F.);
#34457=ORIENTED_EDGE('',*,*,#26753,.F.);
#34458=ORIENTED_EDGE('',*,*,#26754,.F.);
#34459=ORIENTED_EDGE('',*,*,#26755,.F.);
#34460=ORIENTED_EDGE('',*,*,#25322,.T.);
#34461=ORIENTED_EDGE('',*,*,#26756,.T.);
#34462=ORIENTED_EDGE('',*,*,#26757,.T.);
#34463=ORIENTED_EDGE('',*,*,#26758,.F.);
#34464=ORIENTED_EDGE('',*,*,#26759,.F.);
#34465=ORIENTED_EDGE('',*,*,#26760,.F.);
#34466=ORIENTED_EDGE('',*,*,#26725,.T.);
#34467=ORIENTED_EDGE('',*,*,#26761,.F.);
#34468=ORIENTED_EDGE('',*,*,#26762,.F.);
#34469=ORIENTED_EDGE('',*,*,#26740,.F.);
#34470=ORIENTED_EDGE('',*,*,#26763,.F.);
#34471=ORIENTED_EDGE('',*,*,#26764,.F.);
#34472=ORIENTED_EDGE('',*,*,#26765,.F.);
#34473=ORIENTED_EDGE('',*,*,#26704,.F.);
#34474=ORIENTED_EDGE('',*,*,#26766,.F.);
#34475=ORIENTED_EDGE('',*,*,#26767,.F.);
#34476=ORIENTED_EDGE('',*,*,#26768,.F.);
#34477=ORIENTED_EDGE('',*,*,#26668,.F.);
#34478=ORIENTED_EDGE('',*,*,#26769,.F.);
#34479=ORIENTED_EDGE('',*,*,#26770,.F.);
#34480=ORIENTED_EDGE('',*,*,#26771,.F.);
#34481=ORIENTED_EDGE('',*,*,#26632,.F.);
#34482=ORIENTED_EDGE('',*,*,#26772,.F.);
#34483=ORIENTED_EDGE('',*,*,#26773,.F.);
#34484=ORIENTED_EDGE('',*,*,#26774,.F.);
#34485=ORIENTED_EDGE('',*,*,#26596,.F.);
#34486=ORIENTED_EDGE('',*,*,#26775,.F.);
#34487=ORIENTED_EDGE('',*,*,#26776,.F.);
#34488=ORIENTED_EDGE('',*,*,#26777,.F.);
#34489=ORIENTED_EDGE('',*,*,#26560,.F.);
#34490=ORIENTED_EDGE('',*,*,#26778,.F.);
#34491=ORIENTED_EDGE('',*,*,#26779,.F.);
#34492=ORIENTED_EDGE('',*,*,#26780,.F.);
#34493=ORIENTED_EDGE('',*,*,#26524,.F.);
#34494=ORIENTED_EDGE('',*,*,#26781,.F.);
#34495=ORIENTED_EDGE('',*,*,#26782,.F.);
#34496=ORIENTED_EDGE('',*,*,#26783,.F.);
#34497=ORIENTED_EDGE('',*,*,#26488,.F.);
#34498=ORIENTED_EDGE('',*,*,#26784,.F.);
#34499=ORIENTED_EDGE('',*,*,#26785,.F.);
#34500=ORIENTED_EDGE('',*,*,#26786,.F.);
#34501=ORIENTED_EDGE('',*,*,#26452,.F.);
#34502=ORIENTED_EDGE('',*,*,#26787,.F.);
#34503=ORIENTED_EDGE('',*,*,#26788,.F.);
#34504=ORIENTED_EDGE('',*,*,#26789,.F.);
#34505=ORIENTED_EDGE('',*,*,#26416,.F.);
#34506=ORIENTED_EDGE('',*,*,#26790,.F.);
#34507=ORIENTED_EDGE('',*,*,#26791,.F.);
#34508=ORIENTED_EDGE('',*,*,#26792,.F.);
#34509=ORIENTED_EDGE('',*,*,#26380,.F.);
#34510=ORIENTED_EDGE('',*,*,#26793,.F.);
#34511=ORIENTED_EDGE('',*,*,#26794,.F.);
#34512=ORIENTED_EDGE('',*,*,#26795,.F.);
#34513=ORIENTED_EDGE('',*,*,#26344,.F.);
#34514=ORIENTED_EDGE('',*,*,#26796,.F.);
#34515=ORIENTED_EDGE('',*,*,#26797,.F.);
#34516=ORIENTED_EDGE('',*,*,#26798,.F.);
#34517=ORIENTED_EDGE('',*,*,#26308,.F.);
#34518=ORIENTED_EDGE('',*,*,#26799,.F.);
#34519=ORIENTED_EDGE('',*,*,#26800,.F.);
#34520=ORIENTED_EDGE('',*,*,#26801,.F.);
#34521=ORIENTED_EDGE('',*,*,#26272,.F.);
#34522=ORIENTED_EDGE('',*,*,#26802,.F.);
#34523=ORIENTED_EDGE('',*,*,#26803,.F.);
#34524=ORIENTED_EDGE('',*,*,#26804,.F.);
#34525=ORIENTED_EDGE('',*,*,#26236,.F.);
#34526=ORIENTED_EDGE('',*,*,#26805,.F.);
#34527=ORIENTED_EDGE('',*,*,#26806,.F.);
#34528=ORIENTED_EDGE('',*,*,#26807,.F.);
#34529=ORIENTED_EDGE('',*,*,#26200,.F.);
#34530=ORIENTED_EDGE('',*,*,#26808,.F.);
#34531=ORIENTED_EDGE('',*,*,#26809,.F.);
#34532=ORIENTED_EDGE('',*,*,#26810,.F.);
#34533=ORIENTED_EDGE('',*,*,#26164,.F.);
#34534=ORIENTED_EDGE('',*,*,#26811,.F.);
#34535=ORIENTED_EDGE('',*,*,#26812,.F.);
#34536=ORIENTED_EDGE('',*,*,#26813,.F.);
#34537=ORIENTED_EDGE('',*,*,#26128,.F.);
#34538=ORIENTED_EDGE('',*,*,#26814,.F.);
#34539=ORIENTED_EDGE('',*,*,#26815,.F.);
#34540=ORIENTED_EDGE('',*,*,#26816,.F.);
#34541=ORIENTED_EDGE('',*,*,#26092,.F.);
#34542=ORIENTED_EDGE('',*,*,#26817,.F.);
#34543=ORIENTED_EDGE('',*,*,#26818,.F.);
#34544=ORIENTED_EDGE('',*,*,#26819,.F.);
#34545=ORIENTED_EDGE('',*,*,#26056,.F.);
#34546=ORIENTED_EDGE('',*,*,#26820,.F.);
#34547=ORIENTED_EDGE('',*,*,#26821,.F.);
#34548=ORIENTED_EDGE('',*,*,#26822,.F.);
#34549=ORIENTED_EDGE('',*,*,#26020,.F.);
#34550=ORIENTED_EDGE('',*,*,#26823,.F.);
#34551=ORIENTED_EDGE('',*,*,#26824,.F.);
#34552=ORIENTED_EDGE('',*,*,#26825,.F.);
#34553=ORIENTED_EDGE('',*,*,#25984,.F.);
#34554=ORIENTED_EDGE('',*,*,#26826,.F.);
#34555=ORIENTED_EDGE('',*,*,#26827,.F.);
#34556=ORIENTED_EDGE('',*,*,#26828,.F.);
#34557=ORIENTED_EDGE('',*,*,#25948,.F.);
#34558=ORIENTED_EDGE('',*,*,#26829,.F.);
#34559=ORIENTED_EDGE('',*,*,#26830,.F.);
#34560=ORIENTED_EDGE('',*,*,#26831,.F.);
#34561=ORIENTED_EDGE('',*,*,#25912,.F.);
#34562=ORIENTED_EDGE('',*,*,#26832,.F.);
#34563=ORIENTED_EDGE('',*,*,#26833,.F.);
#34564=ORIENTED_EDGE('',*,*,#26834,.F.);
#34565=ORIENTED_EDGE('',*,*,#25876,.F.);
#34566=ORIENTED_EDGE('',*,*,#26835,.F.);
#34567=ORIENTED_EDGE('',*,*,#26836,.F.);
#34568=ORIENTED_EDGE('',*,*,#26837,.F.);
#34569=ORIENTED_EDGE('',*,*,#25840,.F.);
#34570=ORIENTED_EDGE('',*,*,#26838,.F.);
#34571=ORIENTED_EDGE('',*,*,#26839,.F.);
#34572=ORIENTED_EDGE('',*,*,#26840,.F.);
#34573=ORIENTED_EDGE('',*,*,#25804,.F.);
#34574=ORIENTED_EDGE('',*,*,#26841,.F.);
#34575=ORIENTED_EDGE('',*,*,#26842,.F.);
#34576=ORIENTED_EDGE('',*,*,#26843,.F.);
#34577=ORIENTED_EDGE('',*,*,#25768,.F.);
#34578=ORIENTED_EDGE('',*,*,#26844,.F.);
#34579=ORIENTED_EDGE('',*,*,#26845,.F.);
#34580=ORIENTED_EDGE('',*,*,#26846,.F.);
#34581=ORIENTED_EDGE('',*,*,#25732,.F.);
#34582=ORIENTED_EDGE('',*,*,#26847,.F.);
#34583=ORIENTED_EDGE('',*,*,#26848,.F.);
#34584=ORIENTED_EDGE('',*,*,#26849,.F.);
#34585=ORIENTED_EDGE('',*,*,#25696,.F.);
#34586=ORIENTED_EDGE('',*,*,#26850,.F.);
#34587=ORIENTED_EDGE('',*,*,#26851,.F.);
#34588=ORIENTED_EDGE('',*,*,#26852,.F.);
#34589=ORIENTED_EDGE('',*,*,#25660,.F.);
#34590=ORIENTED_EDGE('',*,*,#26853,.F.);
#34591=ORIENTED_EDGE('',*,*,#26854,.F.);
#34592=ORIENTED_EDGE('',*,*,#26855,.F.);
#34593=ORIENTED_EDGE('',*,*,#25624,.F.);
#34594=ORIENTED_EDGE('',*,*,#26856,.F.);
#34595=ORIENTED_EDGE('',*,*,#26857,.F.);
#34596=ORIENTED_EDGE('',*,*,#26858,.F.);
#34597=ORIENTED_EDGE('',*,*,#25588,.F.);
#34598=ORIENTED_EDGE('',*,*,#26859,.F.);
#34599=ORIENTED_EDGE('',*,*,#26860,.F.);
#34600=ORIENTED_EDGE('',*,*,#26861,.F.);
#34601=ORIENTED_EDGE('',*,*,#25552,.F.);
#34602=ORIENTED_EDGE('',*,*,#26862,.F.);
#34603=ORIENTED_EDGE('',*,*,#26863,.F.);
#34604=ORIENTED_EDGE('',*,*,#26864,.F.);
#34605=ORIENTED_EDGE('',*,*,#25516,.F.);
#34606=ORIENTED_EDGE('',*,*,#26865,.F.);
#34607=ORIENTED_EDGE('',*,*,#26866,.F.);
#34608=ORIENTED_EDGE('',*,*,#26867,.F.);
#34609=ORIENTED_EDGE('',*,*,#25480,.F.);
#34610=ORIENTED_EDGE('',*,*,#26868,.F.);
#34611=ORIENTED_EDGE('',*,*,#26867,.T.);
#34612=ORIENTED_EDGE('',*,*,#26869,.T.);
#34613=ORIENTED_EDGE('',*,*,#26870,.T.);
#34614=ORIENTED_EDGE('',*,*,#26871,.F.);
#34615=ORIENTED_EDGE('',*,*,#26872,.F.);
#34616=ORIENTED_EDGE('',*,*,#26873,.F.);
#34617=ORIENTED_EDGE('',*,*,#25481,.T.);
#34618=ORIENTED_EDGE('',*,*,#26864,.T.);
#34619=ORIENTED_EDGE('',*,*,#26874,.T.);
#34620=ORIENTED_EDGE('',*,*,#26875,.T.);
#34621=ORIENTED_EDGE('',*,*,#26876,.F.);
#34622=ORIENTED_EDGE('',*,*,#26877,.F.);
#34623=ORIENTED_EDGE('',*,*,#26878,.F.);
#34624=ORIENTED_EDGE('',*,*,#25517,.T.);
#34625=ORIENTED_EDGE('',*,*,#26861,.T.);
#34626=ORIENTED_EDGE('',*,*,#26879,.T.);
#34627=ORIENTED_EDGE('',*,*,#26880,.T.);
#34628=ORIENTED_EDGE('',*,*,#26881,.F.);
#34629=ORIENTED_EDGE('',*,*,#26882,.F.);
#34630=ORIENTED_EDGE('',*,*,#26883,.F.);
#34631=ORIENTED_EDGE('',*,*,#25553,.T.);
#34632=ORIENTED_EDGE('',*,*,#26858,.T.);
#34633=ORIENTED_EDGE('',*,*,#26884,.T.);
#34634=ORIENTED_EDGE('',*,*,#26885,.T.);
#34635=ORIENTED_EDGE('',*,*,#26886,.F.);
#34636=ORIENTED_EDGE('',*,*,#26887,.F.);
#34637=ORIENTED_EDGE('',*,*,#26888,.F.);
#34638=ORIENTED_EDGE('',*,*,#25589,.T.);
#34639=ORIENTED_EDGE('',*,*,#26855,.T.);
#34640=ORIENTED_EDGE('',*,*,#26889,.T.);
#34641=ORIENTED_EDGE('',*,*,#26890,.T.);
#34642=ORIENTED_EDGE('',*,*,#26891,.F.);
#34643=ORIENTED_EDGE('',*,*,#26892,.F.);
#34644=ORIENTED_EDGE('',*,*,#26893,.F.);
#34645=ORIENTED_EDGE('',*,*,#25625,.T.);
#34646=ORIENTED_EDGE('',*,*,#26852,.T.);
#34647=ORIENTED_EDGE('',*,*,#26894,.T.);
#34648=ORIENTED_EDGE('',*,*,#26895,.T.);
#34649=ORIENTED_EDGE('',*,*,#26896,.F.);
#34650=ORIENTED_EDGE('',*,*,#26897,.F.);
#34651=ORIENTED_EDGE('',*,*,#26898,.F.);
#34652=ORIENTED_EDGE('',*,*,#25661,.T.);
#34653=ORIENTED_EDGE('',*,*,#26849,.T.);
#34654=ORIENTED_EDGE('',*,*,#26899,.T.);
#34655=ORIENTED_EDGE('',*,*,#26900,.T.);
#34656=ORIENTED_EDGE('',*,*,#26901,.F.);
#34657=ORIENTED_EDGE('',*,*,#26902,.F.);
#34658=ORIENTED_EDGE('',*,*,#26903,.F.);
#34659=ORIENTED_EDGE('',*,*,#25697,.T.);
#34660=ORIENTED_EDGE('',*,*,#26846,.T.);
#34661=ORIENTED_EDGE('',*,*,#26904,.T.);
#34662=ORIENTED_EDGE('',*,*,#26905,.T.);
#34663=ORIENTED_EDGE('',*,*,#26906,.F.);
#34664=ORIENTED_EDGE('',*,*,#26907,.F.);
#34665=ORIENTED_EDGE('',*,*,#26908,.F.);
#34666=ORIENTED_EDGE('',*,*,#25733,.T.);
#34667=ORIENTED_EDGE('',*,*,#26843,.T.);
#34668=ORIENTED_EDGE('',*,*,#26909,.T.);
#34669=ORIENTED_EDGE('',*,*,#26910,.T.);
#34670=ORIENTED_EDGE('',*,*,#26911,.F.);
#34671=ORIENTED_EDGE('',*,*,#26912,.F.);
#34672=ORIENTED_EDGE('',*,*,#26913,.F.);
#34673=ORIENTED_EDGE('',*,*,#25769,.T.);
#34674=ORIENTED_EDGE('',*,*,#26840,.T.);
#34675=ORIENTED_EDGE('',*,*,#26914,.T.);
#34676=ORIENTED_EDGE('',*,*,#26915,.T.);
#34677=ORIENTED_EDGE('',*,*,#26916,.F.);
#34678=ORIENTED_EDGE('',*,*,#26917,.F.);
#34679=ORIENTED_EDGE('',*,*,#26918,.F.);
#34680=ORIENTED_EDGE('',*,*,#25805,.T.);
#34681=ORIENTED_EDGE('',*,*,#26837,.T.);
#34682=ORIENTED_EDGE('',*,*,#26919,.T.);
#34683=ORIENTED_EDGE('',*,*,#26920,.T.);
#34684=ORIENTED_EDGE('',*,*,#26921,.F.);
#34685=ORIENTED_EDGE('',*,*,#26922,.F.);
#34686=ORIENTED_EDGE('',*,*,#26923,.F.);
#34687=ORIENTED_EDGE('',*,*,#25841,.T.);
#34688=ORIENTED_EDGE('',*,*,#26834,.T.);
#34689=ORIENTED_EDGE('',*,*,#26924,.T.);
#34690=ORIENTED_EDGE('',*,*,#26925,.T.);
#34691=ORIENTED_EDGE('',*,*,#26926,.F.);
#34692=ORIENTED_EDGE('',*,*,#26927,.F.);
#34693=ORIENTED_EDGE('',*,*,#26928,.F.);
#34694=ORIENTED_EDGE('',*,*,#25877,.T.);
#34695=ORIENTED_EDGE('',*,*,#26831,.T.);
#34696=ORIENTED_EDGE('',*,*,#26929,.T.);
#34697=ORIENTED_EDGE('',*,*,#26930,.T.);
#34698=ORIENTED_EDGE('',*,*,#26931,.F.);
#34699=ORIENTED_EDGE('',*,*,#26932,.F.);
#34700=ORIENTED_EDGE('',*,*,#26933,.F.);
#34701=ORIENTED_EDGE('',*,*,#25913,.T.);
#34702=ORIENTED_EDGE('',*,*,#26828,.T.);
#34703=ORIENTED_EDGE('',*,*,#26934,.T.);
#34704=ORIENTED_EDGE('',*,*,#26935,.T.);
#34705=ORIENTED_EDGE('',*,*,#26936,.F.);
#34706=ORIENTED_EDGE('',*,*,#26937,.F.);
#34707=ORIENTED_EDGE('',*,*,#26938,.F.);
#34708=ORIENTED_EDGE('',*,*,#25949,.T.);
#34709=ORIENTED_EDGE('',*,*,#26825,.T.);
#34710=ORIENTED_EDGE('',*,*,#26939,.T.);
#34711=ORIENTED_EDGE('',*,*,#26940,.T.);
#34712=ORIENTED_EDGE('',*,*,#26941,.F.);
#34713=ORIENTED_EDGE('',*,*,#26942,.F.);
#34714=ORIENTED_EDGE('',*,*,#26943,.F.);
#34715=ORIENTED_EDGE('',*,*,#25985,.T.);
#34716=ORIENTED_EDGE('',*,*,#26822,.T.);
#34717=ORIENTED_EDGE('',*,*,#26944,.T.);
#34718=ORIENTED_EDGE('',*,*,#26945,.T.);
#34719=ORIENTED_EDGE('',*,*,#26946,.F.);
#34720=ORIENTED_EDGE('',*,*,#26947,.F.);
#34721=ORIENTED_EDGE('',*,*,#26948,.F.);
#34722=ORIENTED_EDGE('',*,*,#26021,.T.);
#34723=ORIENTED_EDGE('',*,*,#26819,.T.);
#34724=ORIENTED_EDGE('',*,*,#26949,.T.);
#34725=ORIENTED_EDGE('',*,*,#26950,.T.);
#34726=ORIENTED_EDGE('',*,*,#26951,.F.);
#34727=ORIENTED_EDGE('',*,*,#26952,.F.);
#34728=ORIENTED_EDGE('',*,*,#26953,.F.);
#34729=ORIENTED_EDGE('',*,*,#26057,.T.);
#34730=ORIENTED_EDGE('',*,*,#26816,.T.);
#34731=ORIENTED_EDGE('',*,*,#26954,.T.);
#34732=ORIENTED_EDGE('',*,*,#26955,.T.);
#34733=ORIENTED_EDGE('',*,*,#26956,.F.);
#34734=ORIENTED_EDGE('',*,*,#26957,.F.);
#34735=ORIENTED_EDGE('',*,*,#26958,.F.);
#34736=ORIENTED_EDGE('',*,*,#26093,.T.);
#34737=ORIENTED_EDGE('',*,*,#26813,.T.);
#34738=ORIENTED_EDGE('',*,*,#26959,.T.);
#34739=ORIENTED_EDGE('',*,*,#26960,.T.);
#34740=ORIENTED_EDGE('',*,*,#26961,.F.);
#34741=ORIENTED_EDGE('',*,*,#26962,.F.);
#34742=ORIENTED_EDGE('',*,*,#26963,.F.);
#34743=ORIENTED_EDGE('',*,*,#26129,.T.);
#34744=ORIENTED_EDGE('',*,*,#26810,.T.);
#34745=ORIENTED_EDGE('',*,*,#26964,.T.);
#34746=ORIENTED_EDGE('',*,*,#26965,.T.);
#34747=ORIENTED_EDGE('',*,*,#26966,.F.);
#34748=ORIENTED_EDGE('',*,*,#26967,.F.);
#34749=ORIENTED_EDGE('',*,*,#26968,.F.);
#34750=ORIENTED_EDGE('',*,*,#26165,.T.);
#34751=ORIENTED_EDGE('',*,*,#26807,.T.);
#34752=ORIENTED_EDGE('',*,*,#26969,.T.);
#34753=ORIENTED_EDGE('',*,*,#26970,.T.);
#34754=ORIENTED_EDGE('',*,*,#26971,.F.);
#34755=ORIENTED_EDGE('',*,*,#26972,.F.);
#34756=ORIENTED_EDGE('',*,*,#26973,.F.);
#34757=ORIENTED_EDGE('',*,*,#26201,.T.);
#34758=ORIENTED_EDGE('',*,*,#26804,.T.);
#34759=ORIENTED_EDGE('',*,*,#26974,.T.);
#34760=ORIENTED_EDGE('',*,*,#26975,.T.);
#34761=ORIENTED_EDGE('',*,*,#26976,.F.);
#34762=ORIENTED_EDGE('',*,*,#26977,.F.);
#34763=ORIENTED_EDGE('',*,*,#26978,.F.);
#34764=ORIENTED_EDGE('',*,*,#26237,.T.);
#34765=ORIENTED_EDGE('',*,*,#26801,.T.);
#34766=ORIENTED_EDGE('',*,*,#26979,.T.);
#34767=ORIENTED_EDGE('',*,*,#26980,.T.);
#34768=ORIENTED_EDGE('',*,*,#26981,.F.);
#34769=ORIENTED_EDGE('',*,*,#26982,.F.);
#34770=ORIENTED_EDGE('',*,*,#26983,.F.);
#34771=ORIENTED_EDGE('',*,*,#26273,.T.);
#34772=ORIENTED_EDGE('',*,*,#26798,.T.);
#34773=ORIENTED_EDGE('',*,*,#26984,.T.);
#34774=ORIENTED_EDGE('',*,*,#26985,.T.);
#34775=ORIENTED_EDGE('',*,*,#26986,.F.);
#34776=ORIENTED_EDGE('',*,*,#26987,.F.);
#34777=ORIENTED_EDGE('',*,*,#26988,.F.);
#34778=ORIENTED_EDGE('',*,*,#26309,.T.);
#34779=ORIENTED_EDGE('',*,*,#26795,.T.);
#34780=ORIENTED_EDGE('',*,*,#26989,.T.);
#34781=ORIENTED_EDGE('',*,*,#26990,.T.);
#34782=ORIENTED_EDGE('',*,*,#26991,.F.);
#34783=ORIENTED_EDGE('',*,*,#26992,.F.);
#34784=ORIENTED_EDGE('',*,*,#26993,.F.);
#34785=ORIENTED_EDGE('',*,*,#26345,.T.);
#34786=ORIENTED_EDGE('',*,*,#26792,.T.);
#34787=ORIENTED_EDGE('',*,*,#26994,.T.);
#34788=ORIENTED_EDGE('',*,*,#26995,.T.);
#34789=ORIENTED_EDGE('',*,*,#26996,.F.);
#34790=ORIENTED_EDGE('',*,*,#26997,.F.);
#34791=ORIENTED_EDGE('',*,*,#26998,.F.);
#34792=ORIENTED_EDGE('',*,*,#26381,.T.);
#34793=ORIENTED_EDGE('',*,*,#26789,.T.);
#34794=ORIENTED_EDGE('',*,*,#26999,.T.);
#34795=ORIENTED_EDGE('',*,*,#27000,.T.);
#34796=ORIENTED_EDGE('',*,*,#27001,.F.);
#34797=ORIENTED_EDGE('',*,*,#27002,.F.);
#34798=ORIENTED_EDGE('',*,*,#27003,.F.);
#34799=ORIENTED_EDGE('',*,*,#26417,.T.);
#34800=ORIENTED_EDGE('',*,*,#26786,.T.);
#34801=ORIENTED_EDGE('',*,*,#27004,.T.);
#34802=ORIENTED_EDGE('',*,*,#27005,.T.);
#34803=ORIENTED_EDGE('',*,*,#27006,.F.);
#34804=ORIENTED_EDGE('',*,*,#27007,.F.);
#34805=ORIENTED_EDGE('',*,*,#27008,.F.);
#34806=ORIENTED_EDGE('',*,*,#26453,.T.);
#34807=ORIENTED_EDGE('',*,*,#26783,.T.);
#34808=ORIENTED_EDGE('',*,*,#27009,.T.);
#34809=ORIENTED_EDGE('',*,*,#27010,.T.);
#34810=ORIENTED_EDGE('',*,*,#27011,.F.);
#34811=ORIENTED_EDGE('',*,*,#27012,.F.);
#34812=ORIENTED_EDGE('',*,*,#27013,.F.);
#34813=ORIENTED_EDGE('',*,*,#26489,.T.);
#34814=ORIENTED_EDGE('',*,*,#26780,.T.);
#34815=ORIENTED_EDGE('',*,*,#27014,.T.);
#34816=ORIENTED_EDGE('',*,*,#27015,.T.);
#34817=ORIENTED_EDGE('',*,*,#27016,.F.);
#34818=ORIENTED_EDGE('',*,*,#27017,.F.);
#34819=ORIENTED_EDGE('',*,*,#27018,.F.);
#34820=ORIENTED_EDGE('',*,*,#26525,.T.);
#34821=ORIENTED_EDGE('',*,*,#26777,.T.);
#34822=ORIENTED_EDGE('',*,*,#27019,.T.);
#34823=ORIENTED_EDGE('',*,*,#27020,.T.);
#34824=ORIENTED_EDGE('',*,*,#27021,.F.);
#34825=ORIENTED_EDGE('',*,*,#27022,.F.);
#34826=ORIENTED_EDGE('',*,*,#27023,.F.);
#34827=ORIENTED_EDGE('',*,*,#26561,.T.);
#34828=ORIENTED_EDGE('',*,*,#26774,.T.);
#34829=ORIENTED_EDGE('',*,*,#27024,.T.);
#34830=ORIENTED_EDGE('',*,*,#27025,.T.);
#34831=ORIENTED_EDGE('',*,*,#27026,.F.);
#34832=ORIENTED_EDGE('',*,*,#27027,.F.);
#34833=ORIENTED_EDGE('',*,*,#27028,.F.);
#34834=ORIENTED_EDGE('',*,*,#26597,.T.);
#34835=ORIENTED_EDGE('',*,*,#26771,.T.);
#34836=ORIENTED_EDGE('',*,*,#27029,.T.);
#34837=ORIENTED_EDGE('',*,*,#27030,.T.);
#34838=ORIENTED_EDGE('',*,*,#27031,.F.);
#34839=ORIENTED_EDGE('',*,*,#27032,.F.);
#34840=ORIENTED_EDGE('',*,*,#27033,.F.);
#34841=ORIENTED_EDGE('',*,*,#26633,.T.);
#34842=ORIENTED_EDGE('',*,*,#26768,.T.);
#34843=ORIENTED_EDGE('',*,*,#27034,.T.);
#34844=ORIENTED_EDGE('',*,*,#27035,.T.);
#34845=ORIENTED_EDGE('',*,*,#27036,.F.);
#34846=ORIENTED_EDGE('',*,*,#27037,.F.);
#34847=ORIENTED_EDGE('',*,*,#27038,.F.);
#34848=ORIENTED_EDGE('',*,*,#26669,.T.);
#34849=ORIENTED_EDGE('',*,*,#26765,.T.);
#34850=ORIENTED_EDGE('',*,*,#27039,.T.);
#34851=ORIENTED_EDGE('',*,*,#27040,.T.);
#34852=ORIENTED_EDGE('',*,*,#27041,.F.);
#34853=ORIENTED_EDGE('',*,*,#27042,.F.);
#34854=ORIENTED_EDGE('',*,*,#27043,.F.);
#34855=ORIENTED_EDGE('',*,*,#26705,.T.);
#34856=ORIENTED_EDGE('',*,*,#26762,.T.);
#34857=ORIENTED_EDGE('',*,*,#27044,.T.);
#34858=ORIENTED_EDGE('',*,*,#27045,.T.);
#34859=ORIENTED_EDGE('',*,*,#27046,.F.);
#34860=ORIENTED_EDGE('',*,*,#27047,.F.);
#34861=ORIENTED_EDGE('',*,*,#27048,.F.);
#34862=ORIENTED_EDGE('',*,*,#26741,.T.);
#34863=ORIENTED_EDGE('',*,*,#25461,.T.);
#34864=ORIENTED_EDGE('',*,*,#27049,.F.);
#34865=ORIENTED_EDGE('',*,*,#27050,.F.);
#34866=ORIENTED_EDGE('',*,*,#25496,.F.);
#34867=ORIENTED_EDGE('',*,*,#25457,.T.);
#34868=ORIENTED_EDGE('',*,*,#27051,.F.);
#34869=ORIENTED_EDGE('',*,*,#27052,.F.);
#34870=ORIENTED_EDGE('',*,*,#25532,.F.);
#34871=ORIENTED_EDGE('',*,*,#25453,.T.);
#34872=ORIENTED_EDGE('',*,*,#27053,.F.);
#34873=ORIENTED_EDGE('',*,*,#27054,.F.);
#34874=ORIENTED_EDGE('',*,*,#25568,.F.);
#34875=ORIENTED_EDGE('',*,*,#25449,.T.);
#34876=ORIENTED_EDGE('',*,*,#27055,.F.);
#34877=ORIENTED_EDGE('',*,*,#27056,.F.);
#34878=ORIENTED_EDGE('',*,*,#25604,.F.);
#34879=ORIENTED_EDGE('',*,*,#25445,.T.);
#34880=ORIENTED_EDGE('',*,*,#27057,.F.);
#34881=ORIENTED_EDGE('',*,*,#27058,.F.);
#34882=ORIENTED_EDGE('',*,*,#25640,.F.);
#34883=ORIENTED_EDGE('',*,*,#25441,.T.);
#34884=ORIENTED_EDGE('',*,*,#27059,.F.);
#34885=ORIENTED_EDGE('',*,*,#27060,.F.);
#34886=ORIENTED_EDGE('',*,*,#25676,.F.);
#34887=ORIENTED_EDGE('',*,*,#25437,.T.);
#34888=ORIENTED_EDGE('',*,*,#27061,.F.);
#34889=ORIENTED_EDGE('',*,*,#27062,.F.);
#34890=ORIENTED_EDGE('',*,*,#25712,.F.);
#34891=ORIENTED_EDGE('',*,*,#25433,.T.);
#34892=ORIENTED_EDGE('',*,*,#27063,.F.);
#34893=ORIENTED_EDGE('',*,*,#27064,.F.);
#34894=ORIENTED_EDGE('',*,*,#25748,.F.);
#34895=ORIENTED_EDGE('',*,*,#25429,.T.);
#34896=ORIENTED_EDGE('',*,*,#27065,.F.);
#34897=ORIENTED_EDGE('',*,*,#27066,.F.);
#34898=ORIENTED_EDGE('',*,*,#25784,.F.);
#34899=ORIENTED_EDGE('',*,*,#25425,.T.);
#34900=ORIENTED_EDGE('',*,*,#27067,.F.);
#34901=ORIENTED_EDGE('',*,*,#27068,.F.);
#34902=ORIENTED_EDGE('',*,*,#25820,.F.);
#34903=ORIENTED_EDGE('',*,*,#25421,.T.);
#34904=ORIENTED_EDGE('',*,*,#27069,.F.);
#34905=ORIENTED_EDGE('',*,*,#27070,.F.);
#34906=ORIENTED_EDGE('',*,*,#25856,.F.);
#34907=ORIENTED_EDGE('',*,*,#25417,.T.);
#34908=ORIENTED_EDGE('',*,*,#27071,.F.);
#34909=ORIENTED_EDGE('',*,*,#27072,.F.);
#34910=ORIENTED_EDGE('',*,*,#25892,.F.);
#34911=ORIENTED_EDGE('',*,*,#25413,.T.);
#34912=ORIENTED_EDGE('',*,*,#27073,.F.);
#34913=ORIENTED_EDGE('',*,*,#27074,.F.);
#34914=ORIENTED_EDGE('',*,*,#25928,.F.);
#34915=ORIENTED_EDGE('',*,*,#25409,.T.);
#34916=ORIENTED_EDGE('',*,*,#27075,.F.);
#34917=ORIENTED_EDGE('',*,*,#27076,.F.);
#34918=ORIENTED_EDGE('',*,*,#25964,.F.);
#34919=ORIENTED_EDGE('',*,*,#25405,.T.);
#34920=ORIENTED_EDGE('',*,*,#27077,.F.);
#34921=ORIENTED_EDGE('',*,*,#27078,.F.);
#34922=ORIENTED_EDGE('',*,*,#26000,.F.);
#34923=ORIENTED_EDGE('',*,*,#25401,.T.);
#34924=ORIENTED_EDGE('',*,*,#27079,.F.);
#34925=ORIENTED_EDGE('',*,*,#27080,.F.);
#34926=ORIENTED_EDGE('',*,*,#26036,.F.);
#34927=ORIENTED_EDGE('',*,*,#25397,.T.);
#34928=ORIENTED_EDGE('',*,*,#27081,.F.);
#34929=ORIENTED_EDGE('',*,*,#27082,.F.);
#34930=ORIENTED_EDGE('',*,*,#26072,.F.);
#34931=ORIENTED_EDGE('',*,*,#25393,.T.);
#34932=ORIENTED_EDGE('',*,*,#27083,.F.);
#34933=ORIENTED_EDGE('',*,*,#27084,.F.);
#34934=ORIENTED_EDGE('',*,*,#26108,.F.);
#34935=ORIENTED_EDGE('',*,*,#25389,.T.);
#34936=ORIENTED_EDGE('',*,*,#27085,.F.);
#34937=ORIENTED_EDGE('',*,*,#27086,.F.);
#34938=ORIENTED_EDGE('',*,*,#26144,.F.);
#34939=ORIENTED_EDGE('',*,*,#25385,.T.);
#34940=ORIENTED_EDGE('',*,*,#27087,.F.);
#34941=ORIENTED_EDGE('',*,*,#27088,.F.);
#34942=ORIENTED_EDGE('',*,*,#26180,.F.);
#34943=ORIENTED_EDGE('',*,*,#25381,.T.);
#34944=ORIENTED_EDGE('',*,*,#27089,.F.);
#34945=ORIENTED_EDGE('',*,*,#27090,.F.);
#34946=ORIENTED_EDGE('',*,*,#26216,.F.);
#34947=ORIENTED_EDGE('',*,*,#25377,.T.);
#34948=ORIENTED_EDGE('',*,*,#27091,.F.);
#34949=ORIENTED_EDGE('',*,*,#27092,.F.);
#34950=ORIENTED_EDGE('',*,*,#26252,.F.);
#34951=ORIENTED_EDGE('',*,*,#25373,.T.);
#34952=ORIENTED_EDGE('',*,*,#27093,.F.);
#34953=ORIENTED_EDGE('',*,*,#27094,.F.);
#34954=ORIENTED_EDGE('',*,*,#26288,.F.);
#34955=ORIENTED_EDGE('',*,*,#25369,.T.);
#34956=ORIENTED_EDGE('',*,*,#27095,.F.);
#34957=ORIENTED_EDGE('',*,*,#27096,.F.);
#34958=ORIENTED_EDGE('',*,*,#26324,.F.);
#34959=ORIENTED_EDGE('',*,*,#25365,.T.);
#34960=ORIENTED_EDGE('',*,*,#27097,.F.);
#34961=ORIENTED_EDGE('',*,*,#27098,.F.);
#34962=ORIENTED_EDGE('',*,*,#26360,.F.);
#34963=ORIENTED_EDGE('',*,*,#25361,.T.);
#34964=ORIENTED_EDGE('',*,*,#27099,.F.);
#34965=ORIENTED_EDGE('',*,*,#27100,.F.);
#34966=ORIENTED_EDGE('',*,*,#26396,.F.);
#34967=ORIENTED_EDGE('',*,*,#25357,.T.);
#34968=ORIENTED_EDGE('',*,*,#27101,.F.);
#34969=ORIENTED_EDGE('',*,*,#27102,.F.);
#34970=ORIENTED_EDGE('',*,*,#26432,.F.);
#34971=ORIENTED_EDGE('',*,*,#25353,.T.);
#34972=ORIENTED_EDGE('',*,*,#27103,.F.);
#34973=ORIENTED_EDGE('',*,*,#27104,.F.);
#34974=ORIENTED_EDGE('',*,*,#26468,.F.);
#34975=ORIENTED_EDGE('',*,*,#25349,.T.);
#34976=ORIENTED_EDGE('',*,*,#27105,.F.);
#34977=ORIENTED_EDGE('',*,*,#27106,.F.);
#34978=ORIENTED_EDGE('',*,*,#26504,.F.);
#34979=ORIENTED_EDGE('',*,*,#25345,.T.);
#34980=ORIENTED_EDGE('',*,*,#27107,.F.);
#34981=ORIENTED_EDGE('',*,*,#27108,.F.);
#34982=ORIENTED_EDGE('',*,*,#26540,.F.);
#34983=ORIENTED_EDGE('',*,*,#25341,.T.);
#34984=ORIENTED_EDGE('',*,*,#27109,.F.);
#34985=ORIENTED_EDGE('',*,*,#27110,.F.);
#34986=ORIENTED_EDGE('',*,*,#26576,.F.);
#34987=ORIENTED_EDGE('',*,*,#25337,.T.);
#34988=ORIENTED_EDGE('',*,*,#27111,.F.);
#34989=ORIENTED_EDGE('',*,*,#27112,.F.);
#34990=ORIENTED_EDGE('',*,*,#26612,.F.);
#34991=ORIENTED_EDGE('',*,*,#25333,.T.);
#34992=ORIENTED_EDGE('',*,*,#27113,.F.);
#34993=ORIENTED_EDGE('',*,*,#27114,.F.);
#34994=ORIENTED_EDGE('',*,*,#26648,.F.);
#34995=ORIENTED_EDGE('',*,*,#25329,.T.);
#34996=ORIENTED_EDGE('',*,*,#27115,.F.);
#34997=ORIENTED_EDGE('',*,*,#27116,.F.);
#34998=ORIENTED_EDGE('',*,*,#26684,.F.);
#34999=ORIENTED_EDGE('',*,*,#25325,.T.);
#35000=ORIENTED_EDGE('',*,*,#27117,.F.);
#35001=ORIENTED_EDGE('',*,*,#27118,.F.);
#35002=ORIENTED_EDGE('',*,*,#26720,.F.);
#35003=ORIENTED_EDGE('',*,*,#25321,.T.);
#35004=ORIENTED_EDGE('',*,*,#27119,.F.);
#35005=ORIENTED_EDGE('',*,*,#27120,.F.);
#35006=ORIENTED_EDGE('',*,*,#26756,.F.);
#35007=ORIENTED_EDGE('',*,*,#25324,.T.);
#35008=ORIENTED_EDGE('',*,*,#26755,.T.);
#35009=ORIENTED_EDGE('',*,*,#27121,.T.);
#35010=ORIENTED_EDGE('',*,*,#27122,.F.);
#35011=ORIENTED_EDGE('',*,*,#27123,.F.);
#35012=ORIENTED_EDGE('',*,*,#27124,.T.);
#35013=ORIENTED_EDGE('',*,*,#27119,.T.);
#35014=ORIENTED_EDGE('',*,*,#25328,.T.);
#35015=ORIENTED_EDGE('',*,*,#26719,.T.);
#35016=ORIENTED_EDGE('',*,*,#27125,.T.);
#35017=ORIENTED_EDGE('',*,*,#27126,.F.);
#35018=ORIENTED_EDGE('',*,*,#27127,.F.);
#35019=ORIENTED_EDGE('',*,*,#27128,.T.);
#35020=ORIENTED_EDGE('',*,*,#27117,.T.);
#35021=ORIENTED_EDGE('',*,*,#25332,.T.);
#35022=ORIENTED_EDGE('',*,*,#26683,.T.);
#35023=ORIENTED_EDGE('',*,*,#27129,.T.);
#35024=ORIENTED_EDGE('',*,*,#27130,.F.);
#35025=ORIENTED_EDGE('',*,*,#27131,.F.);
#35026=ORIENTED_EDGE('',*,*,#27132,.T.);
#35027=ORIENTED_EDGE('',*,*,#27115,.T.);
#35028=ORIENTED_EDGE('',*,*,#25336,.T.);
#35029=ORIENTED_EDGE('',*,*,#26647,.T.);
#35030=ORIENTED_EDGE('',*,*,#27133,.T.);
#35031=ORIENTED_EDGE('',*,*,#27134,.F.);
#35032=ORIENTED_EDGE('',*,*,#27135,.F.);
#35033=ORIENTED_EDGE('',*,*,#27136,.T.);
#35034=ORIENTED_EDGE('',*,*,#27113,.T.);
#35035=ORIENTED_EDGE('',*,*,#25340,.T.);
#35036=ORIENTED_EDGE('',*,*,#26611,.T.);
#35037=ORIENTED_EDGE('',*,*,#27137,.T.);
#35038=ORIENTED_EDGE('',*,*,#27138,.F.);
#35039=ORIENTED_EDGE('',*,*,#27139,.F.);
#35040=ORIENTED_EDGE('',*,*,#27140,.T.);
#35041=ORIENTED_EDGE('',*,*,#27111,.T.);
#35042=ORIENTED_EDGE('',*,*,#25344,.T.);
#35043=ORIENTED_EDGE('',*,*,#26575,.T.);
#35044=ORIENTED_EDGE('',*,*,#27141,.T.);
#35045=ORIENTED_EDGE('',*,*,#27142,.F.);
#35046=ORIENTED_EDGE('',*,*,#27143,.F.);
#35047=ORIENTED_EDGE('',*,*,#27144,.T.);
#35048=ORIENTED_EDGE('',*,*,#27109,.T.);
#35049=ORIENTED_EDGE('',*,*,#25348,.T.);
#35050=ORIENTED_EDGE('',*,*,#26539,.T.);
#35051=ORIENTED_EDGE('',*,*,#27145,.T.);
#35052=ORIENTED_EDGE('',*,*,#27146,.F.);
#35053=ORIENTED_EDGE('',*,*,#27147,.F.);
#35054=ORIENTED_EDGE('',*,*,#27148,.T.);
#35055=ORIENTED_EDGE('',*,*,#27107,.T.);
#35056=ORIENTED_EDGE('',*,*,#25352,.T.);
#35057=ORIENTED_EDGE('',*,*,#26503,.T.);
#35058=ORIENTED_EDGE('',*,*,#27149,.T.);
#35059=ORIENTED_EDGE('',*,*,#27150,.F.);
#35060=ORIENTED_EDGE('',*,*,#27151,.F.);
#35061=ORIENTED_EDGE('',*,*,#27152,.T.);
#35062=ORIENTED_EDGE('',*,*,#27105,.T.);
#35063=ORIENTED_EDGE('',*,*,#25356,.T.);
#35064=ORIENTED_EDGE('',*,*,#26467,.T.);
#35065=ORIENTED_EDGE('',*,*,#27153,.T.);
#35066=ORIENTED_EDGE('',*,*,#27154,.F.);
#35067=ORIENTED_EDGE('',*,*,#27155,.F.);
#35068=ORIENTED_EDGE('',*,*,#27156,.T.);
#35069=ORIENTED_EDGE('',*,*,#27103,.T.);
#35070=ORIENTED_EDGE('',*,*,#25360,.T.);
#35071=ORIENTED_EDGE('',*,*,#26431,.T.);
#35072=ORIENTED_EDGE('',*,*,#27157,.T.);
#35073=ORIENTED_EDGE('',*,*,#27158,.F.);
#35074=ORIENTED_EDGE('',*,*,#27159,.F.);
#35075=ORIENTED_EDGE('',*,*,#27160,.T.);
#35076=ORIENTED_EDGE('',*,*,#27101,.T.);
#35077=ORIENTED_EDGE('',*,*,#25364,.T.);
#35078=ORIENTED_EDGE('',*,*,#26395,.T.);
#35079=ORIENTED_EDGE('',*,*,#27161,.T.);
#35080=ORIENTED_EDGE('',*,*,#27162,.F.);
#35081=ORIENTED_EDGE('',*,*,#27163,.F.);
#35082=ORIENTED_EDGE('',*,*,#27164,.T.);
#35083=ORIENTED_EDGE('',*,*,#27099,.T.);
#35084=ORIENTED_EDGE('',*,*,#25368,.T.);
#35085=ORIENTED_EDGE('',*,*,#26359,.T.);
#35086=ORIENTED_EDGE('',*,*,#27165,.T.);
#35087=ORIENTED_EDGE('',*,*,#27166,.F.);
#35088=ORIENTED_EDGE('',*,*,#27167,.F.);
#35089=ORIENTED_EDGE('',*,*,#27168,.T.);
#35090=ORIENTED_EDGE('',*,*,#27097,.T.);
#35091=ORIENTED_EDGE('',*,*,#25372,.T.);
#35092=ORIENTED_EDGE('',*,*,#26323,.T.);
#35093=ORIENTED_EDGE('',*,*,#27169,.T.);
#35094=ORIENTED_EDGE('',*,*,#27170,.F.);
#35095=ORIENTED_EDGE('',*,*,#27171,.F.);
#35096=ORIENTED_EDGE('',*,*,#27172,.T.);
#35097=ORIENTED_EDGE('',*,*,#27095,.T.);
#35098=ORIENTED_EDGE('',*,*,#25376,.T.);
#35099=ORIENTED_EDGE('',*,*,#26287,.T.);
#35100=ORIENTED_EDGE('',*,*,#27173,.T.);
#35101=ORIENTED_EDGE('',*,*,#27174,.F.);
#35102=ORIENTED_EDGE('',*,*,#27175,.F.);
#35103=ORIENTED_EDGE('',*,*,#27176,.T.);
#35104=ORIENTED_EDGE('',*,*,#27093,.T.);
#35105=ORIENTED_EDGE('',*,*,#25380,.T.);
#35106=ORIENTED_EDGE('',*,*,#26251,.T.);
#35107=ORIENTED_EDGE('',*,*,#27177,.T.);
#35108=ORIENTED_EDGE('',*,*,#27178,.F.);
#35109=ORIENTED_EDGE('',*,*,#27179,.F.);
#35110=ORIENTED_EDGE('',*,*,#27180,.T.);
#35111=ORIENTED_EDGE('',*,*,#27091,.T.);
#35112=ORIENTED_EDGE('',*,*,#25384,.T.);
#35113=ORIENTED_EDGE('',*,*,#26215,.T.);
#35114=ORIENTED_EDGE('',*,*,#27181,.T.);
#35115=ORIENTED_EDGE('',*,*,#27182,.F.);
#35116=ORIENTED_EDGE('',*,*,#27183,.F.);
#35117=ORIENTED_EDGE('',*,*,#27184,.T.);
#35118=ORIENTED_EDGE('',*,*,#27089,.T.);
#35119=ORIENTED_EDGE('',*,*,#25388,.T.);
#35120=ORIENTED_EDGE('',*,*,#26179,.T.);
#35121=ORIENTED_EDGE('',*,*,#27185,.T.);
#35122=ORIENTED_EDGE('',*,*,#27186,.F.);
#35123=ORIENTED_EDGE('',*,*,#27187,.F.);
#35124=ORIENTED_EDGE('',*,*,#27188,.T.);
#35125=ORIENTED_EDGE('',*,*,#27087,.T.);
#35126=ORIENTED_EDGE('',*,*,#25392,.T.);
#35127=ORIENTED_EDGE('',*,*,#26143,.T.);
#35128=ORIENTED_EDGE('',*,*,#27189,.T.);
#35129=ORIENTED_EDGE('',*,*,#27190,.F.);
#35130=ORIENTED_EDGE('',*,*,#27191,.F.);
#35131=ORIENTED_EDGE('',*,*,#27192,.T.);
#35132=ORIENTED_EDGE('',*,*,#27085,.T.);
#35133=ORIENTED_EDGE('',*,*,#25396,.T.);
#35134=ORIENTED_EDGE('',*,*,#26107,.T.);
#35135=ORIENTED_EDGE('',*,*,#27193,.T.);
#35136=ORIENTED_EDGE('',*,*,#27194,.F.);
#35137=ORIENTED_EDGE('',*,*,#27195,.F.);
#35138=ORIENTED_EDGE('',*,*,#27196,.T.);
#35139=ORIENTED_EDGE('',*,*,#27083,.T.);
#35140=ORIENTED_EDGE('',*,*,#25400,.T.);
#35141=ORIENTED_EDGE('',*,*,#26071,.T.);
#35142=ORIENTED_EDGE('',*,*,#27197,.T.);
#35143=ORIENTED_EDGE('',*,*,#27198,.F.);
#35144=ORIENTED_EDGE('',*,*,#27199,.F.);
#35145=ORIENTED_EDGE('',*,*,#27200,.T.);
#35146=ORIENTED_EDGE('',*,*,#27081,.T.);
#35147=ORIENTED_EDGE('',*,*,#25404,.T.);
#35148=ORIENTED_EDGE('',*,*,#26035,.T.);
#35149=ORIENTED_EDGE('',*,*,#27201,.T.);
#35150=ORIENTED_EDGE('',*,*,#27202,.F.);
#35151=ORIENTED_EDGE('',*,*,#27203,.F.);
#35152=ORIENTED_EDGE('',*,*,#27204,.T.);
#35153=ORIENTED_EDGE('',*,*,#27079,.T.);
#35154=ORIENTED_EDGE('',*,*,#25408,.T.);
#35155=ORIENTED_EDGE('',*,*,#25999,.T.);
#35156=ORIENTED_EDGE('',*,*,#27205,.T.);
#35157=ORIENTED_EDGE('',*,*,#27206,.F.);
#35158=ORIENTED_EDGE('',*,*,#27207,.F.);
#35159=ORIENTED_EDGE('',*,*,#27208,.T.);
#35160=ORIENTED_EDGE('',*,*,#27077,.T.);
#35161=ORIENTED_EDGE('',*,*,#25412,.T.);
#35162=ORIENTED_EDGE('',*,*,#25963,.T.);
#35163=ORIENTED_EDGE('',*,*,#27209,.T.);
#35164=ORIENTED_EDGE('',*,*,#27210,.F.);
#35165=ORIENTED_EDGE('',*,*,#27211,.F.);
#35166=ORIENTED_EDGE('',*,*,#27212,.T.);
#35167=ORIENTED_EDGE('',*,*,#27075,.T.);
#35168=ORIENTED_EDGE('',*,*,#25416,.T.);
#35169=ORIENTED_EDGE('',*,*,#25927,.T.);
#35170=ORIENTED_EDGE('',*,*,#27213,.T.);
#35171=ORIENTED_EDGE('',*,*,#27214,.F.);
#35172=ORIENTED_EDGE('',*,*,#27215,.F.);
#35173=ORIENTED_EDGE('',*,*,#27216,.T.);
#35174=ORIENTED_EDGE('',*,*,#27073,.T.);
#35175=ORIENTED_EDGE('',*,*,#25420,.T.);
#35176=ORIENTED_EDGE('',*,*,#25891,.T.);
#35177=ORIENTED_EDGE('',*,*,#27217,.T.);
#35178=ORIENTED_EDGE('',*,*,#27218,.F.);
#35179=ORIENTED_EDGE('',*,*,#27219,.F.);
#35180=ORIENTED_EDGE('',*,*,#27220,.T.);
#35181=ORIENTED_EDGE('',*,*,#27071,.T.);
#35182=ORIENTED_EDGE('',*,*,#25424,.T.);
#35183=ORIENTED_EDGE('',*,*,#25855,.T.);
#35184=ORIENTED_EDGE('',*,*,#27221,.T.);
#35185=ORIENTED_EDGE('',*,*,#27222,.F.);
#35186=ORIENTED_EDGE('',*,*,#27223,.F.);
#35187=ORIENTED_EDGE('',*,*,#27224,.T.);
#35188=ORIENTED_EDGE('',*,*,#27069,.T.);
#35189=ORIENTED_EDGE('',*,*,#25428,.T.);
#35190=ORIENTED_EDGE('',*,*,#25819,.T.);
#35191=ORIENTED_EDGE('',*,*,#27225,.T.);
#35192=ORIENTED_EDGE('',*,*,#27226,.F.);
#35193=ORIENTED_EDGE('',*,*,#27227,.F.);
#35194=ORIENTED_EDGE('',*,*,#27228,.T.);
#35195=ORIENTED_EDGE('',*,*,#27067,.T.);
#35196=ORIENTED_EDGE('',*,*,#25432,.T.);
#35197=ORIENTED_EDGE('',*,*,#25783,.T.);
#35198=ORIENTED_EDGE('',*,*,#27229,.T.);
#35199=ORIENTED_EDGE('',*,*,#27230,.F.);
#35200=ORIENTED_EDGE('',*,*,#27231,.F.);
#35201=ORIENTED_EDGE('',*,*,#27232,.T.);
#35202=ORIENTED_EDGE('',*,*,#27065,.T.);
#35203=ORIENTED_EDGE('',*,*,#25436,.T.);
#35204=ORIENTED_EDGE('',*,*,#25747,.T.);
#35205=ORIENTED_EDGE('',*,*,#27233,.T.);
#35206=ORIENTED_EDGE('',*,*,#27234,.F.);
#35207=ORIENTED_EDGE('',*,*,#27235,.F.);
#35208=ORIENTED_EDGE('',*,*,#27236,.T.);
#35209=ORIENTED_EDGE('',*,*,#27063,.T.);
#35210=ORIENTED_EDGE('',*,*,#25440,.T.);
#35211=ORIENTED_EDGE('',*,*,#25711,.T.);
#35212=ORIENTED_EDGE('',*,*,#27237,.T.);
#35213=ORIENTED_EDGE('',*,*,#27238,.F.);
#35214=ORIENTED_EDGE('',*,*,#27239,.F.);
#35215=ORIENTED_EDGE('',*,*,#27240,.T.);
#35216=ORIENTED_EDGE('',*,*,#27061,.T.);
#35217=ORIENTED_EDGE('',*,*,#25444,.T.);
#35218=ORIENTED_EDGE('',*,*,#25675,.T.);
#35219=ORIENTED_EDGE('',*,*,#27241,.T.);
#35220=ORIENTED_EDGE('',*,*,#27242,.F.);
#35221=ORIENTED_EDGE('',*,*,#27243,.F.);
#35222=ORIENTED_EDGE('',*,*,#27244,.T.);
#35223=ORIENTED_EDGE('',*,*,#27059,.T.);
#35224=ORIENTED_EDGE('',*,*,#25448,.T.);
#35225=ORIENTED_EDGE('',*,*,#25639,.T.);
#35226=ORIENTED_EDGE('',*,*,#27245,.T.);
#35227=ORIENTED_EDGE('',*,*,#27246,.F.);
#35228=ORIENTED_EDGE('',*,*,#27247,.F.);
#35229=ORIENTED_EDGE('',*,*,#27248,.T.);
#35230=ORIENTED_EDGE('',*,*,#27057,.T.);
#35231=ORIENTED_EDGE('',*,*,#25452,.T.);
#35232=ORIENTED_EDGE('',*,*,#25603,.T.);
#35233=ORIENTED_EDGE('',*,*,#27249,.T.);
#35234=ORIENTED_EDGE('',*,*,#27250,.F.);
#35235=ORIENTED_EDGE('',*,*,#27251,.F.);
#35236=ORIENTED_EDGE('',*,*,#27252,.T.);
#35237=ORIENTED_EDGE('',*,*,#27055,.T.);
#35238=ORIENTED_EDGE('',*,*,#25456,.T.);
#35239=ORIENTED_EDGE('',*,*,#25567,.T.);
#35240=ORIENTED_EDGE('',*,*,#27253,.T.);
#35241=ORIENTED_EDGE('',*,*,#27254,.F.);
#35242=ORIENTED_EDGE('',*,*,#27255,.F.);
#35243=ORIENTED_EDGE('',*,*,#27256,.T.);
#35244=ORIENTED_EDGE('',*,*,#27053,.T.);
#35245=ORIENTED_EDGE('',*,*,#25460,.T.);
#35246=ORIENTED_EDGE('',*,*,#25531,.T.);
#35247=ORIENTED_EDGE('',*,*,#27257,.T.);
#35248=ORIENTED_EDGE('',*,*,#27258,.F.);
#35249=ORIENTED_EDGE('',*,*,#27259,.F.);
#35250=ORIENTED_EDGE('',*,*,#27260,.T.);
#35251=ORIENTED_EDGE('',*,*,#27051,.T.);
#35252=ORIENTED_EDGE('',*,*,#27050,.T.);
#35253=ORIENTED_EDGE('',*,*,#27261,.F.);
#35254=ORIENTED_EDGE('',*,*,#27262,.F.);
#35255=ORIENTED_EDGE('',*,*,#25497,.F.);
#35256=ORIENTED_EDGE('',*,*,#26866,.T.);
#35257=ORIENTED_EDGE('',*,*,#27263,.F.);
#35258=ORIENTED_EDGE('',*,*,#27264,.F.);
#35259=ORIENTED_EDGE('',*,*,#26869,.F.);
#35260=ORIENTED_EDGE('',*,*,#26863,.T.);
#35261=ORIENTED_EDGE('',*,*,#27265,.F.);
#35262=ORIENTED_EDGE('',*,*,#27266,.F.);
#35263=ORIENTED_EDGE('',*,*,#26874,.F.);
#35264=ORIENTED_EDGE('',*,*,#26860,.T.);
#35265=ORIENTED_EDGE('',*,*,#27267,.F.);
#35266=ORIENTED_EDGE('',*,*,#27268,.F.);
#35267=ORIENTED_EDGE('',*,*,#26879,.F.);
#35268=ORIENTED_EDGE('',*,*,#26857,.T.);
#35269=ORIENTED_EDGE('',*,*,#27269,.F.);
#35270=ORIENTED_EDGE('',*,*,#27270,.F.);
#35271=ORIENTED_EDGE('',*,*,#26884,.F.);
#35272=ORIENTED_EDGE('',*,*,#26854,.T.);
#35273=ORIENTED_EDGE('',*,*,#27271,.F.);
#35274=ORIENTED_EDGE('',*,*,#27272,.F.);
#35275=ORIENTED_EDGE('',*,*,#26889,.F.);
#35276=ORIENTED_EDGE('',*,*,#26851,.T.);
#35277=ORIENTED_EDGE('',*,*,#27273,.F.);
#35278=ORIENTED_EDGE('',*,*,#27274,.F.);
#35279=ORIENTED_EDGE('',*,*,#26894,.F.);
#35280=ORIENTED_EDGE('',*,*,#26848,.T.);
#35281=ORIENTED_EDGE('',*,*,#27275,.F.);
#35282=ORIENTED_EDGE('',*,*,#27276,.F.);
#35283=ORIENTED_EDGE('',*,*,#26899,.F.);
#35284=ORIENTED_EDGE('',*,*,#26845,.T.);
#35285=ORIENTED_EDGE('',*,*,#27277,.F.);
#35286=ORIENTED_EDGE('',*,*,#27278,.F.);
#35287=ORIENTED_EDGE('',*,*,#26904,.F.);
#35288=ORIENTED_EDGE('',*,*,#26842,.T.);
#35289=ORIENTED_EDGE('',*,*,#27279,.F.);
#35290=ORIENTED_EDGE('',*,*,#27280,.F.);
#35291=ORIENTED_EDGE('',*,*,#26909,.F.);
#35292=ORIENTED_EDGE('',*,*,#26839,.T.);
#35293=ORIENTED_EDGE('',*,*,#27281,.F.);
#35294=ORIENTED_EDGE('',*,*,#27282,.F.);
#35295=ORIENTED_EDGE('',*,*,#26914,.F.);
#35296=ORIENTED_EDGE('',*,*,#26836,.T.);
#35297=ORIENTED_EDGE('',*,*,#27283,.F.);
#35298=ORIENTED_EDGE('',*,*,#27284,.F.);
#35299=ORIENTED_EDGE('',*,*,#26919,.F.);
#35300=ORIENTED_EDGE('',*,*,#26833,.T.);
#35301=ORIENTED_EDGE('',*,*,#27285,.F.);
#35302=ORIENTED_EDGE('',*,*,#27286,.F.);
#35303=ORIENTED_EDGE('',*,*,#26924,.F.);
#35304=ORIENTED_EDGE('',*,*,#26830,.T.);
#35305=ORIENTED_EDGE('',*,*,#27287,.F.);
#35306=ORIENTED_EDGE('',*,*,#27288,.F.);
#35307=ORIENTED_EDGE('',*,*,#26929,.F.);
#35308=ORIENTED_EDGE('',*,*,#26827,.T.);
#35309=ORIENTED_EDGE('',*,*,#27289,.F.);
#35310=ORIENTED_EDGE('',*,*,#27290,.F.);
#35311=ORIENTED_EDGE('',*,*,#26934,.F.);
#35312=ORIENTED_EDGE('',*,*,#26824,.T.);
#35313=ORIENTED_EDGE('',*,*,#27291,.F.);
#35314=ORIENTED_EDGE('',*,*,#27292,.F.);
#35315=ORIENTED_EDGE('',*,*,#26939,.F.);
#35316=ORIENTED_EDGE('',*,*,#26821,.T.);
#35317=ORIENTED_EDGE('',*,*,#27293,.F.);
#35318=ORIENTED_EDGE('',*,*,#27294,.F.);
#35319=ORIENTED_EDGE('',*,*,#26944,.F.);
#35320=ORIENTED_EDGE('',*,*,#26818,.T.);
#35321=ORIENTED_EDGE('',*,*,#27295,.F.);
#35322=ORIENTED_EDGE('',*,*,#27296,.F.);
#35323=ORIENTED_EDGE('',*,*,#26949,.F.);
#35324=ORIENTED_EDGE('',*,*,#26815,.T.);
#35325=ORIENTED_EDGE('',*,*,#27297,.F.);
#35326=ORIENTED_EDGE('',*,*,#27298,.F.);
#35327=ORIENTED_EDGE('',*,*,#26954,.F.);
#35328=ORIENTED_EDGE('',*,*,#26812,.T.);
#35329=ORIENTED_EDGE('',*,*,#27299,.F.);
#35330=ORIENTED_EDGE('',*,*,#27300,.F.);
#35331=ORIENTED_EDGE('',*,*,#26959,.F.);
#35332=ORIENTED_EDGE('',*,*,#26809,.T.);
#35333=ORIENTED_EDGE('',*,*,#27301,.F.);
#35334=ORIENTED_EDGE('',*,*,#27302,.F.);
#35335=ORIENTED_EDGE('',*,*,#26964,.F.);
#35336=ORIENTED_EDGE('',*,*,#26806,.T.);
#35337=ORIENTED_EDGE('',*,*,#27303,.F.);
#35338=ORIENTED_EDGE('',*,*,#27304,.F.);
#35339=ORIENTED_EDGE('',*,*,#26969,.F.);
#35340=ORIENTED_EDGE('',*,*,#26803,.T.);
#35341=ORIENTED_EDGE('',*,*,#27305,.F.);
#35342=ORIENTED_EDGE('',*,*,#27306,.F.);
#35343=ORIENTED_EDGE('',*,*,#26974,.F.);
#35344=ORIENTED_EDGE('',*,*,#26800,.T.);
#35345=ORIENTED_EDGE('',*,*,#27307,.F.);
#35346=ORIENTED_EDGE('',*,*,#27308,.F.);
#35347=ORIENTED_EDGE('',*,*,#26979,.F.);
#35348=ORIENTED_EDGE('',*,*,#26797,.T.);
#35349=ORIENTED_EDGE('',*,*,#27309,.F.);
#35350=ORIENTED_EDGE('',*,*,#27310,.F.);
#35351=ORIENTED_EDGE('',*,*,#26984,.F.);
#35352=ORIENTED_EDGE('',*,*,#26794,.T.);
#35353=ORIENTED_EDGE('',*,*,#27311,.F.);
#35354=ORIENTED_EDGE('',*,*,#27312,.F.);
#35355=ORIENTED_EDGE('',*,*,#26989,.F.);
#35356=ORIENTED_EDGE('',*,*,#26791,.T.);
#35357=ORIENTED_EDGE('',*,*,#27313,.F.);
#35358=ORIENTED_EDGE('',*,*,#27314,.F.);
#35359=ORIENTED_EDGE('',*,*,#26994,.F.);
#35360=ORIENTED_EDGE('',*,*,#26788,.T.);
#35361=ORIENTED_EDGE('',*,*,#27315,.F.);
#35362=ORIENTED_EDGE('',*,*,#27316,.F.);
#35363=ORIENTED_EDGE('',*,*,#26999,.F.);
#35364=ORIENTED_EDGE('',*,*,#26785,.T.);
#35365=ORIENTED_EDGE('',*,*,#27317,.F.);
#35366=ORIENTED_EDGE('',*,*,#27318,.F.);
#35367=ORIENTED_EDGE('',*,*,#27004,.F.);
#35368=ORIENTED_EDGE('',*,*,#26782,.T.);
#35369=ORIENTED_EDGE('',*,*,#27319,.F.);
#35370=ORIENTED_EDGE('',*,*,#27320,.F.);
#35371=ORIENTED_EDGE('',*,*,#27009,.F.);
#35372=ORIENTED_EDGE('',*,*,#26779,.T.);
#35373=ORIENTED_EDGE('',*,*,#27321,.F.);
#35374=ORIENTED_EDGE('',*,*,#27322,.F.);
#35375=ORIENTED_EDGE('',*,*,#27014,.F.);
#35376=ORIENTED_EDGE('',*,*,#26776,.T.);
#35377=ORIENTED_EDGE('',*,*,#27323,.F.);
#35378=ORIENTED_EDGE('',*,*,#27324,.F.);
#35379=ORIENTED_EDGE('',*,*,#27019,.F.);
#35380=ORIENTED_EDGE('',*,*,#26773,.T.);
#35381=ORIENTED_EDGE('',*,*,#27325,.F.);
#35382=ORIENTED_EDGE('',*,*,#27326,.F.);
#35383=ORIENTED_EDGE('',*,*,#27024,.F.);
#35384=ORIENTED_EDGE('',*,*,#26770,.T.);
#35385=ORIENTED_EDGE('',*,*,#27327,.F.);
#35386=ORIENTED_EDGE('',*,*,#27328,.F.);
#35387=ORIENTED_EDGE('',*,*,#27029,.F.);
#35388=ORIENTED_EDGE('',*,*,#26767,.T.);
#35389=ORIENTED_EDGE('',*,*,#27329,.F.);
#35390=ORIENTED_EDGE('',*,*,#27330,.F.);
#35391=ORIENTED_EDGE('',*,*,#27034,.F.);
#35392=ORIENTED_EDGE('',*,*,#26764,.T.);
#35393=ORIENTED_EDGE('',*,*,#27331,.F.);
#35394=ORIENTED_EDGE('',*,*,#27332,.F.);
#35395=ORIENTED_EDGE('',*,*,#27039,.F.);
#35396=ORIENTED_EDGE('',*,*,#26761,.T.);
#35397=ORIENTED_EDGE('',*,*,#27333,.F.);
#35398=ORIENTED_EDGE('',*,*,#27334,.F.);
#35399=ORIENTED_EDGE('',*,*,#27044,.F.);
#35400=ORIENTED_EDGE('',*,*,#27334,.T.);
#35401=ORIENTED_EDGE('',*,*,#27335,.F.);
#35402=ORIENTED_EDGE('',*,*,#27336,.F.);
#35403=ORIENTED_EDGE('',*,*,#27045,.F.);
#35404=ORIENTED_EDGE('',*,*,#27332,.T.);
#35405=ORIENTED_EDGE('',*,*,#27337,.F.);
#35406=ORIENTED_EDGE('',*,*,#27338,.F.);
#35407=ORIENTED_EDGE('',*,*,#27040,.F.);
#35408=ORIENTED_EDGE('',*,*,#27330,.T.);
#35409=ORIENTED_EDGE('',*,*,#27339,.F.);
#35410=ORIENTED_EDGE('',*,*,#27340,.F.);
#35411=ORIENTED_EDGE('',*,*,#27035,.F.);
#35412=ORIENTED_EDGE('',*,*,#27328,.T.);
#35413=ORIENTED_EDGE('',*,*,#27341,.F.);
#35414=ORIENTED_EDGE('',*,*,#27342,.F.);
#35415=ORIENTED_EDGE('',*,*,#27030,.F.);
#35416=ORIENTED_EDGE('',*,*,#27326,.T.);
#35417=ORIENTED_EDGE('',*,*,#27343,.F.);
#35418=ORIENTED_EDGE('',*,*,#27344,.F.);
#35419=ORIENTED_EDGE('',*,*,#27025,.F.);
#35420=ORIENTED_EDGE('',*,*,#27324,.T.);
#35421=ORIENTED_EDGE('',*,*,#27345,.F.);
#35422=ORIENTED_EDGE('',*,*,#27346,.F.);
#35423=ORIENTED_EDGE('',*,*,#27020,.F.);
#35424=ORIENTED_EDGE('',*,*,#27322,.T.);
#35425=ORIENTED_EDGE('',*,*,#27347,.F.);
#35426=ORIENTED_EDGE('',*,*,#27348,.F.);
#35427=ORIENTED_EDGE('',*,*,#27015,.F.);
#35428=ORIENTED_EDGE('',*,*,#27320,.T.);
#35429=ORIENTED_EDGE('',*,*,#27349,.F.);
#35430=ORIENTED_EDGE('',*,*,#27350,.F.);
#35431=ORIENTED_EDGE('',*,*,#27010,.F.);
#35432=ORIENTED_EDGE('',*,*,#27318,.T.);
#35433=ORIENTED_EDGE('',*,*,#27351,.F.);
#35434=ORIENTED_EDGE('',*,*,#27352,.F.);
#35435=ORIENTED_EDGE('',*,*,#27005,.F.);
#35436=ORIENTED_EDGE('',*,*,#27316,.T.);
#35437=ORIENTED_EDGE('',*,*,#27353,.F.);
#35438=ORIENTED_EDGE('',*,*,#27354,.F.);
#35439=ORIENTED_EDGE('',*,*,#27000,.F.);
#35440=ORIENTED_EDGE('',*,*,#27314,.T.);
#35441=ORIENTED_EDGE('',*,*,#27355,.F.);
#35442=ORIENTED_EDGE('',*,*,#27356,.F.);
#35443=ORIENTED_EDGE('',*,*,#26995,.F.);
#35444=ORIENTED_EDGE('',*,*,#27312,.T.);
#35445=ORIENTED_EDGE('',*,*,#27357,.F.);
#35446=ORIENTED_EDGE('',*,*,#27358,.F.);
#35447=ORIENTED_EDGE('',*,*,#26990,.F.);
#35448=ORIENTED_EDGE('',*,*,#27310,.T.);
#35449=ORIENTED_EDGE('',*,*,#27359,.F.);
#35450=ORIENTED_EDGE('',*,*,#27360,.F.);
#35451=ORIENTED_EDGE('',*,*,#26985,.F.);
#35452=ORIENTED_EDGE('',*,*,#27308,.T.);
#35453=ORIENTED_EDGE('',*,*,#27361,.F.);
#35454=ORIENTED_EDGE('',*,*,#27362,.F.);
#35455=ORIENTED_EDGE('',*,*,#26980,.F.);
#35456=ORIENTED_EDGE('',*,*,#27306,.T.);
#35457=ORIENTED_EDGE('',*,*,#27363,.F.);
#35458=ORIENTED_EDGE('',*,*,#27364,.F.);
#35459=ORIENTED_EDGE('',*,*,#26975,.F.);
#35460=ORIENTED_EDGE('',*,*,#27304,.T.);
#35461=ORIENTED_EDGE('',*,*,#27365,.F.);
#35462=ORIENTED_EDGE('',*,*,#27366,.F.);
#35463=ORIENTED_EDGE('',*,*,#26970,.F.);
#35464=ORIENTED_EDGE('',*,*,#27302,.T.);
#35465=ORIENTED_EDGE('',*,*,#27367,.F.);
#35466=ORIENTED_EDGE('',*,*,#27368,.F.);
#35467=ORIENTED_EDGE('',*,*,#26965,.F.);
#35468=ORIENTED_EDGE('',*,*,#27300,.T.);
#35469=ORIENTED_EDGE('',*,*,#27369,.F.);
#35470=ORIENTED_EDGE('',*,*,#27370,.F.);
#35471=ORIENTED_EDGE('',*,*,#27371,.F.);
#35472=ORIENTED_EDGE('',*,*,#26960,.F.);
#35473=ORIENTED_EDGE('',*,*,#27298,.T.);
#35474=ORIENTED_EDGE('',*,*,#27372,.F.);
#35475=ORIENTED_EDGE('',*,*,#27373,.F.);
#35476=ORIENTED_EDGE('',*,*,#26955,.F.);
#35477=ORIENTED_EDGE('',*,*,#27296,.T.);
#35478=ORIENTED_EDGE('',*,*,#27374,.F.);
#35479=ORIENTED_EDGE('',*,*,#27375,.F.);
#35480=ORIENTED_EDGE('',*,*,#26950,.F.);
#35481=ORIENTED_EDGE('',*,*,#27294,.T.);
#35482=ORIENTED_EDGE('',*,*,#27376,.F.);
#35483=ORIENTED_EDGE('',*,*,#27377,.F.);
#35484=ORIENTED_EDGE('',*,*,#26945,.F.);
#35485=ORIENTED_EDGE('',*,*,#27292,.T.);
#35486=ORIENTED_EDGE('',*,*,#27378,.F.);
#35487=ORIENTED_EDGE('',*,*,#27379,.F.);
#35488=ORIENTED_EDGE('',*,*,#26940,.F.);
#35489=ORIENTED_EDGE('',*,*,#27290,.T.);
#35490=ORIENTED_EDGE('',*,*,#27380,.F.);
#35491=ORIENTED_EDGE('',*,*,#27381,.F.);
#35492=ORIENTED_EDGE('',*,*,#26935,.F.);
#35493=ORIENTED_EDGE('',*,*,#27288,.T.);
#35494=ORIENTED_EDGE('',*,*,#27382,.F.);
#35495=ORIENTED_EDGE('',*,*,#27383,.F.);
#35496=ORIENTED_EDGE('',*,*,#26930,.F.);
#35497=ORIENTED_EDGE('',*,*,#27286,.T.);
#35498=ORIENTED_EDGE('',*,*,#27384,.F.);
#35499=ORIENTED_EDGE('',*,*,#27385,.F.);
#35500=ORIENTED_EDGE('',*,*,#26925,.F.);
#35501=ORIENTED_EDGE('',*,*,#27284,.T.);
#35502=ORIENTED_EDGE('',*,*,#27386,.F.);
#35503=ORIENTED_EDGE('',*,*,#27387,.F.);
#35504=ORIENTED_EDGE('',*,*,#26920,.F.);
#35505=ORIENTED_EDGE('',*,*,#27282,.T.);
#35506=ORIENTED_EDGE('',*,*,#27388,.F.);
#35507=ORIENTED_EDGE('',*,*,#27389,.F.);
#35508=ORIENTED_EDGE('',*,*,#26915,.F.);
#35509=ORIENTED_EDGE('',*,*,#27280,.T.);
#35510=ORIENTED_EDGE('',*,*,#27390,.F.);
#35511=ORIENTED_EDGE('',*,*,#27391,.F.);
#35512=ORIENTED_EDGE('',*,*,#26910,.F.);
#35513=ORIENTED_EDGE('',*,*,#27278,.T.);
#35514=ORIENTED_EDGE('',*,*,#27392,.F.);
#35515=ORIENTED_EDGE('',*,*,#27393,.F.);
#35516=ORIENTED_EDGE('',*,*,#26905,.F.);
#35517=ORIENTED_EDGE('',*,*,#27276,.T.);
#35518=ORIENTED_EDGE('',*,*,#27394,.F.);
#35519=ORIENTED_EDGE('',*,*,#27395,.F.);
#35520=ORIENTED_EDGE('',*,*,#26900,.F.);
#35521=ORIENTED_EDGE('',*,*,#27274,.T.);
#35522=ORIENTED_EDGE('',*,*,#27396,.F.);
#35523=ORIENTED_EDGE('',*,*,#27397,.F.);
#35524=ORIENTED_EDGE('',*,*,#26895,.F.);
#35525=ORIENTED_EDGE('',*,*,#27272,.T.);
#35526=ORIENTED_EDGE('',*,*,#27398,.F.);
#35527=ORIENTED_EDGE('',*,*,#27399,.F.);
#35528=ORIENTED_EDGE('',*,*,#26890,.F.);
#35529=ORIENTED_EDGE('',*,*,#27270,.T.);
#35530=ORIENTED_EDGE('',*,*,#27400,.F.);
#35531=ORIENTED_EDGE('',*,*,#27401,.F.);
#35532=ORIENTED_EDGE('',*,*,#26885,.F.);
#35533=ORIENTED_EDGE('',*,*,#27268,.T.);
#35534=ORIENTED_EDGE('',*,*,#27402,.F.);
#35535=ORIENTED_EDGE('',*,*,#27403,.F.);
#35536=ORIENTED_EDGE('',*,*,#26880,.F.);
#35537=ORIENTED_EDGE('',*,*,#27266,.T.);
#35538=ORIENTED_EDGE('',*,*,#27404,.F.);
#35539=ORIENTED_EDGE('',*,*,#27405,.F.);
#35540=ORIENTED_EDGE('',*,*,#26875,.F.);
#35541=ORIENTED_EDGE('',*,*,#27264,.T.);
#35542=ORIENTED_EDGE('',*,*,#27406,.F.);
#35543=ORIENTED_EDGE('',*,*,#27407,.F.);
#35544=ORIENTED_EDGE('',*,*,#26870,.F.);
#35545=ORIENTED_EDGE('',*,*,#27408,.F.);
#35546=ORIENTED_EDGE('',*,*,#27409,.F.);
#35547=ORIENTED_EDGE('',*,*,#26726,.T.);
#35548=ORIENTED_EDGE('',*,*,#26760,.T.);
#35549=ORIENTED_EDGE('',*,*,#27410,.F.);
#35550=ORIENTED_EDGE('',*,*,#27411,.F.);
#35551=ORIENTED_EDGE('',*,*,#26727,.T.);
#35552=ORIENTED_EDGE('',*,*,#27409,.T.);
#35553=ORIENTED_EDGE('',*,*,#27412,.F.);
#35554=ORIENTED_EDGE('',*,*,#27413,.F.);
#35555=ORIENTED_EDGE('',*,*,#26728,.T.);
#35556=ORIENTED_EDGE('',*,*,#27411,.T.);
#35557=ORIENTED_EDGE('',*,*,#27414,.F.);
#35558=ORIENTED_EDGE('',*,*,#27415,.F.);
#35559=ORIENTED_EDGE('',*,*,#26729,.T.);
#35560=ORIENTED_EDGE('',*,*,#27413,.T.);
#35561=ORIENTED_EDGE('',*,*,#27416,.F.);
#35562=ORIENTED_EDGE('',*,*,#27417,.F.);
#35563=ORIENTED_EDGE('',*,*,#26730,.T.);
#35564=ORIENTED_EDGE('',*,*,#27415,.T.);
#35565=ORIENTED_EDGE('',*,*,#27418,.F.);
#35566=ORIENTED_EDGE('',*,*,#27419,.F.);
#35567=ORIENTED_EDGE('',*,*,#26731,.T.);
#35568=ORIENTED_EDGE('',*,*,#27417,.T.);
#35569=ORIENTED_EDGE('',*,*,#27420,.F.);
#35570=ORIENTED_EDGE('',*,*,#27421,.F.);
#35571=ORIENTED_EDGE('',*,*,#26732,.T.);
#35572=ORIENTED_EDGE('',*,*,#27419,.T.);
#35573=ORIENTED_EDGE('',*,*,#27422,.F.);
#35574=ORIENTED_EDGE('',*,*,#27423,.F.);
#35575=ORIENTED_EDGE('',*,*,#26733,.T.);
#35576=ORIENTED_EDGE('',*,*,#27421,.T.);
#35577=ORIENTED_EDGE('',*,*,#27424,.F.);
#35578=ORIENTED_EDGE('',*,*,#27425,.F.);
#35579=ORIENTED_EDGE('',*,*,#26734,.T.);
#35580=ORIENTED_EDGE('',*,*,#27423,.T.);
#35581=ORIENTED_EDGE('',*,*,#27426,.F.);
#35582=ORIENTED_EDGE('',*,*,#27427,.F.);
#35583=ORIENTED_EDGE('',*,*,#26735,.T.);
#35584=ORIENTED_EDGE('',*,*,#27425,.T.);
#35585=ORIENTED_EDGE('',*,*,#27428,.F.);
#35586=ORIENTED_EDGE('',*,*,#27429,.F.);
#35587=ORIENTED_EDGE('',*,*,#26736,.T.);
#35588=ORIENTED_EDGE('',*,*,#27427,.T.);
#35589=ORIENTED_EDGE('',*,*,#27430,.F.);
#35590=ORIENTED_EDGE('',*,*,#27431,.F.);
#35591=ORIENTED_EDGE('',*,*,#26737,.T.);
#35592=ORIENTED_EDGE('',*,*,#27429,.T.);
#35593=ORIENTED_EDGE('',*,*,#27432,.F.);
#35594=ORIENTED_EDGE('',*,*,#27433,.F.);
#35595=ORIENTED_EDGE('',*,*,#26738,.T.);
#35596=ORIENTED_EDGE('',*,*,#27431,.T.);
#35597=ORIENTED_EDGE('',*,*,#26763,.T.);
#35598=ORIENTED_EDGE('',*,*,#26739,.T.);
#35599=ORIENTED_EDGE('',*,*,#27433,.T.);
#35600=ORIENTED_EDGE('',*,*,#27434,.F.);
#35601=ORIENTED_EDGE('',*,*,#27435,.F.);
#35602=ORIENTED_EDGE('',*,*,#27335,.T.);
#35603=ORIENTED_EDGE('',*,*,#27333,.T.);
#35604=ORIENTED_EDGE('',*,*,#27436,.F.);
#35605=ORIENTED_EDGE('',*,*,#27437,.F.);
#35606=ORIENTED_EDGE('',*,*,#26742,.T.);
#35607=ORIENTED_EDGE('',*,*,#27048,.T.);
#35608=ORIENTED_EDGE('',*,*,#27438,.F.);
#35609=ORIENTED_EDGE('',*,*,#27439,.F.);
#35610=ORIENTED_EDGE('',*,*,#26743,.T.);
#35611=ORIENTED_EDGE('',*,*,#27437,.T.);
#35612=ORIENTED_EDGE('',*,*,#27440,.F.);
#35613=ORIENTED_EDGE('',*,*,#27441,.F.);
#35614=ORIENTED_EDGE('',*,*,#26744,.T.);
#35615=ORIENTED_EDGE('',*,*,#27439,.T.);
#35616=ORIENTED_EDGE('',*,*,#27442,.F.);
#35617=ORIENTED_EDGE('',*,*,#27443,.F.);
#35618=ORIENTED_EDGE('',*,*,#26745,.T.);
#35619=ORIENTED_EDGE('',*,*,#27441,.T.);
#35620=ORIENTED_EDGE('',*,*,#27444,.F.);
#35621=ORIENTED_EDGE('',*,*,#27445,.F.);
#35622=ORIENTED_EDGE('',*,*,#26746,.T.);
#35623=ORIENTED_EDGE('',*,*,#27443,.T.);
#35624=ORIENTED_EDGE('',*,*,#27446,.F.);
#35625=ORIENTED_EDGE('',*,*,#27447,.F.);
#35626=ORIENTED_EDGE('',*,*,#26747,.T.);
#35627=ORIENTED_EDGE('',*,*,#27445,.T.);
#35628=ORIENTED_EDGE('',*,*,#27448,.F.);
#35629=ORIENTED_EDGE('',*,*,#27449,.F.);
#35630=ORIENTED_EDGE('',*,*,#26748,.T.);
#35631=ORIENTED_EDGE('',*,*,#27447,.T.);
#35632=ORIENTED_EDGE('',*,*,#27450,.F.);
#35633=ORIENTED_EDGE('',*,*,#27451,.F.);
#35634=ORIENTED_EDGE('',*,*,#26749,.T.);
#35635=ORIENTED_EDGE('',*,*,#27449,.T.);
#35636=ORIENTED_EDGE('',*,*,#27452,.F.);
#35637=ORIENTED_EDGE('',*,*,#27453,.F.);
#35638=ORIENTED_EDGE('',*,*,#26750,.T.);
#35639=ORIENTED_EDGE('',*,*,#27451,.T.);
#35640=ORIENTED_EDGE('',*,*,#27454,.F.);
#35641=ORIENTED_EDGE('',*,*,#27455,.F.);
#35642=ORIENTED_EDGE('',*,*,#26751,.T.);
#35643=ORIENTED_EDGE('',*,*,#27453,.T.);
#35644=ORIENTED_EDGE('',*,*,#27456,.F.);
#35645=ORIENTED_EDGE('',*,*,#27457,.F.);
#35646=ORIENTED_EDGE('',*,*,#26752,.T.);
#35647=ORIENTED_EDGE('',*,*,#27455,.T.);
#35648=ORIENTED_EDGE('',*,*,#27458,.F.);
#35649=ORIENTED_EDGE('',*,*,#27459,.F.);
#35650=ORIENTED_EDGE('',*,*,#26753,.T.);
#35651=ORIENTED_EDGE('',*,*,#27457,.T.);
#35652=ORIENTED_EDGE('',*,*,#27460,.F.);
#35653=ORIENTED_EDGE('',*,*,#27121,.F.);
#35654=ORIENTED_EDGE('',*,*,#26754,.T.);
#35655=ORIENTED_EDGE('',*,*,#27459,.T.);
#35656=ORIENTED_EDGE('',*,*,#27120,.T.);
#35657=ORIENTED_EDGE('',*,*,#27124,.F.);
#35658=ORIENTED_EDGE('',*,*,#27461,.F.);
#35659=ORIENTED_EDGE('',*,*,#26757,.F.);
#35660=ORIENTED_EDGE('',*,*,#27462,.T.);
#35661=ORIENTED_EDGE('',*,*,#27463,.T.);
#35662=ORIENTED_EDGE('',*,*,#27464,.T.);
#35663=ORIENTED_EDGE('',*,*,#27191,.T.);
#35664=ORIENTED_EDGE('',*,*,#27465,.F.);
#35665=ORIENTED_EDGE('',*,*,#26110,.T.);
#35666=ORIENTED_EDGE('',*,*,#27466,.T.);
#35667=ORIENTED_EDGE('',*,*,#27195,.T.);
#35668=ORIENTED_EDGE('',*,*,#27467,.F.);
#35669=ORIENTED_EDGE('',*,*,#26074,.T.);
#35670=ORIENTED_EDGE('',*,*,#27468,.T.);
#35671=ORIENTED_EDGE('',*,*,#27199,.T.);
#35672=ORIENTED_EDGE('',*,*,#27469,.F.);
#35673=ORIENTED_EDGE('',*,*,#26038,.T.);
#35674=ORIENTED_EDGE('',*,*,#27470,.T.);
#35675=ORIENTED_EDGE('',*,*,#27203,.T.);
#35676=ORIENTED_EDGE('',*,*,#27471,.F.);
#35677=ORIENTED_EDGE('',*,*,#26002,.T.);
#35678=ORIENTED_EDGE('',*,*,#27472,.T.);
#35679=ORIENTED_EDGE('',*,*,#27207,.T.);
#35680=ORIENTED_EDGE('',*,*,#27473,.F.);
#35681=ORIENTED_EDGE('',*,*,#25966,.T.);
#35682=ORIENTED_EDGE('',*,*,#27474,.T.);
#35683=ORIENTED_EDGE('',*,*,#27211,.T.);
#35684=ORIENTED_EDGE('',*,*,#27475,.F.);
#35685=ORIENTED_EDGE('',*,*,#25930,.T.);
#35686=ORIENTED_EDGE('',*,*,#27476,.T.);
#35687=ORIENTED_EDGE('',*,*,#27215,.T.);
#35688=ORIENTED_EDGE('',*,*,#27477,.F.);
#35689=ORIENTED_EDGE('',*,*,#25894,.T.);
#35690=ORIENTED_EDGE('',*,*,#27478,.T.);
#35691=ORIENTED_EDGE('',*,*,#27219,.T.);
#35692=ORIENTED_EDGE('',*,*,#27479,.F.);
#35693=ORIENTED_EDGE('',*,*,#25858,.T.);
#35694=ORIENTED_EDGE('',*,*,#27480,.T.);
#35695=ORIENTED_EDGE('',*,*,#27223,.T.);
#35696=ORIENTED_EDGE('',*,*,#27481,.F.);
#35697=ORIENTED_EDGE('',*,*,#25822,.T.);
#35698=ORIENTED_EDGE('',*,*,#27482,.T.);
#35699=ORIENTED_EDGE('',*,*,#27227,.T.);
#35700=ORIENTED_EDGE('',*,*,#27483,.F.);
#35701=ORIENTED_EDGE('',*,*,#25786,.T.);
#35702=ORIENTED_EDGE('',*,*,#27484,.T.);
#35703=ORIENTED_EDGE('',*,*,#27231,.T.);
#35704=ORIENTED_EDGE('',*,*,#27485,.F.);
#35705=ORIENTED_EDGE('',*,*,#25750,.T.);
#35706=ORIENTED_EDGE('',*,*,#27486,.T.);
#35707=ORIENTED_EDGE('',*,*,#27235,.T.);
#35708=ORIENTED_EDGE('',*,*,#27487,.F.);
#35709=ORIENTED_EDGE('',*,*,#25714,.T.);
#35710=ORIENTED_EDGE('',*,*,#27488,.T.);
#35711=ORIENTED_EDGE('',*,*,#27239,.T.);
#35712=ORIENTED_EDGE('',*,*,#27489,.F.);
#35713=ORIENTED_EDGE('',*,*,#25678,.T.);
#35714=ORIENTED_EDGE('',*,*,#27490,.T.);
#35715=ORIENTED_EDGE('',*,*,#27243,.T.);
#35716=ORIENTED_EDGE('',*,*,#27491,.F.);
#35717=ORIENTED_EDGE('',*,*,#25642,.T.);
#35718=ORIENTED_EDGE('',*,*,#27492,.T.);
#35719=ORIENTED_EDGE('',*,*,#27247,.T.);
#35720=ORIENTED_EDGE('',*,*,#27493,.F.);
#35721=ORIENTED_EDGE('',*,*,#25606,.T.);
#35722=ORIENTED_EDGE('',*,*,#27494,.T.);
#35723=ORIENTED_EDGE('',*,*,#27251,.T.);
#35724=ORIENTED_EDGE('',*,*,#27495,.F.);
#35725=ORIENTED_EDGE('',*,*,#25570,.T.);
#35726=ORIENTED_EDGE('',*,*,#27496,.T.);
#35727=ORIENTED_EDGE('',*,*,#27255,.T.);
#35728=ORIENTED_EDGE('',*,*,#27497,.F.);
#35729=ORIENTED_EDGE('',*,*,#25534,.T.);
#35730=ORIENTED_EDGE('',*,*,#27498,.T.);
#35731=ORIENTED_EDGE('',*,*,#27259,.T.);
#35732=ORIENTED_EDGE('',*,*,#27499,.F.);
#35733=ORIENTED_EDGE('',*,*,#25498,.T.);
#35734=ORIENTED_EDGE('',*,*,#27262,.T.);
#35735=ORIENTED_EDGE('',*,*,#27500,.T.);
#35736=ORIENTED_EDGE('',*,*,#27501,.F.);
#35737=ORIENTED_EDGE('',*,*,#26758,.T.);
#35738=ORIENTED_EDGE('',*,*,#27461,.T.);
#35739=ORIENTED_EDGE('',*,*,#27123,.T.);
#35740=ORIENTED_EDGE('',*,*,#27502,.F.);
#35741=ORIENTED_EDGE('',*,*,#26722,.T.);
#35742=ORIENTED_EDGE('',*,*,#27503,.T.);
#35743=ORIENTED_EDGE('',*,*,#27127,.T.);
#35744=ORIENTED_EDGE('',*,*,#27504,.F.);
#35745=ORIENTED_EDGE('',*,*,#26686,.T.);
#35746=ORIENTED_EDGE('',*,*,#27505,.T.);
#35747=ORIENTED_EDGE('',*,*,#27131,.T.);
#35748=ORIENTED_EDGE('',*,*,#27506,.F.);
#35749=ORIENTED_EDGE('',*,*,#26650,.T.);
#35750=ORIENTED_EDGE('',*,*,#27507,.T.);
#35751=ORIENTED_EDGE('',*,*,#27135,.T.);
#35752=ORIENTED_EDGE('',*,*,#27508,.F.);
#35753=ORIENTED_EDGE('',*,*,#26614,.T.);
#35754=ORIENTED_EDGE('',*,*,#27509,.T.);
#35755=ORIENTED_EDGE('',*,*,#27139,.T.);
#35756=ORIENTED_EDGE('',*,*,#27510,.F.);
#35757=ORIENTED_EDGE('',*,*,#26578,.T.);
#35758=ORIENTED_EDGE('',*,*,#27511,.T.);
#35759=ORIENTED_EDGE('',*,*,#27143,.T.);
#35760=ORIENTED_EDGE('',*,*,#27512,.F.);
#35761=ORIENTED_EDGE('',*,*,#26542,.T.);
#35762=ORIENTED_EDGE('',*,*,#27513,.T.);
#35763=ORIENTED_EDGE('',*,*,#27147,.T.);
#35764=ORIENTED_EDGE('',*,*,#27514,.F.);
#35765=ORIENTED_EDGE('',*,*,#26506,.T.);
#35766=ORIENTED_EDGE('',*,*,#27515,.T.);
#35767=ORIENTED_EDGE('',*,*,#27151,.T.);
#35768=ORIENTED_EDGE('',*,*,#27516,.F.);
#35769=ORIENTED_EDGE('',*,*,#26470,.T.);
#35770=ORIENTED_EDGE('',*,*,#27517,.T.);
#35771=ORIENTED_EDGE('',*,*,#27155,.T.);
#35772=ORIENTED_EDGE('',*,*,#27518,.F.);
#35773=ORIENTED_EDGE('',*,*,#26434,.T.);
#35774=ORIENTED_EDGE('',*,*,#27519,.T.);
#35775=ORIENTED_EDGE('',*,*,#27159,.T.);
#35776=ORIENTED_EDGE('',*,*,#27520,.F.);
#35777=ORIENTED_EDGE('',*,*,#26398,.T.);
#35778=ORIENTED_EDGE('',*,*,#27521,.T.);
#35779=ORIENTED_EDGE('',*,*,#27163,.T.);
#35780=ORIENTED_EDGE('',*,*,#27522,.F.);
#35781=ORIENTED_EDGE('',*,*,#26362,.T.);
#35782=ORIENTED_EDGE('',*,*,#27523,.T.);
#35783=ORIENTED_EDGE('',*,*,#27167,.T.);
#35784=ORIENTED_EDGE('',*,*,#27524,.F.);
#35785=ORIENTED_EDGE('',*,*,#26326,.T.);
#35786=ORIENTED_EDGE('',*,*,#27525,.T.);
#35787=ORIENTED_EDGE('',*,*,#27171,.T.);
#35788=ORIENTED_EDGE('',*,*,#27526,.F.);
#35789=ORIENTED_EDGE('',*,*,#26290,.T.);
#35790=ORIENTED_EDGE('',*,*,#27527,.T.);
#35791=ORIENTED_EDGE('',*,*,#27175,.T.);
#35792=ORIENTED_EDGE('',*,*,#27528,.F.);
#35793=ORIENTED_EDGE('',*,*,#26254,.T.);
#35794=ORIENTED_EDGE('',*,*,#27529,.T.);
#35795=ORIENTED_EDGE('',*,*,#27179,.T.);
#35796=ORIENTED_EDGE('',*,*,#27530,.F.);
#35797=ORIENTED_EDGE('',*,*,#26218,.T.);
#35798=ORIENTED_EDGE('',*,*,#27531,.T.);
#35799=ORIENTED_EDGE('',*,*,#27183,.T.);
#35800=ORIENTED_EDGE('',*,*,#27532,.F.);
#35801=ORIENTED_EDGE('',*,*,#26182,.T.);
#35802=ORIENTED_EDGE('',*,*,#27533,.T.);
#35803=ORIENTED_EDGE('',*,*,#27187,.T.);
#35804=ORIENTED_EDGE('',*,*,#27534,.F.);
#35805=ORIENTED_EDGE('',*,*,#26146,.T.);
#35806=ORIENTED_EDGE('',*,*,#27535,.T.);
#35807=ORIENTED_EDGE('',*,*,#27463,.F.);
#35808=ORIENTED_EDGE('',*,*,#27122,.T.);
#35809=ORIENTED_EDGE('',*,*,#27460,.T.);
#35810=ORIENTED_EDGE('',*,*,#27458,.T.);
#35811=ORIENTED_EDGE('',*,*,#27456,.T.);
#35812=ORIENTED_EDGE('',*,*,#27454,.T.);
#35813=ORIENTED_EDGE('',*,*,#27452,.T.);
#35814=ORIENTED_EDGE('',*,*,#27450,.T.);
#35815=ORIENTED_EDGE('',*,*,#27448,.T.);
#35816=ORIENTED_EDGE('',*,*,#27446,.T.);
#35817=ORIENTED_EDGE('',*,*,#27444,.T.);
#35818=ORIENTED_EDGE('',*,*,#27442,.T.);
#35819=ORIENTED_EDGE('',*,*,#27440,.T.);
#35820=ORIENTED_EDGE('',*,*,#27438,.T.);
#35821=ORIENTED_EDGE('',*,*,#27436,.T.);
#35822=ORIENTED_EDGE('',*,*,#27047,.T.);
#35823=ORIENTED_EDGE('',*,*,#27536,.F.);
#35824=ORIENTED_EDGE('',*,*,#27537,.T.);
#35825=ORIENTED_EDGE('',*,*,#27538,.T.);
#35826=ORIENTED_EDGE('',*,*,#27539,.T.);
#35827=ORIENTED_EDGE('',*,*,#27540,.T.);
#35828=ORIENTED_EDGE('',*,*,#27541,.T.);
#35829=ORIENTED_EDGE('',*,*,#27542,.T.);
#35830=ORIENTED_EDGE('',*,*,#27543,.T.);
#35831=ORIENTED_EDGE('',*,*,#27544,.T.);
#35832=ORIENTED_EDGE('',*,*,#27545,.T.);
#35833=ORIENTED_EDGE('',*,*,#27546,.T.);
#35834=ORIENTED_EDGE('',*,*,#27547,.T.);
#35835=ORIENTED_EDGE('',*,*,#27548,.T.);
#35836=ORIENTED_EDGE('',*,*,#27549,.T.);
#35837=ORIENTED_EDGE('',*,*,#27550,.T.);
#35838=ORIENTED_EDGE('',*,*,#26723,.T.);
#35839=ORIENTED_EDGE('',*,*,#27502,.T.);
#35840=ORIENTED_EDGE('',*,*,#27550,.F.);
#35841=ORIENTED_EDGE('',*,*,#27551,.F.);
#35842=ORIENTED_EDGE('',*,*,#26690,.T.);
#35843=ORIENTED_EDGE('',*,*,#26724,.T.);
#35844=ORIENTED_EDGE('',*,*,#27549,.F.);
#35845=ORIENTED_EDGE('',*,*,#27552,.F.);
#35846=ORIENTED_EDGE('',*,*,#26691,.T.);
#35847=ORIENTED_EDGE('',*,*,#27551,.T.);
#35848=ORIENTED_EDGE('',*,*,#27548,.F.);
#35849=ORIENTED_EDGE('',*,*,#27553,.F.);
#35850=ORIENTED_EDGE('',*,*,#26692,.T.);
#35851=ORIENTED_EDGE('',*,*,#27552,.T.);
#35852=ORIENTED_EDGE('',*,*,#27547,.F.);
#35853=ORIENTED_EDGE('',*,*,#27554,.F.);
#35854=ORIENTED_EDGE('',*,*,#26693,.T.);
#35855=ORIENTED_EDGE('',*,*,#27553,.T.);
#35856=ORIENTED_EDGE('',*,*,#27546,.F.);
#35857=ORIENTED_EDGE('',*,*,#27555,.F.);
#35858=ORIENTED_EDGE('',*,*,#26694,.T.);
#35859=ORIENTED_EDGE('',*,*,#27554,.T.);
#35860=ORIENTED_EDGE('',*,*,#27545,.F.);
#35861=ORIENTED_EDGE('',*,*,#27556,.F.);
#35862=ORIENTED_EDGE('',*,*,#26695,.T.);
#35863=ORIENTED_EDGE('',*,*,#27555,.T.);
#35864=ORIENTED_EDGE('',*,*,#27544,.F.);
#35865=ORIENTED_EDGE('',*,*,#27557,.F.);
#35866=ORIENTED_EDGE('',*,*,#26696,.T.);
#35867=ORIENTED_EDGE('',*,*,#27556,.T.);
#35868=ORIENTED_EDGE('',*,*,#27543,.F.);
#35869=ORIENTED_EDGE('',*,*,#27558,.F.);
#35870=ORIENTED_EDGE('',*,*,#26697,.T.);
#35871=ORIENTED_EDGE('',*,*,#27557,.T.);
#35872=ORIENTED_EDGE('',*,*,#27542,.F.);
#35873=ORIENTED_EDGE('',*,*,#27559,.F.);
#35874=ORIENTED_EDGE('',*,*,#26698,.T.);
#35875=ORIENTED_EDGE('',*,*,#27558,.T.);
#35876=ORIENTED_EDGE('',*,*,#27541,.F.);
#35877=ORIENTED_EDGE('',*,*,#27560,.F.);
#35878=ORIENTED_EDGE('',*,*,#26699,.T.);
#35879=ORIENTED_EDGE('',*,*,#27559,.T.);
#35880=ORIENTED_EDGE('',*,*,#27540,.F.);
#35881=ORIENTED_EDGE('',*,*,#27561,.F.);
#35882=ORIENTED_EDGE('',*,*,#26700,.T.);
#35883=ORIENTED_EDGE('',*,*,#27560,.T.);
#35884=ORIENTED_EDGE('',*,*,#27539,.F.);
#35885=ORIENTED_EDGE('',*,*,#27562,.F.);
#35886=ORIENTED_EDGE('',*,*,#26701,.T.);
#35887=ORIENTED_EDGE('',*,*,#27561,.T.);
#35888=ORIENTED_EDGE('',*,*,#27538,.F.);
#35889=ORIENTED_EDGE('',*,*,#27563,.F.);
#35890=ORIENTED_EDGE('',*,*,#26702,.T.);
#35891=ORIENTED_EDGE('',*,*,#27562,.T.);
#35892=ORIENTED_EDGE('',*,*,#26766,.T.);
#35893=ORIENTED_EDGE('',*,*,#26703,.T.);
#35894=ORIENTED_EDGE('',*,*,#27563,.T.);
#35895=ORIENTED_EDGE('',*,*,#27537,.F.);
#35896=ORIENTED_EDGE('',*,*,#27564,.F.);
#35897=ORIENTED_EDGE('',*,*,#27337,.T.);
#35898=ORIENTED_EDGE('',*,*,#27331,.T.);
#35899=ORIENTED_EDGE('',*,*,#27565,.F.);
#35900=ORIENTED_EDGE('',*,*,#27566,.F.);
#35901=ORIENTED_EDGE('',*,*,#26706,.T.);
#35902=ORIENTED_EDGE('',*,*,#27043,.T.);
#35903=ORIENTED_EDGE('',*,*,#27567,.F.);
#35904=ORIENTED_EDGE('',*,*,#27568,.F.);
#35905=ORIENTED_EDGE('',*,*,#26707,.T.);
#35906=ORIENTED_EDGE('',*,*,#27566,.T.);
#35907=ORIENTED_EDGE('',*,*,#27569,.F.);
#35908=ORIENTED_EDGE('',*,*,#27570,.F.);
#35909=ORIENTED_EDGE('',*,*,#26708,.T.);
#35910=ORIENTED_EDGE('',*,*,#27568,.T.);
#35911=ORIENTED_EDGE('',*,*,#27571,.F.);
#35912=ORIENTED_EDGE('',*,*,#27572,.F.);
#35913=ORIENTED_EDGE('',*,*,#26709,.T.);
#35914=ORIENTED_EDGE('',*,*,#27570,.T.);
#35915=ORIENTED_EDGE('',*,*,#27573,.F.);
#35916=ORIENTED_EDGE('',*,*,#27574,.F.);
#35917=ORIENTED_EDGE('',*,*,#26710,.T.);
#35918=ORIENTED_EDGE('',*,*,#27572,.T.);
#35919=ORIENTED_EDGE('',*,*,#27575,.F.);
#35920=ORIENTED_EDGE('',*,*,#27576,.F.);
#35921=ORIENTED_EDGE('',*,*,#26711,.T.);
#35922=ORIENTED_EDGE('',*,*,#27574,.T.);
#35923=ORIENTED_EDGE('',*,*,#27577,.F.);
#35924=ORIENTED_EDGE('',*,*,#27578,.F.);
#35925=ORIENTED_EDGE('',*,*,#26712,.T.);
#35926=ORIENTED_EDGE('',*,*,#27576,.T.);
#35927=ORIENTED_EDGE('',*,*,#27579,.F.);
#35928=ORIENTED_EDGE('',*,*,#27580,.F.);
#35929=ORIENTED_EDGE('',*,*,#26713,.T.);
#35930=ORIENTED_EDGE('',*,*,#27578,.T.);
#35931=ORIENTED_EDGE('',*,*,#27581,.F.);
#35932=ORIENTED_EDGE('',*,*,#27582,.F.);
#35933=ORIENTED_EDGE('',*,*,#26714,.T.);
#35934=ORIENTED_EDGE('',*,*,#27580,.T.);
#35935=ORIENTED_EDGE('',*,*,#27583,.F.);
#35936=ORIENTED_EDGE('',*,*,#27584,.F.);
#35937=ORIENTED_EDGE('',*,*,#26715,.T.);
#35938=ORIENTED_EDGE('',*,*,#27582,.T.);
#35939=ORIENTED_EDGE('',*,*,#27585,.F.);
#35940=ORIENTED_EDGE('',*,*,#27586,.F.);
#35941=ORIENTED_EDGE('',*,*,#26716,.T.);
#35942=ORIENTED_EDGE('',*,*,#27584,.T.);
#35943=ORIENTED_EDGE('',*,*,#27587,.F.);
#35944=ORIENTED_EDGE('',*,*,#27588,.F.);
#35945=ORIENTED_EDGE('',*,*,#26717,.T.);
#35946=ORIENTED_EDGE('',*,*,#27586,.T.);
#35947=ORIENTED_EDGE('',*,*,#27589,.F.);
#35948=ORIENTED_EDGE('',*,*,#27125,.F.);
#35949=ORIENTED_EDGE('',*,*,#26718,.T.);
#35950=ORIENTED_EDGE('',*,*,#27588,.T.);
#35951=ORIENTED_EDGE('',*,*,#27118,.T.);
#35952=ORIENTED_EDGE('',*,*,#27128,.F.);
#35953=ORIENTED_EDGE('',*,*,#27503,.F.);
#35954=ORIENTED_EDGE('',*,*,#26721,.F.);
#35955=ORIENTED_EDGE('',*,*,#27126,.T.);
#35956=ORIENTED_EDGE('',*,*,#27589,.T.);
#35957=ORIENTED_EDGE('',*,*,#27587,.T.);
#35958=ORIENTED_EDGE('',*,*,#27585,.T.);
#35959=ORIENTED_EDGE('',*,*,#27583,.T.);
#35960=ORIENTED_EDGE('',*,*,#27581,.T.);
#35961=ORIENTED_EDGE('',*,*,#27579,.T.);
#35962=ORIENTED_EDGE('',*,*,#27577,.T.);
#35963=ORIENTED_EDGE('',*,*,#27575,.T.);
#35964=ORIENTED_EDGE('',*,*,#27573,.T.);
#35965=ORIENTED_EDGE('',*,*,#27571,.T.);
#35966=ORIENTED_EDGE('',*,*,#27569,.T.);
#35967=ORIENTED_EDGE('',*,*,#27567,.T.);
#35968=ORIENTED_EDGE('',*,*,#27565,.T.);
#35969=ORIENTED_EDGE('',*,*,#27042,.T.);
#35970=ORIENTED_EDGE('',*,*,#27590,.F.);
#35971=ORIENTED_EDGE('',*,*,#27591,.T.);
#35972=ORIENTED_EDGE('',*,*,#27592,.T.);
#35973=ORIENTED_EDGE('',*,*,#27593,.T.);
#35974=ORIENTED_EDGE('',*,*,#27594,.T.);
#35975=ORIENTED_EDGE('',*,*,#27595,.T.);
#35976=ORIENTED_EDGE('',*,*,#27596,.T.);
#35977=ORIENTED_EDGE('',*,*,#27597,.T.);
#35978=ORIENTED_EDGE('',*,*,#27598,.T.);
#35979=ORIENTED_EDGE('',*,*,#27599,.T.);
#35980=ORIENTED_EDGE('',*,*,#27600,.T.);
#35981=ORIENTED_EDGE('',*,*,#27601,.T.);
#35982=ORIENTED_EDGE('',*,*,#27602,.T.);
#35983=ORIENTED_EDGE('',*,*,#27603,.T.);
#35984=ORIENTED_EDGE('',*,*,#27604,.T.);
#35985=ORIENTED_EDGE('',*,*,#26687,.T.);
#35986=ORIENTED_EDGE('',*,*,#27504,.T.);
#35987=ORIENTED_EDGE('',*,*,#27604,.F.);
#35988=ORIENTED_EDGE('',*,*,#27605,.F.);
#35989=ORIENTED_EDGE('',*,*,#26654,.T.);
#35990=ORIENTED_EDGE('',*,*,#26688,.T.);
#35991=ORIENTED_EDGE('',*,*,#27603,.F.);
#35992=ORIENTED_EDGE('',*,*,#27606,.F.);
#35993=ORIENTED_EDGE('',*,*,#26655,.T.);
#35994=ORIENTED_EDGE('',*,*,#27605,.T.);
#35995=ORIENTED_EDGE('',*,*,#27602,.F.);
#35996=ORIENTED_EDGE('',*,*,#27607,.F.);
#35997=ORIENTED_EDGE('',*,*,#26656,.T.);
#35998=ORIENTED_EDGE('',*,*,#27606,.T.);
#35999=ORIENTED_EDGE('',*,*,#27601,.F.);
#36000=ORIENTED_EDGE('',*,*,#27608,.F.);
#36001=ORIENTED_EDGE('',*,*,#26657,.T.);
#36002=ORIENTED_EDGE('',*,*,#27607,.T.);
#36003=ORIENTED_EDGE('',*,*,#27600,.F.);
#36004=ORIENTED_EDGE('',*,*,#27609,.F.);
#36005=ORIENTED_EDGE('',*,*,#26658,.T.);
#36006=ORIENTED_EDGE('',*,*,#27608,.T.);
#36007=ORIENTED_EDGE('',*,*,#27599,.F.);
#36008=ORIENTED_EDGE('',*,*,#27610,.F.);
#36009=ORIENTED_EDGE('',*,*,#26659,.T.);
#36010=ORIENTED_EDGE('',*,*,#27609,.T.);
#36011=ORIENTED_EDGE('',*,*,#27598,.F.);
#36012=ORIENTED_EDGE('',*,*,#27611,.F.);
#36013=ORIENTED_EDGE('',*,*,#26660,.T.);
#36014=ORIENTED_EDGE('',*,*,#27610,.T.);
#36015=ORIENTED_EDGE('',*,*,#27597,.F.);
#36016=ORIENTED_EDGE('',*,*,#27612,.F.);
#36017=ORIENTED_EDGE('',*,*,#26661,.T.);
#36018=ORIENTED_EDGE('',*,*,#27611,.T.);
#36019=ORIENTED_EDGE('',*,*,#27596,.F.);
#36020=ORIENTED_EDGE('',*,*,#27613,.F.);
#36021=ORIENTED_EDGE('',*,*,#26662,.T.);
#36022=ORIENTED_EDGE('',*,*,#27612,.T.);
#36023=ORIENTED_EDGE('',*,*,#27595,.F.);
#36024=ORIENTED_EDGE('',*,*,#27614,.F.);
#36025=ORIENTED_EDGE('',*,*,#26663,.T.);
#36026=ORIENTED_EDGE('',*,*,#27613,.T.);
#36027=ORIENTED_EDGE('',*,*,#27594,.F.);
#36028=ORIENTED_EDGE('',*,*,#27615,.F.);
#36029=ORIENTED_EDGE('',*,*,#26664,.T.);
#36030=ORIENTED_EDGE('',*,*,#27614,.T.);
#36031=ORIENTED_EDGE('',*,*,#27593,.F.);
#36032=ORIENTED_EDGE('',*,*,#27616,.F.);
#36033=ORIENTED_EDGE('',*,*,#26665,.T.);
#36034=ORIENTED_EDGE('',*,*,#27615,.T.);
#36035=ORIENTED_EDGE('',*,*,#27592,.F.);
#36036=ORIENTED_EDGE('',*,*,#27617,.F.);
#36037=ORIENTED_EDGE('',*,*,#26666,.T.);
#36038=ORIENTED_EDGE('',*,*,#27616,.T.);
#36039=ORIENTED_EDGE('',*,*,#26769,.T.);
#36040=ORIENTED_EDGE('',*,*,#26667,.T.);
#36041=ORIENTED_EDGE('',*,*,#27617,.T.);
#36042=ORIENTED_EDGE('',*,*,#27591,.F.);
#36043=ORIENTED_EDGE('',*,*,#27618,.F.);
#36044=ORIENTED_EDGE('',*,*,#27339,.T.);
#36045=ORIENTED_EDGE('',*,*,#27329,.T.);
#36046=ORIENTED_EDGE('',*,*,#27619,.F.);
#36047=ORIENTED_EDGE('',*,*,#27620,.F.);
#36048=ORIENTED_EDGE('',*,*,#26670,.T.);
#36049=ORIENTED_EDGE('',*,*,#27038,.T.);
#36050=ORIENTED_EDGE('',*,*,#27621,.F.);
#36051=ORIENTED_EDGE('',*,*,#27622,.F.);
#36052=ORIENTED_EDGE('',*,*,#26671,.T.);
#36053=ORIENTED_EDGE('',*,*,#27620,.T.);
#36054=ORIENTED_EDGE('',*,*,#27623,.F.);
#36055=ORIENTED_EDGE('',*,*,#27624,.F.);
#36056=ORIENTED_EDGE('',*,*,#26672,.T.);
#36057=ORIENTED_EDGE('',*,*,#27622,.T.);
#36058=ORIENTED_EDGE('',*,*,#27625,.F.);
#36059=ORIENTED_EDGE('',*,*,#27626,.F.);
#36060=ORIENTED_EDGE('',*,*,#26673,.T.);
#36061=ORIENTED_EDGE('',*,*,#27624,.T.);
#36062=ORIENTED_EDGE('',*,*,#27627,.F.);
#36063=ORIENTED_EDGE('',*,*,#27628,.F.);
#36064=ORIENTED_EDGE('',*,*,#26674,.T.);
#36065=ORIENTED_EDGE('',*,*,#27626,.T.);
#36066=ORIENTED_EDGE('',*,*,#27629,.F.);
#36067=ORIENTED_EDGE('',*,*,#27630,.F.);
#36068=ORIENTED_EDGE('',*,*,#26675,.T.);
#36069=ORIENTED_EDGE('',*,*,#27628,.T.);
#36070=ORIENTED_EDGE('',*,*,#27631,.F.);
#36071=ORIENTED_EDGE('',*,*,#27632,.F.);
#36072=ORIENTED_EDGE('',*,*,#26676,.T.);
#36073=ORIENTED_EDGE('',*,*,#27630,.T.);
#36074=ORIENTED_EDGE('',*,*,#27633,.F.);
#36075=ORIENTED_EDGE('',*,*,#27634,.F.);
#36076=ORIENTED_EDGE('',*,*,#26677,.T.);
#36077=ORIENTED_EDGE('',*,*,#27632,.T.);
#36078=ORIENTED_EDGE('',*,*,#27635,.F.);
#36079=ORIENTED_EDGE('',*,*,#27636,.F.);
#36080=ORIENTED_EDGE('',*,*,#26678,.T.);
#36081=ORIENTED_EDGE('',*,*,#27634,.T.);
#36082=ORIENTED_EDGE('',*,*,#27637,.F.);
#36083=ORIENTED_EDGE('',*,*,#27638,.F.);
#36084=ORIENTED_EDGE('',*,*,#26679,.T.);
#36085=ORIENTED_EDGE('',*,*,#27636,.T.);
#36086=ORIENTED_EDGE('',*,*,#27639,.F.);
#36087=ORIENTED_EDGE('',*,*,#27640,.F.);
#36088=ORIENTED_EDGE('',*,*,#26680,.T.);
#36089=ORIENTED_EDGE('',*,*,#27638,.T.);
#36090=ORIENTED_EDGE('',*,*,#27641,.F.);
#36091=ORIENTED_EDGE('',*,*,#27642,.F.);
#36092=ORIENTED_EDGE('',*,*,#26681,.T.);
#36093=ORIENTED_EDGE('',*,*,#27640,.T.);
#36094=ORIENTED_EDGE('',*,*,#27643,.F.);
#36095=ORIENTED_EDGE('',*,*,#27129,.F.);
#36096=ORIENTED_EDGE('',*,*,#26682,.T.);
#36097=ORIENTED_EDGE('',*,*,#27642,.T.);
#36098=ORIENTED_EDGE('',*,*,#27116,.T.);
#36099=ORIENTED_EDGE('',*,*,#27132,.F.);
#36100=ORIENTED_EDGE('',*,*,#27505,.F.);
#36101=ORIENTED_EDGE('',*,*,#26685,.F.);
#36102=ORIENTED_EDGE('',*,*,#27130,.T.);
#36103=ORIENTED_EDGE('',*,*,#27643,.T.);
#36104=ORIENTED_EDGE('',*,*,#27641,.T.);
#36105=ORIENTED_EDGE('',*,*,#27639,.T.);
#36106=ORIENTED_EDGE('',*,*,#27637,.T.);
#36107=ORIENTED_EDGE('',*,*,#27635,.T.);
#36108=ORIENTED_EDGE('',*,*,#27633,.T.);
#36109=ORIENTED_EDGE('',*,*,#27631,.T.);
#36110=ORIENTED_EDGE('',*,*,#27629,.T.);
#36111=ORIENTED_EDGE('',*,*,#27627,.T.);
#36112=ORIENTED_EDGE('',*,*,#27625,.T.);
#36113=ORIENTED_EDGE('',*,*,#27623,.T.);
#36114=ORIENTED_EDGE('',*,*,#27621,.T.);
#36115=ORIENTED_EDGE('',*,*,#27619,.T.);
#36116=ORIENTED_EDGE('',*,*,#27037,.T.);
#36117=ORIENTED_EDGE('',*,*,#27644,.F.);
#36118=ORIENTED_EDGE('',*,*,#27645,.T.);
#36119=ORIENTED_EDGE('',*,*,#27646,.T.);
#36120=ORIENTED_EDGE('',*,*,#27647,.T.);
#36121=ORIENTED_EDGE('',*,*,#27648,.T.);
#36122=ORIENTED_EDGE('',*,*,#27649,.T.);
#36123=ORIENTED_EDGE('',*,*,#27650,.T.);
#36124=ORIENTED_EDGE('',*,*,#27651,.T.);
#36125=ORIENTED_EDGE('',*,*,#27652,.T.);
#36126=ORIENTED_EDGE('',*,*,#27653,.T.);
#36127=ORIENTED_EDGE('',*,*,#27654,.T.);
#36128=ORIENTED_EDGE('',*,*,#27655,.T.);
#36129=ORIENTED_EDGE('',*,*,#27656,.T.);
#36130=ORIENTED_EDGE('',*,*,#27657,.T.);
#36131=ORIENTED_EDGE('',*,*,#27658,.T.);
#36132=ORIENTED_EDGE('',*,*,#26651,.T.);
#36133=ORIENTED_EDGE('',*,*,#27506,.T.);
#36134=ORIENTED_EDGE('',*,*,#27658,.F.);
#36135=ORIENTED_EDGE('',*,*,#27659,.F.);
#36136=ORIENTED_EDGE('',*,*,#26618,.T.);
#36137=ORIENTED_EDGE('',*,*,#26652,.T.);
#36138=ORIENTED_EDGE('',*,*,#27657,.F.);
#36139=ORIENTED_EDGE('',*,*,#27660,.F.);
#36140=ORIENTED_EDGE('',*,*,#26619,.T.);
#36141=ORIENTED_EDGE('',*,*,#27659,.T.);
#36142=ORIENTED_EDGE('',*,*,#27656,.F.);
#36143=ORIENTED_EDGE('',*,*,#27661,.F.);
#36144=ORIENTED_EDGE('',*,*,#26620,.T.);
#36145=ORIENTED_EDGE('',*,*,#27660,.T.);
#36146=ORIENTED_EDGE('',*,*,#27655,.F.);
#36147=ORIENTED_EDGE('',*,*,#27662,.F.);
#36148=ORIENTED_EDGE('',*,*,#26621,.T.);
#36149=ORIENTED_EDGE('',*,*,#27661,.T.);
#36150=ORIENTED_EDGE('',*,*,#27654,.F.);
#36151=ORIENTED_EDGE('',*,*,#27663,.F.);
#36152=ORIENTED_EDGE('',*,*,#26622,.T.);
#36153=ORIENTED_EDGE('',*,*,#27662,.T.);
#36154=ORIENTED_EDGE('',*,*,#27653,.F.);
#36155=ORIENTED_EDGE('',*,*,#27664,.F.);
#36156=ORIENTED_EDGE('',*,*,#26623,.T.);
#36157=ORIENTED_EDGE('',*,*,#27663,.T.);
#36158=ORIENTED_EDGE('',*,*,#27652,.F.);
#36159=ORIENTED_EDGE('',*,*,#27665,.F.);
#36160=ORIENTED_EDGE('',*,*,#26624,.T.);
#36161=ORIENTED_EDGE('',*,*,#27664,.T.);
#36162=ORIENTED_EDGE('',*,*,#27651,.F.);
#36163=ORIENTED_EDGE('',*,*,#27666,.F.);
#36164=ORIENTED_EDGE('',*,*,#26625,.T.);
#36165=ORIENTED_EDGE('',*,*,#27665,.T.);
#36166=ORIENTED_EDGE('',*,*,#27650,.F.);
#36167=ORIENTED_EDGE('',*,*,#27667,.F.);
#36168=ORIENTED_EDGE('',*,*,#26626,.T.);
#36169=ORIENTED_EDGE('',*,*,#27666,.T.);
#36170=ORIENTED_EDGE('',*,*,#27649,.F.);
#36171=ORIENTED_EDGE('',*,*,#27668,.F.);
#36172=ORIENTED_EDGE('',*,*,#26627,.T.);
#36173=ORIENTED_EDGE('',*,*,#27667,.T.);
#36174=ORIENTED_EDGE('',*,*,#27648,.F.);
#36175=ORIENTED_EDGE('',*,*,#27669,.F.);
#36176=ORIENTED_EDGE('',*,*,#26628,.T.);
#36177=ORIENTED_EDGE('',*,*,#27668,.T.);
#36178=ORIENTED_EDGE('',*,*,#27647,.F.);
#36179=ORIENTED_EDGE('',*,*,#27670,.F.);
#36180=ORIENTED_EDGE('',*,*,#26629,.T.);
#36181=ORIENTED_EDGE('',*,*,#27669,.T.);
#36182=ORIENTED_EDGE('',*,*,#27646,.F.);
#36183=ORIENTED_EDGE('',*,*,#27671,.F.);
#36184=ORIENTED_EDGE('',*,*,#26630,.T.);
#36185=ORIENTED_EDGE('',*,*,#27670,.T.);
#36186=ORIENTED_EDGE('',*,*,#26772,.T.);
#36187=ORIENTED_EDGE('',*,*,#26631,.T.);
#36188=ORIENTED_EDGE('',*,*,#27671,.T.);
#36189=ORIENTED_EDGE('',*,*,#27645,.F.);
#36190=ORIENTED_EDGE('',*,*,#27672,.F.);
#36191=ORIENTED_EDGE('',*,*,#27341,.T.);
#36192=ORIENTED_EDGE('',*,*,#27327,.T.);
#36193=ORIENTED_EDGE('',*,*,#27673,.F.);
#36194=ORIENTED_EDGE('',*,*,#27674,.F.);
#36195=ORIENTED_EDGE('',*,*,#26634,.T.);
#36196=ORIENTED_EDGE('',*,*,#27033,.T.);
#36197=ORIENTED_EDGE('',*,*,#27675,.F.);
#36198=ORIENTED_EDGE('',*,*,#27676,.F.);
#36199=ORIENTED_EDGE('',*,*,#26635,.T.);
#36200=ORIENTED_EDGE('',*,*,#27674,.T.);
#36201=ORIENTED_EDGE('',*,*,#27677,.F.);
#36202=ORIENTED_EDGE('',*,*,#27678,.F.);
#36203=ORIENTED_EDGE('',*,*,#26636,.T.);
#36204=ORIENTED_EDGE('',*,*,#27676,.T.);
#36205=ORIENTED_EDGE('',*,*,#27679,.F.);
#36206=ORIENTED_EDGE('',*,*,#27680,.F.);
#36207=ORIENTED_EDGE('',*,*,#26637,.T.);
#36208=ORIENTED_EDGE('',*,*,#27678,.T.);
#36209=ORIENTED_EDGE('',*,*,#27681,.F.);
#36210=ORIENTED_EDGE('',*,*,#27682,.F.);
#36211=ORIENTED_EDGE('',*,*,#26638,.T.);
#36212=ORIENTED_EDGE('',*,*,#27680,.T.);
#36213=ORIENTED_EDGE('',*,*,#27683,.F.);
#36214=ORIENTED_EDGE('',*,*,#27684,.F.);
#36215=ORIENTED_EDGE('',*,*,#26639,.T.);
#36216=ORIENTED_EDGE('',*,*,#27682,.T.);
#36217=ORIENTED_EDGE('',*,*,#27685,.F.);
#36218=ORIENTED_EDGE('',*,*,#27686,.F.);
#36219=ORIENTED_EDGE('',*,*,#26640,.T.);
#36220=ORIENTED_EDGE('',*,*,#27684,.T.);
#36221=ORIENTED_EDGE('',*,*,#27687,.F.);
#36222=ORIENTED_EDGE('',*,*,#27688,.F.);
#36223=ORIENTED_EDGE('',*,*,#26641,.T.);
#36224=ORIENTED_EDGE('',*,*,#27686,.T.);
#36225=ORIENTED_EDGE('',*,*,#27689,.F.);
#36226=ORIENTED_EDGE('',*,*,#27690,.F.);
#36227=ORIENTED_EDGE('',*,*,#26642,.T.);
#36228=ORIENTED_EDGE('',*,*,#27688,.T.);
#36229=ORIENTED_EDGE('',*,*,#27691,.F.);
#36230=ORIENTED_EDGE('',*,*,#27692,.F.);
#36231=ORIENTED_EDGE('',*,*,#26643,.T.);
#36232=ORIENTED_EDGE('',*,*,#27690,.T.);
#36233=ORIENTED_EDGE('',*,*,#27693,.F.);
#36234=ORIENTED_EDGE('',*,*,#27694,.F.);
#36235=ORIENTED_EDGE('',*,*,#26644,.T.);
#36236=ORIENTED_EDGE('',*,*,#27692,.T.);
#36237=ORIENTED_EDGE('',*,*,#27695,.F.);
#36238=ORIENTED_EDGE('',*,*,#27696,.F.);
#36239=ORIENTED_EDGE('',*,*,#26645,.T.);
#36240=ORIENTED_EDGE('',*,*,#27694,.T.);
#36241=ORIENTED_EDGE('',*,*,#27697,.F.);
#36242=ORIENTED_EDGE('',*,*,#27133,.F.);
#36243=ORIENTED_EDGE('',*,*,#26646,.T.);
#36244=ORIENTED_EDGE('',*,*,#27696,.T.);
#36245=ORIENTED_EDGE('',*,*,#27114,.T.);
#36246=ORIENTED_EDGE('',*,*,#27136,.F.);
#36247=ORIENTED_EDGE('',*,*,#27507,.F.);
#36248=ORIENTED_EDGE('',*,*,#26649,.F.);
#36249=ORIENTED_EDGE('',*,*,#27134,.T.);
#36250=ORIENTED_EDGE('',*,*,#27697,.T.);
#36251=ORIENTED_EDGE('',*,*,#27695,.T.);
#36252=ORIENTED_EDGE('',*,*,#27693,.T.);
#36253=ORIENTED_EDGE('',*,*,#27691,.T.);
#36254=ORIENTED_EDGE('',*,*,#27689,.T.);
#36255=ORIENTED_EDGE('',*,*,#27687,.T.);
#36256=ORIENTED_EDGE('',*,*,#27685,.T.);
#36257=ORIENTED_EDGE('',*,*,#27683,.T.);
#36258=ORIENTED_EDGE('',*,*,#27681,.T.);
#36259=ORIENTED_EDGE('',*,*,#27679,.T.);
#36260=ORIENTED_EDGE('',*,*,#27677,.T.);
#36261=ORIENTED_EDGE('',*,*,#27675,.T.);
#36262=ORIENTED_EDGE('',*,*,#27673,.T.);
#36263=ORIENTED_EDGE('',*,*,#27032,.T.);
#36264=ORIENTED_EDGE('',*,*,#27698,.F.);
#36265=ORIENTED_EDGE('',*,*,#27699,.T.);
#36266=ORIENTED_EDGE('',*,*,#27700,.T.);
#36267=ORIENTED_EDGE('',*,*,#27701,.T.);
#36268=ORIENTED_EDGE('',*,*,#27702,.T.);
#36269=ORIENTED_EDGE('',*,*,#27703,.T.);
#36270=ORIENTED_EDGE('',*,*,#27704,.T.);
#36271=ORIENTED_EDGE('',*,*,#27705,.T.);
#36272=ORIENTED_EDGE('',*,*,#27706,.T.);
#36273=ORIENTED_EDGE('',*,*,#27707,.T.);
#36274=ORIENTED_EDGE('',*,*,#27708,.T.);
#36275=ORIENTED_EDGE('',*,*,#27709,.T.);
#36276=ORIENTED_EDGE('',*,*,#27710,.T.);
#36277=ORIENTED_EDGE('',*,*,#27711,.T.);
#36278=ORIENTED_EDGE('',*,*,#27712,.T.);
#36279=ORIENTED_EDGE('',*,*,#26615,.T.);
#36280=ORIENTED_EDGE('',*,*,#27508,.T.);
#36281=ORIENTED_EDGE('',*,*,#27712,.F.);
#36282=ORIENTED_EDGE('',*,*,#27713,.F.);
#36283=ORIENTED_EDGE('',*,*,#26582,.T.);
#36284=ORIENTED_EDGE('',*,*,#26616,.T.);
#36285=ORIENTED_EDGE('',*,*,#27711,.F.);
#36286=ORIENTED_EDGE('',*,*,#27714,.F.);
#36287=ORIENTED_EDGE('',*,*,#26583,.T.);
#36288=ORIENTED_EDGE('',*,*,#27713,.T.);
#36289=ORIENTED_EDGE('',*,*,#27710,.F.);
#36290=ORIENTED_EDGE('',*,*,#27715,.F.);
#36291=ORIENTED_EDGE('',*,*,#26584,.T.);
#36292=ORIENTED_EDGE('',*,*,#27714,.T.);
#36293=ORIENTED_EDGE('',*,*,#27709,.F.);
#36294=ORIENTED_EDGE('',*,*,#27716,.F.);
#36295=ORIENTED_EDGE('',*,*,#26585,.T.);
#36296=ORIENTED_EDGE('',*,*,#27715,.T.);
#36297=ORIENTED_EDGE('',*,*,#27708,.F.);
#36298=ORIENTED_EDGE('',*,*,#27717,.F.);
#36299=ORIENTED_EDGE('',*,*,#26586,.T.);
#36300=ORIENTED_EDGE('',*,*,#27716,.T.);
#36301=ORIENTED_EDGE('',*,*,#27707,.F.);
#36302=ORIENTED_EDGE('',*,*,#27718,.F.);
#36303=ORIENTED_EDGE('',*,*,#26587,.T.);
#36304=ORIENTED_EDGE('',*,*,#27717,.T.);
#36305=ORIENTED_EDGE('',*,*,#27706,.F.);
#36306=ORIENTED_EDGE('',*,*,#27719,.F.);
#36307=ORIENTED_EDGE('',*,*,#26588,.T.);
#36308=ORIENTED_EDGE('',*,*,#27718,.T.);
#36309=ORIENTED_EDGE('',*,*,#27705,.F.);
#36310=ORIENTED_EDGE('',*,*,#27720,.F.);
#36311=ORIENTED_EDGE('',*,*,#26589,.T.);
#36312=ORIENTED_EDGE('',*,*,#27719,.T.);
#36313=ORIENTED_EDGE('',*,*,#27704,.F.);
#36314=ORIENTED_EDGE('',*,*,#27721,.F.);
#36315=ORIENTED_EDGE('',*,*,#26590,.T.);
#36316=ORIENTED_EDGE('',*,*,#27720,.T.);
#36317=ORIENTED_EDGE('',*,*,#27703,.F.);
#36318=ORIENTED_EDGE('',*,*,#27722,.F.);
#36319=ORIENTED_EDGE('',*,*,#26591,.T.);
#36320=ORIENTED_EDGE('',*,*,#27721,.T.);
#36321=ORIENTED_EDGE('',*,*,#27702,.F.);
#36322=ORIENTED_EDGE('',*,*,#27723,.F.);
#36323=ORIENTED_EDGE('',*,*,#26592,.T.);
#36324=ORIENTED_EDGE('',*,*,#27722,.T.);
#36325=ORIENTED_EDGE('',*,*,#27701,.F.);
#36326=ORIENTED_EDGE('',*,*,#27724,.F.);
#36327=ORIENTED_EDGE('',*,*,#26593,.T.);
#36328=ORIENTED_EDGE('',*,*,#27723,.T.);
#36329=ORIENTED_EDGE('',*,*,#27700,.F.);
#36330=ORIENTED_EDGE('',*,*,#27725,.F.);
#36331=ORIENTED_EDGE('',*,*,#26594,.T.);
#36332=ORIENTED_EDGE('',*,*,#27724,.T.);
#36333=ORIENTED_EDGE('',*,*,#26775,.T.);
#36334=ORIENTED_EDGE('',*,*,#26595,.T.);
#36335=ORIENTED_EDGE('',*,*,#27725,.T.);
#36336=ORIENTED_EDGE('',*,*,#27699,.F.);
#36337=ORIENTED_EDGE('',*,*,#27726,.F.);
#36338=ORIENTED_EDGE('',*,*,#27343,.T.);
#36339=ORIENTED_EDGE('',*,*,#27325,.T.);
#36340=ORIENTED_EDGE('',*,*,#27727,.F.);
#36341=ORIENTED_EDGE('',*,*,#27728,.F.);
#36342=ORIENTED_EDGE('',*,*,#26598,.T.);
#36343=ORIENTED_EDGE('',*,*,#27028,.T.);
#36344=ORIENTED_EDGE('',*,*,#27729,.F.);
#36345=ORIENTED_EDGE('',*,*,#27730,.F.);
#36346=ORIENTED_EDGE('',*,*,#26599,.T.);
#36347=ORIENTED_EDGE('',*,*,#27728,.T.);
#36348=ORIENTED_EDGE('',*,*,#27731,.F.);
#36349=ORIENTED_EDGE('',*,*,#27732,.F.);
#36350=ORIENTED_EDGE('',*,*,#26600,.T.);
#36351=ORIENTED_EDGE('',*,*,#27730,.T.);
#36352=ORIENTED_EDGE('',*,*,#27733,.F.);
#36353=ORIENTED_EDGE('',*,*,#27734,.F.);
#36354=ORIENTED_EDGE('',*,*,#26601,.T.);
#36355=ORIENTED_EDGE('',*,*,#27732,.T.);
#36356=ORIENTED_EDGE('',*,*,#27735,.F.);
#36357=ORIENTED_EDGE('',*,*,#27736,.F.);
#36358=ORIENTED_EDGE('',*,*,#26602,.T.);
#36359=ORIENTED_EDGE('',*,*,#27734,.T.);
#36360=ORIENTED_EDGE('',*,*,#27737,.F.);
#36361=ORIENTED_EDGE('',*,*,#27738,.F.);
#36362=ORIENTED_EDGE('',*,*,#26603,.T.);
#36363=ORIENTED_EDGE('',*,*,#27736,.T.);
#36364=ORIENTED_EDGE('',*,*,#27739,.F.);
#36365=ORIENTED_EDGE('',*,*,#27740,.F.);
#36366=ORIENTED_EDGE('',*,*,#26604,.T.);
#36367=ORIENTED_EDGE('',*,*,#27738,.T.);
#36368=ORIENTED_EDGE('',*,*,#27741,.F.);
#36369=ORIENTED_EDGE('',*,*,#27742,.F.);
#36370=ORIENTED_EDGE('',*,*,#26605,.T.);
#36371=ORIENTED_EDGE('',*,*,#27740,.T.);
#36372=ORIENTED_EDGE('',*,*,#27743,.F.);
#36373=ORIENTED_EDGE('',*,*,#27744,.F.);
#36374=ORIENTED_EDGE('',*,*,#26606,.T.);
#36375=ORIENTED_EDGE('',*,*,#27742,.T.);
#36376=ORIENTED_EDGE('',*,*,#27745,.F.);
#36377=ORIENTED_EDGE('',*,*,#27746,.F.);
#36378=ORIENTED_EDGE('',*,*,#26607,.T.);
#36379=ORIENTED_EDGE('',*,*,#27744,.T.);
#36380=ORIENTED_EDGE('',*,*,#27747,.F.);
#36381=ORIENTED_EDGE('',*,*,#27748,.F.);
#36382=ORIENTED_EDGE('',*,*,#26608,.T.);
#36383=ORIENTED_EDGE('',*,*,#27746,.T.);
#36384=ORIENTED_EDGE('',*,*,#27749,.F.);
#36385=ORIENTED_EDGE('',*,*,#27750,.F.);
#36386=ORIENTED_EDGE('',*,*,#26609,.T.);
#36387=ORIENTED_EDGE('',*,*,#27748,.T.);
#36388=ORIENTED_EDGE('',*,*,#27751,.F.);
#36389=ORIENTED_EDGE('',*,*,#27137,.F.);
#36390=ORIENTED_EDGE('',*,*,#26610,.T.);
#36391=ORIENTED_EDGE('',*,*,#27750,.T.);
#36392=ORIENTED_EDGE('',*,*,#27112,.T.);
#36393=ORIENTED_EDGE('',*,*,#27140,.F.);
#36394=ORIENTED_EDGE('',*,*,#27509,.F.);
#36395=ORIENTED_EDGE('',*,*,#26613,.F.);
#36396=ORIENTED_EDGE('',*,*,#27138,.T.);
#36397=ORIENTED_EDGE('',*,*,#27751,.T.);
#36398=ORIENTED_EDGE('',*,*,#27749,.T.);
#36399=ORIENTED_EDGE('',*,*,#27747,.T.);
#36400=ORIENTED_EDGE('',*,*,#27745,.T.);
#36401=ORIENTED_EDGE('',*,*,#27743,.T.);
#36402=ORIENTED_EDGE('',*,*,#27741,.T.);
#36403=ORIENTED_EDGE('',*,*,#27739,.T.);
#36404=ORIENTED_EDGE('',*,*,#27737,.T.);
#36405=ORIENTED_EDGE('',*,*,#27735,.T.);
#36406=ORIENTED_EDGE('',*,*,#27733,.T.);
#36407=ORIENTED_EDGE('',*,*,#27731,.T.);
#36408=ORIENTED_EDGE('',*,*,#27729,.T.);
#36409=ORIENTED_EDGE('',*,*,#27727,.T.);
#36410=ORIENTED_EDGE('',*,*,#27027,.T.);
#36411=ORIENTED_EDGE('',*,*,#27752,.F.);
#36412=ORIENTED_EDGE('',*,*,#27753,.T.);
#36413=ORIENTED_EDGE('',*,*,#27754,.T.);
#36414=ORIENTED_EDGE('',*,*,#27755,.T.);
#36415=ORIENTED_EDGE('',*,*,#27756,.T.);
#36416=ORIENTED_EDGE('',*,*,#27757,.T.);
#36417=ORIENTED_EDGE('',*,*,#27758,.T.);
#36418=ORIENTED_EDGE('',*,*,#27759,.T.);
#36419=ORIENTED_EDGE('',*,*,#27760,.T.);
#36420=ORIENTED_EDGE('',*,*,#27761,.T.);
#36421=ORIENTED_EDGE('',*,*,#27762,.T.);
#36422=ORIENTED_EDGE('',*,*,#27763,.T.);
#36423=ORIENTED_EDGE('',*,*,#27764,.T.);
#36424=ORIENTED_EDGE('',*,*,#27765,.T.);
#36425=ORIENTED_EDGE('',*,*,#27766,.T.);
#36426=ORIENTED_EDGE('',*,*,#26579,.T.);
#36427=ORIENTED_EDGE('',*,*,#27510,.T.);
#36428=ORIENTED_EDGE('',*,*,#27766,.F.);
#36429=ORIENTED_EDGE('',*,*,#27767,.F.);
#36430=ORIENTED_EDGE('',*,*,#26546,.T.);
#36431=ORIENTED_EDGE('',*,*,#26580,.T.);
#36432=ORIENTED_EDGE('',*,*,#27765,.F.);
#36433=ORIENTED_EDGE('',*,*,#27768,.F.);
#36434=ORIENTED_EDGE('',*,*,#26547,.T.);
#36435=ORIENTED_EDGE('',*,*,#27767,.T.);
#36436=ORIENTED_EDGE('',*,*,#27764,.F.);
#36437=ORIENTED_EDGE('',*,*,#27769,.F.);
#36438=ORIENTED_EDGE('',*,*,#26548,.T.);
#36439=ORIENTED_EDGE('',*,*,#27768,.T.);
#36440=ORIENTED_EDGE('',*,*,#27763,.F.);
#36441=ORIENTED_EDGE('',*,*,#27770,.F.);
#36442=ORIENTED_EDGE('',*,*,#26549,.T.);
#36443=ORIENTED_EDGE('',*,*,#27769,.T.);
#36444=ORIENTED_EDGE('',*,*,#27762,.F.);
#36445=ORIENTED_EDGE('',*,*,#27771,.F.);
#36446=ORIENTED_EDGE('',*,*,#26550,.T.);
#36447=ORIENTED_EDGE('',*,*,#27770,.T.);
#36448=ORIENTED_EDGE('',*,*,#27761,.F.);
#36449=ORIENTED_EDGE('',*,*,#27772,.F.);
#36450=ORIENTED_EDGE('',*,*,#26551,.T.);
#36451=ORIENTED_EDGE('',*,*,#27771,.T.);
#36452=ORIENTED_EDGE('',*,*,#27760,.F.);
#36453=ORIENTED_EDGE('',*,*,#27773,.F.);
#36454=ORIENTED_EDGE('',*,*,#26552,.T.);
#36455=ORIENTED_EDGE('',*,*,#27772,.T.);
#36456=ORIENTED_EDGE('',*,*,#27759,.F.);
#36457=ORIENTED_EDGE('',*,*,#27774,.F.);
#36458=ORIENTED_EDGE('',*,*,#26553,.T.);
#36459=ORIENTED_EDGE('',*,*,#27773,.T.);
#36460=ORIENTED_EDGE('',*,*,#27758,.F.);
#36461=ORIENTED_EDGE('',*,*,#27775,.F.);
#36462=ORIENTED_EDGE('',*,*,#26554,.T.);
#36463=ORIENTED_EDGE('',*,*,#27774,.T.);
#36464=ORIENTED_EDGE('',*,*,#27757,.F.);
#36465=ORIENTED_EDGE('',*,*,#27776,.F.);
#36466=ORIENTED_EDGE('',*,*,#26555,.T.);
#36467=ORIENTED_EDGE('',*,*,#27775,.T.);
#36468=ORIENTED_EDGE('',*,*,#27756,.F.);
#36469=ORIENTED_EDGE('',*,*,#27777,.F.);
#36470=ORIENTED_EDGE('',*,*,#26556,.T.);
#36471=ORIENTED_EDGE('',*,*,#27776,.T.);
#36472=ORIENTED_EDGE('',*,*,#27755,.F.);
#36473=ORIENTED_EDGE('',*,*,#27778,.F.);
#36474=ORIENTED_EDGE('',*,*,#26557,.T.);
#36475=ORIENTED_EDGE('',*,*,#27777,.T.);
#36476=ORIENTED_EDGE('',*,*,#27754,.F.);
#36477=ORIENTED_EDGE('',*,*,#27779,.F.);
#36478=ORIENTED_EDGE('',*,*,#26558,.T.);
#36479=ORIENTED_EDGE('',*,*,#27778,.T.);
#36480=ORIENTED_EDGE('',*,*,#26778,.T.);
#36481=ORIENTED_EDGE('',*,*,#26559,.T.);
#36482=ORIENTED_EDGE('',*,*,#27779,.T.);
#36483=ORIENTED_EDGE('',*,*,#27753,.F.);
#36484=ORIENTED_EDGE('',*,*,#27780,.F.);
#36485=ORIENTED_EDGE('',*,*,#27345,.T.);
#36486=ORIENTED_EDGE('',*,*,#27323,.T.);
#36487=ORIENTED_EDGE('',*,*,#27781,.F.);
#36488=ORIENTED_EDGE('',*,*,#27782,.F.);
#36489=ORIENTED_EDGE('',*,*,#26562,.T.);
#36490=ORIENTED_EDGE('',*,*,#27023,.T.);
#36491=ORIENTED_EDGE('',*,*,#27783,.F.);
#36492=ORIENTED_EDGE('',*,*,#27784,.F.);
#36493=ORIENTED_EDGE('',*,*,#26563,.T.);
#36494=ORIENTED_EDGE('',*,*,#27782,.T.);
#36495=ORIENTED_EDGE('',*,*,#27785,.F.);
#36496=ORIENTED_EDGE('',*,*,#27786,.F.);
#36497=ORIENTED_EDGE('',*,*,#26564,.T.);
#36498=ORIENTED_EDGE('',*,*,#27784,.T.);
#36499=ORIENTED_EDGE('',*,*,#27787,.F.);
#36500=ORIENTED_EDGE('',*,*,#27788,.F.);
#36501=ORIENTED_EDGE('',*,*,#26565,.T.);
#36502=ORIENTED_EDGE('',*,*,#27786,.T.);
#36503=ORIENTED_EDGE('',*,*,#27789,.F.);
#36504=ORIENTED_EDGE('',*,*,#27790,.F.);
#36505=ORIENTED_EDGE('',*,*,#26566,.T.);
#36506=ORIENTED_EDGE('',*,*,#27788,.T.);
#36507=ORIENTED_EDGE('',*,*,#27791,.F.);
#36508=ORIENTED_EDGE('',*,*,#27792,.F.);
#36509=ORIENTED_EDGE('',*,*,#26567,.T.);
#36510=ORIENTED_EDGE('',*,*,#27790,.T.);
#36511=ORIENTED_EDGE('',*,*,#27793,.F.);
#36512=ORIENTED_EDGE('',*,*,#27794,.F.);
#36513=ORIENTED_EDGE('',*,*,#26568,.T.);
#36514=ORIENTED_EDGE('',*,*,#27792,.T.);
#36515=ORIENTED_EDGE('',*,*,#27795,.F.);
#36516=ORIENTED_EDGE('',*,*,#27796,.F.);
#36517=ORIENTED_EDGE('',*,*,#26569,.T.);
#36518=ORIENTED_EDGE('',*,*,#27794,.T.);
#36519=ORIENTED_EDGE('',*,*,#27797,.F.);
#36520=ORIENTED_EDGE('',*,*,#27798,.F.);
#36521=ORIENTED_EDGE('',*,*,#26570,.T.);
#36522=ORIENTED_EDGE('',*,*,#27796,.T.);
#36523=ORIENTED_EDGE('',*,*,#27799,.F.);
#36524=ORIENTED_EDGE('',*,*,#27800,.F.);
#36525=ORIENTED_EDGE('',*,*,#26571,.T.);
#36526=ORIENTED_EDGE('',*,*,#27798,.T.);
#36527=ORIENTED_EDGE('',*,*,#27801,.F.);
#36528=ORIENTED_EDGE('',*,*,#27802,.F.);
#36529=ORIENTED_EDGE('',*,*,#26572,.T.);
#36530=ORIENTED_EDGE('',*,*,#27800,.T.);
#36531=ORIENTED_EDGE('',*,*,#27803,.F.);
#36532=ORIENTED_EDGE('',*,*,#27804,.F.);
#36533=ORIENTED_EDGE('',*,*,#26573,.T.);
#36534=ORIENTED_EDGE('',*,*,#27802,.T.);
#36535=ORIENTED_EDGE('',*,*,#27805,.F.);
#36536=ORIENTED_EDGE('',*,*,#27141,.F.);
#36537=ORIENTED_EDGE('',*,*,#26574,.T.);
#36538=ORIENTED_EDGE('',*,*,#27804,.T.);
#36539=ORIENTED_EDGE('',*,*,#27110,.T.);
#36540=ORIENTED_EDGE('',*,*,#27144,.F.);
#36541=ORIENTED_EDGE('',*,*,#27511,.F.);
#36542=ORIENTED_EDGE('',*,*,#26577,.F.);
#36543=ORIENTED_EDGE('',*,*,#27142,.T.);
#36544=ORIENTED_EDGE('',*,*,#27805,.T.);
#36545=ORIENTED_EDGE('',*,*,#27803,.T.);
#36546=ORIENTED_EDGE('',*,*,#27801,.T.);
#36547=ORIENTED_EDGE('',*,*,#27799,.T.);
#36548=ORIENTED_EDGE('',*,*,#27797,.T.);
#36549=ORIENTED_EDGE('',*,*,#27795,.T.);
#36550=ORIENTED_EDGE('',*,*,#27793,.T.);
#36551=ORIENTED_EDGE('',*,*,#27791,.T.);
#36552=ORIENTED_EDGE('',*,*,#27789,.T.);
#36553=ORIENTED_EDGE('',*,*,#27787,.T.);
#36554=ORIENTED_EDGE('',*,*,#27785,.T.);
#36555=ORIENTED_EDGE('',*,*,#27783,.T.);
#36556=ORIENTED_EDGE('',*,*,#27781,.T.);
#36557=ORIENTED_EDGE('',*,*,#27022,.T.);
#36558=ORIENTED_EDGE('',*,*,#27806,.F.);
#36559=ORIENTED_EDGE('',*,*,#27807,.T.);
#36560=ORIENTED_EDGE('',*,*,#27808,.T.);
#36561=ORIENTED_EDGE('',*,*,#27809,.T.);
#36562=ORIENTED_EDGE('',*,*,#27810,.T.);
#36563=ORIENTED_EDGE('',*,*,#27811,.T.);
#36564=ORIENTED_EDGE('',*,*,#27812,.T.);
#36565=ORIENTED_EDGE('',*,*,#27813,.T.);
#36566=ORIENTED_EDGE('',*,*,#27814,.T.);
#36567=ORIENTED_EDGE('',*,*,#27815,.T.);
#36568=ORIENTED_EDGE('',*,*,#27816,.T.);
#36569=ORIENTED_EDGE('',*,*,#27817,.T.);
#36570=ORIENTED_EDGE('',*,*,#27818,.T.);
#36571=ORIENTED_EDGE('',*,*,#27819,.T.);
#36572=ORIENTED_EDGE('',*,*,#27820,.T.);
#36573=ORIENTED_EDGE('',*,*,#26543,.T.);
#36574=ORIENTED_EDGE('',*,*,#27512,.T.);
#36575=ORIENTED_EDGE('',*,*,#27820,.F.);
#36576=ORIENTED_EDGE('',*,*,#27821,.F.);
#36577=ORIENTED_EDGE('',*,*,#26510,.T.);
#36578=ORIENTED_EDGE('',*,*,#26544,.T.);
#36579=ORIENTED_EDGE('',*,*,#27819,.F.);
#36580=ORIENTED_EDGE('',*,*,#27822,.F.);
#36581=ORIENTED_EDGE('',*,*,#26511,.T.);
#36582=ORIENTED_EDGE('',*,*,#27821,.T.);
#36583=ORIENTED_EDGE('',*,*,#27818,.F.);
#36584=ORIENTED_EDGE('',*,*,#27823,.F.);
#36585=ORIENTED_EDGE('',*,*,#26512,.T.);
#36586=ORIENTED_EDGE('',*,*,#27822,.T.);
#36587=ORIENTED_EDGE('',*,*,#27817,.F.);
#36588=ORIENTED_EDGE('',*,*,#27824,.F.);
#36589=ORIENTED_EDGE('',*,*,#26513,.T.);
#36590=ORIENTED_EDGE('',*,*,#27823,.T.);
#36591=ORIENTED_EDGE('',*,*,#27816,.F.);
#36592=ORIENTED_EDGE('',*,*,#27825,.F.);
#36593=ORIENTED_EDGE('',*,*,#26514,.T.);
#36594=ORIENTED_EDGE('',*,*,#27824,.T.);
#36595=ORIENTED_EDGE('',*,*,#27815,.F.);
#36596=ORIENTED_EDGE('',*,*,#27826,.F.);
#36597=ORIENTED_EDGE('',*,*,#26515,.T.);
#36598=ORIENTED_EDGE('',*,*,#27825,.T.);
#36599=ORIENTED_EDGE('',*,*,#27814,.F.);
#36600=ORIENTED_EDGE('',*,*,#27827,.F.);
#36601=ORIENTED_EDGE('',*,*,#26516,.T.);
#36602=ORIENTED_EDGE('',*,*,#27826,.T.);
#36603=ORIENTED_EDGE('',*,*,#27813,.F.);
#36604=ORIENTED_EDGE('',*,*,#27828,.F.);
#36605=ORIENTED_EDGE('',*,*,#26517,.T.);
#36606=ORIENTED_EDGE('',*,*,#27827,.T.);
#36607=ORIENTED_EDGE('',*,*,#27812,.F.);
#36608=ORIENTED_EDGE('',*,*,#27829,.F.);
#36609=ORIENTED_EDGE('',*,*,#26518,.T.);
#36610=ORIENTED_EDGE('',*,*,#27828,.T.);
#36611=ORIENTED_EDGE('',*,*,#27811,.F.);
#36612=ORIENTED_EDGE('',*,*,#27830,.F.);
#36613=ORIENTED_EDGE('',*,*,#26519,.T.);
#36614=ORIENTED_EDGE('',*,*,#27829,.T.);
#36615=ORIENTED_EDGE('',*,*,#27810,.F.);
#36616=ORIENTED_EDGE('',*,*,#27831,.F.);
#36617=ORIENTED_EDGE('',*,*,#26520,.T.);
#36618=ORIENTED_EDGE('',*,*,#27830,.T.);
#36619=ORIENTED_EDGE('',*,*,#27809,.F.);
#36620=ORIENTED_EDGE('',*,*,#27832,.F.);
#36621=ORIENTED_EDGE('',*,*,#26521,.T.);
#36622=ORIENTED_EDGE('',*,*,#27831,.T.);
#36623=ORIENTED_EDGE('',*,*,#27808,.F.);
#36624=ORIENTED_EDGE('',*,*,#27833,.F.);
#36625=ORIENTED_EDGE('',*,*,#26522,.T.);
#36626=ORIENTED_EDGE('',*,*,#27832,.T.);
#36627=ORIENTED_EDGE('',*,*,#26781,.T.);
#36628=ORIENTED_EDGE('',*,*,#26523,.T.);
#36629=ORIENTED_EDGE('',*,*,#27833,.T.);
#36630=ORIENTED_EDGE('',*,*,#27807,.F.);
#36631=ORIENTED_EDGE('',*,*,#27834,.F.);
#36632=ORIENTED_EDGE('',*,*,#27347,.T.);
#36633=ORIENTED_EDGE('',*,*,#27321,.T.);
#36634=ORIENTED_EDGE('',*,*,#27835,.F.);
#36635=ORIENTED_EDGE('',*,*,#27836,.F.);
#36636=ORIENTED_EDGE('',*,*,#26526,.T.);
#36637=ORIENTED_EDGE('',*,*,#27018,.T.);
#36638=ORIENTED_EDGE('',*,*,#27837,.F.);
#36639=ORIENTED_EDGE('',*,*,#27838,.F.);
#36640=ORIENTED_EDGE('',*,*,#26527,.T.);
#36641=ORIENTED_EDGE('',*,*,#27836,.T.);
#36642=ORIENTED_EDGE('',*,*,#27839,.F.);
#36643=ORIENTED_EDGE('',*,*,#27840,.F.);
#36644=ORIENTED_EDGE('',*,*,#26528,.T.);
#36645=ORIENTED_EDGE('',*,*,#27838,.T.);
#36646=ORIENTED_EDGE('',*,*,#27841,.F.);
#36647=ORIENTED_EDGE('',*,*,#27842,.F.);
#36648=ORIENTED_EDGE('',*,*,#26529,.T.);
#36649=ORIENTED_EDGE('',*,*,#27840,.T.);
#36650=ORIENTED_EDGE('',*,*,#27843,.F.);
#36651=ORIENTED_EDGE('',*,*,#27844,.F.);
#36652=ORIENTED_EDGE('',*,*,#26530,.T.);
#36653=ORIENTED_EDGE('',*,*,#27842,.T.);
#36654=ORIENTED_EDGE('',*,*,#27845,.F.);
#36655=ORIENTED_EDGE('',*,*,#27846,.F.);
#36656=ORIENTED_EDGE('',*,*,#26531,.T.);
#36657=ORIENTED_EDGE('',*,*,#27844,.T.);
#36658=ORIENTED_EDGE('',*,*,#27847,.F.);
#36659=ORIENTED_EDGE('',*,*,#27848,.F.);
#36660=ORIENTED_EDGE('',*,*,#26532,.T.);
#36661=ORIENTED_EDGE('',*,*,#27846,.T.);
#36662=ORIENTED_EDGE('',*,*,#27849,.F.);
#36663=ORIENTED_EDGE('',*,*,#27850,.F.);
#36664=ORIENTED_EDGE('',*,*,#26533,.T.);
#36665=ORIENTED_EDGE('',*,*,#27848,.T.);
#36666=ORIENTED_EDGE('',*,*,#27851,.F.);
#36667=ORIENTED_EDGE('',*,*,#27852,.F.);
#36668=ORIENTED_EDGE('',*,*,#26534,.T.);
#36669=ORIENTED_EDGE('',*,*,#27850,.T.);
#36670=ORIENTED_EDGE('',*,*,#27853,.F.);
#36671=ORIENTED_EDGE('',*,*,#27854,.F.);
#36672=ORIENTED_EDGE('',*,*,#26535,.T.);
#36673=ORIENTED_EDGE('',*,*,#27852,.T.);
#36674=ORIENTED_EDGE('',*,*,#27855,.F.);
#36675=ORIENTED_EDGE('',*,*,#27856,.F.);
#36676=ORIENTED_EDGE('',*,*,#26536,.T.);
#36677=ORIENTED_EDGE('',*,*,#27854,.T.);
#36678=ORIENTED_EDGE('',*,*,#27857,.F.);
#36679=ORIENTED_EDGE('',*,*,#27858,.F.);
#36680=ORIENTED_EDGE('',*,*,#26537,.T.);
#36681=ORIENTED_EDGE('',*,*,#27856,.T.);
#36682=ORIENTED_EDGE('',*,*,#27859,.F.);
#36683=ORIENTED_EDGE('',*,*,#27145,.F.);
#36684=ORIENTED_EDGE('',*,*,#26538,.T.);
#36685=ORIENTED_EDGE('',*,*,#27858,.T.);
#36686=ORIENTED_EDGE('',*,*,#27108,.T.);
#36687=ORIENTED_EDGE('',*,*,#27148,.F.);
#36688=ORIENTED_EDGE('',*,*,#27513,.F.);
#36689=ORIENTED_EDGE('',*,*,#26541,.F.);
#36690=ORIENTED_EDGE('',*,*,#27146,.T.);
#36691=ORIENTED_EDGE('',*,*,#27859,.T.);
#36692=ORIENTED_EDGE('',*,*,#27857,.T.);
#36693=ORIENTED_EDGE('',*,*,#27855,.T.);
#36694=ORIENTED_EDGE('',*,*,#27853,.T.);
#36695=ORIENTED_EDGE('',*,*,#27851,.T.);
#36696=ORIENTED_EDGE('',*,*,#27849,.T.);
#36697=ORIENTED_EDGE('',*,*,#27847,.T.);
#36698=ORIENTED_EDGE('',*,*,#27845,.T.);
#36699=ORIENTED_EDGE('',*,*,#27843,.T.);
#36700=ORIENTED_EDGE('',*,*,#27841,.T.);
#36701=ORIENTED_EDGE('',*,*,#27839,.T.);
#36702=ORIENTED_EDGE('',*,*,#27837,.T.);
#36703=ORIENTED_EDGE('',*,*,#27835,.T.);
#36704=ORIENTED_EDGE('',*,*,#27017,.T.);
#36705=ORIENTED_EDGE('',*,*,#27860,.F.);
#36706=ORIENTED_EDGE('',*,*,#27861,.T.);
#36707=ORIENTED_EDGE('',*,*,#27862,.T.);
#36708=ORIENTED_EDGE('',*,*,#27863,.T.);
#36709=ORIENTED_EDGE('',*,*,#27864,.T.);
#36710=ORIENTED_EDGE('',*,*,#27865,.T.);
#36711=ORIENTED_EDGE('',*,*,#27866,.T.);
#36712=ORIENTED_EDGE('',*,*,#27867,.T.);
#36713=ORIENTED_EDGE('',*,*,#27868,.T.);
#36714=ORIENTED_EDGE('',*,*,#27869,.T.);
#36715=ORIENTED_EDGE('',*,*,#27870,.T.);
#36716=ORIENTED_EDGE('',*,*,#27871,.T.);
#36717=ORIENTED_EDGE('',*,*,#27872,.T.);
#36718=ORIENTED_EDGE('',*,*,#27873,.T.);
#36719=ORIENTED_EDGE('',*,*,#27874,.T.);
#36720=ORIENTED_EDGE('',*,*,#26507,.T.);
#36721=ORIENTED_EDGE('',*,*,#27514,.T.);
#36722=ORIENTED_EDGE('',*,*,#27874,.F.);
#36723=ORIENTED_EDGE('',*,*,#27875,.F.);
#36724=ORIENTED_EDGE('',*,*,#26474,.T.);
#36725=ORIENTED_EDGE('',*,*,#26508,.T.);
#36726=ORIENTED_EDGE('',*,*,#27873,.F.);
#36727=ORIENTED_EDGE('',*,*,#27876,.F.);
#36728=ORIENTED_EDGE('',*,*,#26475,.T.);
#36729=ORIENTED_EDGE('',*,*,#27875,.T.);
#36730=ORIENTED_EDGE('',*,*,#27872,.F.);
#36731=ORIENTED_EDGE('',*,*,#27877,.F.);
#36732=ORIENTED_EDGE('',*,*,#26476,.T.);
#36733=ORIENTED_EDGE('',*,*,#27876,.T.);
#36734=ORIENTED_EDGE('',*,*,#27871,.F.);
#36735=ORIENTED_EDGE('',*,*,#27878,.F.);
#36736=ORIENTED_EDGE('',*,*,#26477,.T.);
#36737=ORIENTED_EDGE('',*,*,#27877,.T.);
#36738=ORIENTED_EDGE('',*,*,#27870,.F.);
#36739=ORIENTED_EDGE('',*,*,#27879,.F.);
#36740=ORIENTED_EDGE('',*,*,#26478,.T.);
#36741=ORIENTED_EDGE('',*,*,#27878,.T.);
#36742=ORIENTED_EDGE('',*,*,#27869,.F.);
#36743=ORIENTED_EDGE('',*,*,#27880,.F.);
#36744=ORIENTED_EDGE('',*,*,#26479,.T.);
#36745=ORIENTED_EDGE('',*,*,#27879,.T.);
#36746=ORIENTED_EDGE('',*,*,#27868,.F.);
#36747=ORIENTED_EDGE('',*,*,#27881,.F.);
#36748=ORIENTED_EDGE('',*,*,#26480,.T.);
#36749=ORIENTED_EDGE('',*,*,#27880,.T.);
#36750=ORIENTED_EDGE('',*,*,#27867,.F.);
#36751=ORIENTED_EDGE('',*,*,#27882,.F.);
#36752=ORIENTED_EDGE('',*,*,#26481,.T.);
#36753=ORIENTED_EDGE('',*,*,#27881,.T.);
#36754=ORIENTED_EDGE('',*,*,#27866,.F.);
#36755=ORIENTED_EDGE('',*,*,#27883,.F.);
#36756=ORIENTED_EDGE('',*,*,#26482,.T.);
#36757=ORIENTED_EDGE('',*,*,#27882,.T.);
#36758=ORIENTED_EDGE('',*,*,#27865,.F.);
#36759=ORIENTED_EDGE('',*,*,#27884,.F.);
#36760=ORIENTED_EDGE('',*,*,#26483,.T.);
#36761=ORIENTED_EDGE('',*,*,#27883,.T.);
#36762=ORIENTED_EDGE('',*,*,#27864,.F.);
#36763=ORIENTED_EDGE('',*,*,#27885,.F.);
#36764=ORIENTED_EDGE('',*,*,#26484,.T.);
#36765=ORIENTED_EDGE('',*,*,#27884,.T.);
#36766=ORIENTED_EDGE('',*,*,#27863,.F.);
#36767=ORIENTED_EDGE('',*,*,#27886,.F.);
#36768=ORIENTED_EDGE('',*,*,#26485,.T.);
#36769=ORIENTED_EDGE('',*,*,#27885,.T.);
#36770=ORIENTED_EDGE('',*,*,#27862,.F.);
#36771=ORIENTED_EDGE('',*,*,#27887,.F.);
#36772=ORIENTED_EDGE('',*,*,#26486,.T.);
#36773=ORIENTED_EDGE('',*,*,#27886,.T.);
#36774=ORIENTED_EDGE('',*,*,#26784,.T.);
#36775=ORIENTED_EDGE('',*,*,#26487,.T.);
#36776=ORIENTED_EDGE('',*,*,#27887,.T.);
#36777=ORIENTED_EDGE('',*,*,#27861,.F.);
#36778=ORIENTED_EDGE('',*,*,#27888,.F.);
#36779=ORIENTED_EDGE('',*,*,#27349,.T.);
#36780=ORIENTED_EDGE('',*,*,#27319,.T.);
#36781=ORIENTED_EDGE('',*,*,#27889,.F.);
#36782=ORIENTED_EDGE('',*,*,#27890,.F.);
#36783=ORIENTED_EDGE('',*,*,#26490,.T.);
#36784=ORIENTED_EDGE('',*,*,#27013,.T.);
#36785=ORIENTED_EDGE('',*,*,#27891,.F.);
#36786=ORIENTED_EDGE('',*,*,#27892,.F.);
#36787=ORIENTED_EDGE('',*,*,#26491,.T.);
#36788=ORIENTED_EDGE('',*,*,#27890,.T.);
#36789=ORIENTED_EDGE('',*,*,#27893,.F.);
#36790=ORIENTED_EDGE('',*,*,#27894,.F.);
#36791=ORIENTED_EDGE('',*,*,#26492,.T.);
#36792=ORIENTED_EDGE('',*,*,#27892,.T.);
#36793=ORIENTED_EDGE('',*,*,#27895,.F.);
#36794=ORIENTED_EDGE('',*,*,#27896,.F.);
#36795=ORIENTED_EDGE('',*,*,#26493,.T.);
#36796=ORIENTED_EDGE('',*,*,#27894,.T.);
#36797=ORIENTED_EDGE('',*,*,#27897,.F.);
#36798=ORIENTED_EDGE('',*,*,#27898,.F.);
#36799=ORIENTED_EDGE('',*,*,#26494,.T.);
#36800=ORIENTED_EDGE('',*,*,#27896,.T.);
#36801=ORIENTED_EDGE('',*,*,#27899,.F.);
#36802=ORIENTED_EDGE('',*,*,#27900,.F.);
#36803=ORIENTED_EDGE('',*,*,#26495,.T.);
#36804=ORIENTED_EDGE('',*,*,#27898,.T.);
#36805=ORIENTED_EDGE('',*,*,#27901,.F.);
#36806=ORIENTED_EDGE('',*,*,#27902,.F.);
#36807=ORIENTED_EDGE('',*,*,#26496,.T.);
#36808=ORIENTED_EDGE('',*,*,#27900,.T.);
#36809=ORIENTED_EDGE('',*,*,#27903,.F.);
#36810=ORIENTED_EDGE('',*,*,#27904,.F.);
#36811=ORIENTED_EDGE('',*,*,#26497,.T.);
#36812=ORIENTED_EDGE('',*,*,#27902,.T.);
#36813=ORIENTED_EDGE('',*,*,#27905,.F.);
#36814=ORIENTED_EDGE('',*,*,#27906,.F.);
#36815=ORIENTED_EDGE('',*,*,#26498,.T.);
#36816=ORIENTED_EDGE('',*,*,#27904,.T.);
#36817=ORIENTED_EDGE('',*,*,#27907,.F.);
#36818=ORIENTED_EDGE('',*,*,#27908,.F.);
#36819=ORIENTED_EDGE('',*,*,#26499,.T.);
#36820=ORIENTED_EDGE('',*,*,#27906,.T.);
#36821=ORIENTED_EDGE('',*,*,#27909,.F.);
#36822=ORIENTED_EDGE('',*,*,#27910,.F.);
#36823=ORIENTED_EDGE('',*,*,#26500,.T.);
#36824=ORIENTED_EDGE('',*,*,#27908,.T.);
#36825=ORIENTED_EDGE('',*,*,#27911,.F.);
#36826=ORIENTED_EDGE('',*,*,#27912,.F.);
#36827=ORIENTED_EDGE('',*,*,#26501,.T.);
#36828=ORIENTED_EDGE('',*,*,#27910,.T.);
#36829=ORIENTED_EDGE('',*,*,#27913,.F.);
#36830=ORIENTED_EDGE('',*,*,#27149,.F.);
#36831=ORIENTED_EDGE('',*,*,#26502,.T.);
#36832=ORIENTED_EDGE('',*,*,#27912,.T.);
#36833=ORIENTED_EDGE('',*,*,#27106,.T.);
#36834=ORIENTED_EDGE('',*,*,#27152,.F.);
#36835=ORIENTED_EDGE('',*,*,#27515,.F.);
#36836=ORIENTED_EDGE('',*,*,#26505,.F.);
#36837=ORIENTED_EDGE('',*,*,#27150,.T.);
#36838=ORIENTED_EDGE('',*,*,#27913,.T.);
#36839=ORIENTED_EDGE('',*,*,#27911,.T.);
#36840=ORIENTED_EDGE('',*,*,#27909,.T.);
#36841=ORIENTED_EDGE('',*,*,#27907,.T.);
#36842=ORIENTED_EDGE('',*,*,#27905,.T.);
#36843=ORIENTED_EDGE('',*,*,#27903,.T.);
#36844=ORIENTED_EDGE('',*,*,#27901,.T.);
#36845=ORIENTED_EDGE('',*,*,#27899,.T.);
#36846=ORIENTED_EDGE('',*,*,#27897,.T.);
#36847=ORIENTED_EDGE('',*,*,#27895,.T.);
#36848=ORIENTED_EDGE('',*,*,#27893,.T.);
#36849=ORIENTED_EDGE('',*,*,#27891,.T.);
#36850=ORIENTED_EDGE('',*,*,#27889,.T.);
#36851=ORIENTED_EDGE('',*,*,#27012,.T.);
#36852=ORIENTED_EDGE('',*,*,#27914,.F.);
#36853=ORIENTED_EDGE('',*,*,#27915,.T.);
#36854=ORIENTED_EDGE('',*,*,#27916,.T.);
#36855=ORIENTED_EDGE('',*,*,#27917,.T.);
#36856=ORIENTED_EDGE('',*,*,#27918,.T.);
#36857=ORIENTED_EDGE('',*,*,#27919,.T.);
#36858=ORIENTED_EDGE('',*,*,#27920,.T.);
#36859=ORIENTED_EDGE('',*,*,#27921,.T.);
#36860=ORIENTED_EDGE('',*,*,#27922,.T.);
#36861=ORIENTED_EDGE('',*,*,#27923,.T.);
#36862=ORIENTED_EDGE('',*,*,#27924,.T.);
#36863=ORIENTED_EDGE('',*,*,#27925,.T.);
#36864=ORIENTED_EDGE('',*,*,#27926,.T.);
#36865=ORIENTED_EDGE('',*,*,#27927,.T.);
#36866=ORIENTED_EDGE('',*,*,#27928,.T.);
#36867=ORIENTED_EDGE('',*,*,#26471,.T.);
#36868=ORIENTED_EDGE('',*,*,#27516,.T.);
#36869=ORIENTED_EDGE('',*,*,#27928,.F.);
#36870=ORIENTED_EDGE('',*,*,#27929,.F.);
#36871=ORIENTED_EDGE('',*,*,#26438,.T.);
#36872=ORIENTED_EDGE('',*,*,#26472,.T.);
#36873=ORIENTED_EDGE('',*,*,#27927,.F.);
#36874=ORIENTED_EDGE('',*,*,#27930,.F.);
#36875=ORIENTED_EDGE('',*,*,#26439,.T.);
#36876=ORIENTED_EDGE('',*,*,#27929,.T.);
#36877=ORIENTED_EDGE('',*,*,#27926,.F.);
#36878=ORIENTED_EDGE('',*,*,#27931,.F.);
#36879=ORIENTED_EDGE('',*,*,#26440,.T.);
#36880=ORIENTED_EDGE('',*,*,#27930,.T.);
#36881=ORIENTED_EDGE('',*,*,#27925,.F.);
#36882=ORIENTED_EDGE('',*,*,#27932,.F.);
#36883=ORIENTED_EDGE('',*,*,#26441,.T.);
#36884=ORIENTED_EDGE('',*,*,#27931,.T.);
#36885=ORIENTED_EDGE('',*,*,#27924,.F.);
#36886=ORIENTED_EDGE('',*,*,#27933,.F.);
#36887=ORIENTED_EDGE('',*,*,#26442,.T.);
#36888=ORIENTED_EDGE('',*,*,#27932,.T.);
#36889=ORIENTED_EDGE('',*,*,#27923,.F.);
#36890=ORIENTED_EDGE('',*,*,#27934,.F.);
#36891=ORIENTED_EDGE('',*,*,#26443,.T.);
#36892=ORIENTED_EDGE('',*,*,#27933,.T.);
#36893=ORIENTED_EDGE('',*,*,#27922,.F.);
#36894=ORIENTED_EDGE('',*,*,#27935,.F.);
#36895=ORIENTED_EDGE('',*,*,#26444,.T.);
#36896=ORIENTED_EDGE('',*,*,#27934,.T.);
#36897=ORIENTED_EDGE('',*,*,#27921,.F.);
#36898=ORIENTED_EDGE('',*,*,#27936,.F.);
#36899=ORIENTED_EDGE('',*,*,#26445,.T.);
#36900=ORIENTED_EDGE('',*,*,#27935,.T.);
#36901=ORIENTED_EDGE('',*,*,#27920,.F.);
#36902=ORIENTED_EDGE('',*,*,#27937,.F.);
#36903=ORIENTED_EDGE('',*,*,#26446,.T.);
#36904=ORIENTED_EDGE('',*,*,#27936,.T.);
#36905=ORIENTED_EDGE('',*,*,#27919,.F.);
#36906=ORIENTED_EDGE('',*,*,#27938,.F.);
#36907=ORIENTED_EDGE('',*,*,#26447,.T.);
#36908=ORIENTED_EDGE('',*,*,#27937,.T.);
#36909=ORIENTED_EDGE('',*,*,#27918,.F.);
#36910=ORIENTED_EDGE('',*,*,#27939,.F.);
#36911=ORIENTED_EDGE('',*,*,#26448,.T.);
#36912=ORIENTED_EDGE('',*,*,#27938,.T.);
#36913=ORIENTED_EDGE('',*,*,#27917,.F.);
#36914=ORIENTED_EDGE('',*,*,#27940,.F.);
#36915=ORIENTED_EDGE('',*,*,#26449,.T.);
#36916=ORIENTED_EDGE('',*,*,#27939,.T.);
#36917=ORIENTED_EDGE('',*,*,#27916,.F.);
#36918=ORIENTED_EDGE('',*,*,#27941,.F.);
#36919=ORIENTED_EDGE('',*,*,#26450,.T.);
#36920=ORIENTED_EDGE('',*,*,#27940,.T.);
#36921=ORIENTED_EDGE('',*,*,#26787,.T.);
#36922=ORIENTED_EDGE('',*,*,#26451,.T.);
#36923=ORIENTED_EDGE('',*,*,#27941,.T.);
#36924=ORIENTED_EDGE('',*,*,#27915,.F.);
#36925=ORIENTED_EDGE('',*,*,#27942,.F.);
#36926=ORIENTED_EDGE('',*,*,#27351,.T.);
#36927=ORIENTED_EDGE('',*,*,#27317,.T.);
#36928=ORIENTED_EDGE('',*,*,#27943,.F.);
#36929=ORIENTED_EDGE('',*,*,#27944,.F.);
#36930=ORIENTED_EDGE('',*,*,#26454,.T.);
#36931=ORIENTED_EDGE('',*,*,#27008,.T.);
#36932=ORIENTED_EDGE('',*,*,#27945,.F.);
#36933=ORIENTED_EDGE('',*,*,#27946,.F.);
#36934=ORIENTED_EDGE('',*,*,#26455,.T.);
#36935=ORIENTED_EDGE('',*,*,#27944,.T.);
#36936=ORIENTED_EDGE('',*,*,#27947,.F.);
#36937=ORIENTED_EDGE('',*,*,#27948,.F.);
#36938=ORIENTED_EDGE('',*,*,#26456,.T.);
#36939=ORIENTED_EDGE('',*,*,#27946,.T.);
#36940=ORIENTED_EDGE('',*,*,#27949,.F.);
#36941=ORIENTED_EDGE('',*,*,#27950,.F.);
#36942=ORIENTED_EDGE('',*,*,#26457,.T.);
#36943=ORIENTED_EDGE('',*,*,#27948,.T.);
#36944=ORIENTED_EDGE('',*,*,#27951,.F.);
#36945=ORIENTED_EDGE('',*,*,#27952,.F.);
#36946=ORIENTED_EDGE('',*,*,#26458,.T.);
#36947=ORIENTED_EDGE('',*,*,#27950,.T.);
#36948=ORIENTED_EDGE('',*,*,#27953,.F.);
#36949=ORIENTED_EDGE('',*,*,#27954,.F.);
#36950=ORIENTED_EDGE('',*,*,#26459,.T.);
#36951=ORIENTED_EDGE('',*,*,#27952,.T.);
#36952=ORIENTED_EDGE('',*,*,#27955,.F.);
#36953=ORIENTED_EDGE('',*,*,#27956,.F.);
#36954=ORIENTED_EDGE('',*,*,#26460,.T.);
#36955=ORIENTED_EDGE('',*,*,#27954,.T.);
#36956=ORIENTED_EDGE('',*,*,#27957,.F.);
#36957=ORIENTED_EDGE('',*,*,#27958,.F.);
#36958=ORIENTED_EDGE('',*,*,#26461,.T.);
#36959=ORIENTED_EDGE('',*,*,#27956,.T.);
#36960=ORIENTED_EDGE('',*,*,#27959,.F.);
#36961=ORIENTED_EDGE('',*,*,#27960,.F.);
#36962=ORIENTED_EDGE('',*,*,#26462,.T.);
#36963=ORIENTED_EDGE('',*,*,#27958,.T.);
#36964=ORIENTED_EDGE('',*,*,#27961,.F.);
#36965=ORIENTED_EDGE('',*,*,#27962,.F.);
#36966=ORIENTED_EDGE('',*,*,#26463,.T.);
#36967=ORIENTED_EDGE('',*,*,#27960,.T.);
#36968=ORIENTED_EDGE('',*,*,#27963,.F.);
#36969=ORIENTED_EDGE('',*,*,#27964,.F.);
#36970=ORIENTED_EDGE('',*,*,#26464,.T.);
#36971=ORIENTED_EDGE('',*,*,#27962,.T.);
#36972=ORIENTED_EDGE('',*,*,#27965,.F.);
#36973=ORIENTED_EDGE('',*,*,#27966,.F.);
#36974=ORIENTED_EDGE('',*,*,#26465,.T.);
#36975=ORIENTED_EDGE('',*,*,#27964,.T.);
#36976=ORIENTED_EDGE('',*,*,#27967,.F.);
#36977=ORIENTED_EDGE('',*,*,#27153,.F.);
#36978=ORIENTED_EDGE('',*,*,#26466,.T.);
#36979=ORIENTED_EDGE('',*,*,#27966,.T.);
#36980=ORIENTED_EDGE('',*,*,#27104,.T.);
#36981=ORIENTED_EDGE('',*,*,#27156,.F.);
#36982=ORIENTED_EDGE('',*,*,#27517,.F.);
#36983=ORIENTED_EDGE('',*,*,#26469,.F.);
#36984=ORIENTED_EDGE('',*,*,#27154,.T.);
#36985=ORIENTED_EDGE('',*,*,#27967,.T.);
#36986=ORIENTED_EDGE('',*,*,#27965,.T.);
#36987=ORIENTED_EDGE('',*,*,#27963,.T.);
#36988=ORIENTED_EDGE('',*,*,#27961,.T.);
#36989=ORIENTED_EDGE('',*,*,#27959,.T.);
#36990=ORIENTED_EDGE('',*,*,#27957,.T.);
#36991=ORIENTED_EDGE('',*,*,#27955,.T.);
#36992=ORIENTED_EDGE('',*,*,#27953,.T.);
#36993=ORIENTED_EDGE('',*,*,#27951,.T.);
#36994=ORIENTED_EDGE('',*,*,#27949,.T.);
#36995=ORIENTED_EDGE('',*,*,#27947,.T.);
#36996=ORIENTED_EDGE('',*,*,#27945,.T.);
#36997=ORIENTED_EDGE('',*,*,#27943,.T.);
#36998=ORIENTED_EDGE('',*,*,#27007,.T.);
#36999=ORIENTED_EDGE('',*,*,#27968,.F.);
#37000=ORIENTED_EDGE('',*,*,#27969,.T.);
#37001=ORIENTED_EDGE('',*,*,#27970,.T.);
#37002=ORIENTED_EDGE('',*,*,#27971,.T.);
#37003=ORIENTED_EDGE('',*,*,#27972,.T.);
#37004=ORIENTED_EDGE('',*,*,#27973,.T.);
#37005=ORIENTED_EDGE('',*,*,#27974,.T.);
#37006=ORIENTED_EDGE('',*,*,#27975,.T.);
#37007=ORIENTED_EDGE('',*,*,#27976,.T.);
#37008=ORIENTED_EDGE('',*,*,#27977,.T.);
#37009=ORIENTED_EDGE('',*,*,#27978,.T.);
#37010=ORIENTED_EDGE('',*,*,#27979,.T.);
#37011=ORIENTED_EDGE('',*,*,#27980,.T.);
#37012=ORIENTED_EDGE('',*,*,#27981,.T.);
#37013=ORIENTED_EDGE('',*,*,#27982,.T.);
#37014=ORIENTED_EDGE('',*,*,#26435,.T.);
#37015=ORIENTED_EDGE('',*,*,#27518,.T.);
#37016=ORIENTED_EDGE('',*,*,#27982,.F.);
#37017=ORIENTED_EDGE('',*,*,#27983,.F.);
#37018=ORIENTED_EDGE('',*,*,#26402,.T.);
#37019=ORIENTED_EDGE('',*,*,#26436,.T.);
#37020=ORIENTED_EDGE('',*,*,#27981,.F.);
#37021=ORIENTED_EDGE('',*,*,#27984,.F.);
#37022=ORIENTED_EDGE('',*,*,#26403,.T.);
#37023=ORIENTED_EDGE('',*,*,#27983,.T.);
#37024=ORIENTED_EDGE('',*,*,#27980,.F.);
#37025=ORIENTED_EDGE('',*,*,#27985,.F.);
#37026=ORIENTED_EDGE('',*,*,#26404,.T.);
#37027=ORIENTED_EDGE('',*,*,#27984,.T.);
#37028=ORIENTED_EDGE('',*,*,#27979,.F.);
#37029=ORIENTED_EDGE('',*,*,#27986,.F.);
#37030=ORIENTED_EDGE('',*,*,#26405,.T.);
#37031=ORIENTED_EDGE('',*,*,#27985,.T.);
#37032=ORIENTED_EDGE('',*,*,#27978,.F.);
#37033=ORIENTED_EDGE('',*,*,#27987,.F.);
#37034=ORIENTED_EDGE('',*,*,#26406,.T.);
#37035=ORIENTED_EDGE('',*,*,#27986,.T.);
#37036=ORIENTED_EDGE('',*,*,#27977,.F.);
#37037=ORIENTED_EDGE('',*,*,#27988,.F.);
#37038=ORIENTED_EDGE('',*,*,#26407,.T.);
#37039=ORIENTED_EDGE('',*,*,#27987,.T.);
#37040=ORIENTED_EDGE('',*,*,#27976,.F.);
#37041=ORIENTED_EDGE('',*,*,#27989,.F.);
#37042=ORIENTED_EDGE('',*,*,#26408,.T.);
#37043=ORIENTED_EDGE('',*,*,#27988,.T.);
#37044=ORIENTED_EDGE('',*,*,#27975,.F.);
#37045=ORIENTED_EDGE('',*,*,#27990,.F.);
#37046=ORIENTED_EDGE('',*,*,#26409,.T.);
#37047=ORIENTED_EDGE('',*,*,#27989,.T.);
#37048=ORIENTED_EDGE('',*,*,#27974,.F.);
#37049=ORIENTED_EDGE('',*,*,#27991,.F.);
#37050=ORIENTED_EDGE('',*,*,#26410,.T.);
#37051=ORIENTED_EDGE('',*,*,#27990,.T.);
#37052=ORIENTED_EDGE('',*,*,#27973,.F.);
#37053=ORIENTED_EDGE('',*,*,#27992,.F.);
#37054=ORIENTED_EDGE('',*,*,#26411,.T.);
#37055=ORIENTED_EDGE('',*,*,#27991,.T.);
#37056=ORIENTED_EDGE('',*,*,#27972,.F.);
#37057=ORIENTED_EDGE('',*,*,#27993,.F.);
#37058=ORIENTED_EDGE('',*,*,#26412,.T.);
#37059=ORIENTED_EDGE('',*,*,#27992,.T.);
#37060=ORIENTED_EDGE('',*,*,#27971,.F.);
#37061=ORIENTED_EDGE('',*,*,#27994,.F.);
#37062=ORIENTED_EDGE('',*,*,#26413,.T.);
#37063=ORIENTED_EDGE('',*,*,#27993,.T.);
#37064=ORIENTED_EDGE('',*,*,#27970,.F.);
#37065=ORIENTED_EDGE('',*,*,#27995,.F.);
#37066=ORIENTED_EDGE('',*,*,#26414,.T.);
#37067=ORIENTED_EDGE('',*,*,#27994,.T.);
#37068=ORIENTED_EDGE('',*,*,#26790,.T.);
#37069=ORIENTED_EDGE('',*,*,#26415,.T.);
#37070=ORIENTED_EDGE('',*,*,#27995,.T.);
#37071=ORIENTED_EDGE('',*,*,#27969,.F.);
#37072=ORIENTED_EDGE('',*,*,#27996,.F.);
#37073=ORIENTED_EDGE('',*,*,#27353,.T.);
#37074=ORIENTED_EDGE('',*,*,#27315,.T.);
#37075=ORIENTED_EDGE('',*,*,#27997,.F.);
#37076=ORIENTED_EDGE('',*,*,#27998,.F.);
#37077=ORIENTED_EDGE('',*,*,#26418,.T.);
#37078=ORIENTED_EDGE('',*,*,#27003,.T.);
#37079=ORIENTED_EDGE('',*,*,#27999,.F.);
#37080=ORIENTED_EDGE('',*,*,#28000,.F.);
#37081=ORIENTED_EDGE('',*,*,#26419,.T.);
#37082=ORIENTED_EDGE('',*,*,#27998,.T.);
#37083=ORIENTED_EDGE('',*,*,#28001,.F.);
#37084=ORIENTED_EDGE('',*,*,#28002,.F.);
#37085=ORIENTED_EDGE('',*,*,#26420,.T.);
#37086=ORIENTED_EDGE('',*,*,#28000,.T.);
#37087=ORIENTED_EDGE('',*,*,#28003,.F.);
#37088=ORIENTED_EDGE('',*,*,#28004,.F.);
#37089=ORIENTED_EDGE('',*,*,#26421,.T.);
#37090=ORIENTED_EDGE('',*,*,#28002,.T.);
#37091=ORIENTED_EDGE('',*,*,#28005,.F.);
#37092=ORIENTED_EDGE('',*,*,#28006,.F.);
#37093=ORIENTED_EDGE('',*,*,#26422,.T.);
#37094=ORIENTED_EDGE('',*,*,#28004,.T.);
#37095=ORIENTED_EDGE('',*,*,#28007,.F.);
#37096=ORIENTED_EDGE('',*,*,#28008,.F.);
#37097=ORIENTED_EDGE('',*,*,#26423,.T.);
#37098=ORIENTED_EDGE('',*,*,#28006,.T.);
#37099=ORIENTED_EDGE('',*,*,#28009,.F.);
#37100=ORIENTED_EDGE('',*,*,#28010,.F.);
#37101=ORIENTED_EDGE('',*,*,#26424,.T.);
#37102=ORIENTED_EDGE('',*,*,#28008,.T.);
#37103=ORIENTED_EDGE('',*,*,#28011,.F.);
#37104=ORIENTED_EDGE('',*,*,#28012,.F.);
#37105=ORIENTED_EDGE('',*,*,#26425,.T.);
#37106=ORIENTED_EDGE('',*,*,#28010,.T.);
#37107=ORIENTED_EDGE('',*,*,#28013,.F.);
#37108=ORIENTED_EDGE('',*,*,#28014,.F.);
#37109=ORIENTED_EDGE('',*,*,#26426,.T.);
#37110=ORIENTED_EDGE('',*,*,#28012,.T.);
#37111=ORIENTED_EDGE('',*,*,#28015,.F.);
#37112=ORIENTED_EDGE('',*,*,#28016,.F.);
#37113=ORIENTED_EDGE('',*,*,#26427,.T.);
#37114=ORIENTED_EDGE('',*,*,#28014,.T.);
#37115=ORIENTED_EDGE('',*,*,#28017,.F.);
#37116=ORIENTED_EDGE('',*,*,#28018,.F.);
#37117=ORIENTED_EDGE('',*,*,#26428,.T.);
#37118=ORIENTED_EDGE('',*,*,#28016,.T.);
#37119=ORIENTED_EDGE('',*,*,#28019,.F.);
#37120=ORIENTED_EDGE('',*,*,#28020,.F.);
#37121=ORIENTED_EDGE('',*,*,#26429,.T.);
#37122=ORIENTED_EDGE('',*,*,#28018,.T.);
#37123=ORIENTED_EDGE('',*,*,#28021,.F.);
#37124=ORIENTED_EDGE('',*,*,#27157,.F.);
#37125=ORIENTED_EDGE('',*,*,#26430,.T.);
#37126=ORIENTED_EDGE('',*,*,#28020,.T.);
#37127=ORIENTED_EDGE('',*,*,#27102,.T.);
#37128=ORIENTED_EDGE('',*,*,#27160,.F.);
#37129=ORIENTED_EDGE('',*,*,#27519,.F.);
#37130=ORIENTED_EDGE('',*,*,#26433,.F.);
#37131=ORIENTED_EDGE('',*,*,#27158,.T.);
#37132=ORIENTED_EDGE('',*,*,#28021,.T.);
#37133=ORIENTED_EDGE('',*,*,#28019,.T.);
#37134=ORIENTED_EDGE('',*,*,#28017,.T.);
#37135=ORIENTED_EDGE('',*,*,#28015,.T.);
#37136=ORIENTED_EDGE('',*,*,#28013,.T.);
#37137=ORIENTED_EDGE('',*,*,#28011,.T.);
#37138=ORIENTED_EDGE('',*,*,#28009,.T.);
#37139=ORIENTED_EDGE('',*,*,#28007,.T.);
#37140=ORIENTED_EDGE('',*,*,#28005,.T.);
#37141=ORIENTED_EDGE('',*,*,#28003,.T.);
#37142=ORIENTED_EDGE('',*,*,#28001,.T.);
#37143=ORIENTED_EDGE('',*,*,#27999,.T.);
#37144=ORIENTED_EDGE('',*,*,#27997,.T.);
#37145=ORIENTED_EDGE('',*,*,#27002,.T.);
#37146=ORIENTED_EDGE('',*,*,#28022,.F.);
#37147=ORIENTED_EDGE('',*,*,#28023,.T.);
#37148=ORIENTED_EDGE('',*,*,#28024,.T.);
#37149=ORIENTED_EDGE('',*,*,#28025,.T.);
#37150=ORIENTED_EDGE('',*,*,#28026,.T.);
#37151=ORIENTED_EDGE('',*,*,#28027,.T.);
#37152=ORIENTED_EDGE('',*,*,#28028,.T.);
#37153=ORIENTED_EDGE('',*,*,#28029,.T.);
#37154=ORIENTED_EDGE('',*,*,#28030,.T.);
#37155=ORIENTED_EDGE('',*,*,#28031,.T.);
#37156=ORIENTED_EDGE('',*,*,#28032,.T.);
#37157=ORIENTED_EDGE('',*,*,#28033,.T.);
#37158=ORIENTED_EDGE('',*,*,#28034,.T.);
#37159=ORIENTED_EDGE('',*,*,#28035,.T.);
#37160=ORIENTED_EDGE('',*,*,#28036,.T.);
#37161=ORIENTED_EDGE('',*,*,#26399,.T.);
#37162=ORIENTED_EDGE('',*,*,#27520,.T.);
#37163=ORIENTED_EDGE('',*,*,#28036,.F.);
#37164=ORIENTED_EDGE('',*,*,#28037,.F.);
#37165=ORIENTED_EDGE('',*,*,#26366,.T.);
#37166=ORIENTED_EDGE('',*,*,#26400,.T.);
#37167=ORIENTED_EDGE('',*,*,#28035,.F.);
#37168=ORIENTED_EDGE('',*,*,#28038,.F.);
#37169=ORIENTED_EDGE('',*,*,#26367,.T.);
#37170=ORIENTED_EDGE('',*,*,#28037,.T.);
#37171=ORIENTED_EDGE('',*,*,#28034,.F.);
#37172=ORIENTED_EDGE('',*,*,#28039,.F.);
#37173=ORIENTED_EDGE('',*,*,#26368,.T.);
#37174=ORIENTED_EDGE('',*,*,#28038,.T.);
#37175=ORIENTED_EDGE('',*,*,#28033,.F.);
#37176=ORIENTED_EDGE('',*,*,#28040,.F.);
#37177=ORIENTED_EDGE('',*,*,#26369,.T.);
#37178=ORIENTED_EDGE('',*,*,#28039,.T.);
#37179=ORIENTED_EDGE('',*,*,#28032,.F.);
#37180=ORIENTED_EDGE('',*,*,#28041,.F.);
#37181=ORIENTED_EDGE('',*,*,#26370,.T.);
#37182=ORIENTED_EDGE('',*,*,#28040,.T.);
#37183=ORIENTED_EDGE('',*,*,#28031,.F.);
#37184=ORIENTED_EDGE('',*,*,#28042,.F.);
#37185=ORIENTED_EDGE('',*,*,#26371,.T.);
#37186=ORIENTED_EDGE('',*,*,#28041,.T.);
#37187=ORIENTED_EDGE('',*,*,#28030,.F.);
#37188=ORIENTED_EDGE('',*,*,#28043,.F.);
#37189=ORIENTED_EDGE('',*,*,#26372,.T.);
#37190=ORIENTED_EDGE('',*,*,#28042,.T.);
#37191=ORIENTED_EDGE('',*,*,#28029,.F.);
#37192=ORIENTED_EDGE('',*,*,#28044,.F.);
#37193=ORIENTED_EDGE('',*,*,#26373,.T.);
#37194=ORIENTED_EDGE('',*,*,#28043,.T.);
#37195=ORIENTED_EDGE('',*,*,#28028,.F.);
#37196=ORIENTED_EDGE('',*,*,#28045,.F.);
#37197=ORIENTED_EDGE('',*,*,#26374,.T.);
#37198=ORIENTED_EDGE('',*,*,#28044,.T.);
#37199=ORIENTED_EDGE('',*,*,#28027,.F.);
#37200=ORIENTED_EDGE('',*,*,#28046,.F.);
#37201=ORIENTED_EDGE('',*,*,#26375,.T.);
#37202=ORIENTED_EDGE('',*,*,#28045,.T.);
#37203=ORIENTED_EDGE('',*,*,#28026,.F.);
#37204=ORIENTED_EDGE('',*,*,#28047,.F.);
#37205=ORIENTED_EDGE('',*,*,#26376,.T.);
#37206=ORIENTED_EDGE('',*,*,#28046,.T.);
#37207=ORIENTED_EDGE('',*,*,#28025,.F.);
#37208=ORIENTED_EDGE('',*,*,#28048,.F.);
#37209=ORIENTED_EDGE('',*,*,#26377,.T.);
#37210=ORIENTED_EDGE('',*,*,#28047,.T.);
#37211=ORIENTED_EDGE('',*,*,#28024,.F.);
#37212=ORIENTED_EDGE('',*,*,#28049,.F.);
#37213=ORIENTED_EDGE('',*,*,#26378,.T.);
#37214=ORIENTED_EDGE('',*,*,#28048,.T.);
#37215=ORIENTED_EDGE('',*,*,#26793,.T.);
#37216=ORIENTED_EDGE('',*,*,#26379,.T.);
#37217=ORIENTED_EDGE('',*,*,#28049,.T.);
#37218=ORIENTED_EDGE('',*,*,#28023,.F.);
#37219=ORIENTED_EDGE('',*,*,#28050,.F.);
#37220=ORIENTED_EDGE('',*,*,#27355,.T.);
#37221=ORIENTED_EDGE('',*,*,#27313,.T.);
#37222=ORIENTED_EDGE('',*,*,#28051,.F.);
#37223=ORIENTED_EDGE('',*,*,#28052,.F.);
#37224=ORIENTED_EDGE('',*,*,#26382,.T.);
#37225=ORIENTED_EDGE('',*,*,#26998,.T.);
#37226=ORIENTED_EDGE('',*,*,#28053,.F.);
#37227=ORIENTED_EDGE('',*,*,#28054,.F.);
#37228=ORIENTED_EDGE('',*,*,#26383,.T.);
#37229=ORIENTED_EDGE('',*,*,#28052,.T.);
#37230=ORIENTED_EDGE('',*,*,#28055,.F.);
#37231=ORIENTED_EDGE('',*,*,#28056,.F.);
#37232=ORIENTED_EDGE('',*,*,#26384,.T.);
#37233=ORIENTED_EDGE('',*,*,#28054,.T.);
#37234=ORIENTED_EDGE('',*,*,#28057,.F.);
#37235=ORIENTED_EDGE('',*,*,#28058,.F.);
#37236=ORIENTED_EDGE('',*,*,#26385,.T.);
#37237=ORIENTED_EDGE('',*,*,#28056,.T.);
#37238=ORIENTED_EDGE('',*,*,#28059,.F.);
#37239=ORIENTED_EDGE('',*,*,#28060,.F.);
#37240=ORIENTED_EDGE('',*,*,#26386,.T.);
#37241=ORIENTED_EDGE('',*,*,#28058,.T.);
#37242=ORIENTED_EDGE('',*,*,#28061,.F.);
#37243=ORIENTED_EDGE('',*,*,#28062,.F.);
#37244=ORIENTED_EDGE('',*,*,#26387,.T.);
#37245=ORIENTED_EDGE('',*,*,#28060,.T.);
#37246=ORIENTED_EDGE('',*,*,#28063,.F.);
#37247=ORIENTED_EDGE('',*,*,#28064,.F.);
#37248=ORIENTED_EDGE('',*,*,#26388,.T.);
#37249=ORIENTED_EDGE('',*,*,#28062,.T.);
#37250=ORIENTED_EDGE('',*,*,#28065,.F.);
#37251=ORIENTED_EDGE('',*,*,#28066,.F.);
#37252=ORIENTED_EDGE('',*,*,#26389,.T.);
#37253=ORIENTED_EDGE('',*,*,#28064,.T.);
#37254=ORIENTED_EDGE('',*,*,#28067,.F.);
#37255=ORIENTED_EDGE('',*,*,#28068,.F.);
#37256=ORIENTED_EDGE('',*,*,#26390,.T.);
#37257=ORIENTED_EDGE('',*,*,#28066,.T.);
#37258=ORIENTED_EDGE('',*,*,#28069,.F.);
#37259=ORIENTED_EDGE('',*,*,#28070,.F.);
#37260=ORIENTED_EDGE('',*,*,#26391,.T.);
#37261=ORIENTED_EDGE('',*,*,#28068,.T.);
#37262=ORIENTED_EDGE('',*,*,#28071,.F.);
#37263=ORIENTED_EDGE('',*,*,#28072,.F.);
#37264=ORIENTED_EDGE('',*,*,#26392,.T.);
#37265=ORIENTED_EDGE('',*,*,#28070,.T.);
#37266=ORIENTED_EDGE('',*,*,#28073,.F.);
#37267=ORIENTED_EDGE('',*,*,#28074,.F.);
#37268=ORIENTED_EDGE('',*,*,#26393,.T.);
#37269=ORIENTED_EDGE('',*,*,#28072,.T.);
#37270=ORIENTED_EDGE('',*,*,#28075,.F.);
#37271=ORIENTED_EDGE('',*,*,#27161,.F.);
#37272=ORIENTED_EDGE('',*,*,#26394,.T.);
#37273=ORIENTED_EDGE('',*,*,#28074,.T.);
#37274=ORIENTED_EDGE('',*,*,#27100,.T.);
#37275=ORIENTED_EDGE('',*,*,#27164,.F.);
#37276=ORIENTED_EDGE('',*,*,#27521,.F.);
#37277=ORIENTED_EDGE('',*,*,#26397,.F.);
#37278=ORIENTED_EDGE('',*,*,#27162,.T.);
#37279=ORIENTED_EDGE('',*,*,#28075,.T.);
#37280=ORIENTED_EDGE('',*,*,#28073,.T.);
#37281=ORIENTED_EDGE('',*,*,#28071,.T.);
#37282=ORIENTED_EDGE('',*,*,#28069,.T.);
#37283=ORIENTED_EDGE('',*,*,#28067,.T.);
#37284=ORIENTED_EDGE('',*,*,#28065,.T.);
#37285=ORIENTED_EDGE('',*,*,#28063,.T.);
#37286=ORIENTED_EDGE('',*,*,#28061,.T.);
#37287=ORIENTED_EDGE('',*,*,#28059,.T.);
#37288=ORIENTED_EDGE('',*,*,#28057,.T.);
#37289=ORIENTED_EDGE('',*,*,#28055,.T.);
#37290=ORIENTED_EDGE('',*,*,#28053,.T.);
#37291=ORIENTED_EDGE('',*,*,#28051,.T.);
#37292=ORIENTED_EDGE('',*,*,#26997,.T.);
#37293=ORIENTED_EDGE('',*,*,#28076,.F.);
#37294=ORIENTED_EDGE('',*,*,#28077,.T.);
#37295=ORIENTED_EDGE('',*,*,#28078,.T.);
#37296=ORIENTED_EDGE('',*,*,#28079,.T.);
#37297=ORIENTED_EDGE('',*,*,#28080,.T.);
#37298=ORIENTED_EDGE('',*,*,#28081,.T.);
#37299=ORIENTED_EDGE('',*,*,#28082,.T.);
#37300=ORIENTED_EDGE('',*,*,#28083,.T.);
#37301=ORIENTED_EDGE('',*,*,#28084,.T.);
#37302=ORIENTED_EDGE('',*,*,#28085,.T.);
#37303=ORIENTED_EDGE('',*,*,#28086,.T.);
#37304=ORIENTED_EDGE('',*,*,#28087,.T.);
#37305=ORIENTED_EDGE('',*,*,#28088,.T.);
#37306=ORIENTED_EDGE('',*,*,#28089,.T.);
#37307=ORIENTED_EDGE('',*,*,#28090,.T.);
#37308=ORIENTED_EDGE('',*,*,#26363,.T.);
#37309=ORIENTED_EDGE('',*,*,#27522,.T.);
#37310=ORIENTED_EDGE('',*,*,#28090,.F.);
#37311=ORIENTED_EDGE('',*,*,#28091,.F.);
#37312=ORIENTED_EDGE('',*,*,#26330,.T.);
#37313=ORIENTED_EDGE('',*,*,#26364,.T.);
#37314=ORIENTED_EDGE('',*,*,#28089,.F.);
#37315=ORIENTED_EDGE('',*,*,#28092,.F.);
#37316=ORIENTED_EDGE('',*,*,#26331,.T.);
#37317=ORIENTED_EDGE('',*,*,#28091,.T.);
#37318=ORIENTED_EDGE('',*,*,#28088,.F.);
#37319=ORIENTED_EDGE('',*,*,#28093,.F.);
#37320=ORIENTED_EDGE('',*,*,#26332,.T.);
#37321=ORIENTED_EDGE('',*,*,#28092,.T.);
#37322=ORIENTED_EDGE('',*,*,#28087,.F.);
#37323=ORIENTED_EDGE('',*,*,#28094,.F.);
#37324=ORIENTED_EDGE('',*,*,#26333,.T.);
#37325=ORIENTED_EDGE('',*,*,#28093,.T.);
#37326=ORIENTED_EDGE('',*,*,#28086,.F.);
#37327=ORIENTED_EDGE('',*,*,#28095,.F.);
#37328=ORIENTED_EDGE('',*,*,#26334,.T.);
#37329=ORIENTED_EDGE('',*,*,#28094,.T.);
#37330=ORIENTED_EDGE('',*,*,#28085,.F.);
#37331=ORIENTED_EDGE('',*,*,#28096,.F.);
#37332=ORIENTED_EDGE('',*,*,#26335,.T.);
#37333=ORIENTED_EDGE('',*,*,#28095,.T.);
#37334=ORIENTED_EDGE('',*,*,#28084,.F.);
#37335=ORIENTED_EDGE('',*,*,#28097,.F.);
#37336=ORIENTED_EDGE('',*,*,#26336,.T.);
#37337=ORIENTED_EDGE('',*,*,#28096,.T.);
#37338=ORIENTED_EDGE('',*,*,#28083,.F.);
#37339=ORIENTED_EDGE('',*,*,#28098,.F.);
#37340=ORIENTED_EDGE('',*,*,#26337,.T.);
#37341=ORIENTED_EDGE('',*,*,#28097,.T.);
#37342=ORIENTED_EDGE('',*,*,#28082,.F.);
#37343=ORIENTED_EDGE('',*,*,#28099,.F.);
#37344=ORIENTED_EDGE('',*,*,#26338,.T.);
#37345=ORIENTED_EDGE('',*,*,#28098,.T.);
#37346=ORIENTED_EDGE('',*,*,#28081,.F.);
#37347=ORIENTED_EDGE('',*,*,#28100,.F.);
#37348=ORIENTED_EDGE('',*,*,#26339,.T.);
#37349=ORIENTED_EDGE('',*,*,#28099,.T.);
#37350=ORIENTED_EDGE('',*,*,#28080,.F.);
#37351=ORIENTED_EDGE('',*,*,#28101,.F.);
#37352=ORIENTED_EDGE('',*,*,#26340,.T.);
#37353=ORIENTED_EDGE('',*,*,#28100,.T.);
#37354=ORIENTED_EDGE('',*,*,#28079,.F.);
#37355=ORIENTED_EDGE('',*,*,#28102,.F.);
#37356=ORIENTED_EDGE('',*,*,#26341,.T.);
#37357=ORIENTED_EDGE('',*,*,#28101,.T.);
#37358=ORIENTED_EDGE('',*,*,#28078,.F.);
#37359=ORIENTED_EDGE('',*,*,#28103,.F.);
#37360=ORIENTED_EDGE('',*,*,#26342,.T.);
#37361=ORIENTED_EDGE('',*,*,#28102,.T.);
#37362=ORIENTED_EDGE('',*,*,#26796,.T.);
#37363=ORIENTED_EDGE('',*,*,#26343,.T.);
#37364=ORIENTED_EDGE('',*,*,#28103,.T.);
#37365=ORIENTED_EDGE('',*,*,#28077,.F.);
#37366=ORIENTED_EDGE('',*,*,#28104,.F.);
#37367=ORIENTED_EDGE('',*,*,#27357,.T.);
#37368=ORIENTED_EDGE('',*,*,#27311,.T.);
#37369=ORIENTED_EDGE('',*,*,#28105,.F.);
#37370=ORIENTED_EDGE('',*,*,#28106,.F.);
#37371=ORIENTED_EDGE('',*,*,#26346,.T.);
#37372=ORIENTED_EDGE('',*,*,#26993,.T.);
#37373=ORIENTED_EDGE('',*,*,#28107,.F.);
#37374=ORIENTED_EDGE('',*,*,#28108,.F.);
#37375=ORIENTED_EDGE('',*,*,#26347,.T.);
#37376=ORIENTED_EDGE('',*,*,#28106,.T.);
#37377=ORIENTED_EDGE('',*,*,#28109,.F.);
#37378=ORIENTED_EDGE('',*,*,#28110,.F.);
#37379=ORIENTED_EDGE('',*,*,#26348,.T.);
#37380=ORIENTED_EDGE('',*,*,#28108,.T.);
#37381=ORIENTED_EDGE('',*,*,#28111,.F.);
#37382=ORIENTED_EDGE('',*,*,#28112,.F.);
#37383=ORIENTED_EDGE('',*,*,#26349,.T.);
#37384=ORIENTED_EDGE('',*,*,#28110,.T.);
#37385=ORIENTED_EDGE('',*,*,#28113,.F.);
#37386=ORIENTED_EDGE('',*,*,#28114,.F.);
#37387=ORIENTED_EDGE('',*,*,#26350,.T.);
#37388=ORIENTED_EDGE('',*,*,#28112,.T.);
#37389=ORIENTED_EDGE('',*,*,#28115,.F.);
#37390=ORIENTED_EDGE('',*,*,#28116,.F.);
#37391=ORIENTED_EDGE('',*,*,#26351,.T.);
#37392=ORIENTED_EDGE('',*,*,#28114,.T.);
#37393=ORIENTED_EDGE('',*,*,#28117,.F.);
#37394=ORIENTED_EDGE('',*,*,#28118,.F.);
#37395=ORIENTED_EDGE('',*,*,#26352,.T.);
#37396=ORIENTED_EDGE('',*,*,#28116,.T.);
#37397=ORIENTED_EDGE('',*,*,#28119,.F.);
#37398=ORIENTED_EDGE('',*,*,#28120,.F.);
#37399=ORIENTED_EDGE('',*,*,#26353,.T.);
#37400=ORIENTED_EDGE('',*,*,#28118,.T.);
#37401=ORIENTED_EDGE('',*,*,#28121,.F.);
#37402=ORIENTED_EDGE('',*,*,#28122,.F.);
#37403=ORIENTED_EDGE('',*,*,#26354,.T.);
#37404=ORIENTED_EDGE('',*,*,#28120,.T.);
#37405=ORIENTED_EDGE('',*,*,#28123,.F.);
#37406=ORIENTED_EDGE('',*,*,#28124,.F.);
#37407=ORIENTED_EDGE('',*,*,#26355,.T.);
#37408=ORIENTED_EDGE('',*,*,#28122,.T.);
#37409=ORIENTED_EDGE('',*,*,#28125,.F.);
#37410=ORIENTED_EDGE('',*,*,#28126,.F.);
#37411=ORIENTED_EDGE('',*,*,#26356,.T.);
#37412=ORIENTED_EDGE('',*,*,#28124,.T.);
#37413=ORIENTED_EDGE('',*,*,#28127,.F.);
#37414=ORIENTED_EDGE('',*,*,#28128,.F.);
#37415=ORIENTED_EDGE('',*,*,#26357,.T.);
#37416=ORIENTED_EDGE('',*,*,#28126,.T.);
#37417=ORIENTED_EDGE('',*,*,#28129,.F.);
#37418=ORIENTED_EDGE('',*,*,#27165,.F.);
#37419=ORIENTED_EDGE('',*,*,#26358,.T.);
#37420=ORIENTED_EDGE('',*,*,#28128,.T.);
#37421=ORIENTED_EDGE('',*,*,#27098,.T.);
#37422=ORIENTED_EDGE('',*,*,#27168,.F.);
#37423=ORIENTED_EDGE('',*,*,#27523,.F.);
#37424=ORIENTED_EDGE('',*,*,#26361,.F.);
#37425=ORIENTED_EDGE('',*,*,#27166,.T.);
#37426=ORIENTED_EDGE('',*,*,#28129,.T.);
#37427=ORIENTED_EDGE('',*,*,#28127,.T.);
#37428=ORIENTED_EDGE('',*,*,#28125,.T.);
#37429=ORIENTED_EDGE('',*,*,#28123,.T.);
#37430=ORIENTED_EDGE('',*,*,#28121,.T.);
#37431=ORIENTED_EDGE('',*,*,#28119,.T.);
#37432=ORIENTED_EDGE('',*,*,#28117,.T.);
#37433=ORIENTED_EDGE('',*,*,#28115,.T.);
#37434=ORIENTED_EDGE('',*,*,#28113,.T.);
#37435=ORIENTED_EDGE('',*,*,#28111,.T.);
#37436=ORIENTED_EDGE('',*,*,#28109,.T.);
#37437=ORIENTED_EDGE('',*,*,#28107,.T.);
#37438=ORIENTED_EDGE('',*,*,#28105,.T.);
#37439=ORIENTED_EDGE('',*,*,#26992,.T.);
#37440=ORIENTED_EDGE('',*,*,#28130,.F.);
#37441=ORIENTED_EDGE('',*,*,#28131,.T.);
#37442=ORIENTED_EDGE('',*,*,#28132,.T.);
#37443=ORIENTED_EDGE('',*,*,#28133,.T.);
#37444=ORIENTED_EDGE('',*,*,#28134,.T.);
#37445=ORIENTED_EDGE('',*,*,#28135,.T.);
#37446=ORIENTED_EDGE('',*,*,#28136,.T.);
#37447=ORIENTED_EDGE('',*,*,#28137,.T.);
#37448=ORIENTED_EDGE('',*,*,#28138,.T.);
#37449=ORIENTED_EDGE('',*,*,#28139,.T.);
#37450=ORIENTED_EDGE('',*,*,#28140,.T.);
#37451=ORIENTED_EDGE('',*,*,#28141,.T.);
#37452=ORIENTED_EDGE('',*,*,#28142,.T.);
#37453=ORIENTED_EDGE('',*,*,#28143,.T.);
#37454=ORIENTED_EDGE('',*,*,#28144,.T.);
#37455=ORIENTED_EDGE('',*,*,#26327,.T.);
#37456=ORIENTED_EDGE('',*,*,#27524,.T.);
#37457=ORIENTED_EDGE('',*,*,#28144,.F.);
#37458=ORIENTED_EDGE('',*,*,#28145,.F.);
#37459=ORIENTED_EDGE('',*,*,#26294,.T.);
#37460=ORIENTED_EDGE('',*,*,#26328,.T.);
#37461=ORIENTED_EDGE('',*,*,#28143,.F.);
#37462=ORIENTED_EDGE('',*,*,#28146,.F.);
#37463=ORIENTED_EDGE('',*,*,#26295,.T.);
#37464=ORIENTED_EDGE('',*,*,#28145,.T.);
#37465=ORIENTED_EDGE('',*,*,#28142,.F.);
#37466=ORIENTED_EDGE('',*,*,#28147,.F.);
#37467=ORIENTED_EDGE('',*,*,#26296,.T.);
#37468=ORIENTED_EDGE('',*,*,#28146,.T.);
#37469=ORIENTED_EDGE('',*,*,#28141,.F.);
#37470=ORIENTED_EDGE('',*,*,#28148,.F.);
#37471=ORIENTED_EDGE('',*,*,#26297,.T.);
#37472=ORIENTED_EDGE('',*,*,#28147,.T.);
#37473=ORIENTED_EDGE('',*,*,#28140,.F.);
#37474=ORIENTED_EDGE('',*,*,#28149,.F.);
#37475=ORIENTED_EDGE('',*,*,#26298,.T.);
#37476=ORIENTED_EDGE('',*,*,#28148,.T.);
#37477=ORIENTED_EDGE('',*,*,#28139,.F.);
#37478=ORIENTED_EDGE('',*,*,#28150,.F.);
#37479=ORIENTED_EDGE('',*,*,#26299,.T.);
#37480=ORIENTED_EDGE('',*,*,#28149,.T.);
#37481=ORIENTED_EDGE('',*,*,#28138,.F.);
#37482=ORIENTED_EDGE('',*,*,#28151,.F.);
#37483=ORIENTED_EDGE('',*,*,#26300,.T.);
#37484=ORIENTED_EDGE('',*,*,#28150,.T.);
#37485=ORIENTED_EDGE('',*,*,#28137,.F.);
#37486=ORIENTED_EDGE('',*,*,#28152,.F.);
#37487=ORIENTED_EDGE('',*,*,#26301,.T.);
#37488=ORIENTED_EDGE('',*,*,#28151,.T.);
#37489=ORIENTED_EDGE('',*,*,#28136,.F.);
#37490=ORIENTED_EDGE('',*,*,#28153,.F.);
#37491=ORIENTED_EDGE('',*,*,#26302,.T.);
#37492=ORIENTED_EDGE('',*,*,#28152,.T.);
#37493=ORIENTED_EDGE('',*,*,#28135,.F.);
#37494=ORIENTED_EDGE('',*,*,#28154,.F.);
#37495=ORIENTED_EDGE('',*,*,#26303,.T.);
#37496=ORIENTED_EDGE('',*,*,#28153,.T.);
#37497=ORIENTED_EDGE('',*,*,#28134,.F.);
#37498=ORIENTED_EDGE('',*,*,#28155,.F.);
#37499=ORIENTED_EDGE('',*,*,#26304,.T.);
#37500=ORIENTED_EDGE('',*,*,#28154,.T.);
#37501=ORIENTED_EDGE('',*,*,#28133,.F.);
#37502=ORIENTED_EDGE('',*,*,#28156,.F.);
#37503=ORIENTED_EDGE('',*,*,#26305,.T.);
#37504=ORIENTED_EDGE('',*,*,#28155,.T.);
#37505=ORIENTED_EDGE('',*,*,#28132,.F.);
#37506=ORIENTED_EDGE('',*,*,#28157,.F.);
#37507=ORIENTED_EDGE('',*,*,#26306,.T.);
#37508=ORIENTED_EDGE('',*,*,#28156,.T.);
#37509=ORIENTED_EDGE('',*,*,#26799,.T.);
#37510=ORIENTED_EDGE('',*,*,#26307,.T.);
#37511=ORIENTED_EDGE('',*,*,#28157,.T.);
#37512=ORIENTED_EDGE('',*,*,#28131,.F.);
#37513=ORIENTED_EDGE('',*,*,#28158,.F.);
#37514=ORIENTED_EDGE('',*,*,#27359,.T.);
#37515=ORIENTED_EDGE('',*,*,#27309,.T.);
#37516=ORIENTED_EDGE('',*,*,#28159,.F.);
#37517=ORIENTED_EDGE('',*,*,#28160,.F.);
#37518=ORIENTED_EDGE('',*,*,#26310,.T.);
#37519=ORIENTED_EDGE('',*,*,#26988,.T.);
#37520=ORIENTED_EDGE('',*,*,#28161,.F.);
#37521=ORIENTED_EDGE('',*,*,#28162,.F.);
#37522=ORIENTED_EDGE('',*,*,#26311,.T.);
#37523=ORIENTED_EDGE('',*,*,#28160,.T.);
#37524=ORIENTED_EDGE('',*,*,#28163,.F.);
#37525=ORIENTED_EDGE('',*,*,#28164,.F.);
#37526=ORIENTED_EDGE('',*,*,#26312,.T.);
#37527=ORIENTED_EDGE('',*,*,#28162,.T.);
#37528=ORIENTED_EDGE('',*,*,#28165,.F.);
#37529=ORIENTED_EDGE('',*,*,#28166,.F.);
#37530=ORIENTED_EDGE('',*,*,#26313,.T.);
#37531=ORIENTED_EDGE('',*,*,#28164,.T.);
#37532=ORIENTED_EDGE('',*,*,#28167,.F.);
#37533=ORIENTED_EDGE('',*,*,#28168,.F.);
#37534=ORIENTED_EDGE('',*,*,#26314,.T.);
#37535=ORIENTED_EDGE('',*,*,#28166,.T.);
#37536=ORIENTED_EDGE('',*,*,#28169,.F.);
#37537=ORIENTED_EDGE('',*,*,#28170,.F.);
#37538=ORIENTED_EDGE('',*,*,#26315,.T.);
#37539=ORIENTED_EDGE('',*,*,#28168,.T.);
#37540=ORIENTED_EDGE('',*,*,#28171,.F.);
#37541=ORIENTED_EDGE('',*,*,#28172,.F.);
#37542=ORIENTED_EDGE('',*,*,#26316,.T.);
#37543=ORIENTED_EDGE('',*,*,#28170,.T.);
#37544=ORIENTED_EDGE('',*,*,#28173,.F.);
#37545=ORIENTED_EDGE('',*,*,#28174,.F.);
#37546=ORIENTED_EDGE('',*,*,#26317,.T.);
#37547=ORIENTED_EDGE('',*,*,#28172,.T.);
#37548=ORIENTED_EDGE('',*,*,#28175,.F.);
#37549=ORIENTED_EDGE('',*,*,#28176,.F.);
#37550=ORIENTED_EDGE('',*,*,#26318,.T.);
#37551=ORIENTED_EDGE('',*,*,#28174,.T.);
#37552=ORIENTED_EDGE('',*,*,#28177,.F.);
#37553=ORIENTED_EDGE('',*,*,#28178,.F.);
#37554=ORIENTED_EDGE('',*,*,#26319,.T.);
#37555=ORIENTED_EDGE('',*,*,#28176,.T.);
#37556=ORIENTED_EDGE('',*,*,#28179,.F.);
#37557=ORIENTED_EDGE('',*,*,#28180,.F.);
#37558=ORIENTED_EDGE('',*,*,#26320,.T.);
#37559=ORIENTED_EDGE('',*,*,#28178,.T.);
#37560=ORIENTED_EDGE('',*,*,#28181,.F.);
#37561=ORIENTED_EDGE('',*,*,#28182,.F.);
#37562=ORIENTED_EDGE('',*,*,#26321,.T.);
#37563=ORIENTED_EDGE('',*,*,#28180,.T.);
#37564=ORIENTED_EDGE('',*,*,#28183,.F.);
#37565=ORIENTED_EDGE('',*,*,#27169,.F.);
#37566=ORIENTED_EDGE('',*,*,#26322,.T.);
#37567=ORIENTED_EDGE('',*,*,#28182,.T.);
#37568=ORIENTED_EDGE('',*,*,#27096,.T.);
#37569=ORIENTED_EDGE('',*,*,#27172,.F.);
#37570=ORIENTED_EDGE('',*,*,#27525,.F.);
#37571=ORIENTED_EDGE('',*,*,#26325,.F.);
#37572=ORIENTED_EDGE('',*,*,#27170,.T.);
#37573=ORIENTED_EDGE('',*,*,#28183,.T.);
#37574=ORIENTED_EDGE('',*,*,#28181,.T.);
#37575=ORIENTED_EDGE('',*,*,#28179,.T.);
#37576=ORIENTED_EDGE('',*,*,#28177,.T.);
#37577=ORIENTED_EDGE('',*,*,#28175,.T.);
#37578=ORIENTED_EDGE('',*,*,#28173,.T.);
#37579=ORIENTED_EDGE('',*,*,#28171,.T.);
#37580=ORIENTED_EDGE('',*,*,#28169,.T.);
#37581=ORIENTED_EDGE('',*,*,#28167,.T.);
#37582=ORIENTED_EDGE('',*,*,#28165,.T.);
#37583=ORIENTED_EDGE('',*,*,#28163,.T.);
#37584=ORIENTED_EDGE('',*,*,#28161,.T.);
#37585=ORIENTED_EDGE('',*,*,#28159,.T.);
#37586=ORIENTED_EDGE('',*,*,#26987,.T.);
#37587=ORIENTED_EDGE('',*,*,#28184,.F.);
#37588=ORIENTED_EDGE('',*,*,#28185,.T.);
#37589=ORIENTED_EDGE('',*,*,#28186,.T.);
#37590=ORIENTED_EDGE('',*,*,#28187,.T.);
#37591=ORIENTED_EDGE('',*,*,#28188,.T.);
#37592=ORIENTED_EDGE('',*,*,#28189,.T.);
#37593=ORIENTED_EDGE('',*,*,#28190,.T.);
#37594=ORIENTED_EDGE('',*,*,#28191,.T.);
#37595=ORIENTED_EDGE('',*,*,#28192,.T.);
#37596=ORIENTED_EDGE('',*,*,#28193,.T.);
#37597=ORIENTED_EDGE('',*,*,#28194,.T.);
#37598=ORIENTED_EDGE('',*,*,#28195,.T.);
#37599=ORIENTED_EDGE('',*,*,#28196,.T.);
#37600=ORIENTED_EDGE('',*,*,#28197,.T.);
#37601=ORIENTED_EDGE('',*,*,#28198,.T.);
#37602=ORIENTED_EDGE('',*,*,#26291,.T.);
#37603=ORIENTED_EDGE('',*,*,#27526,.T.);
#37604=ORIENTED_EDGE('',*,*,#28198,.F.);
#37605=ORIENTED_EDGE('',*,*,#28199,.F.);
#37606=ORIENTED_EDGE('',*,*,#26258,.T.);
#37607=ORIENTED_EDGE('',*,*,#26292,.T.);
#37608=ORIENTED_EDGE('',*,*,#28197,.F.);
#37609=ORIENTED_EDGE('',*,*,#28200,.F.);
#37610=ORIENTED_EDGE('',*,*,#26259,.T.);
#37611=ORIENTED_EDGE('',*,*,#28199,.T.);
#37612=ORIENTED_EDGE('',*,*,#28196,.F.);
#37613=ORIENTED_EDGE('',*,*,#28201,.F.);
#37614=ORIENTED_EDGE('',*,*,#26260,.T.);
#37615=ORIENTED_EDGE('',*,*,#28200,.T.);
#37616=ORIENTED_EDGE('',*,*,#28195,.F.);
#37617=ORIENTED_EDGE('',*,*,#28202,.F.);
#37618=ORIENTED_EDGE('',*,*,#26261,.T.);
#37619=ORIENTED_EDGE('',*,*,#28201,.T.);
#37620=ORIENTED_EDGE('',*,*,#28194,.F.);
#37621=ORIENTED_EDGE('',*,*,#28203,.F.);
#37622=ORIENTED_EDGE('',*,*,#26262,.T.);
#37623=ORIENTED_EDGE('',*,*,#28202,.T.);
#37624=ORIENTED_EDGE('',*,*,#28193,.F.);
#37625=ORIENTED_EDGE('',*,*,#28204,.F.);
#37626=ORIENTED_EDGE('',*,*,#26263,.T.);
#37627=ORIENTED_EDGE('',*,*,#28203,.T.);
#37628=ORIENTED_EDGE('',*,*,#28192,.F.);
#37629=ORIENTED_EDGE('',*,*,#28205,.F.);
#37630=ORIENTED_EDGE('',*,*,#26264,.T.);
#37631=ORIENTED_EDGE('',*,*,#28204,.T.);
#37632=ORIENTED_EDGE('',*,*,#28191,.F.);
#37633=ORIENTED_EDGE('',*,*,#28206,.F.);
#37634=ORIENTED_EDGE('',*,*,#26265,.T.);
#37635=ORIENTED_EDGE('',*,*,#28205,.T.);
#37636=ORIENTED_EDGE('',*,*,#28190,.F.);
#37637=ORIENTED_EDGE('',*,*,#28207,.F.);
#37638=ORIENTED_EDGE('',*,*,#26266,.T.);
#37639=ORIENTED_EDGE('',*,*,#28206,.T.);
#37640=ORIENTED_EDGE('',*,*,#28189,.F.);
#37641=ORIENTED_EDGE('',*,*,#28208,.F.);
#37642=ORIENTED_EDGE('',*,*,#26267,.T.);
#37643=ORIENTED_EDGE('',*,*,#28207,.T.);
#37644=ORIENTED_EDGE('',*,*,#28188,.F.);
#37645=ORIENTED_EDGE('',*,*,#28209,.F.);
#37646=ORIENTED_EDGE('',*,*,#26268,.T.);
#37647=ORIENTED_EDGE('',*,*,#28208,.T.);
#37648=ORIENTED_EDGE('',*,*,#28187,.F.);
#37649=ORIENTED_EDGE('',*,*,#28210,.F.);
#37650=ORIENTED_EDGE('',*,*,#26269,.T.);
#37651=ORIENTED_EDGE('',*,*,#28209,.T.);
#37652=ORIENTED_EDGE('',*,*,#28186,.F.);
#37653=ORIENTED_EDGE('',*,*,#28211,.F.);
#37654=ORIENTED_EDGE('',*,*,#26270,.T.);
#37655=ORIENTED_EDGE('',*,*,#28210,.T.);
#37656=ORIENTED_EDGE('',*,*,#26802,.T.);
#37657=ORIENTED_EDGE('',*,*,#26271,.T.);
#37658=ORIENTED_EDGE('',*,*,#28211,.T.);
#37659=ORIENTED_EDGE('',*,*,#28185,.F.);
#37660=ORIENTED_EDGE('',*,*,#28212,.F.);
#37661=ORIENTED_EDGE('',*,*,#27361,.T.);
#37662=ORIENTED_EDGE('',*,*,#27307,.T.);
#37663=ORIENTED_EDGE('',*,*,#28213,.F.);
#37664=ORIENTED_EDGE('',*,*,#28214,.F.);
#37665=ORIENTED_EDGE('',*,*,#26274,.T.);
#37666=ORIENTED_EDGE('',*,*,#26983,.T.);
#37667=ORIENTED_EDGE('',*,*,#28215,.F.);
#37668=ORIENTED_EDGE('',*,*,#28216,.F.);
#37669=ORIENTED_EDGE('',*,*,#26275,.T.);
#37670=ORIENTED_EDGE('',*,*,#28214,.T.);
#37671=ORIENTED_EDGE('',*,*,#28217,.F.);
#37672=ORIENTED_EDGE('',*,*,#28218,.F.);
#37673=ORIENTED_EDGE('',*,*,#26276,.T.);
#37674=ORIENTED_EDGE('',*,*,#28216,.T.);
#37675=ORIENTED_EDGE('',*,*,#28219,.F.);
#37676=ORIENTED_EDGE('',*,*,#28220,.F.);
#37677=ORIENTED_EDGE('',*,*,#26277,.T.);
#37678=ORIENTED_EDGE('',*,*,#28218,.T.);
#37679=ORIENTED_EDGE('',*,*,#28221,.F.);
#37680=ORIENTED_EDGE('',*,*,#28222,.F.);
#37681=ORIENTED_EDGE('',*,*,#26278,.T.);
#37682=ORIENTED_EDGE('',*,*,#28220,.T.);
#37683=ORIENTED_EDGE('',*,*,#28223,.F.);
#37684=ORIENTED_EDGE('',*,*,#28224,.F.);
#37685=ORIENTED_EDGE('',*,*,#26279,.T.);
#37686=ORIENTED_EDGE('',*,*,#28222,.T.);
#37687=ORIENTED_EDGE('',*,*,#28225,.F.);
#37688=ORIENTED_EDGE('',*,*,#28226,.F.);
#37689=ORIENTED_EDGE('',*,*,#26280,.T.);
#37690=ORIENTED_EDGE('',*,*,#28224,.T.);
#37691=ORIENTED_EDGE('',*,*,#28227,.F.);
#37692=ORIENTED_EDGE('',*,*,#28228,.F.);
#37693=ORIENTED_EDGE('',*,*,#26281,.T.);
#37694=ORIENTED_EDGE('',*,*,#28226,.T.);
#37695=ORIENTED_EDGE('',*,*,#28229,.F.);
#37696=ORIENTED_EDGE('',*,*,#28230,.F.);
#37697=ORIENTED_EDGE('',*,*,#26282,.T.);
#37698=ORIENTED_EDGE('',*,*,#28228,.T.);
#37699=ORIENTED_EDGE('',*,*,#28231,.F.);
#37700=ORIENTED_EDGE('',*,*,#28232,.F.);
#37701=ORIENTED_EDGE('',*,*,#26283,.T.);
#37702=ORIENTED_EDGE('',*,*,#28230,.T.);
#37703=ORIENTED_EDGE('',*,*,#28233,.F.);
#37704=ORIENTED_EDGE('',*,*,#28234,.F.);
#37705=ORIENTED_EDGE('',*,*,#26284,.T.);
#37706=ORIENTED_EDGE('',*,*,#28232,.T.);
#37707=ORIENTED_EDGE('',*,*,#28235,.F.);
#37708=ORIENTED_EDGE('',*,*,#28236,.F.);
#37709=ORIENTED_EDGE('',*,*,#26285,.T.);
#37710=ORIENTED_EDGE('',*,*,#28234,.T.);
#37711=ORIENTED_EDGE('',*,*,#28237,.F.);
#37712=ORIENTED_EDGE('',*,*,#27173,.F.);
#37713=ORIENTED_EDGE('',*,*,#26286,.T.);
#37714=ORIENTED_EDGE('',*,*,#28236,.T.);
#37715=ORIENTED_EDGE('',*,*,#27094,.T.);
#37716=ORIENTED_EDGE('',*,*,#27176,.F.);
#37717=ORIENTED_EDGE('',*,*,#27527,.F.);
#37718=ORIENTED_EDGE('',*,*,#26289,.F.);
#37719=ORIENTED_EDGE('',*,*,#27174,.T.);
#37720=ORIENTED_EDGE('',*,*,#28237,.T.);
#37721=ORIENTED_EDGE('',*,*,#28235,.T.);
#37722=ORIENTED_EDGE('',*,*,#28233,.T.);
#37723=ORIENTED_EDGE('',*,*,#28231,.T.);
#37724=ORIENTED_EDGE('',*,*,#28229,.T.);
#37725=ORIENTED_EDGE('',*,*,#28227,.T.);
#37726=ORIENTED_EDGE('',*,*,#28225,.T.);
#37727=ORIENTED_EDGE('',*,*,#28223,.T.);
#37728=ORIENTED_EDGE('',*,*,#28221,.T.);
#37729=ORIENTED_EDGE('',*,*,#28219,.T.);
#37730=ORIENTED_EDGE('',*,*,#28217,.T.);
#37731=ORIENTED_EDGE('',*,*,#28215,.T.);
#37732=ORIENTED_EDGE('',*,*,#28213,.T.);
#37733=ORIENTED_EDGE('',*,*,#26982,.T.);
#37734=ORIENTED_EDGE('',*,*,#28238,.F.);
#37735=ORIENTED_EDGE('',*,*,#28239,.T.);
#37736=ORIENTED_EDGE('',*,*,#28240,.T.);
#37737=ORIENTED_EDGE('',*,*,#28241,.T.);
#37738=ORIENTED_EDGE('',*,*,#28242,.T.);
#37739=ORIENTED_EDGE('',*,*,#28243,.T.);
#37740=ORIENTED_EDGE('',*,*,#28244,.T.);
#37741=ORIENTED_EDGE('',*,*,#28245,.T.);
#37742=ORIENTED_EDGE('',*,*,#28246,.T.);
#37743=ORIENTED_EDGE('',*,*,#28247,.T.);
#37744=ORIENTED_EDGE('',*,*,#28248,.T.);
#37745=ORIENTED_EDGE('',*,*,#28249,.T.);
#37746=ORIENTED_EDGE('',*,*,#28250,.T.);
#37747=ORIENTED_EDGE('',*,*,#28251,.T.);
#37748=ORIENTED_EDGE('',*,*,#28252,.T.);
#37749=ORIENTED_EDGE('',*,*,#26255,.T.);
#37750=ORIENTED_EDGE('',*,*,#27528,.T.);
#37751=ORIENTED_EDGE('',*,*,#28252,.F.);
#37752=ORIENTED_EDGE('',*,*,#28253,.F.);
#37753=ORIENTED_EDGE('',*,*,#26222,.T.);
#37754=ORIENTED_EDGE('',*,*,#26256,.T.);
#37755=ORIENTED_EDGE('',*,*,#28251,.F.);
#37756=ORIENTED_EDGE('',*,*,#28254,.F.);
#37757=ORIENTED_EDGE('',*,*,#26223,.T.);
#37758=ORIENTED_EDGE('',*,*,#28253,.T.);
#37759=ORIENTED_EDGE('',*,*,#28250,.F.);
#37760=ORIENTED_EDGE('',*,*,#28255,.F.);
#37761=ORIENTED_EDGE('',*,*,#26224,.T.);
#37762=ORIENTED_EDGE('',*,*,#28254,.T.);
#37763=ORIENTED_EDGE('',*,*,#28249,.F.);
#37764=ORIENTED_EDGE('',*,*,#28256,.F.);
#37765=ORIENTED_EDGE('',*,*,#26225,.T.);
#37766=ORIENTED_EDGE('',*,*,#28255,.T.);
#37767=ORIENTED_EDGE('',*,*,#28248,.F.);
#37768=ORIENTED_EDGE('',*,*,#28257,.F.);
#37769=ORIENTED_EDGE('',*,*,#26226,.T.);
#37770=ORIENTED_EDGE('',*,*,#28256,.T.);
#37771=ORIENTED_EDGE('',*,*,#28247,.F.);
#37772=ORIENTED_EDGE('',*,*,#28258,.F.);
#37773=ORIENTED_EDGE('',*,*,#26227,.T.);
#37774=ORIENTED_EDGE('',*,*,#28257,.T.);
#37775=ORIENTED_EDGE('',*,*,#28246,.F.);
#37776=ORIENTED_EDGE('',*,*,#28259,.F.);
#37777=ORIENTED_EDGE('',*,*,#26228,.T.);
#37778=ORIENTED_EDGE('',*,*,#28258,.T.);
#37779=ORIENTED_EDGE('',*,*,#28245,.F.);
#37780=ORIENTED_EDGE('',*,*,#28260,.F.);
#37781=ORIENTED_EDGE('',*,*,#26229,.T.);
#37782=ORIENTED_EDGE('',*,*,#28259,.T.);
#37783=ORIENTED_EDGE('',*,*,#28244,.F.);
#37784=ORIENTED_EDGE('',*,*,#28261,.F.);
#37785=ORIENTED_EDGE('',*,*,#26230,.T.);
#37786=ORIENTED_EDGE('',*,*,#28260,.T.);
#37787=ORIENTED_EDGE('',*,*,#28243,.F.);
#37788=ORIENTED_EDGE('',*,*,#28262,.F.);
#37789=ORIENTED_EDGE('',*,*,#26231,.T.);
#37790=ORIENTED_EDGE('',*,*,#28261,.T.);
#37791=ORIENTED_EDGE('',*,*,#28242,.F.);
#37792=ORIENTED_EDGE('',*,*,#28263,.F.);
#37793=ORIENTED_EDGE('',*,*,#26232,.T.);
#37794=ORIENTED_EDGE('',*,*,#28262,.T.);
#37795=ORIENTED_EDGE('',*,*,#28241,.F.);
#37796=ORIENTED_EDGE('',*,*,#28264,.F.);
#37797=ORIENTED_EDGE('',*,*,#26233,.T.);
#37798=ORIENTED_EDGE('',*,*,#28263,.T.);
#37799=ORIENTED_EDGE('',*,*,#28240,.F.);
#37800=ORIENTED_EDGE('',*,*,#28265,.F.);
#37801=ORIENTED_EDGE('',*,*,#26234,.T.);
#37802=ORIENTED_EDGE('',*,*,#28264,.T.);
#37803=ORIENTED_EDGE('',*,*,#26805,.T.);
#37804=ORIENTED_EDGE('',*,*,#26235,.T.);
#37805=ORIENTED_EDGE('',*,*,#28265,.T.);
#37806=ORIENTED_EDGE('',*,*,#28239,.F.);
#37807=ORIENTED_EDGE('',*,*,#28266,.F.);
#37808=ORIENTED_EDGE('',*,*,#27363,.T.);
#37809=ORIENTED_EDGE('',*,*,#27305,.T.);
#37810=ORIENTED_EDGE('',*,*,#28267,.F.);
#37811=ORIENTED_EDGE('',*,*,#28268,.F.);
#37812=ORIENTED_EDGE('',*,*,#26238,.T.);
#37813=ORIENTED_EDGE('',*,*,#26978,.T.);
#37814=ORIENTED_EDGE('',*,*,#28269,.F.);
#37815=ORIENTED_EDGE('',*,*,#28270,.F.);
#37816=ORIENTED_EDGE('',*,*,#26239,.T.);
#37817=ORIENTED_EDGE('',*,*,#28268,.T.);
#37818=ORIENTED_EDGE('',*,*,#28271,.F.);
#37819=ORIENTED_EDGE('',*,*,#28272,.F.);
#37820=ORIENTED_EDGE('',*,*,#26240,.T.);
#37821=ORIENTED_EDGE('',*,*,#28270,.T.);
#37822=ORIENTED_EDGE('',*,*,#28273,.F.);
#37823=ORIENTED_EDGE('',*,*,#28274,.F.);
#37824=ORIENTED_EDGE('',*,*,#26241,.T.);
#37825=ORIENTED_EDGE('',*,*,#28272,.T.);
#37826=ORIENTED_EDGE('',*,*,#28275,.F.);
#37827=ORIENTED_EDGE('',*,*,#28276,.F.);
#37828=ORIENTED_EDGE('',*,*,#26242,.T.);
#37829=ORIENTED_EDGE('',*,*,#28274,.T.);
#37830=ORIENTED_EDGE('',*,*,#28277,.F.);
#37831=ORIENTED_EDGE('',*,*,#28278,.F.);
#37832=ORIENTED_EDGE('',*,*,#26243,.T.);
#37833=ORIENTED_EDGE('',*,*,#28276,.T.);
#37834=ORIENTED_EDGE('',*,*,#28279,.F.);
#37835=ORIENTED_EDGE('',*,*,#28280,.F.);
#37836=ORIENTED_EDGE('',*,*,#26244,.T.);
#37837=ORIENTED_EDGE('',*,*,#28278,.T.);
#37838=ORIENTED_EDGE('',*,*,#28281,.F.);
#37839=ORIENTED_EDGE('',*,*,#28282,.F.);
#37840=ORIENTED_EDGE('',*,*,#26245,.T.);
#37841=ORIENTED_EDGE('',*,*,#28280,.T.);
#37842=ORIENTED_EDGE('',*,*,#28283,.F.);
#37843=ORIENTED_EDGE('',*,*,#28284,.F.);
#37844=ORIENTED_EDGE('',*,*,#26246,.T.);
#37845=ORIENTED_EDGE('',*,*,#28282,.T.);
#37846=ORIENTED_EDGE('',*,*,#28285,.F.);
#37847=ORIENTED_EDGE('',*,*,#28286,.F.);
#37848=ORIENTED_EDGE('',*,*,#26247,.T.);
#37849=ORIENTED_EDGE('',*,*,#28284,.T.);
#37850=ORIENTED_EDGE('',*,*,#28287,.F.);
#37851=ORIENTED_EDGE('',*,*,#28288,.F.);
#37852=ORIENTED_EDGE('',*,*,#26248,.T.);
#37853=ORIENTED_EDGE('',*,*,#28286,.T.);
#37854=ORIENTED_EDGE('',*,*,#28289,.F.);
#37855=ORIENTED_EDGE('',*,*,#28290,.F.);
#37856=ORIENTED_EDGE('',*,*,#26249,.T.);
#37857=ORIENTED_EDGE('',*,*,#28288,.T.);
#37858=ORIENTED_EDGE('',*,*,#28291,.F.);
#37859=ORIENTED_EDGE('',*,*,#27177,.F.);
#37860=ORIENTED_EDGE('',*,*,#26250,.T.);
#37861=ORIENTED_EDGE('',*,*,#28290,.T.);
#37862=ORIENTED_EDGE('',*,*,#27092,.T.);
#37863=ORIENTED_EDGE('',*,*,#27180,.F.);
#37864=ORIENTED_EDGE('',*,*,#27529,.F.);
#37865=ORIENTED_EDGE('',*,*,#26253,.F.);
#37866=ORIENTED_EDGE('',*,*,#27178,.T.);
#37867=ORIENTED_EDGE('',*,*,#28291,.T.);
#37868=ORIENTED_EDGE('',*,*,#28289,.T.);
#37869=ORIENTED_EDGE('',*,*,#28287,.T.);
#37870=ORIENTED_EDGE('',*,*,#28285,.T.);
#37871=ORIENTED_EDGE('',*,*,#28283,.T.);
#37872=ORIENTED_EDGE('',*,*,#28281,.T.);
#37873=ORIENTED_EDGE('',*,*,#28279,.T.);
#37874=ORIENTED_EDGE('',*,*,#28277,.T.);
#37875=ORIENTED_EDGE('',*,*,#28275,.T.);
#37876=ORIENTED_EDGE('',*,*,#28273,.T.);
#37877=ORIENTED_EDGE('',*,*,#28271,.T.);
#37878=ORIENTED_EDGE('',*,*,#28269,.T.);
#37879=ORIENTED_EDGE('',*,*,#28267,.T.);
#37880=ORIENTED_EDGE('',*,*,#26977,.T.);
#37881=ORIENTED_EDGE('',*,*,#28292,.F.);
#37882=ORIENTED_EDGE('',*,*,#28293,.T.);
#37883=ORIENTED_EDGE('',*,*,#28294,.T.);
#37884=ORIENTED_EDGE('',*,*,#28295,.T.);
#37885=ORIENTED_EDGE('',*,*,#28296,.T.);
#37886=ORIENTED_EDGE('',*,*,#28297,.T.);
#37887=ORIENTED_EDGE('',*,*,#28298,.T.);
#37888=ORIENTED_EDGE('',*,*,#28299,.T.);
#37889=ORIENTED_EDGE('',*,*,#28300,.T.);
#37890=ORIENTED_EDGE('',*,*,#28301,.T.);
#37891=ORIENTED_EDGE('',*,*,#28302,.T.);
#37892=ORIENTED_EDGE('',*,*,#28303,.T.);
#37893=ORIENTED_EDGE('',*,*,#28304,.T.);
#37894=ORIENTED_EDGE('',*,*,#28305,.T.);
#37895=ORIENTED_EDGE('',*,*,#28306,.T.);
#37896=ORIENTED_EDGE('',*,*,#26219,.T.);
#37897=ORIENTED_EDGE('',*,*,#27530,.T.);
#37898=ORIENTED_EDGE('',*,*,#28306,.F.);
#37899=ORIENTED_EDGE('',*,*,#28307,.F.);
#37900=ORIENTED_EDGE('',*,*,#26186,.T.);
#37901=ORIENTED_EDGE('',*,*,#26220,.T.);
#37902=ORIENTED_EDGE('',*,*,#28305,.F.);
#37903=ORIENTED_EDGE('',*,*,#28308,.F.);
#37904=ORIENTED_EDGE('',*,*,#26187,.T.);
#37905=ORIENTED_EDGE('',*,*,#28307,.T.);
#37906=ORIENTED_EDGE('',*,*,#28304,.F.);
#37907=ORIENTED_EDGE('',*,*,#28309,.F.);
#37908=ORIENTED_EDGE('',*,*,#26188,.T.);
#37909=ORIENTED_EDGE('',*,*,#28308,.T.);
#37910=ORIENTED_EDGE('',*,*,#28303,.F.);
#37911=ORIENTED_EDGE('',*,*,#28310,.F.);
#37912=ORIENTED_EDGE('',*,*,#26189,.T.);
#37913=ORIENTED_EDGE('',*,*,#28309,.T.);
#37914=ORIENTED_EDGE('',*,*,#28302,.F.);
#37915=ORIENTED_EDGE('',*,*,#28311,.F.);
#37916=ORIENTED_EDGE('',*,*,#26190,.T.);
#37917=ORIENTED_EDGE('',*,*,#28310,.T.);
#37918=ORIENTED_EDGE('',*,*,#28301,.F.);
#37919=ORIENTED_EDGE('',*,*,#28312,.F.);
#37920=ORIENTED_EDGE('',*,*,#26191,.T.);
#37921=ORIENTED_EDGE('',*,*,#28311,.T.);
#37922=ORIENTED_EDGE('',*,*,#28300,.F.);
#37923=ORIENTED_EDGE('',*,*,#28313,.F.);
#37924=ORIENTED_EDGE('',*,*,#26192,.T.);
#37925=ORIENTED_EDGE('',*,*,#28312,.T.);
#37926=ORIENTED_EDGE('',*,*,#28299,.F.);
#37927=ORIENTED_EDGE('',*,*,#28314,.F.);
#37928=ORIENTED_EDGE('',*,*,#26193,.T.);
#37929=ORIENTED_EDGE('',*,*,#28313,.T.);
#37930=ORIENTED_EDGE('',*,*,#28298,.F.);
#37931=ORIENTED_EDGE('',*,*,#28315,.F.);
#37932=ORIENTED_EDGE('',*,*,#26194,.T.);
#37933=ORIENTED_EDGE('',*,*,#28314,.T.);
#37934=ORIENTED_EDGE('',*,*,#28297,.F.);
#37935=ORIENTED_EDGE('',*,*,#28316,.F.);
#37936=ORIENTED_EDGE('',*,*,#26195,.T.);
#37937=ORIENTED_EDGE('',*,*,#28315,.T.);
#37938=ORIENTED_EDGE('',*,*,#28296,.F.);
#37939=ORIENTED_EDGE('',*,*,#28317,.F.);
#37940=ORIENTED_EDGE('',*,*,#26196,.T.);
#37941=ORIENTED_EDGE('',*,*,#28316,.T.);
#37942=ORIENTED_EDGE('',*,*,#28295,.F.);
#37943=ORIENTED_EDGE('',*,*,#28318,.F.);
#37944=ORIENTED_EDGE('',*,*,#26197,.T.);
#37945=ORIENTED_EDGE('',*,*,#28317,.T.);
#37946=ORIENTED_EDGE('',*,*,#28294,.F.);
#37947=ORIENTED_EDGE('',*,*,#28319,.F.);
#37948=ORIENTED_EDGE('',*,*,#26198,.T.);
#37949=ORIENTED_EDGE('',*,*,#28318,.T.);
#37950=ORIENTED_EDGE('',*,*,#26808,.T.);
#37951=ORIENTED_EDGE('',*,*,#26199,.T.);
#37952=ORIENTED_EDGE('',*,*,#28319,.T.);
#37953=ORIENTED_EDGE('',*,*,#28293,.F.);
#37954=ORIENTED_EDGE('',*,*,#28320,.F.);
#37955=ORIENTED_EDGE('',*,*,#27365,.T.);
#37956=ORIENTED_EDGE('',*,*,#27303,.T.);
#37957=ORIENTED_EDGE('',*,*,#28321,.F.);
#37958=ORIENTED_EDGE('',*,*,#28322,.F.);
#37959=ORIENTED_EDGE('',*,*,#26202,.T.);
#37960=ORIENTED_EDGE('',*,*,#26973,.T.);
#37961=ORIENTED_EDGE('',*,*,#28323,.F.);
#37962=ORIENTED_EDGE('',*,*,#28324,.F.);
#37963=ORIENTED_EDGE('',*,*,#26203,.T.);
#37964=ORIENTED_EDGE('',*,*,#28322,.T.);
#37965=ORIENTED_EDGE('',*,*,#28325,.F.);
#37966=ORIENTED_EDGE('',*,*,#28326,.F.);
#37967=ORIENTED_EDGE('',*,*,#26204,.T.);
#37968=ORIENTED_EDGE('',*,*,#28324,.T.);
#37969=ORIENTED_EDGE('',*,*,#28327,.F.);
#37970=ORIENTED_EDGE('',*,*,#28328,.F.);
#37971=ORIENTED_EDGE('',*,*,#26205,.T.);
#37972=ORIENTED_EDGE('',*,*,#28326,.T.);
#37973=ORIENTED_EDGE('',*,*,#28329,.F.);
#37974=ORIENTED_EDGE('',*,*,#28330,.F.);
#37975=ORIENTED_EDGE('',*,*,#26206,.T.);
#37976=ORIENTED_EDGE('',*,*,#28328,.T.);
#37977=ORIENTED_EDGE('',*,*,#28331,.F.);
#37978=ORIENTED_EDGE('',*,*,#28332,.F.);
#37979=ORIENTED_EDGE('',*,*,#26207,.T.);
#37980=ORIENTED_EDGE('',*,*,#28330,.T.);
#37981=ORIENTED_EDGE('',*,*,#28333,.F.);
#37982=ORIENTED_EDGE('',*,*,#28334,.F.);
#37983=ORIENTED_EDGE('',*,*,#26208,.T.);
#37984=ORIENTED_EDGE('',*,*,#28332,.T.);
#37985=ORIENTED_EDGE('',*,*,#28335,.F.);
#37986=ORIENTED_EDGE('',*,*,#28336,.F.);
#37987=ORIENTED_EDGE('',*,*,#26209,.T.);
#37988=ORIENTED_EDGE('',*,*,#28334,.T.);
#37989=ORIENTED_EDGE('',*,*,#28337,.F.);
#37990=ORIENTED_EDGE('',*,*,#28338,.F.);
#37991=ORIENTED_EDGE('',*,*,#26210,.T.);
#37992=ORIENTED_EDGE('',*,*,#28336,.T.);
#37993=ORIENTED_EDGE('',*,*,#28339,.F.);
#37994=ORIENTED_EDGE('',*,*,#28340,.F.);
#37995=ORIENTED_EDGE('',*,*,#26211,.T.);
#37996=ORIENTED_EDGE('',*,*,#28338,.T.);
#37997=ORIENTED_EDGE('',*,*,#28341,.F.);
#37998=ORIENTED_EDGE('',*,*,#28342,.F.);
#37999=ORIENTED_EDGE('',*,*,#26212,.T.);
#38000=ORIENTED_EDGE('',*,*,#28340,.T.);
#38001=ORIENTED_EDGE('',*,*,#28343,.F.);
#38002=ORIENTED_EDGE('',*,*,#28344,.F.);
#38003=ORIENTED_EDGE('',*,*,#26213,.T.);
#38004=ORIENTED_EDGE('',*,*,#28342,.T.);
#38005=ORIENTED_EDGE('',*,*,#28345,.F.);
#38006=ORIENTED_EDGE('',*,*,#27181,.F.);
#38007=ORIENTED_EDGE('',*,*,#26214,.T.);
#38008=ORIENTED_EDGE('',*,*,#28344,.T.);
#38009=ORIENTED_EDGE('',*,*,#27090,.T.);
#38010=ORIENTED_EDGE('',*,*,#27184,.F.);
#38011=ORIENTED_EDGE('',*,*,#27531,.F.);
#38012=ORIENTED_EDGE('',*,*,#26217,.F.);
#38013=ORIENTED_EDGE('',*,*,#27182,.T.);
#38014=ORIENTED_EDGE('',*,*,#28345,.T.);
#38015=ORIENTED_EDGE('',*,*,#28343,.T.);
#38016=ORIENTED_EDGE('',*,*,#28341,.T.);
#38017=ORIENTED_EDGE('',*,*,#28339,.T.);
#38018=ORIENTED_EDGE('',*,*,#28337,.T.);
#38019=ORIENTED_EDGE('',*,*,#28335,.T.);
#38020=ORIENTED_EDGE('',*,*,#28333,.T.);
#38021=ORIENTED_EDGE('',*,*,#28331,.T.);
#38022=ORIENTED_EDGE('',*,*,#28329,.T.);
#38023=ORIENTED_EDGE('',*,*,#28327,.T.);
#38024=ORIENTED_EDGE('',*,*,#28325,.T.);
#38025=ORIENTED_EDGE('',*,*,#28323,.T.);
#38026=ORIENTED_EDGE('',*,*,#28321,.T.);
#38027=ORIENTED_EDGE('',*,*,#26972,.T.);
#38028=ORIENTED_EDGE('',*,*,#28346,.F.);
#38029=ORIENTED_EDGE('',*,*,#28347,.T.);
#38030=ORIENTED_EDGE('',*,*,#28348,.T.);
#38031=ORIENTED_EDGE('',*,*,#28349,.T.);
#38032=ORIENTED_EDGE('',*,*,#28350,.T.);
#38033=ORIENTED_EDGE('',*,*,#28351,.T.);
#38034=ORIENTED_EDGE('',*,*,#28352,.T.);
#38035=ORIENTED_EDGE('',*,*,#28353,.T.);
#38036=ORIENTED_EDGE('',*,*,#28354,.T.);
#38037=ORIENTED_EDGE('',*,*,#28355,.T.);
#38038=ORIENTED_EDGE('',*,*,#28356,.T.);
#38039=ORIENTED_EDGE('',*,*,#28357,.T.);
#38040=ORIENTED_EDGE('',*,*,#28358,.T.);
#38041=ORIENTED_EDGE('',*,*,#28359,.T.);
#38042=ORIENTED_EDGE('',*,*,#28360,.T.);
#38043=ORIENTED_EDGE('',*,*,#26183,.T.);
#38044=ORIENTED_EDGE('',*,*,#27532,.T.);
#38045=ORIENTED_EDGE('',*,*,#28360,.F.);
#38046=ORIENTED_EDGE('',*,*,#28361,.F.);
#38047=ORIENTED_EDGE('',*,*,#26150,.T.);
#38048=ORIENTED_EDGE('',*,*,#26184,.T.);
#38049=ORIENTED_EDGE('',*,*,#28359,.F.);
#38050=ORIENTED_EDGE('',*,*,#28362,.F.);
#38051=ORIENTED_EDGE('',*,*,#26151,.T.);
#38052=ORIENTED_EDGE('',*,*,#28361,.T.);
#38053=ORIENTED_EDGE('',*,*,#28358,.F.);
#38054=ORIENTED_EDGE('',*,*,#28363,.F.);
#38055=ORIENTED_EDGE('',*,*,#26152,.T.);
#38056=ORIENTED_EDGE('',*,*,#28362,.T.);
#38057=ORIENTED_EDGE('',*,*,#28357,.F.);
#38058=ORIENTED_EDGE('',*,*,#28364,.F.);
#38059=ORIENTED_EDGE('',*,*,#26153,.T.);
#38060=ORIENTED_EDGE('',*,*,#28363,.T.);
#38061=ORIENTED_EDGE('',*,*,#28356,.F.);
#38062=ORIENTED_EDGE('',*,*,#28365,.F.);
#38063=ORIENTED_EDGE('',*,*,#26154,.T.);
#38064=ORIENTED_EDGE('',*,*,#28364,.T.);
#38065=ORIENTED_EDGE('',*,*,#28355,.F.);
#38066=ORIENTED_EDGE('',*,*,#28366,.F.);
#38067=ORIENTED_EDGE('',*,*,#26155,.T.);
#38068=ORIENTED_EDGE('',*,*,#28365,.T.);
#38069=ORIENTED_EDGE('',*,*,#28354,.F.);
#38070=ORIENTED_EDGE('',*,*,#28367,.F.);
#38071=ORIENTED_EDGE('',*,*,#26156,.T.);
#38072=ORIENTED_EDGE('',*,*,#28366,.T.);
#38073=ORIENTED_EDGE('',*,*,#28353,.F.);
#38074=ORIENTED_EDGE('',*,*,#28368,.F.);
#38075=ORIENTED_EDGE('',*,*,#26157,.T.);
#38076=ORIENTED_EDGE('',*,*,#28367,.T.);
#38077=ORIENTED_EDGE('',*,*,#28352,.F.);
#38078=ORIENTED_EDGE('',*,*,#28369,.F.);
#38079=ORIENTED_EDGE('',*,*,#26158,.T.);
#38080=ORIENTED_EDGE('',*,*,#28368,.T.);
#38081=ORIENTED_EDGE('',*,*,#28351,.F.);
#38082=ORIENTED_EDGE('',*,*,#28370,.F.);
#38083=ORIENTED_EDGE('',*,*,#26159,.T.);
#38084=ORIENTED_EDGE('',*,*,#28369,.T.);
#38085=ORIENTED_EDGE('',*,*,#28350,.F.);
#38086=ORIENTED_EDGE('',*,*,#28371,.F.);
#38087=ORIENTED_EDGE('',*,*,#26160,.T.);
#38088=ORIENTED_EDGE('',*,*,#28370,.T.);
#38089=ORIENTED_EDGE('',*,*,#28349,.F.);
#38090=ORIENTED_EDGE('',*,*,#28372,.F.);
#38091=ORIENTED_EDGE('',*,*,#26161,.T.);
#38092=ORIENTED_EDGE('',*,*,#28371,.T.);
#38093=ORIENTED_EDGE('',*,*,#28348,.F.);
#38094=ORIENTED_EDGE('',*,*,#28373,.F.);
#38095=ORIENTED_EDGE('',*,*,#26162,.T.);
#38096=ORIENTED_EDGE('',*,*,#28372,.T.);
#38097=ORIENTED_EDGE('',*,*,#26811,.T.);
#38098=ORIENTED_EDGE('',*,*,#26163,.T.);
#38099=ORIENTED_EDGE('',*,*,#28373,.T.);
#38100=ORIENTED_EDGE('',*,*,#28347,.F.);
#38101=ORIENTED_EDGE('',*,*,#28374,.F.);
#38102=ORIENTED_EDGE('',*,*,#27367,.T.);
#38103=ORIENTED_EDGE('',*,*,#27301,.T.);
#38104=ORIENTED_EDGE('',*,*,#28375,.F.);
#38105=ORIENTED_EDGE('',*,*,#28376,.F.);
#38106=ORIENTED_EDGE('',*,*,#26166,.T.);
#38107=ORIENTED_EDGE('',*,*,#26968,.T.);
#38108=ORIENTED_EDGE('',*,*,#28377,.F.);
#38109=ORIENTED_EDGE('',*,*,#28378,.F.);
#38110=ORIENTED_EDGE('',*,*,#26167,.T.);
#38111=ORIENTED_EDGE('',*,*,#28376,.T.);
#38112=ORIENTED_EDGE('',*,*,#28379,.F.);
#38113=ORIENTED_EDGE('',*,*,#28380,.F.);
#38114=ORIENTED_EDGE('',*,*,#26168,.T.);
#38115=ORIENTED_EDGE('',*,*,#28378,.T.);
#38116=ORIENTED_EDGE('',*,*,#28381,.F.);
#38117=ORIENTED_EDGE('',*,*,#28382,.F.);
#38118=ORIENTED_EDGE('',*,*,#26169,.T.);
#38119=ORIENTED_EDGE('',*,*,#28380,.T.);
#38120=ORIENTED_EDGE('',*,*,#28383,.F.);
#38121=ORIENTED_EDGE('',*,*,#28384,.F.);
#38122=ORIENTED_EDGE('',*,*,#26170,.T.);
#38123=ORIENTED_EDGE('',*,*,#28382,.T.);
#38124=ORIENTED_EDGE('',*,*,#28385,.F.);
#38125=ORIENTED_EDGE('',*,*,#28386,.F.);
#38126=ORIENTED_EDGE('',*,*,#26171,.T.);
#38127=ORIENTED_EDGE('',*,*,#28384,.T.);
#38128=ORIENTED_EDGE('',*,*,#28387,.F.);
#38129=ORIENTED_EDGE('',*,*,#28388,.F.);
#38130=ORIENTED_EDGE('',*,*,#26172,.T.);
#38131=ORIENTED_EDGE('',*,*,#28386,.T.);
#38132=ORIENTED_EDGE('',*,*,#28389,.F.);
#38133=ORIENTED_EDGE('',*,*,#28390,.F.);
#38134=ORIENTED_EDGE('',*,*,#26173,.T.);
#38135=ORIENTED_EDGE('',*,*,#28388,.T.);
#38136=ORIENTED_EDGE('',*,*,#28391,.F.);
#38137=ORIENTED_EDGE('',*,*,#28392,.F.);
#38138=ORIENTED_EDGE('',*,*,#26174,.T.);
#38139=ORIENTED_EDGE('',*,*,#28390,.T.);
#38140=ORIENTED_EDGE('',*,*,#28393,.F.);
#38141=ORIENTED_EDGE('',*,*,#28394,.F.);
#38142=ORIENTED_EDGE('',*,*,#26175,.T.);
#38143=ORIENTED_EDGE('',*,*,#28392,.T.);
#38144=ORIENTED_EDGE('',*,*,#28395,.F.);
#38145=ORIENTED_EDGE('',*,*,#28396,.F.);
#38146=ORIENTED_EDGE('',*,*,#26176,.T.);
#38147=ORIENTED_EDGE('',*,*,#28394,.T.);
#38148=ORIENTED_EDGE('',*,*,#28397,.F.);
#38149=ORIENTED_EDGE('',*,*,#28398,.F.);
#38150=ORIENTED_EDGE('',*,*,#26177,.T.);
#38151=ORIENTED_EDGE('',*,*,#28396,.T.);
#38152=ORIENTED_EDGE('',*,*,#28399,.F.);
#38153=ORIENTED_EDGE('',*,*,#27185,.F.);
#38154=ORIENTED_EDGE('',*,*,#26178,.T.);
#38155=ORIENTED_EDGE('',*,*,#28398,.T.);
#38156=ORIENTED_EDGE('',*,*,#27088,.T.);
#38157=ORIENTED_EDGE('',*,*,#27188,.F.);
#38158=ORIENTED_EDGE('',*,*,#27533,.F.);
#38159=ORIENTED_EDGE('',*,*,#26181,.F.);
#38160=ORIENTED_EDGE('',*,*,#27186,.T.);
#38161=ORIENTED_EDGE('',*,*,#28399,.T.);
#38162=ORIENTED_EDGE('',*,*,#28397,.T.);
#38163=ORIENTED_EDGE('',*,*,#28395,.T.);
#38164=ORIENTED_EDGE('',*,*,#28393,.T.);
#38165=ORIENTED_EDGE('',*,*,#28391,.T.);
#38166=ORIENTED_EDGE('',*,*,#28389,.T.);
#38167=ORIENTED_EDGE('',*,*,#28387,.T.);
#38168=ORIENTED_EDGE('',*,*,#28385,.T.);
#38169=ORIENTED_EDGE('',*,*,#28383,.T.);
#38170=ORIENTED_EDGE('',*,*,#28381,.T.);
#38171=ORIENTED_EDGE('',*,*,#28379,.T.);
#38172=ORIENTED_EDGE('',*,*,#28377,.T.);
#38173=ORIENTED_EDGE('',*,*,#28375,.T.);
#38174=ORIENTED_EDGE('',*,*,#26967,.T.);
#38175=ORIENTED_EDGE('',*,*,#28400,.F.);
#38176=ORIENTED_EDGE('',*,*,#28401,.T.);
#38177=ORIENTED_EDGE('',*,*,#28402,.T.);
#38178=ORIENTED_EDGE('',*,*,#28403,.T.);
#38179=ORIENTED_EDGE('',*,*,#28404,.T.);
#38180=ORIENTED_EDGE('',*,*,#28405,.T.);
#38181=ORIENTED_EDGE('',*,*,#28406,.T.);
#38182=ORIENTED_EDGE('',*,*,#28407,.T.);
#38183=ORIENTED_EDGE('',*,*,#28408,.T.);
#38184=ORIENTED_EDGE('',*,*,#28409,.T.);
#38185=ORIENTED_EDGE('',*,*,#28410,.T.);
#38186=ORIENTED_EDGE('',*,*,#28411,.T.);
#38187=ORIENTED_EDGE('',*,*,#28412,.T.);
#38188=ORIENTED_EDGE('',*,*,#28413,.T.);
#38189=ORIENTED_EDGE('',*,*,#28414,.T.);
#38190=ORIENTED_EDGE('',*,*,#26147,.T.);
#38191=ORIENTED_EDGE('',*,*,#27534,.T.);
#38192=ORIENTED_EDGE('',*,*,#28414,.F.);
#38193=ORIENTED_EDGE('',*,*,#28415,.F.);
#38194=ORIENTED_EDGE('',*,*,#26114,.T.);
#38195=ORIENTED_EDGE('',*,*,#26148,.T.);
#38196=ORIENTED_EDGE('',*,*,#28413,.F.);
#38197=ORIENTED_EDGE('',*,*,#28416,.F.);
#38198=ORIENTED_EDGE('',*,*,#26115,.T.);
#38199=ORIENTED_EDGE('',*,*,#28415,.T.);
#38200=ORIENTED_EDGE('',*,*,#28412,.F.);
#38201=ORIENTED_EDGE('',*,*,#28417,.F.);
#38202=ORIENTED_EDGE('',*,*,#26116,.T.);
#38203=ORIENTED_EDGE('',*,*,#28416,.T.);
#38204=ORIENTED_EDGE('',*,*,#28411,.F.);
#38205=ORIENTED_EDGE('',*,*,#28418,.F.);
#38206=ORIENTED_EDGE('',*,*,#26117,.T.);
#38207=ORIENTED_EDGE('',*,*,#28417,.T.);
#38208=ORIENTED_EDGE('',*,*,#28410,.F.);
#38209=ORIENTED_EDGE('',*,*,#28419,.F.);
#38210=ORIENTED_EDGE('',*,*,#26118,.T.);
#38211=ORIENTED_EDGE('',*,*,#28418,.T.);
#38212=ORIENTED_EDGE('',*,*,#28409,.F.);
#38213=ORIENTED_EDGE('',*,*,#28420,.F.);
#38214=ORIENTED_EDGE('',*,*,#26119,.T.);
#38215=ORIENTED_EDGE('',*,*,#28419,.T.);
#38216=ORIENTED_EDGE('',*,*,#28408,.F.);
#38217=ORIENTED_EDGE('',*,*,#28421,.F.);
#38218=ORIENTED_EDGE('',*,*,#26120,.T.);
#38219=ORIENTED_EDGE('',*,*,#28420,.T.);
#38220=ORIENTED_EDGE('',*,*,#28407,.F.);
#38221=ORIENTED_EDGE('',*,*,#28422,.F.);
#38222=ORIENTED_EDGE('',*,*,#26121,.T.);
#38223=ORIENTED_EDGE('',*,*,#28421,.T.);
#38224=ORIENTED_EDGE('',*,*,#28406,.F.);
#38225=ORIENTED_EDGE('',*,*,#28423,.F.);
#38226=ORIENTED_EDGE('',*,*,#26122,.T.);
#38227=ORIENTED_EDGE('',*,*,#28422,.T.);
#38228=ORIENTED_EDGE('',*,*,#28405,.F.);
#38229=ORIENTED_EDGE('',*,*,#28424,.F.);
#38230=ORIENTED_EDGE('',*,*,#26123,.T.);
#38231=ORIENTED_EDGE('',*,*,#28423,.T.);
#38232=ORIENTED_EDGE('',*,*,#28404,.F.);
#38233=ORIENTED_EDGE('',*,*,#28425,.F.);
#38234=ORIENTED_EDGE('',*,*,#26124,.T.);
#38235=ORIENTED_EDGE('',*,*,#28424,.T.);
#38236=ORIENTED_EDGE('',*,*,#28403,.F.);
#38237=ORIENTED_EDGE('',*,*,#28426,.F.);
#38238=ORIENTED_EDGE('',*,*,#26125,.T.);
#38239=ORIENTED_EDGE('',*,*,#28425,.T.);
#38240=ORIENTED_EDGE('',*,*,#28402,.F.);
#38241=ORIENTED_EDGE('',*,*,#28427,.F.);
#38242=ORIENTED_EDGE('',*,*,#26126,.T.);
#38243=ORIENTED_EDGE('',*,*,#28426,.T.);
#38244=ORIENTED_EDGE('',*,*,#26814,.T.);
#38245=ORIENTED_EDGE('',*,*,#26127,.T.);
#38246=ORIENTED_EDGE('',*,*,#28427,.T.);
#38247=ORIENTED_EDGE('',*,*,#28401,.F.);
#38248=ORIENTED_EDGE('',*,*,#28428,.F.);
#38249=ORIENTED_EDGE('',*,*,#27369,.T.);
#38250=ORIENTED_EDGE('',*,*,#27299,.T.);
#38251=ORIENTED_EDGE('',*,*,#28429,.F.);
#38252=ORIENTED_EDGE('',*,*,#28430,.F.);
#38253=ORIENTED_EDGE('',*,*,#26130,.T.);
#38254=ORIENTED_EDGE('',*,*,#26963,.T.);
#38255=ORIENTED_EDGE('',*,*,#28431,.F.);
#38256=ORIENTED_EDGE('',*,*,#28432,.F.);
#38257=ORIENTED_EDGE('',*,*,#26131,.T.);
#38258=ORIENTED_EDGE('',*,*,#28430,.T.);
#38259=ORIENTED_EDGE('',*,*,#28433,.F.);
#38260=ORIENTED_EDGE('',*,*,#28434,.F.);
#38261=ORIENTED_EDGE('',*,*,#26132,.T.);
#38262=ORIENTED_EDGE('',*,*,#28432,.T.);
#38263=ORIENTED_EDGE('',*,*,#28435,.F.);
#38264=ORIENTED_EDGE('',*,*,#28436,.F.);
#38265=ORIENTED_EDGE('',*,*,#26133,.T.);
#38266=ORIENTED_EDGE('',*,*,#28434,.T.);
#38267=ORIENTED_EDGE('',*,*,#28437,.F.);
#38268=ORIENTED_EDGE('',*,*,#28438,.F.);
#38269=ORIENTED_EDGE('',*,*,#26134,.T.);
#38270=ORIENTED_EDGE('',*,*,#28436,.T.);
#38271=ORIENTED_EDGE('',*,*,#28439,.F.);
#38272=ORIENTED_EDGE('',*,*,#28440,.F.);
#38273=ORIENTED_EDGE('',*,*,#26135,.T.);
#38274=ORIENTED_EDGE('',*,*,#28438,.T.);
#38275=ORIENTED_EDGE('',*,*,#28441,.F.);
#38276=ORIENTED_EDGE('',*,*,#28442,.F.);
#38277=ORIENTED_EDGE('',*,*,#26136,.T.);
#38278=ORIENTED_EDGE('',*,*,#28440,.T.);
#38279=ORIENTED_EDGE('',*,*,#28443,.F.);
#38280=ORIENTED_EDGE('',*,*,#28444,.F.);
#38281=ORIENTED_EDGE('',*,*,#26137,.T.);
#38282=ORIENTED_EDGE('',*,*,#28442,.T.);
#38283=ORIENTED_EDGE('',*,*,#28445,.F.);
#38284=ORIENTED_EDGE('',*,*,#28446,.F.);
#38285=ORIENTED_EDGE('',*,*,#26138,.T.);
#38286=ORIENTED_EDGE('',*,*,#28444,.T.);
#38287=ORIENTED_EDGE('',*,*,#28447,.F.);
#38288=ORIENTED_EDGE('',*,*,#28448,.F.);
#38289=ORIENTED_EDGE('',*,*,#26139,.T.);
#38290=ORIENTED_EDGE('',*,*,#28446,.T.);
#38291=ORIENTED_EDGE('',*,*,#28449,.F.);
#38292=ORIENTED_EDGE('',*,*,#28450,.F.);
#38293=ORIENTED_EDGE('',*,*,#26140,.T.);
#38294=ORIENTED_EDGE('',*,*,#28448,.T.);
#38295=ORIENTED_EDGE('',*,*,#28451,.F.);
#38296=ORIENTED_EDGE('',*,*,#28452,.F.);
#38297=ORIENTED_EDGE('',*,*,#26141,.T.);
#38298=ORIENTED_EDGE('',*,*,#28450,.T.);
#38299=ORIENTED_EDGE('',*,*,#28453,.F.);
#38300=ORIENTED_EDGE('',*,*,#27189,.F.);
#38301=ORIENTED_EDGE('',*,*,#26142,.T.);
#38302=ORIENTED_EDGE('',*,*,#28452,.T.);
#38303=ORIENTED_EDGE('',*,*,#27086,.T.);
#38304=ORIENTED_EDGE('',*,*,#27192,.F.);
#38305=ORIENTED_EDGE('',*,*,#27464,.F.);
#38306=ORIENTED_EDGE('',*,*,#27535,.F.);
#38307=ORIENTED_EDGE('',*,*,#26145,.F.);
#38308=ORIENTED_EDGE('',*,*,#27190,.T.);
#38309=ORIENTED_EDGE('',*,*,#28453,.T.);
#38310=ORIENTED_EDGE('',*,*,#28451,.T.);
#38311=ORIENTED_EDGE('',*,*,#28449,.T.);
#38312=ORIENTED_EDGE('',*,*,#28447,.T.);
#38313=ORIENTED_EDGE('',*,*,#28445,.T.);
#38314=ORIENTED_EDGE('',*,*,#28443,.T.);
#38315=ORIENTED_EDGE('',*,*,#28441,.T.);
#38316=ORIENTED_EDGE('',*,*,#28439,.T.);
#38317=ORIENTED_EDGE('',*,*,#28437,.T.);
#38318=ORIENTED_EDGE('',*,*,#28435,.T.);
#38319=ORIENTED_EDGE('',*,*,#28433,.T.);
#38320=ORIENTED_EDGE('',*,*,#28431,.T.);
#38321=ORIENTED_EDGE('',*,*,#28429,.T.);
#38322=ORIENTED_EDGE('',*,*,#26962,.T.);
#38323=ORIENTED_EDGE('',*,*,#28454,.F.);
#38324=ORIENTED_EDGE('',*,*,#28455,.T.);
#38325=ORIENTED_EDGE('',*,*,#28456,.T.);
#38326=ORIENTED_EDGE('',*,*,#28457,.T.);
#38327=ORIENTED_EDGE('',*,*,#28458,.T.);
#38328=ORIENTED_EDGE('',*,*,#28459,.T.);
#38329=ORIENTED_EDGE('',*,*,#28460,.T.);
#38330=ORIENTED_EDGE('',*,*,#28461,.T.);
#38331=ORIENTED_EDGE('',*,*,#28462,.T.);
#38332=ORIENTED_EDGE('',*,*,#28463,.T.);
#38333=ORIENTED_EDGE('',*,*,#28464,.T.);
#38334=ORIENTED_EDGE('',*,*,#28465,.T.);
#38335=ORIENTED_EDGE('',*,*,#28466,.T.);
#38336=ORIENTED_EDGE('',*,*,#28467,.T.);
#38337=ORIENTED_EDGE('',*,*,#28468,.T.);
#38338=ORIENTED_EDGE('',*,*,#26111,.T.);
#38339=ORIENTED_EDGE('',*,*,#27465,.T.);
#38340=ORIENTED_EDGE('',*,*,#28468,.F.);
#38341=ORIENTED_EDGE('',*,*,#28469,.F.);
#38342=ORIENTED_EDGE('',*,*,#26078,.T.);
#38343=ORIENTED_EDGE('',*,*,#26112,.T.);
#38344=ORIENTED_EDGE('',*,*,#28467,.F.);
#38345=ORIENTED_EDGE('',*,*,#28470,.F.);
#38346=ORIENTED_EDGE('',*,*,#26079,.T.);
#38347=ORIENTED_EDGE('',*,*,#28469,.T.);
#38348=ORIENTED_EDGE('',*,*,#28466,.F.);
#38349=ORIENTED_EDGE('',*,*,#28471,.F.);
#38350=ORIENTED_EDGE('',*,*,#26080,.T.);
#38351=ORIENTED_EDGE('',*,*,#28470,.T.);
#38352=ORIENTED_EDGE('',*,*,#28465,.F.);
#38353=ORIENTED_EDGE('',*,*,#28472,.F.);
#38354=ORIENTED_EDGE('',*,*,#26081,.T.);
#38355=ORIENTED_EDGE('',*,*,#28471,.T.);
#38356=ORIENTED_EDGE('',*,*,#28464,.F.);
#38357=ORIENTED_EDGE('',*,*,#28473,.F.);
#38358=ORIENTED_EDGE('',*,*,#26082,.T.);
#38359=ORIENTED_EDGE('',*,*,#28472,.T.);
#38360=ORIENTED_EDGE('',*,*,#28463,.F.);
#38361=ORIENTED_EDGE('',*,*,#28474,.F.);
#38362=ORIENTED_EDGE('',*,*,#26083,.T.);
#38363=ORIENTED_EDGE('',*,*,#28473,.T.);
#38364=ORIENTED_EDGE('',*,*,#28462,.F.);
#38365=ORIENTED_EDGE('',*,*,#28475,.F.);
#38366=ORIENTED_EDGE('',*,*,#26084,.T.);
#38367=ORIENTED_EDGE('',*,*,#28474,.T.);
#38368=ORIENTED_EDGE('',*,*,#28461,.F.);
#38369=ORIENTED_EDGE('',*,*,#28476,.F.);
#38370=ORIENTED_EDGE('',*,*,#26085,.T.);
#38371=ORIENTED_EDGE('',*,*,#28475,.T.);
#38372=ORIENTED_EDGE('',*,*,#28460,.F.);
#38373=ORIENTED_EDGE('',*,*,#28477,.F.);
#38374=ORIENTED_EDGE('',*,*,#26086,.T.);
#38375=ORIENTED_EDGE('',*,*,#28476,.T.);
#38376=ORIENTED_EDGE('',*,*,#28459,.F.);
#38377=ORIENTED_EDGE('',*,*,#28478,.F.);
#38378=ORIENTED_EDGE('',*,*,#26087,.T.);
#38379=ORIENTED_EDGE('',*,*,#28477,.T.);
#38380=ORIENTED_EDGE('',*,*,#28458,.F.);
#38381=ORIENTED_EDGE('',*,*,#28479,.F.);
#38382=ORIENTED_EDGE('',*,*,#26088,.T.);
#38383=ORIENTED_EDGE('',*,*,#28478,.T.);
#38384=ORIENTED_EDGE('',*,*,#28457,.F.);
#38385=ORIENTED_EDGE('',*,*,#28480,.F.);
#38386=ORIENTED_EDGE('',*,*,#26089,.T.);
#38387=ORIENTED_EDGE('',*,*,#28479,.T.);
#38388=ORIENTED_EDGE('',*,*,#28456,.F.);
#38389=ORIENTED_EDGE('',*,*,#28481,.F.);
#38390=ORIENTED_EDGE('',*,*,#26090,.T.);
#38391=ORIENTED_EDGE('',*,*,#28480,.T.);
#38392=ORIENTED_EDGE('',*,*,#26817,.T.);
#38393=ORIENTED_EDGE('',*,*,#26091,.T.);
#38394=ORIENTED_EDGE('',*,*,#28481,.T.);
#38395=ORIENTED_EDGE('',*,*,#28455,.F.);
#38396=ORIENTED_EDGE('',*,*,#28482,.F.);
#38397=ORIENTED_EDGE('',*,*,#27372,.T.);
#38398=ORIENTED_EDGE('',*,*,#27297,.T.);
#38399=ORIENTED_EDGE('',*,*,#28483,.F.);
#38400=ORIENTED_EDGE('',*,*,#28484,.F.);
#38401=ORIENTED_EDGE('',*,*,#26094,.T.);
#38402=ORIENTED_EDGE('',*,*,#26958,.T.);
#38403=ORIENTED_EDGE('',*,*,#28485,.F.);
#38404=ORIENTED_EDGE('',*,*,#28486,.F.);
#38405=ORIENTED_EDGE('',*,*,#26095,.T.);
#38406=ORIENTED_EDGE('',*,*,#28484,.T.);
#38407=ORIENTED_EDGE('',*,*,#28487,.F.);
#38408=ORIENTED_EDGE('',*,*,#28488,.F.);
#38409=ORIENTED_EDGE('',*,*,#26096,.T.);
#38410=ORIENTED_EDGE('',*,*,#28486,.T.);
#38411=ORIENTED_EDGE('',*,*,#28489,.F.);
#38412=ORIENTED_EDGE('',*,*,#28490,.F.);
#38413=ORIENTED_EDGE('',*,*,#26097,.T.);
#38414=ORIENTED_EDGE('',*,*,#28488,.T.);
#38415=ORIENTED_EDGE('',*,*,#28491,.F.);
#38416=ORIENTED_EDGE('',*,*,#28492,.F.);
#38417=ORIENTED_EDGE('',*,*,#26098,.T.);
#38418=ORIENTED_EDGE('',*,*,#28490,.T.);
#38419=ORIENTED_EDGE('',*,*,#28493,.F.);
#38420=ORIENTED_EDGE('',*,*,#28494,.F.);
#38421=ORIENTED_EDGE('',*,*,#26099,.T.);
#38422=ORIENTED_EDGE('',*,*,#28492,.T.);
#38423=ORIENTED_EDGE('',*,*,#28495,.F.);
#38424=ORIENTED_EDGE('',*,*,#28496,.F.);
#38425=ORIENTED_EDGE('',*,*,#26100,.T.);
#38426=ORIENTED_EDGE('',*,*,#28494,.T.);
#38427=ORIENTED_EDGE('',*,*,#28497,.F.);
#38428=ORIENTED_EDGE('',*,*,#28498,.F.);
#38429=ORIENTED_EDGE('',*,*,#26101,.T.);
#38430=ORIENTED_EDGE('',*,*,#28496,.T.);
#38431=ORIENTED_EDGE('',*,*,#28499,.F.);
#38432=ORIENTED_EDGE('',*,*,#28500,.F.);
#38433=ORIENTED_EDGE('',*,*,#26102,.T.);
#38434=ORIENTED_EDGE('',*,*,#28498,.T.);
#38435=ORIENTED_EDGE('',*,*,#28501,.F.);
#38436=ORIENTED_EDGE('',*,*,#28502,.F.);
#38437=ORIENTED_EDGE('',*,*,#26103,.T.);
#38438=ORIENTED_EDGE('',*,*,#28500,.T.);
#38439=ORIENTED_EDGE('',*,*,#28503,.F.);
#38440=ORIENTED_EDGE('',*,*,#28504,.F.);
#38441=ORIENTED_EDGE('',*,*,#26104,.T.);
#38442=ORIENTED_EDGE('',*,*,#28502,.T.);
#38443=ORIENTED_EDGE('',*,*,#28505,.F.);
#38444=ORIENTED_EDGE('',*,*,#28506,.F.);
#38445=ORIENTED_EDGE('',*,*,#26105,.T.);
#38446=ORIENTED_EDGE('',*,*,#28504,.T.);
#38447=ORIENTED_EDGE('',*,*,#28507,.F.);
#38448=ORIENTED_EDGE('',*,*,#27193,.F.);
#38449=ORIENTED_EDGE('',*,*,#26106,.T.);
#38450=ORIENTED_EDGE('',*,*,#28506,.T.);
#38451=ORIENTED_EDGE('',*,*,#27084,.T.);
#38452=ORIENTED_EDGE('',*,*,#27196,.F.);
#38453=ORIENTED_EDGE('',*,*,#27466,.F.);
#38454=ORIENTED_EDGE('',*,*,#26109,.F.);
#38455=ORIENTED_EDGE('',*,*,#27194,.T.);
#38456=ORIENTED_EDGE('',*,*,#28507,.T.);
#38457=ORIENTED_EDGE('',*,*,#28505,.T.);
#38458=ORIENTED_EDGE('',*,*,#28503,.T.);
#38459=ORIENTED_EDGE('',*,*,#28501,.T.);
#38460=ORIENTED_EDGE('',*,*,#28499,.T.);
#38461=ORIENTED_EDGE('',*,*,#28497,.T.);
#38462=ORIENTED_EDGE('',*,*,#28495,.T.);
#38463=ORIENTED_EDGE('',*,*,#28493,.T.);
#38464=ORIENTED_EDGE('',*,*,#28491,.T.);
#38465=ORIENTED_EDGE('',*,*,#28489,.T.);
#38466=ORIENTED_EDGE('',*,*,#28487,.T.);
#38467=ORIENTED_EDGE('',*,*,#28485,.T.);
#38468=ORIENTED_EDGE('',*,*,#28483,.T.);
#38469=ORIENTED_EDGE('',*,*,#26957,.T.);
#38470=ORIENTED_EDGE('',*,*,#28508,.F.);
#38471=ORIENTED_EDGE('',*,*,#28509,.T.);
#38472=ORIENTED_EDGE('',*,*,#28510,.T.);
#38473=ORIENTED_EDGE('',*,*,#28511,.T.);
#38474=ORIENTED_EDGE('',*,*,#28512,.T.);
#38475=ORIENTED_EDGE('',*,*,#28513,.T.);
#38476=ORIENTED_EDGE('',*,*,#28514,.T.);
#38477=ORIENTED_EDGE('',*,*,#28515,.T.);
#38478=ORIENTED_EDGE('',*,*,#28516,.T.);
#38479=ORIENTED_EDGE('',*,*,#28517,.T.);
#38480=ORIENTED_EDGE('',*,*,#28518,.T.);
#38481=ORIENTED_EDGE('',*,*,#28519,.T.);
#38482=ORIENTED_EDGE('',*,*,#28520,.T.);
#38483=ORIENTED_EDGE('',*,*,#28521,.T.);
#38484=ORIENTED_EDGE('',*,*,#28522,.T.);
#38485=ORIENTED_EDGE('',*,*,#26075,.T.);
#38486=ORIENTED_EDGE('',*,*,#27467,.T.);
#38487=ORIENTED_EDGE('',*,*,#28522,.F.);
#38488=ORIENTED_EDGE('',*,*,#28523,.F.);
#38489=ORIENTED_EDGE('',*,*,#26042,.T.);
#38490=ORIENTED_EDGE('',*,*,#26076,.T.);
#38491=ORIENTED_EDGE('',*,*,#28521,.F.);
#38492=ORIENTED_EDGE('',*,*,#28524,.F.);
#38493=ORIENTED_EDGE('',*,*,#26043,.T.);
#38494=ORIENTED_EDGE('',*,*,#28523,.T.);
#38495=ORIENTED_EDGE('',*,*,#28520,.F.);
#38496=ORIENTED_EDGE('',*,*,#28525,.F.);
#38497=ORIENTED_EDGE('',*,*,#26044,.T.);
#38498=ORIENTED_EDGE('',*,*,#28524,.T.);
#38499=ORIENTED_EDGE('',*,*,#28519,.F.);
#38500=ORIENTED_EDGE('',*,*,#28526,.F.);
#38501=ORIENTED_EDGE('',*,*,#26045,.T.);
#38502=ORIENTED_EDGE('',*,*,#28525,.T.);
#38503=ORIENTED_EDGE('',*,*,#28518,.F.);
#38504=ORIENTED_EDGE('',*,*,#28527,.F.);
#38505=ORIENTED_EDGE('',*,*,#26046,.T.);
#38506=ORIENTED_EDGE('',*,*,#28526,.T.);
#38507=ORIENTED_EDGE('',*,*,#28517,.F.);
#38508=ORIENTED_EDGE('',*,*,#28528,.F.);
#38509=ORIENTED_EDGE('',*,*,#26047,.T.);
#38510=ORIENTED_EDGE('',*,*,#28527,.T.);
#38511=ORIENTED_EDGE('',*,*,#28516,.F.);
#38512=ORIENTED_EDGE('',*,*,#28529,.F.);
#38513=ORIENTED_EDGE('',*,*,#26048,.T.);
#38514=ORIENTED_EDGE('',*,*,#28528,.T.);
#38515=ORIENTED_EDGE('',*,*,#28515,.F.);
#38516=ORIENTED_EDGE('',*,*,#28530,.F.);
#38517=ORIENTED_EDGE('',*,*,#26049,.T.);
#38518=ORIENTED_EDGE('',*,*,#28529,.T.);
#38519=ORIENTED_EDGE('',*,*,#28514,.F.);
#38520=ORIENTED_EDGE('',*,*,#28531,.F.);
#38521=ORIENTED_EDGE('',*,*,#26050,.T.);
#38522=ORIENTED_EDGE('',*,*,#28530,.T.);
#38523=ORIENTED_EDGE('',*,*,#28513,.F.);
#38524=ORIENTED_EDGE('',*,*,#28532,.F.);
#38525=ORIENTED_EDGE('',*,*,#26051,.T.);
#38526=ORIENTED_EDGE('',*,*,#28531,.T.);
#38527=ORIENTED_EDGE('',*,*,#28512,.F.);
#38528=ORIENTED_EDGE('',*,*,#28533,.F.);
#38529=ORIENTED_EDGE('',*,*,#26052,.T.);
#38530=ORIENTED_EDGE('',*,*,#28532,.T.);
#38531=ORIENTED_EDGE('',*,*,#28511,.F.);
#38532=ORIENTED_EDGE('',*,*,#28534,.F.);
#38533=ORIENTED_EDGE('',*,*,#26053,.T.);
#38534=ORIENTED_EDGE('',*,*,#28533,.T.);
#38535=ORIENTED_EDGE('',*,*,#28510,.F.);
#38536=ORIENTED_EDGE('',*,*,#28535,.F.);
#38537=ORIENTED_EDGE('',*,*,#26054,.T.);
#38538=ORIENTED_EDGE('',*,*,#28534,.T.);
#38539=ORIENTED_EDGE('',*,*,#26820,.T.);
#38540=ORIENTED_EDGE('',*,*,#26055,.T.);
#38541=ORIENTED_EDGE('',*,*,#28535,.T.);
#38542=ORIENTED_EDGE('',*,*,#28509,.F.);
#38543=ORIENTED_EDGE('',*,*,#28536,.F.);
#38544=ORIENTED_EDGE('',*,*,#27374,.T.);
#38545=ORIENTED_EDGE('',*,*,#27295,.T.);
#38546=ORIENTED_EDGE('',*,*,#28537,.F.);
#38547=ORIENTED_EDGE('',*,*,#28538,.F.);
#38548=ORIENTED_EDGE('',*,*,#26058,.T.);
#38549=ORIENTED_EDGE('',*,*,#26953,.T.);
#38550=ORIENTED_EDGE('',*,*,#28539,.F.);
#38551=ORIENTED_EDGE('',*,*,#28540,.F.);
#38552=ORIENTED_EDGE('',*,*,#26059,.T.);
#38553=ORIENTED_EDGE('',*,*,#28538,.T.);
#38554=ORIENTED_EDGE('',*,*,#28541,.F.);
#38555=ORIENTED_EDGE('',*,*,#28542,.F.);
#38556=ORIENTED_EDGE('',*,*,#26060,.T.);
#38557=ORIENTED_EDGE('',*,*,#28540,.T.);
#38558=ORIENTED_EDGE('',*,*,#28543,.F.);
#38559=ORIENTED_EDGE('',*,*,#28544,.F.);
#38560=ORIENTED_EDGE('',*,*,#26061,.T.);
#38561=ORIENTED_EDGE('',*,*,#28542,.T.);
#38562=ORIENTED_EDGE('',*,*,#28545,.F.);
#38563=ORIENTED_EDGE('',*,*,#28546,.F.);
#38564=ORIENTED_EDGE('',*,*,#26062,.T.);
#38565=ORIENTED_EDGE('',*,*,#28544,.T.);
#38566=ORIENTED_EDGE('',*,*,#28547,.F.);
#38567=ORIENTED_EDGE('',*,*,#28548,.F.);
#38568=ORIENTED_EDGE('',*,*,#26063,.T.);
#38569=ORIENTED_EDGE('',*,*,#28546,.T.);
#38570=ORIENTED_EDGE('',*,*,#28549,.F.);
#38571=ORIENTED_EDGE('',*,*,#28550,.F.);
#38572=ORIENTED_EDGE('',*,*,#26064,.T.);
#38573=ORIENTED_EDGE('',*,*,#28548,.T.);
#38574=ORIENTED_EDGE('',*,*,#28551,.F.);
#38575=ORIENTED_EDGE('',*,*,#28552,.F.);
#38576=ORIENTED_EDGE('',*,*,#26065,.T.);
#38577=ORIENTED_EDGE('',*,*,#28550,.T.);
#38578=ORIENTED_EDGE('',*,*,#28553,.F.);
#38579=ORIENTED_EDGE('',*,*,#28554,.F.);
#38580=ORIENTED_EDGE('',*,*,#26066,.T.);
#38581=ORIENTED_EDGE('',*,*,#28552,.T.);
#38582=ORIENTED_EDGE('',*,*,#28555,.F.);
#38583=ORIENTED_EDGE('',*,*,#28556,.F.);
#38584=ORIENTED_EDGE('',*,*,#26067,.T.);
#38585=ORIENTED_EDGE('',*,*,#28554,.T.);
#38586=ORIENTED_EDGE('',*,*,#28557,.F.);
#38587=ORIENTED_EDGE('',*,*,#28558,.F.);
#38588=ORIENTED_EDGE('',*,*,#26068,.T.);
#38589=ORIENTED_EDGE('',*,*,#28556,.T.);
#38590=ORIENTED_EDGE('',*,*,#28559,.F.);
#38591=ORIENTED_EDGE('',*,*,#28560,.F.);
#38592=ORIENTED_EDGE('',*,*,#26069,.T.);
#38593=ORIENTED_EDGE('',*,*,#28558,.T.);
#38594=ORIENTED_EDGE('',*,*,#28561,.F.);
#38595=ORIENTED_EDGE('',*,*,#27197,.F.);
#38596=ORIENTED_EDGE('',*,*,#26070,.T.);
#38597=ORIENTED_EDGE('',*,*,#28560,.T.);
#38598=ORIENTED_EDGE('',*,*,#27082,.T.);
#38599=ORIENTED_EDGE('',*,*,#27200,.F.);
#38600=ORIENTED_EDGE('',*,*,#27468,.F.);
#38601=ORIENTED_EDGE('',*,*,#26073,.F.);
#38602=ORIENTED_EDGE('',*,*,#27198,.T.);
#38603=ORIENTED_EDGE('',*,*,#28561,.T.);
#38604=ORIENTED_EDGE('',*,*,#28559,.T.);
#38605=ORIENTED_EDGE('',*,*,#28557,.T.);
#38606=ORIENTED_EDGE('',*,*,#28555,.T.);
#38607=ORIENTED_EDGE('',*,*,#28553,.T.);
#38608=ORIENTED_EDGE('',*,*,#28551,.T.);
#38609=ORIENTED_EDGE('',*,*,#28549,.T.);
#38610=ORIENTED_EDGE('',*,*,#28547,.T.);
#38611=ORIENTED_EDGE('',*,*,#28545,.T.);
#38612=ORIENTED_EDGE('',*,*,#28543,.T.);
#38613=ORIENTED_EDGE('',*,*,#28541,.T.);
#38614=ORIENTED_EDGE('',*,*,#28539,.T.);
#38615=ORIENTED_EDGE('',*,*,#28537,.T.);
#38616=ORIENTED_EDGE('',*,*,#26952,.T.);
#38617=ORIENTED_EDGE('',*,*,#28562,.F.);
#38618=ORIENTED_EDGE('',*,*,#28563,.T.);
#38619=ORIENTED_EDGE('',*,*,#28564,.T.);
#38620=ORIENTED_EDGE('',*,*,#28565,.T.);
#38621=ORIENTED_EDGE('',*,*,#28566,.T.);
#38622=ORIENTED_EDGE('',*,*,#28567,.T.);
#38623=ORIENTED_EDGE('',*,*,#28568,.T.);
#38624=ORIENTED_EDGE('',*,*,#28569,.T.);
#38625=ORIENTED_EDGE('',*,*,#28570,.T.);
#38626=ORIENTED_EDGE('',*,*,#28571,.T.);
#38627=ORIENTED_EDGE('',*,*,#28572,.T.);
#38628=ORIENTED_EDGE('',*,*,#28573,.T.);
#38629=ORIENTED_EDGE('',*,*,#28574,.T.);
#38630=ORIENTED_EDGE('',*,*,#28575,.T.);
#38631=ORIENTED_EDGE('',*,*,#28576,.T.);
#38632=ORIENTED_EDGE('',*,*,#26039,.T.);
#38633=ORIENTED_EDGE('',*,*,#27469,.T.);
#38634=ORIENTED_EDGE('',*,*,#28576,.F.);
#38635=ORIENTED_EDGE('',*,*,#28577,.F.);
#38636=ORIENTED_EDGE('',*,*,#26006,.T.);
#38637=ORIENTED_EDGE('',*,*,#26040,.T.);
#38638=ORIENTED_EDGE('',*,*,#28575,.F.);
#38639=ORIENTED_EDGE('',*,*,#28578,.F.);
#38640=ORIENTED_EDGE('',*,*,#26007,.T.);
#38641=ORIENTED_EDGE('',*,*,#28577,.T.);
#38642=ORIENTED_EDGE('',*,*,#28574,.F.);
#38643=ORIENTED_EDGE('',*,*,#28579,.F.);
#38644=ORIENTED_EDGE('',*,*,#26008,.T.);
#38645=ORIENTED_EDGE('',*,*,#28578,.T.);
#38646=ORIENTED_EDGE('',*,*,#28573,.F.);
#38647=ORIENTED_EDGE('',*,*,#28580,.F.);
#38648=ORIENTED_EDGE('',*,*,#26009,.T.);
#38649=ORIENTED_EDGE('',*,*,#28579,.T.);
#38650=ORIENTED_EDGE('',*,*,#28572,.F.);
#38651=ORIENTED_EDGE('',*,*,#28581,.F.);
#38652=ORIENTED_EDGE('',*,*,#26010,.T.);
#38653=ORIENTED_EDGE('',*,*,#28580,.T.);
#38654=ORIENTED_EDGE('',*,*,#28571,.F.);
#38655=ORIENTED_EDGE('',*,*,#28582,.F.);
#38656=ORIENTED_EDGE('',*,*,#26011,.T.);
#38657=ORIENTED_EDGE('',*,*,#28581,.T.);
#38658=ORIENTED_EDGE('',*,*,#28570,.F.);
#38659=ORIENTED_EDGE('',*,*,#28583,.F.);
#38660=ORIENTED_EDGE('',*,*,#26012,.T.);
#38661=ORIENTED_EDGE('',*,*,#28582,.T.);
#38662=ORIENTED_EDGE('',*,*,#28569,.F.);
#38663=ORIENTED_EDGE('',*,*,#28584,.F.);
#38664=ORIENTED_EDGE('',*,*,#26013,.T.);
#38665=ORIENTED_EDGE('',*,*,#28583,.T.);
#38666=ORIENTED_EDGE('',*,*,#28568,.F.);
#38667=ORIENTED_EDGE('',*,*,#28585,.F.);
#38668=ORIENTED_EDGE('',*,*,#26014,.T.);
#38669=ORIENTED_EDGE('',*,*,#28584,.T.);
#38670=ORIENTED_EDGE('',*,*,#28567,.F.);
#38671=ORIENTED_EDGE('',*,*,#28586,.F.);
#38672=ORIENTED_EDGE('',*,*,#26015,.T.);
#38673=ORIENTED_EDGE('',*,*,#28585,.T.);
#38674=ORIENTED_EDGE('',*,*,#28566,.F.);
#38675=ORIENTED_EDGE('',*,*,#28587,.F.);
#38676=ORIENTED_EDGE('',*,*,#26016,.T.);
#38677=ORIENTED_EDGE('',*,*,#28586,.T.);
#38678=ORIENTED_EDGE('',*,*,#28565,.F.);
#38679=ORIENTED_EDGE('',*,*,#28588,.F.);
#38680=ORIENTED_EDGE('',*,*,#26017,.T.);
#38681=ORIENTED_EDGE('',*,*,#28587,.T.);
#38682=ORIENTED_EDGE('',*,*,#28564,.F.);
#38683=ORIENTED_EDGE('',*,*,#28589,.F.);
#38684=ORIENTED_EDGE('',*,*,#26018,.T.);
#38685=ORIENTED_EDGE('',*,*,#28588,.T.);
#38686=ORIENTED_EDGE('',*,*,#26823,.T.);
#38687=ORIENTED_EDGE('',*,*,#26019,.T.);
#38688=ORIENTED_EDGE('',*,*,#28589,.T.);
#38689=ORIENTED_EDGE('',*,*,#28563,.F.);
#38690=ORIENTED_EDGE('',*,*,#28590,.F.);
#38691=ORIENTED_EDGE('',*,*,#27376,.T.);
#38692=ORIENTED_EDGE('',*,*,#27293,.T.);
#38693=ORIENTED_EDGE('',*,*,#28591,.F.);
#38694=ORIENTED_EDGE('',*,*,#28592,.F.);
#38695=ORIENTED_EDGE('',*,*,#26022,.T.);
#38696=ORIENTED_EDGE('',*,*,#26948,.T.);
#38697=ORIENTED_EDGE('',*,*,#28593,.F.);
#38698=ORIENTED_EDGE('',*,*,#28594,.F.);
#38699=ORIENTED_EDGE('',*,*,#26023,.T.);
#38700=ORIENTED_EDGE('',*,*,#28592,.T.);
#38701=ORIENTED_EDGE('',*,*,#28595,.F.);
#38702=ORIENTED_EDGE('',*,*,#28596,.F.);
#38703=ORIENTED_EDGE('',*,*,#26024,.T.);
#38704=ORIENTED_EDGE('',*,*,#28594,.T.);
#38705=ORIENTED_EDGE('',*,*,#28597,.F.);
#38706=ORIENTED_EDGE('',*,*,#28598,.F.);
#38707=ORIENTED_EDGE('',*,*,#26025,.T.);
#38708=ORIENTED_EDGE('',*,*,#28596,.T.);
#38709=ORIENTED_EDGE('',*,*,#28599,.F.);
#38710=ORIENTED_EDGE('',*,*,#28600,.F.);
#38711=ORIENTED_EDGE('',*,*,#26026,.T.);
#38712=ORIENTED_EDGE('',*,*,#28598,.T.);
#38713=ORIENTED_EDGE('',*,*,#28601,.F.);
#38714=ORIENTED_EDGE('',*,*,#28602,.F.);
#38715=ORIENTED_EDGE('',*,*,#26027,.T.);
#38716=ORIENTED_EDGE('',*,*,#28600,.T.);
#38717=ORIENTED_EDGE('',*,*,#28603,.F.);
#38718=ORIENTED_EDGE('',*,*,#28604,.F.);
#38719=ORIENTED_EDGE('',*,*,#26028,.T.);
#38720=ORIENTED_EDGE('',*,*,#28602,.T.);
#38721=ORIENTED_EDGE('',*,*,#28605,.F.);
#38722=ORIENTED_EDGE('',*,*,#28606,.F.);
#38723=ORIENTED_EDGE('',*,*,#26029,.T.);
#38724=ORIENTED_EDGE('',*,*,#28604,.T.);
#38725=ORIENTED_EDGE('',*,*,#28607,.F.);
#38726=ORIENTED_EDGE('',*,*,#28608,.F.);
#38727=ORIENTED_EDGE('',*,*,#26030,.T.);
#38728=ORIENTED_EDGE('',*,*,#28606,.T.);
#38729=ORIENTED_EDGE('',*,*,#28609,.F.);
#38730=ORIENTED_EDGE('',*,*,#28610,.F.);
#38731=ORIENTED_EDGE('',*,*,#26031,.T.);
#38732=ORIENTED_EDGE('',*,*,#28608,.T.);
#38733=ORIENTED_EDGE('',*,*,#28611,.F.);
#38734=ORIENTED_EDGE('',*,*,#28612,.F.);
#38735=ORIENTED_EDGE('',*,*,#26032,.T.);
#38736=ORIENTED_EDGE('',*,*,#28610,.T.);
#38737=ORIENTED_EDGE('',*,*,#28613,.F.);
#38738=ORIENTED_EDGE('',*,*,#28614,.F.);
#38739=ORIENTED_EDGE('',*,*,#26033,.T.);
#38740=ORIENTED_EDGE('',*,*,#28612,.T.);
#38741=ORIENTED_EDGE('',*,*,#28615,.F.);
#38742=ORIENTED_EDGE('',*,*,#27201,.F.);
#38743=ORIENTED_EDGE('',*,*,#26034,.T.);
#38744=ORIENTED_EDGE('',*,*,#28614,.T.);
#38745=ORIENTED_EDGE('',*,*,#27080,.T.);
#38746=ORIENTED_EDGE('',*,*,#27204,.F.);
#38747=ORIENTED_EDGE('',*,*,#27470,.F.);
#38748=ORIENTED_EDGE('',*,*,#26037,.F.);
#38749=ORIENTED_EDGE('',*,*,#27202,.T.);
#38750=ORIENTED_EDGE('',*,*,#28615,.T.);
#38751=ORIENTED_EDGE('',*,*,#28613,.T.);
#38752=ORIENTED_EDGE('',*,*,#28611,.T.);
#38753=ORIENTED_EDGE('',*,*,#28609,.T.);
#38754=ORIENTED_EDGE('',*,*,#28607,.T.);
#38755=ORIENTED_EDGE('',*,*,#28605,.T.);
#38756=ORIENTED_EDGE('',*,*,#28603,.T.);
#38757=ORIENTED_EDGE('',*,*,#28601,.T.);
#38758=ORIENTED_EDGE('',*,*,#28599,.T.);
#38759=ORIENTED_EDGE('',*,*,#28597,.T.);
#38760=ORIENTED_EDGE('',*,*,#28595,.T.);
#38761=ORIENTED_EDGE('',*,*,#28593,.T.);
#38762=ORIENTED_EDGE('',*,*,#28591,.T.);
#38763=ORIENTED_EDGE('',*,*,#26947,.T.);
#38764=ORIENTED_EDGE('',*,*,#28616,.F.);
#38765=ORIENTED_EDGE('',*,*,#28617,.T.);
#38766=ORIENTED_EDGE('',*,*,#28618,.T.);
#38767=ORIENTED_EDGE('',*,*,#28619,.T.);
#38768=ORIENTED_EDGE('',*,*,#28620,.T.);
#38769=ORIENTED_EDGE('',*,*,#28621,.T.);
#38770=ORIENTED_EDGE('',*,*,#28622,.T.);
#38771=ORIENTED_EDGE('',*,*,#28623,.T.);
#38772=ORIENTED_EDGE('',*,*,#28624,.T.);
#38773=ORIENTED_EDGE('',*,*,#28625,.T.);
#38774=ORIENTED_EDGE('',*,*,#28626,.T.);
#38775=ORIENTED_EDGE('',*,*,#28627,.T.);
#38776=ORIENTED_EDGE('',*,*,#28628,.T.);
#38777=ORIENTED_EDGE('',*,*,#28629,.T.);
#38778=ORIENTED_EDGE('',*,*,#28630,.T.);
#38779=ORIENTED_EDGE('',*,*,#26003,.T.);
#38780=ORIENTED_EDGE('',*,*,#27471,.T.);
#38781=ORIENTED_EDGE('',*,*,#28630,.F.);
#38782=ORIENTED_EDGE('',*,*,#28631,.F.);
#38783=ORIENTED_EDGE('',*,*,#25970,.T.);
#38784=ORIENTED_EDGE('',*,*,#26004,.T.);
#38785=ORIENTED_EDGE('',*,*,#28629,.F.);
#38786=ORIENTED_EDGE('',*,*,#28632,.F.);
#38787=ORIENTED_EDGE('',*,*,#25971,.T.);
#38788=ORIENTED_EDGE('',*,*,#28631,.T.);
#38789=ORIENTED_EDGE('',*,*,#28628,.F.);
#38790=ORIENTED_EDGE('',*,*,#28633,.F.);
#38791=ORIENTED_EDGE('',*,*,#25972,.T.);
#38792=ORIENTED_EDGE('',*,*,#28632,.T.);
#38793=ORIENTED_EDGE('',*,*,#28627,.F.);
#38794=ORIENTED_EDGE('',*,*,#28634,.F.);
#38795=ORIENTED_EDGE('',*,*,#25973,.T.);
#38796=ORIENTED_EDGE('',*,*,#28633,.T.);
#38797=ORIENTED_EDGE('',*,*,#28626,.F.);
#38798=ORIENTED_EDGE('',*,*,#28635,.F.);
#38799=ORIENTED_EDGE('',*,*,#25974,.T.);
#38800=ORIENTED_EDGE('',*,*,#28634,.T.);
#38801=ORIENTED_EDGE('',*,*,#28625,.F.);
#38802=ORIENTED_EDGE('',*,*,#28636,.F.);
#38803=ORIENTED_EDGE('',*,*,#25975,.T.);
#38804=ORIENTED_EDGE('',*,*,#28635,.T.);
#38805=ORIENTED_EDGE('',*,*,#28624,.F.);
#38806=ORIENTED_EDGE('',*,*,#28637,.F.);
#38807=ORIENTED_EDGE('',*,*,#25976,.T.);
#38808=ORIENTED_EDGE('',*,*,#28636,.T.);
#38809=ORIENTED_EDGE('',*,*,#28623,.F.);
#38810=ORIENTED_EDGE('',*,*,#28638,.F.);
#38811=ORIENTED_EDGE('',*,*,#25977,.T.);
#38812=ORIENTED_EDGE('',*,*,#28637,.T.);
#38813=ORIENTED_EDGE('',*,*,#28622,.F.);
#38814=ORIENTED_EDGE('',*,*,#28639,.F.);
#38815=ORIENTED_EDGE('',*,*,#25978,.T.);
#38816=ORIENTED_EDGE('',*,*,#28638,.T.);
#38817=ORIENTED_EDGE('',*,*,#28621,.F.);
#38818=ORIENTED_EDGE('',*,*,#28640,.F.);
#38819=ORIENTED_EDGE('',*,*,#25979,.T.);
#38820=ORIENTED_EDGE('',*,*,#28639,.T.);
#38821=ORIENTED_EDGE('',*,*,#28620,.F.);
#38822=ORIENTED_EDGE('',*,*,#28641,.F.);
#38823=ORIENTED_EDGE('',*,*,#25980,.T.);
#38824=ORIENTED_EDGE('',*,*,#28640,.T.);
#38825=ORIENTED_EDGE('',*,*,#28619,.F.);
#38826=ORIENTED_EDGE('',*,*,#28642,.F.);
#38827=ORIENTED_EDGE('',*,*,#25981,.T.);
#38828=ORIENTED_EDGE('',*,*,#28641,.T.);
#38829=ORIENTED_EDGE('',*,*,#28618,.F.);
#38830=ORIENTED_EDGE('',*,*,#28643,.F.);
#38831=ORIENTED_EDGE('',*,*,#25982,.T.);
#38832=ORIENTED_EDGE('',*,*,#28642,.T.);
#38833=ORIENTED_EDGE('',*,*,#26826,.T.);
#38834=ORIENTED_EDGE('',*,*,#25983,.T.);
#38835=ORIENTED_EDGE('',*,*,#28643,.T.);
#38836=ORIENTED_EDGE('',*,*,#28617,.F.);
#38837=ORIENTED_EDGE('',*,*,#28644,.F.);
#38838=ORIENTED_EDGE('',*,*,#27378,.T.);
#38839=ORIENTED_EDGE('',*,*,#27291,.T.);
#38840=ORIENTED_EDGE('',*,*,#28645,.F.);
#38841=ORIENTED_EDGE('',*,*,#28646,.F.);
#38842=ORIENTED_EDGE('',*,*,#25986,.T.);
#38843=ORIENTED_EDGE('',*,*,#26943,.T.);
#38844=ORIENTED_EDGE('',*,*,#28647,.F.);
#38845=ORIENTED_EDGE('',*,*,#28648,.F.);
#38846=ORIENTED_EDGE('',*,*,#25987,.T.);
#38847=ORIENTED_EDGE('',*,*,#28646,.T.);
#38848=ORIENTED_EDGE('',*,*,#28649,.F.);
#38849=ORIENTED_EDGE('',*,*,#28650,.F.);
#38850=ORIENTED_EDGE('',*,*,#25988,.T.);
#38851=ORIENTED_EDGE('',*,*,#28648,.T.);
#38852=ORIENTED_EDGE('',*,*,#28651,.F.);
#38853=ORIENTED_EDGE('',*,*,#28652,.F.);
#38854=ORIENTED_EDGE('',*,*,#25989,.T.);
#38855=ORIENTED_EDGE('',*,*,#28650,.T.);
#38856=ORIENTED_EDGE('',*,*,#28653,.F.);
#38857=ORIENTED_EDGE('',*,*,#28654,.F.);
#38858=ORIENTED_EDGE('',*,*,#25990,.T.);
#38859=ORIENTED_EDGE('',*,*,#28652,.T.);
#38860=ORIENTED_EDGE('',*,*,#28655,.F.);
#38861=ORIENTED_EDGE('',*,*,#28656,.F.);
#38862=ORIENTED_EDGE('',*,*,#25991,.T.);
#38863=ORIENTED_EDGE('',*,*,#28654,.T.);
#38864=ORIENTED_EDGE('',*,*,#28657,.F.);
#38865=ORIENTED_EDGE('',*,*,#28658,.F.);
#38866=ORIENTED_EDGE('',*,*,#25992,.T.);
#38867=ORIENTED_EDGE('',*,*,#28656,.T.);
#38868=ORIENTED_EDGE('',*,*,#28659,.F.);
#38869=ORIENTED_EDGE('',*,*,#28660,.F.);
#38870=ORIENTED_EDGE('',*,*,#25993,.T.);
#38871=ORIENTED_EDGE('',*,*,#28658,.T.);
#38872=ORIENTED_EDGE('',*,*,#28661,.F.);
#38873=ORIENTED_EDGE('',*,*,#28662,.F.);
#38874=ORIENTED_EDGE('',*,*,#25994,.T.);
#38875=ORIENTED_EDGE('',*,*,#28660,.T.);
#38876=ORIENTED_EDGE('',*,*,#28663,.F.);
#38877=ORIENTED_EDGE('',*,*,#28664,.F.);
#38878=ORIENTED_EDGE('',*,*,#25995,.T.);
#38879=ORIENTED_EDGE('',*,*,#28662,.T.);
#38880=ORIENTED_EDGE('',*,*,#28665,.F.);
#38881=ORIENTED_EDGE('',*,*,#28666,.F.);
#38882=ORIENTED_EDGE('',*,*,#25996,.T.);
#38883=ORIENTED_EDGE('',*,*,#28664,.T.);
#38884=ORIENTED_EDGE('',*,*,#28667,.F.);
#38885=ORIENTED_EDGE('',*,*,#28668,.F.);
#38886=ORIENTED_EDGE('',*,*,#25997,.T.);
#38887=ORIENTED_EDGE('',*,*,#28666,.T.);
#38888=ORIENTED_EDGE('',*,*,#28669,.F.);
#38889=ORIENTED_EDGE('',*,*,#27205,.F.);
#38890=ORIENTED_EDGE('',*,*,#25998,.T.);
#38891=ORIENTED_EDGE('',*,*,#28668,.T.);
#38892=ORIENTED_EDGE('',*,*,#27078,.T.);
#38893=ORIENTED_EDGE('',*,*,#27208,.F.);
#38894=ORIENTED_EDGE('',*,*,#27472,.F.);
#38895=ORIENTED_EDGE('',*,*,#26001,.F.);
#38896=ORIENTED_EDGE('',*,*,#27206,.T.);
#38897=ORIENTED_EDGE('',*,*,#28669,.T.);
#38898=ORIENTED_EDGE('',*,*,#28667,.T.);
#38899=ORIENTED_EDGE('',*,*,#28665,.T.);
#38900=ORIENTED_EDGE('',*,*,#28663,.T.);
#38901=ORIENTED_EDGE('',*,*,#28661,.T.);
#38902=ORIENTED_EDGE('',*,*,#28659,.T.);
#38903=ORIENTED_EDGE('',*,*,#28657,.T.);
#38904=ORIENTED_EDGE('',*,*,#28655,.T.);
#38905=ORIENTED_EDGE('',*,*,#28653,.T.);
#38906=ORIENTED_EDGE('',*,*,#28651,.T.);
#38907=ORIENTED_EDGE('',*,*,#28649,.T.);
#38908=ORIENTED_EDGE('',*,*,#28647,.T.);
#38909=ORIENTED_EDGE('',*,*,#28645,.T.);
#38910=ORIENTED_EDGE('',*,*,#26942,.T.);
#38911=ORIENTED_EDGE('',*,*,#28670,.F.);
#38912=ORIENTED_EDGE('',*,*,#28671,.T.);
#38913=ORIENTED_EDGE('',*,*,#28672,.T.);
#38914=ORIENTED_EDGE('',*,*,#28673,.T.);
#38915=ORIENTED_EDGE('',*,*,#28674,.T.);
#38916=ORIENTED_EDGE('',*,*,#28675,.T.);
#38917=ORIENTED_EDGE('',*,*,#28676,.T.);
#38918=ORIENTED_EDGE('',*,*,#28677,.T.);
#38919=ORIENTED_EDGE('',*,*,#28678,.T.);
#38920=ORIENTED_EDGE('',*,*,#28679,.T.);
#38921=ORIENTED_EDGE('',*,*,#28680,.T.);
#38922=ORIENTED_EDGE('',*,*,#28681,.T.);
#38923=ORIENTED_EDGE('',*,*,#28682,.T.);
#38924=ORIENTED_EDGE('',*,*,#28683,.T.);
#38925=ORIENTED_EDGE('',*,*,#28684,.T.);
#38926=ORIENTED_EDGE('',*,*,#25967,.T.);
#38927=ORIENTED_EDGE('',*,*,#27473,.T.);
#38928=ORIENTED_EDGE('',*,*,#28684,.F.);
#38929=ORIENTED_EDGE('',*,*,#28685,.F.);
#38930=ORIENTED_EDGE('',*,*,#25934,.T.);
#38931=ORIENTED_EDGE('',*,*,#25968,.T.);
#38932=ORIENTED_EDGE('',*,*,#28683,.F.);
#38933=ORIENTED_EDGE('',*,*,#28686,.F.);
#38934=ORIENTED_EDGE('',*,*,#25935,.T.);
#38935=ORIENTED_EDGE('',*,*,#28685,.T.);
#38936=ORIENTED_EDGE('',*,*,#28682,.F.);
#38937=ORIENTED_EDGE('',*,*,#28687,.F.);
#38938=ORIENTED_EDGE('',*,*,#25936,.T.);
#38939=ORIENTED_EDGE('',*,*,#28686,.T.);
#38940=ORIENTED_EDGE('',*,*,#28681,.F.);
#38941=ORIENTED_EDGE('',*,*,#28688,.F.);
#38942=ORIENTED_EDGE('',*,*,#25937,.T.);
#38943=ORIENTED_EDGE('',*,*,#28687,.T.);
#38944=ORIENTED_EDGE('',*,*,#28680,.F.);
#38945=ORIENTED_EDGE('',*,*,#28689,.F.);
#38946=ORIENTED_EDGE('',*,*,#25938,.T.);
#38947=ORIENTED_EDGE('',*,*,#28688,.T.);
#38948=ORIENTED_EDGE('',*,*,#28679,.F.);
#38949=ORIENTED_EDGE('',*,*,#28690,.F.);
#38950=ORIENTED_EDGE('',*,*,#25939,.T.);
#38951=ORIENTED_EDGE('',*,*,#28689,.T.);
#38952=ORIENTED_EDGE('',*,*,#28678,.F.);
#38953=ORIENTED_EDGE('',*,*,#28691,.F.);
#38954=ORIENTED_EDGE('',*,*,#25940,.T.);
#38955=ORIENTED_EDGE('',*,*,#28690,.T.);
#38956=ORIENTED_EDGE('',*,*,#28677,.F.);
#38957=ORIENTED_EDGE('',*,*,#28692,.F.);
#38958=ORIENTED_EDGE('',*,*,#25941,.T.);
#38959=ORIENTED_EDGE('',*,*,#28691,.T.);
#38960=ORIENTED_EDGE('',*,*,#28676,.F.);
#38961=ORIENTED_EDGE('',*,*,#28693,.F.);
#38962=ORIENTED_EDGE('',*,*,#25942,.T.);
#38963=ORIENTED_EDGE('',*,*,#28692,.T.);
#38964=ORIENTED_EDGE('',*,*,#28675,.F.);
#38965=ORIENTED_EDGE('',*,*,#28694,.F.);
#38966=ORIENTED_EDGE('',*,*,#25943,.T.);
#38967=ORIENTED_EDGE('',*,*,#28693,.T.);
#38968=ORIENTED_EDGE('',*,*,#28674,.F.);
#38969=ORIENTED_EDGE('',*,*,#28695,.F.);
#38970=ORIENTED_EDGE('',*,*,#25944,.T.);
#38971=ORIENTED_EDGE('',*,*,#28694,.T.);
#38972=ORIENTED_EDGE('',*,*,#28673,.F.);
#38973=ORIENTED_EDGE('',*,*,#28696,.F.);
#38974=ORIENTED_EDGE('',*,*,#25945,.T.);
#38975=ORIENTED_EDGE('',*,*,#28695,.T.);
#38976=ORIENTED_EDGE('',*,*,#28672,.F.);
#38977=ORIENTED_EDGE('',*,*,#28697,.F.);
#38978=ORIENTED_EDGE('',*,*,#25946,.T.);
#38979=ORIENTED_EDGE('',*,*,#28696,.T.);
#38980=ORIENTED_EDGE('',*,*,#26829,.T.);
#38981=ORIENTED_EDGE('',*,*,#25947,.T.);
#38982=ORIENTED_EDGE('',*,*,#28697,.T.);
#38983=ORIENTED_EDGE('',*,*,#28671,.F.);
#38984=ORIENTED_EDGE('',*,*,#28698,.F.);
#38985=ORIENTED_EDGE('',*,*,#27380,.T.);
#38986=ORIENTED_EDGE('',*,*,#27289,.T.);
#38987=ORIENTED_EDGE('',*,*,#28699,.F.);
#38988=ORIENTED_EDGE('',*,*,#28700,.F.);
#38989=ORIENTED_EDGE('',*,*,#25950,.T.);
#38990=ORIENTED_EDGE('',*,*,#26938,.T.);
#38991=ORIENTED_EDGE('',*,*,#28701,.F.);
#38992=ORIENTED_EDGE('',*,*,#28702,.F.);
#38993=ORIENTED_EDGE('',*,*,#25951,.T.);
#38994=ORIENTED_EDGE('',*,*,#28700,.T.);
#38995=ORIENTED_EDGE('',*,*,#28703,.F.);
#38996=ORIENTED_EDGE('',*,*,#28704,.F.);
#38997=ORIENTED_EDGE('',*,*,#25952,.T.);
#38998=ORIENTED_EDGE('',*,*,#28702,.T.);
#38999=ORIENTED_EDGE('',*,*,#28705,.F.);
#39000=ORIENTED_EDGE('',*,*,#28706,.F.);
#39001=ORIENTED_EDGE('',*,*,#25953,.T.);
#39002=ORIENTED_EDGE('',*,*,#28704,.T.);
#39003=ORIENTED_EDGE('',*,*,#28707,.F.);
#39004=ORIENTED_EDGE('',*,*,#28708,.F.);
#39005=ORIENTED_EDGE('',*,*,#25954,.T.);
#39006=ORIENTED_EDGE('',*,*,#28706,.T.);
#39007=ORIENTED_EDGE('',*,*,#28709,.F.);
#39008=ORIENTED_EDGE('',*,*,#28710,.F.);
#39009=ORIENTED_EDGE('',*,*,#25955,.T.);
#39010=ORIENTED_EDGE('',*,*,#28708,.T.);
#39011=ORIENTED_EDGE('',*,*,#28711,.F.);
#39012=ORIENTED_EDGE('',*,*,#28712,.F.);
#39013=ORIENTED_EDGE('',*,*,#25956,.T.);
#39014=ORIENTED_EDGE('',*,*,#28710,.T.);
#39015=ORIENTED_EDGE('',*,*,#28713,.F.);
#39016=ORIENTED_EDGE('',*,*,#28714,.F.);
#39017=ORIENTED_EDGE('',*,*,#25957,.T.);
#39018=ORIENTED_EDGE('',*,*,#28712,.T.);
#39019=ORIENTED_EDGE('',*,*,#28715,.F.);
#39020=ORIENTED_EDGE('',*,*,#28716,.F.);
#39021=ORIENTED_EDGE('',*,*,#25958,.T.);
#39022=ORIENTED_EDGE('',*,*,#28714,.T.);
#39023=ORIENTED_EDGE('',*,*,#28717,.F.);
#39024=ORIENTED_EDGE('',*,*,#28718,.F.);
#39025=ORIENTED_EDGE('',*,*,#25959,.T.);
#39026=ORIENTED_EDGE('',*,*,#28716,.T.);
#39027=ORIENTED_EDGE('',*,*,#28719,.F.);
#39028=ORIENTED_EDGE('',*,*,#28720,.F.);
#39029=ORIENTED_EDGE('',*,*,#25960,.T.);
#39030=ORIENTED_EDGE('',*,*,#28718,.T.);
#39031=ORIENTED_EDGE('',*,*,#28721,.F.);
#39032=ORIENTED_EDGE('',*,*,#28722,.F.);
#39033=ORIENTED_EDGE('',*,*,#25961,.T.);
#39034=ORIENTED_EDGE('',*,*,#28720,.T.);
#39035=ORIENTED_EDGE('',*,*,#28723,.F.);
#39036=ORIENTED_EDGE('',*,*,#27209,.F.);
#39037=ORIENTED_EDGE('',*,*,#25962,.T.);
#39038=ORIENTED_EDGE('',*,*,#28722,.T.);
#39039=ORIENTED_EDGE('',*,*,#27076,.T.);
#39040=ORIENTED_EDGE('',*,*,#27212,.F.);
#39041=ORIENTED_EDGE('',*,*,#27474,.F.);
#39042=ORIENTED_EDGE('',*,*,#25965,.F.);
#39043=ORIENTED_EDGE('',*,*,#27210,.T.);
#39044=ORIENTED_EDGE('',*,*,#28723,.T.);
#39045=ORIENTED_EDGE('',*,*,#28721,.T.);
#39046=ORIENTED_EDGE('',*,*,#28719,.T.);
#39047=ORIENTED_EDGE('',*,*,#28717,.T.);
#39048=ORIENTED_EDGE('',*,*,#28715,.T.);
#39049=ORIENTED_EDGE('',*,*,#28713,.T.);
#39050=ORIENTED_EDGE('',*,*,#28711,.T.);
#39051=ORIENTED_EDGE('',*,*,#28709,.T.);
#39052=ORIENTED_EDGE('',*,*,#28707,.T.);
#39053=ORIENTED_EDGE('',*,*,#28705,.T.);
#39054=ORIENTED_EDGE('',*,*,#28703,.T.);
#39055=ORIENTED_EDGE('',*,*,#28701,.T.);
#39056=ORIENTED_EDGE('',*,*,#28699,.T.);
#39057=ORIENTED_EDGE('',*,*,#26937,.T.);
#39058=ORIENTED_EDGE('',*,*,#28724,.F.);
#39059=ORIENTED_EDGE('',*,*,#28725,.T.);
#39060=ORIENTED_EDGE('',*,*,#28726,.T.);
#39061=ORIENTED_EDGE('',*,*,#28727,.T.);
#39062=ORIENTED_EDGE('',*,*,#28728,.T.);
#39063=ORIENTED_EDGE('',*,*,#28729,.T.);
#39064=ORIENTED_EDGE('',*,*,#28730,.T.);
#39065=ORIENTED_EDGE('',*,*,#28731,.T.);
#39066=ORIENTED_EDGE('',*,*,#28732,.T.);
#39067=ORIENTED_EDGE('',*,*,#28733,.T.);
#39068=ORIENTED_EDGE('',*,*,#28734,.T.);
#39069=ORIENTED_EDGE('',*,*,#28735,.T.);
#39070=ORIENTED_EDGE('',*,*,#28736,.T.);
#39071=ORIENTED_EDGE('',*,*,#28737,.T.);
#39072=ORIENTED_EDGE('',*,*,#28738,.T.);
#39073=ORIENTED_EDGE('',*,*,#25931,.T.);
#39074=ORIENTED_EDGE('',*,*,#27475,.T.);
#39075=ORIENTED_EDGE('',*,*,#28738,.F.);
#39076=ORIENTED_EDGE('',*,*,#28739,.F.);
#39077=ORIENTED_EDGE('',*,*,#25898,.T.);
#39078=ORIENTED_EDGE('',*,*,#25932,.T.);
#39079=ORIENTED_EDGE('',*,*,#28737,.F.);
#39080=ORIENTED_EDGE('',*,*,#28740,.F.);
#39081=ORIENTED_EDGE('',*,*,#25899,.T.);
#39082=ORIENTED_EDGE('',*,*,#28739,.T.);
#39083=ORIENTED_EDGE('',*,*,#28736,.F.);
#39084=ORIENTED_EDGE('',*,*,#28741,.F.);
#39085=ORIENTED_EDGE('',*,*,#25900,.T.);
#39086=ORIENTED_EDGE('',*,*,#28740,.T.);
#39087=ORIENTED_EDGE('',*,*,#28735,.F.);
#39088=ORIENTED_EDGE('',*,*,#28742,.F.);
#39089=ORIENTED_EDGE('',*,*,#25901,.T.);
#39090=ORIENTED_EDGE('',*,*,#28741,.T.);
#39091=ORIENTED_EDGE('',*,*,#28734,.F.);
#39092=ORIENTED_EDGE('',*,*,#28743,.F.);
#39093=ORIENTED_EDGE('',*,*,#25902,.T.);
#39094=ORIENTED_EDGE('',*,*,#28742,.T.);
#39095=ORIENTED_EDGE('',*,*,#28733,.F.);
#39096=ORIENTED_EDGE('',*,*,#28744,.F.);
#39097=ORIENTED_EDGE('',*,*,#25903,.T.);
#39098=ORIENTED_EDGE('',*,*,#28743,.T.);
#39099=ORIENTED_EDGE('',*,*,#28732,.F.);
#39100=ORIENTED_EDGE('',*,*,#28745,.F.);
#39101=ORIENTED_EDGE('',*,*,#25904,.T.);
#39102=ORIENTED_EDGE('',*,*,#28744,.T.);
#39103=ORIENTED_EDGE('',*,*,#28731,.F.);
#39104=ORIENTED_EDGE('',*,*,#28746,.F.);
#39105=ORIENTED_EDGE('',*,*,#25905,.T.);
#39106=ORIENTED_EDGE('',*,*,#28745,.T.);
#39107=ORIENTED_EDGE('',*,*,#28730,.F.);
#39108=ORIENTED_EDGE('',*,*,#28747,.F.);
#39109=ORIENTED_EDGE('',*,*,#25906,.T.);
#39110=ORIENTED_EDGE('',*,*,#28746,.T.);
#39111=ORIENTED_EDGE('',*,*,#28729,.F.);
#39112=ORIENTED_EDGE('',*,*,#28748,.F.);
#39113=ORIENTED_EDGE('',*,*,#25907,.T.);
#39114=ORIENTED_EDGE('',*,*,#28747,.T.);
#39115=ORIENTED_EDGE('',*,*,#28728,.F.);
#39116=ORIENTED_EDGE('',*,*,#28749,.F.);
#39117=ORIENTED_EDGE('',*,*,#25908,.T.);
#39118=ORIENTED_EDGE('',*,*,#28748,.T.);
#39119=ORIENTED_EDGE('',*,*,#28727,.F.);
#39120=ORIENTED_EDGE('',*,*,#28750,.F.);
#39121=ORIENTED_EDGE('',*,*,#25909,.T.);
#39122=ORIENTED_EDGE('',*,*,#28749,.T.);
#39123=ORIENTED_EDGE('',*,*,#28726,.F.);
#39124=ORIENTED_EDGE('',*,*,#28751,.F.);
#39125=ORIENTED_EDGE('',*,*,#25910,.T.);
#39126=ORIENTED_EDGE('',*,*,#28750,.T.);
#39127=ORIENTED_EDGE('',*,*,#26832,.T.);
#39128=ORIENTED_EDGE('',*,*,#25911,.T.);
#39129=ORIENTED_EDGE('',*,*,#28751,.T.);
#39130=ORIENTED_EDGE('',*,*,#28725,.F.);
#39131=ORIENTED_EDGE('',*,*,#28752,.F.);
#39132=ORIENTED_EDGE('',*,*,#27382,.T.);
#39133=ORIENTED_EDGE('',*,*,#27287,.T.);
#39134=ORIENTED_EDGE('',*,*,#28753,.F.);
#39135=ORIENTED_EDGE('',*,*,#28754,.F.);
#39136=ORIENTED_EDGE('',*,*,#25914,.T.);
#39137=ORIENTED_EDGE('',*,*,#26933,.T.);
#39138=ORIENTED_EDGE('',*,*,#28755,.F.);
#39139=ORIENTED_EDGE('',*,*,#28756,.F.);
#39140=ORIENTED_EDGE('',*,*,#25915,.T.);
#39141=ORIENTED_EDGE('',*,*,#28754,.T.);
#39142=ORIENTED_EDGE('',*,*,#28757,.F.);
#39143=ORIENTED_EDGE('',*,*,#28758,.F.);
#39144=ORIENTED_EDGE('',*,*,#25916,.T.);
#39145=ORIENTED_EDGE('',*,*,#28756,.T.);
#39146=ORIENTED_EDGE('',*,*,#28759,.F.);
#39147=ORIENTED_EDGE('',*,*,#28760,.F.);
#39148=ORIENTED_EDGE('',*,*,#25917,.T.);
#39149=ORIENTED_EDGE('',*,*,#28758,.T.);
#39150=ORIENTED_EDGE('',*,*,#28761,.F.);
#39151=ORIENTED_EDGE('',*,*,#28762,.F.);
#39152=ORIENTED_EDGE('',*,*,#25918,.T.);
#39153=ORIENTED_EDGE('',*,*,#28760,.T.);
#39154=ORIENTED_EDGE('',*,*,#28763,.F.);
#39155=ORIENTED_EDGE('',*,*,#28764,.F.);
#39156=ORIENTED_EDGE('',*,*,#25919,.T.);
#39157=ORIENTED_EDGE('',*,*,#28762,.T.);
#39158=ORIENTED_EDGE('',*,*,#28765,.F.);
#39159=ORIENTED_EDGE('',*,*,#28766,.F.);
#39160=ORIENTED_EDGE('',*,*,#25920,.T.);
#39161=ORIENTED_EDGE('',*,*,#28764,.T.);
#39162=ORIENTED_EDGE('',*,*,#28767,.F.);
#39163=ORIENTED_EDGE('',*,*,#28768,.F.);
#39164=ORIENTED_EDGE('',*,*,#25921,.T.);
#39165=ORIENTED_EDGE('',*,*,#28766,.T.);
#39166=ORIENTED_EDGE('',*,*,#28769,.F.);
#39167=ORIENTED_EDGE('',*,*,#28770,.F.);
#39168=ORIENTED_EDGE('',*,*,#25922,.T.);
#39169=ORIENTED_EDGE('',*,*,#28768,.T.);
#39170=ORIENTED_EDGE('',*,*,#28771,.F.);
#39171=ORIENTED_EDGE('',*,*,#28772,.F.);
#39172=ORIENTED_EDGE('',*,*,#25923,.T.);
#39173=ORIENTED_EDGE('',*,*,#28770,.T.);
#39174=ORIENTED_EDGE('',*,*,#28773,.F.);
#39175=ORIENTED_EDGE('',*,*,#28774,.F.);
#39176=ORIENTED_EDGE('',*,*,#25924,.T.);
#39177=ORIENTED_EDGE('',*,*,#28772,.T.);
#39178=ORIENTED_EDGE('',*,*,#28775,.F.);
#39179=ORIENTED_EDGE('',*,*,#28776,.F.);
#39180=ORIENTED_EDGE('',*,*,#25925,.T.);
#39181=ORIENTED_EDGE('',*,*,#28774,.T.);
#39182=ORIENTED_EDGE('',*,*,#28777,.F.);
#39183=ORIENTED_EDGE('',*,*,#27213,.F.);
#39184=ORIENTED_EDGE('',*,*,#25926,.T.);
#39185=ORIENTED_EDGE('',*,*,#28776,.T.);
#39186=ORIENTED_EDGE('',*,*,#27074,.T.);
#39187=ORIENTED_EDGE('',*,*,#27216,.F.);
#39188=ORIENTED_EDGE('',*,*,#27476,.F.);
#39189=ORIENTED_EDGE('',*,*,#25929,.F.);
#39190=ORIENTED_EDGE('',*,*,#27214,.T.);
#39191=ORIENTED_EDGE('',*,*,#28777,.T.);
#39192=ORIENTED_EDGE('',*,*,#28775,.T.);
#39193=ORIENTED_EDGE('',*,*,#28773,.T.);
#39194=ORIENTED_EDGE('',*,*,#28771,.T.);
#39195=ORIENTED_EDGE('',*,*,#28769,.T.);
#39196=ORIENTED_EDGE('',*,*,#28767,.T.);
#39197=ORIENTED_EDGE('',*,*,#28765,.T.);
#39198=ORIENTED_EDGE('',*,*,#28763,.T.);
#39199=ORIENTED_EDGE('',*,*,#28761,.T.);
#39200=ORIENTED_EDGE('',*,*,#28759,.T.);
#39201=ORIENTED_EDGE('',*,*,#28757,.T.);
#39202=ORIENTED_EDGE('',*,*,#28755,.T.);
#39203=ORIENTED_EDGE('',*,*,#28753,.T.);
#39204=ORIENTED_EDGE('',*,*,#26932,.T.);
#39205=ORIENTED_EDGE('',*,*,#28778,.F.);
#39206=ORIENTED_EDGE('',*,*,#28779,.T.);
#39207=ORIENTED_EDGE('',*,*,#28780,.T.);
#39208=ORIENTED_EDGE('',*,*,#28781,.T.);
#39209=ORIENTED_EDGE('',*,*,#28782,.T.);
#39210=ORIENTED_EDGE('',*,*,#28783,.T.);
#39211=ORIENTED_EDGE('',*,*,#28784,.T.);
#39212=ORIENTED_EDGE('',*,*,#28785,.T.);
#39213=ORIENTED_EDGE('',*,*,#28786,.T.);
#39214=ORIENTED_EDGE('',*,*,#28787,.T.);
#39215=ORIENTED_EDGE('',*,*,#28788,.T.);
#39216=ORIENTED_EDGE('',*,*,#28789,.T.);
#39217=ORIENTED_EDGE('',*,*,#28790,.T.);
#39218=ORIENTED_EDGE('',*,*,#28791,.T.);
#39219=ORIENTED_EDGE('',*,*,#28792,.T.);
#39220=ORIENTED_EDGE('',*,*,#25895,.T.);
#39221=ORIENTED_EDGE('',*,*,#27477,.T.);
#39222=ORIENTED_EDGE('',*,*,#28792,.F.);
#39223=ORIENTED_EDGE('',*,*,#28793,.F.);
#39224=ORIENTED_EDGE('',*,*,#25862,.T.);
#39225=ORIENTED_EDGE('',*,*,#25896,.T.);
#39226=ORIENTED_EDGE('',*,*,#28791,.F.);
#39227=ORIENTED_EDGE('',*,*,#28794,.F.);
#39228=ORIENTED_EDGE('',*,*,#25863,.T.);
#39229=ORIENTED_EDGE('',*,*,#28793,.T.);
#39230=ORIENTED_EDGE('',*,*,#28790,.F.);
#39231=ORIENTED_EDGE('',*,*,#28795,.F.);
#39232=ORIENTED_EDGE('',*,*,#25864,.T.);
#39233=ORIENTED_EDGE('',*,*,#28794,.T.);
#39234=ORIENTED_EDGE('',*,*,#28789,.F.);
#39235=ORIENTED_EDGE('',*,*,#28796,.F.);
#39236=ORIENTED_EDGE('',*,*,#25865,.T.);
#39237=ORIENTED_EDGE('',*,*,#28795,.T.);
#39238=ORIENTED_EDGE('',*,*,#28788,.F.);
#39239=ORIENTED_EDGE('',*,*,#28797,.F.);
#39240=ORIENTED_EDGE('',*,*,#25866,.T.);
#39241=ORIENTED_EDGE('',*,*,#28796,.T.);
#39242=ORIENTED_EDGE('',*,*,#28787,.F.);
#39243=ORIENTED_EDGE('',*,*,#28798,.F.);
#39244=ORIENTED_EDGE('',*,*,#25867,.T.);
#39245=ORIENTED_EDGE('',*,*,#28797,.T.);
#39246=ORIENTED_EDGE('',*,*,#28786,.F.);
#39247=ORIENTED_EDGE('',*,*,#28799,.F.);
#39248=ORIENTED_EDGE('',*,*,#25868,.T.);
#39249=ORIENTED_EDGE('',*,*,#28798,.T.);
#39250=ORIENTED_EDGE('',*,*,#28785,.F.);
#39251=ORIENTED_EDGE('',*,*,#28800,.F.);
#39252=ORIENTED_EDGE('',*,*,#25869,.T.);
#39253=ORIENTED_EDGE('',*,*,#28799,.T.);
#39254=ORIENTED_EDGE('',*,*,#28784,.F.);
#39255=ORIENTED_EDGE('',*,*,#28801,.F.);
#39256=ORIENTED_EDGE('',*,*,#25870,.T.);
#39257=ORIENTED_EDGE('',*,*,#28800,.T.);
#39258=ORIENTED_EDGE('',*,*,#28783,.F.);
#39259=ORIENTED_EDGE('',*,*,#28802,.F.);
#39260=ORIENTED_EDGE('',*,*,#25871,.T.);
#39261=ORIENTED_EDGE('',*,*,#28801,.T.);
#39262=ORIENTED_EDGE('',*,*,#28782,.F.);
#39263=ORIENTED_EDGE('',*,*,#28803,.F.);
#39264=ORIENTED_EDGE('',*,*,#25872,.T.);
#39265=ORIENTED_EDGE('',*,*,#28802,.T.);
#39266=ORIENTED_EDGE('',*,*,#28781,.F.);
#39267=ORIENTED_EDGE('',*,*,#28804,.F.);
#39268=ORIENTED_EDGE('',*,*,#25873,.T.);
#39269=ORIENTED_EDGE('',*,*,#28803,.T.);
#39270=ORIENTED_EDGE('',*,*,#28780,.F.);
#39271=ORIENTED_EDGE('',*,*,#28805,.F.);
#39272=ORIENTED_EDGE('',*,*,#25874,.T.);
#39273=ORIENTED_EDGE('',*,*,#28804,.T.);
#39274=ORIENTED_EDGE('',*,*,#26835,.T.);
#39275=ORIENTED_EDGE('',*,*,#25875,.T.);
#39276=ORIENTED_EDGE('',*,*,#28805,.T.);
#39277=ORIENTED_EDGE('',*,*,#28779,.F.);
#39278=ORIENTED_EDGE('',*,*,#28806,.F.);
#39279=ORIENTED_EDGE('',*,*,#27384,.T.);
#39280=ORIENTED_EDGE('',*,*,#27285,.T.);
#39281=ORIENTED_EDGE('',*,*,#28807,.F.);
#39282=ORIENTED_EDGE('',*,*,#28808,.F.);
#39283=ORIENTED_EDGE('',*,*,#25878,.T.);
#39284=ORIENTED_EDGE('',*,*,#26928,.T.);
#39285=ORIENTED_EDGE('',*,*,#28809,.F.);
#39286=ORIENTED_EDGE('',*,*,#28810,.F.);
#39287=ORIENTED_EDGE('',*,*,#25879,.T.);
#39288=ORIENTED_EDGE('',*,*,#28808,.T.);
#39289=ORIENTED_EDGE('',*,*,#28811,.F.);
#39290=ORIENTED_EDGE('',*,*,#28812,.F.);
#39291=ORIENTED_EDGE('',*,*,#25880,.T.);
#39292=ORIENTED_EDGE('',*,*,#28810,.T.);
#39293=ORIENTED_EDGE('',*,*,#28813,.F.);
#39294=ORIENTED_EDGE('',*,*,#28814,.F.);
#39295=ORIENTED_EDGE('',*,*,#25881,.T.);
#39296=ORIENTED_EDGE('',*,*,#28812,.T.);
#39297=ORIENTED_EDGE('',*,*,#28815,.F.);
#39298=ORIENTED_EDGE('',*,*,#28816,.F.);
#39299=ORIENTED_EDGE('',*,*,#25882,.T.);
#39300=ORIENTED_EDGE('',*,*,#28814,.T.);
#39301=ORIENTED_EDGE('',*,*,#28817,.F.);
#39302=ORIENTED_EDGE('',*,*,#28818,.F.);
#39303=ORIENTED_EDGE('',*,*,#25883,.T.);
#39304=ORIENTED_EDGE('',*,*,#28816,.T.);
#39305=ORIENTED_EDGE('',*,*,#28819,.F.);
#39306=ORIENTED_EDGE('',*,*,#28820,.F.);
#39307=ORIENTED_EDGE('',*,*,#25884,.T.);
#39308=ORIENTED_EDGE('',*,*,#28818,.T.);
#39309=ORIENTED_EDGE('',*,*,#28821,.F.);
#39310=ORIENTED_EDGE('',*,*,#28822,.F.);
#39311=ORIENTED_EDGE('',*,*,#25885,.T.);
#39312=ORIENTED_EDGE('',*,*,#28820,.T.);
#39313=ORIENTED_EDGE('',*,*,#28823,.F.);
#39314=ORIENTED_EDGE('',*,*,#28824,.F.);
#39315=ORIENTED_EDGE('',*,*,#25886,.T.);
#39316=ORIENTED_EDGE('',*,*,#28822,.T.);
#39317=ORIENTED_EDGE('',*,*,#28825,.F.);
#39318=ORIENTED_EDGE('',*,*,#28826,.F.);
#39319=ORIENTED_EDGE('',*,*,#25887,.T.);
#39320=ORIENTED_EDGE('',*,*,#28824,.T.);
#39321=ORIENTED_EDGE('',*,*,#28827,.F.);
#39322=ORIENTED_EDGE('',*,*,#28828,.F.);
#39323=ORIENTED_EDGE('',*,*,#25888,.T.);
#39324=ORIENTED_EDGE('',*,*,#28826,.T.);
#39325=ORIENTED_EDGE('',*,*,#28829,.F.);
#39326=ORIENTED_EDGE('',*,*,#28830,.F.);
#39327=ORIENTED_EDGE('',*,*,#25889,.T.);
#39328=ORIENTED_EDGE('',*,*,#28828,.T.);
#39329=ORIENTED_EDGE('',*,*,#28831,.F.);
#39330=ORIENTED_EDGE('',*,*,#27217,.F.);
#39331=ORIENTED_EDGE('',*,*,#25890,.T.);
#39332=ORIENTED_EDGE('',*,*,#28830,.T.);
#39333=ORIENTED_EDGE('',*,*,#27072,.T.);
#39334=ORIENTED_EDGE('',*,*,#27220,.F.);
#39335=ORIENTED_EDGE('',*,*,#27478,.F.);
#39336=ORIENTED_EDGE('',*,*,#25893,.F.);
#39337=ORIENTED_EDGE('',*,*,#27218,.T.);
#39338=ORIENTED_EDGE('',*,*,#28831,.T.);
#39339=ORIENTED_EDGE('',*,*,#28829,.T.);
#39340=ORIENTED_EDGE('',*,*,#28827,.T.);
#39341=ORIENTED_EDGE('',*,*,#28825,.T.);
#39342=ORIENTED_EDGE('',*,*,#28823,.T.);
#39343=ORIENTED_EDGE('',*,*,#28821,.T.);
#39344=ORIENTED_EDGE('',*,*,#28819,.T.);
#39345=ORIENTED_EDGE('',*,*,#28817,.T.);
#39346=ORIENTED_EDGE('',*,*,#28815,.T.);
#39347=ORIENTED_EDGE('',*,*,#28813,.T.);
#39348=ORIENTED_EDGE('',*,*,#28811,.T.);
#39349=ORIENTED_EDGE('',*,*,#28809,.T.);
#39350=ORIENTED_EDGE('',*,*,#28807,.T.);
#39351=ORIENTED_EDGE('',*,*,#26927,.T.);
#39352=ORIENTED_EDGE('',*,*,#28832,.F.);
#39353=ORIENTED_EDGE('',*,*,#28833,.T.);
#39354=ORIENTED_EDGE('',*,*,#28834,.T.);
#39355=ORIENTED_EDGE('',*,*,#28835,.T.);
#39356=ORIENTED_EDGE('',*,*,#28836,.T.);
#39357=ORIENTED_EDGE('',*,*,#28837,.T.);
#39358=ORIENTED_EDGE('',*,*,#28838,.T.);
#39359=ORIENTED_EDGE('',*,*,#28839,.T.);
#39360=ORIENTED_EDGE('',*,*,#28840,.T.);
#39361=ORIENTED_EDGE('',*,*,#28841,.T.);
#39362=ORIENTED_EDGE('',*,*,#28842,.T.);
#39363=ORIENTED_EDGE('',*,*,#28843,.T.);
#39364=ORIENTED_EDGE('',*,*,#28844,.T.);
#39365=ORIENTED_EDGE('',*,*,#28845,.T.);
#39366=ORIENTED_EDGE('',*,*,#28846,.T.);
#39367=ORIENTED_EDGE('',*,*,#25859,.T.);
#39368=ORIENTED_EDGE('',*,*,#27479,.T.);
#39369=ORIENTED_EDGE('',*,*,#28846,.F.);
#39370=ORIENTED_EDGE('',*,*,#28847,.F.);
#39371=ORIENTED_EDGE('',*,*,#25826,.T.);
#39372=ORIENTED_EDGE('',*,*,#25860,.T.);
#39373=ORIENTED_EDGE('',*,*,#28845,.F.);
#39374=ORIENTED_EDGE('',*,*,#28848,.F.);
#39375=ORIENTED_EDGE('',*,*,#25827,.T.);
#39376=ORIENTED_EDGE('',*,*,#28847,.T.);
#39377=ORIENTED_EDGE('',*,*,#28844,.F.);
#39378=ORIENTED_EDGE('',*,*,#28849,.F.);
#39379=ORIENTED_EDGE('',*,*,#25828,.T.);
#39380=ORIENTED_EDGE('',*,*,#28848,.T.);
#39381=ORIENTED_EDGE('',*,*,#28843,.F.);
#39382=ORIENTED_EDGE('',*,*,#28850,.F.);
#39383=ORIENTED_EDGE('',*,*,#25829,.T.);
#39384=ORIENTED_EDGE('',*,*,#28849,.T.);
#39385=ORIENTED_EDGE('',*,*,#28842,.F.);
#39386=ORIENTED_EDGE('',*,*,#28851,.F.);
#39387=ORIENTED_EDGE('',*,*,#25830,.T.);
#39388=ORIENTED_EDGE('',*,*,#28850,.T.);
#39389=ORIENTED_EDGE('',*,*,#28841,.F.);
#39390=ORIENTED_EDGE('',*,*,#28852,.F.);
#39391=ORIENTED_EDGE('',*,*,#25831,.T.);
#39392=ORIENTED_EDGE('',*,*,#28851,.T.);
#39393=ORIENTED_EDGE('',*,*,#28840,.F.);
#39394=ORIENTED_EDGE('',*,*,#28853,.F.);
#39395=ORIENTED_EDGE('',*,*,#25832,.T.);
#39396=ORIENTED_EDGE('',*,*,#28852,.T.);
#39397=ORIENTED_EDGE('',*,*,#28839,.F.);
#39398=ORIENTED_EDGE('',*,*,#28854,.F.);
#39399=ORIENTED_EDGE('',*,*,#25833,.T.);
#39400=ORIENTED_EDGE('',*,*,#28853,.T.);
#39401=ORIENTED_EDGE('',*,*,#28838,.F.);
#39402=ORIENTED_EDGE('',*,*,#28855,.F.);
#39403=ORIENTED_EDGE('',*,*,#25834,.T.);
#39404=ORIENTED_EDGE('',*,*,#28854,.T.);
#39405=ORIENTED_EDGE('',*,*,#28837,.F.);
#39406=ORIENTED_EDGE('',*,*,#28856,.F.);
#39407=ORIENTED_EDGE('',*,*,#25835,.T.);
#39408=ORIENTED_EDGE('',*,*,#28855,.T.);
#39409=ORIENTED_EDGE('',*,*,#28836,.F.);
#39410=ORIENTED_EDGE('',*,*,#28857,.F.);
#39411=ORIENTED_EDGE('',*,*,#25836,.T.);
#39412=ORIENTED_EDGE('',*,*,#28856,.T.);
#39413=ORIENTED_EDGE('',*,*,#28835,.F.);
#39414=ORIENTED_EDGE('',*,*,#28858,.F.);
#39415=ORIENTED_EDGE('',*,*,#25837,.T.);
#39416=ORIENTED_EDGE('',*,*,#28857,.T.);
#39417=ORIENTED_EDGE('',*,*,#28834,.F.);
#39418=ORIENTED_EDGE('',*,*,#28859,.F.);
#39419=ORIENTED_EDGE('',*,*,#25838,.T.);
#39420=ORIENTED_EDGE('',*,*,#28858,.T.);
#39421=ORIENTED_EDGE('',*,*,#26838,.T.);
#39422=ORIENTED_EDGE('',*,*,#25839,.T.);
#39423=ORIENTED_EDGE('',*,*,#28859,.T.);
#39424=ORIENTED_EDGE('',*,*,#28833,.F.);
#39425=ORIENTED_EDGE('',*,*,#28860,.F.);
#39426=ORIENTED_EDGE('',*,*,#27386,.T.);
#39427=ORIENTED_EDGE('',*,*,#27283,.T.);
#39428=ORIENTED_EDGE('',*,*,#28861,.F.);
#39429=ORIENTED_EDGE('',*,*,#28862,.F.);
#39430=ORIENTED_EDGE('',*,*,#25842,.T.);
#39431=ORIENTED_EDGE('',*,*,#26923,.T.);
#39432=ORIENTED_EDGE('',*,*,#28863,.F.);
#39433=ORIENTED_EDGE('',*,*,#28864,.F.);
#39434=ORIENTED_EDGE('',*,*,#25843,.T.);
#39435=ORIENTED_EDGE('',*,*,#28862,.T.);
#39436=ORIENTED_EDGE('',*,*,#28865,.F.);
#39437=ORIENTED_EDGE('',*,*,#28866,.F.);
#39438=ORIENTED_EDGE('',*,*,#25844,.T.);
#39439=ORIENTED_EDGE('',*,*,#28864,.T.);
#39440=ORIENTED_EDGE('',*,*,#28867,.F.);
#39441=ORIENTED_EDGE('',*,*,#28868,.F.);
#39442=ORIENTED_EDGE('',*,*,#25845,.T.);
#39443=ORIENTED_EDGE('',*,*,#28866,.T.);
#39444=ORIENTED_EDGE('',*,*,#28869,.F.);
#39445=ORIENTED_EDGE('',*,*,#28870,.F.);
#39446=ORIENTED_EDGE('',*,*,#25846,.T.);
#39447=ORIENTED_EDGE('',*,*,#28868,.T.);
#39448=ORIENTED_EDGE('',*,*,#28871,.F.);
#39449=ORIENTED_EDGE('',*,*,#28872,.F.);
#39450=ORIENTED_EDGE('',*,*,#25847,.T.);
#39451=ORIENTED_EDGE('',*,*,#28870,.T.);
#39452=ORIENTED_EDGE('',*,*,#28873,.F.);
#39453=ORIENTED_EDGE('',*,*,#28874,.F.);
#39454=ORIENTED_EDGE('',*,*,#25848,.T.);
#39455=ORIENTED_EDGE('',*,*,#28872,.T.);
#39456=ORIENTED_EDGE('',*,*,#28875,.F.);
#39457=ORIENTED_EDGE('',*,*,#28876,.F.);
#39458=ORIENTED_EDGE('',*,*,#25849,.T.);
#39459=ORIENTED_EDGE('',*,*,#28874,.T.);
#39460=ORIENTED_EDGE('',*,*,#28877,.F.);
#39461=ORIENTED_EDGE('',*,*,#28878,.F.);
#39462=ORIENTED_EDGE('',*,*,#25850,.T.);
#39463=ORIENTED_EDGE('',*,*,#28876,.T.);
#39464=ORIENTED_EDGE('',*,*,#28879,.F.);
#39465=ORIENTED_EDGE('',*,*,#28880,.F.);
#39466=ORIENTED_EDGE('',*,*,#25851,.T.);
#39467=ORIENTED_EDGE('',*,*,#28878,.T.);
#39468=ORIENTED_EDGE('',*,*,#28881,.F.);
#39469=ORIENTED_EDGE('',*,*,#28882,.F.);
#39470=ORIENTED_EDGE('',*,*,#25852,.T.);
#39471=ORIENTED_EDGE('',*,*,#28880,.T.);
#39472=ORIENTED_EDGE('',*,*,#28883,.F.);
#39473=ORIENTED_EDGE('',*,*,#28884,.F.);
#39474=ORIENTED_EDGE('',*,*,#25853,.T.);
#39475=ORIENTED_EDGE('',*,*,#28882,.T.);
#39476=ORIENTED_EDGE('',*,*,#28885,.F.);
#39477=ORIENTED_EDGE('',*,*,#27221,.F.);
#39478=ORIENTED_EDGE('',*,*,#25854,.T.);
#39479=ORIENTED_EDGE('',*,*,#28884,.T.);
#39480=ORIENTED_EDGE('',*,*,#27070,.T.);
#39481=ORIENTED_EDGE('',*,*,#27224,.F.);
#39482=ORIENTED_EDGE('',*,*,#27480,.F.);
#39483=ORIENTED_EDGE('',*,*,#25857,.F.);
#39484=ORIENTED_EDGE('',*,*,#27222,.T.);
#39485=ORIENTED_EDGE('',*,*,#28885,.T.);
#39486=ORIENTED_EDGE('',*,*,#28883,.T.);
#39487=ORIENTED_EDGE('',*,*,#28881,.T.);
#39488=ORIENTED_EDGE('',*,*,#28879,.T.);
#39489=ORIENTED_EDGE('',*,*,#28877,.T.);
#39490=ORIENTED_EDGE('',*,*,#28875,.T.);
#39491=ORIENTED_EDGE('',*,*,#28873,.T.);
#39492=ORIENTED_EDGE('',*,*,#28871,.T.);
#39493=ORIENTED_EDGE('',*,*,#28869,.T.);
#39494=ORIENTED_EDGE('',*,*,#28867,.T.);
#39495=ORIENTED_EDGE('',*,*,#28865,.T.);
#39496=ORIENTED_EDGE('',*,*,#28863,.T.);
#39497=ORIENTED_EDGE('',*,*,#28861,.T.);
#39498=ORIENTED_EDGE('',*,*,#26922,.T.);
#39499=ORIENTED_EDGE('',*,*,#28886,.F.);
#39500=ORIENTED_EDGE('',*,*,#28887,.T.);
#39501=ORIENTED_EDGE('',*,*,#28888,.T.);
#39502=ORIENTED_EDGE('',*,*,#28889,.T.);
#39503=ORIENTED_EDGE('',*,*,#28890,.T.);
#39504=ORIENTED_EDGE('',*,*,#28891,.T.);
#39505=ORIENTED_EDGE('',*,*,#28892,.T.);
#39506=ORIENTED_EDGE('',*,*,#28893,.T.);
#39507=ORIENTED_EDGE('',*,*,#28894,.T.);
#39508=ORIENTED_EDGE('',*,*,#28895,.T.);
#39509=ORIENTED_EDGE('',*,*,#28896,.T.);
#39510=ORIENTED_EDGE('',*,*,#28897,.T.);
#39511=ORIENTED_EDGE('',*,*,#28898,.T.);
#39512=ORIENTED_EDGE('',*,*,#28899,.T.);
#39513=ORIENTED_EDGE('',*,*,#28900,.T.);
#39514=ORIENTED_EDGE('',*,*,#25823,.T.);
#39515=ORIENTED_EDGE('',*,*,#27481,.T.);
#39516=ORIENTED_EDGE('',*,*,#28900,.F.);
#39517=ORIENTED_EDGE('',*,*,#28901,.F.);
#39518=ORIENTED_EDGE('',*,*,#25790,.T.);
#39519=ORIENTED_EDGE('',*,*,#25824,.T.);
#39520=ORIENTED_EDGE('',*,*,#28899,.F.);
#39521=ORIENTED_EDGE('',*,*,#28902,.F.);
#39522=ORIENTED_EDGE('',*,*,#25791,.T.);
#39523=ORIENTED_EDGE('',*,*,#28901,.T.);
#39524=ORIENTED_EDGE('',*,*,#28898,.F.);
#39525=ORIENTED_EDGE('',*,*,#28903,.F.);
#39526=ORIENTED_EDGE('',*,*,#25792,.T.);
#39527=ORIENTED_EDGE('',*,*,#28902,.T.);
#39528=ORIENTED_EDGE('',*,*,#28897,.F.);
#39529=ORIENTED_EDGE('',*,*,#28904,.F.);
#39530=ORIENTED_EDGE('',*,*,#25793,.T.);
#39531=ORIENTED_EDGE('',*,*,#28903,.T.);
#39532=ORIENTED_EDGE('',*,*,#28896,.F.);
#39533=ORIENTED_EDGE('',*,*,#28905,.F.);
#39534=ORIENTED_EDGE('',*,*,#25794,.T.);
#39535=ORIENTED_EDGE('',*,*,#28904,.T.);
#39536=ORIENTED_EDGE('',*,*,#28895,.F.);
#39537=ORIENTED_EDGE('',*,*,#28906,.F.);
#39538=ORIENTED_EDGE('',*,*,#25795,.T.);
#39539=ORIENTED_EDGE('',*,*,#28905,.T.);
#39540=ORIENTED_EDGE('',*,*,#28894,.F.);
#39541=ORIENTED_EDGE('',*,*,#28907,.F.);
#39542=ORIENTED_EDGE('',*,*,#25796,.T.);
#39543=ORIENTED_EDGE('',*,*,#28906,.T.);
#39544=ORIENTED_EDGE('',*,*,#28893,.F.);
#39545=ORIENTED_EDGE('',*,*,#28908,.F.);
#39546=ORIENTED_EDGE('',*,*,#25797,.T.);
#39547=ORIENTED_EDGE('',*,*,#28907,.T.);
#39548=ORIENTED_EDGE('',*,*,#28892,.F.);
#39549=ORIENTED_EDGE('',*,*,#28909,.F.);
#39550=ORIENTED_EDGE('',*,*,#25798,.T.);
#39551=ORIENTED_EDGE('',*,*,#28908,.T.);
#39552=ORIENTED_EDGE('',*,*,#28891,.F.);
#39553=ORIENTED_EDGE('',*,*,#28910,.F.);
#39554=ORIENTED_EDGE('',*,*,#25799,.T.);
#39555=ORIENTED_EDGE('',*,*,#28909,.T.);
#39556=ORIENTED_EDGE('',*,*,#28890,.F.);
#39557=ORIENTED_EDGE('',*,*,#28911,.F.);
#39558=ORIENTED_EDGE('',*,*,#25800,.T.);
#39559=ORIENTED_EDGE('',*,*,#28910,.T.);
#39560=ORIENTED_EDGE('',*,*,#28889,.F.);
#39561=ORIENTED_EDGE('',*,*,#28912,.F.);
#39562=ORIENTED_EDGE('',*,*,#25801,.T.);
#39563=ORIENTED_EDGE('',*,*,#28911,.T.);
#39564=ORIENTED_EDGE('',*,*,#28888,.F.);
#39565=ORIENTED_EDGE('',*,*,#28913,.F.);
#39566=ORIENTED_EDGE('',*,*,#25802,.T.);
#39567=ORIENTED_EDGE('',*,*,#28912,.T.);
#39568=ORIENTED_EDGE('',*,*,#26841,.T.);
#39569=ORIENTED_EDGE('',*,*,#25803,.T.);
#39570=ORIENTED_EDGE('',*,*,#28913,.T.);
#39571=ORIENTED_EDGE('',*,*,#28887,.F.);
#39572=ORIENTED_EDGE('',*,*,#28914,.F.);
#39573=ORIENTED_EDGE('',*,*,#27388,.T.);
#39574=ORIENTED_EDGE('',*,*,#27281,.T.);
#39575=ORIENTED_EDGE('',*,*,#28915,.F.);
#39576=ORIENTED_EDGE('',*,*,#28916,.F.);
#39577=ORIENTED_EDGE('',*,*,#25806,.T.);
#39578=ORIENTED_EDGE('',*,*,#26918,.T.);
#39579=ORIENTED_EDGE('',*,*,#28917,.F.);
#39580=ORIENTED_EDGE('',*,*,#28918,.F.);
#39581=ORIENTED_EDGE('',*,*,#25807,.T.);
#39582=ORIENTED_EDGE('',*,*,#28916,.T.);
#39583=ORIENTED_EDGE('',*,*,#28919,.F.);
#39584=ORIENTED_EDGE('',*,*,#28920,.F.);
#39585=ORIENTED_EDGE('',*,*,#25808,.T.);
#39586=ORIENTED_EDGE('',*,*,#28918,.T.);
#39587=ORIENTED_EDGE('',*,*,#28921,.F.);
#39588=ORIENTED_EDGE('',*,*,#28922,.F.);
#39589=ORIENTED_EDGE('',*,*,#25809,.T.);
#39590=ORIENTED_EDGE('',*,*,#28920,.T.);
#39591=ORIENTED_EDGE('',*,*,#28923,.F.);
#39592=ORIENTED_EDGE('',*,*,#28924,.F.);
#39593=ORIENTED_EDGE('',*,*,#25810,.T.);
#39594=ORIENTED_EDGE('',*,*,#28922,.T.);
#39595=ORIENTED_EDGE('',*,*,#28925,.F.);
#39596=ORIENTED_EDGE('',*,*,#28926,.F.);
#39597=ORIENTED_EDGE('',*,*,#25811,.T.);
#39598=ORIENTED_EDGE('',*,*,#28924,.T.);
#39599=ORIENTED_EDGE('',*,*,#28927,.F.);
#39600=ORIENTED_EDGE('',*,*,#28928,.F.);
#39601=ORIENTED_EDGE('',*,*,#25812,.T.);
#39602=ORIENTED_EDGE('',*,*,#28926,.T.);
#39603=ORIENTED_EDGE('',*,*,#28929,.F.);
#39604=ORIENTED_EDGE('',*,*,#28930,.F.);
#39605=ORIENTED_EDGE('',*,*,#25813,.T.);
#39606=ORIENTED_EDGE('',*,*,#28928,.T.);
#39607=ORIENTED_EDGE('',*,*,#28931,.F.);
#39608=ORIENTED_EDGE('',*,*,#28932,.F.);
#39609=ORIENTED_EDGE('',*,*,#25814,.T.);
#39610=ORIENTED_EDGE('',*,*,#28930,.T.);
#39611=ORIENTED_EDGE('',*,*,#28933,.F.);
#39612=ORIENTED_EDGE('',*,*,#28934,.F.);
#39613=ORIENTED_EDGE('',*,*,#25815,.T.);
#39614=ORIENTED_EDGE('',*,*,#28932,.T.);
#39615=ORIENTED_EDGE('',*,*,#28935,.F.);
#39616=ORIENTED_EDGE('',*,*,#28936,.F.);
#39617=ORIENTED_EDGE('',*,*,#25816,.T.);
#39618=ORIENTED_EDGE('',*,*,#28934,.T.);
#39619=ORIENTED_EDGE('',*,*,#28937,.F.);
#39620=ORIENTED_EDGE('',*,*,#28938,.F.);
#39621=ORIENTED_EDGE('',*,*,#25817,.T.);
#39622=ORIENTED_EDGE('',*,*,#28936,.T.);
#39623=ORIENTED_EDGE('',*,*,#28939,.F.);
#39624=ORIENTED_EDGE('',*,*,#27225,.F.);
#39625=ORIENTED_EDGE('',*,*,#25818,.T.);
#39626=ORIENTED_EDGE('',*,*,#28938,.T.);
#39627=ORIENTED_EDGE('',*,*,#27068,.T.);
#39628=ORIENTED_EDGE('',*,*,#27228,.F.);
#39629=ORIENTED_EDGE('',*,*,#27482,.F.);
#39630=ORIENTED_EDGE('',*,*,#25821,.F.);
#39631=ORIENTED_EDGE('',*,*,#27226,.T.);
#39632=ORIENTED_EDGE('',*,*,#28939,.T.);
#39633=ORIENTED_EDGE('',*,*,#28937,.T.);
#39634=ORIENTED_EDGE('',*,*,#28935,.T.);
#39635=ORIENTED_EDGE('',*,*,#28933,.T.);
#39636=ORIENTED_EDGE('',*,*,#28931,.T.);
#39637=ORIENTED_EDGE('',*,*,#28929,.T.);
#39638=ORIENTED_EDGE('',*,*,#28927,.T.);
#39639=ORIENTED_EDGE('',*,*,#28925,.T.);
#39640=ORIENTED_EDGE('',*,*,#28923,.T.);
#39641=ORIENTED_EDGE('',*,*,#28921,.T.);
#39642=ORIENTED_EDGE('',*,*,#28919,.T.);
#39643=ORIENTED_EDGE('',*,*,#28917,.T.);
#39644=ORIENTED_EDGE('',*,*,#28915,.T.);
#39645=ORIENTED_EDGE('',*,*,#26917,.T.);
#39646=ORIENTED_EDGE('',*,*,#28940,.F.);
#39647=ORIENTED_EDGE('',*,*,#28941,.T.);
#39648=ORIENTED_EDGE('',*,*,#28942,.T.);
#39649=ORIENTED_EDGE('',*,*,#28943,.T.);
#39650=ORIENTED_EDGE('',*,*,#28944,.T.);
#39651=ORIENTED_EDGE('',*,*,#28945,.T.);
#39652=ORIENTED_EDGE('',*,*,#28946,.T.);
#39653=ORIENTED_EDGE('',*,*,#28947,.T.);
#39654=ORIENTED_EDGE('',*,*,#28948,.T.);
#39655=ORIENTED_EDGE('',*,*,#28949,.T.);
#39656=ORIENTED_EDGE('',*,*,#28950,.T.);
#39657=ORIENTED_EDGE('',*,*,#28951,.T.);
#39658=ORIENTED_EDGE('',*,*,#28952,.T.);
#39659=ORIENTED_EDGE('',*,*,#28953,.T.);
#39660=ORIENTED_EDGE('',*,*,#28954,.T.);
#39661=ORIENTED_EDGE('',*,*,#25787,.T.);
#39662=ORIENTED_EDGE('',*,*,#27483,.T.);
#39663=ORIENTED_EDGE('',*,*,#28954,.F.);
#39664=ORIENTED_EDGE('',*,*,#28955,.F.);
#39665=ORIENTED_EDGE('',*,*,#25754,.T.);
#39666=ORIENTED_EDGE('',*,*,#25788,.T.);
#39667=ORIENTED_EDGE('',*,*,#28953,.F.);
#39668=ORIENTED_EDGE('',*,*,#28956,.F.);
#39669=ORIENTED_EDGE('',*,*,#25755,.T.);
#39670=ORIENTED_EDGE('',*,*,#28955,.T.);
#39671=ORIENTED_EDGE('',*,*,#28952,.F.);
#39672=ORIENTED_EDGE('',*,*,#28957,.F.);
#39673=ORIENTED_EDGE('',*,*,#25756,.T.);
#39674=ORIENTED_EDGE('',*,*,#28956,.T.);
#39675=ORIENTED_EDGE('',*,*,#28951,.F.);
#39676=ORIENTED_EDGE('',*,*,#28958,.F.);
#39677=ORIENTED_EDGE('',*,*,#25757,.T.);
#39678=ORIENTED_EDGE('',*,*,#28957,.T.);
#39679=ORIENTED_EDGE('',*,*,#28950,.F.);
#39680=ORIENTED_EDGE('',*,*,#28959,.F.);
#39681=ORIENTED_EDGE('',*,*,#25758,.T.);
#39682=ORIENTED_EDGE('',*,*,#28958,.T.);
#39683=ORIENTED_EDGE('',*,*,#28949,.F.);
#39684=ORIENTED_EDGE('',*,*,#28960,.F.);
#39685=ORIENTED_EDGE('',*,*,#25759,.T.);
#39686=ORIENTED_EDGE('',*,*,#28959,.T.);
#39687=ORIENTED_EDGE('',*,*,#28948,.F.);
#39688=ORIENTED_EDGE('',*,*,#28961,.F.);
#39689=ORIENTED_EDGE('',*,*,#25760,.T.);
#39690=ORIENTED_EDGE('',*,*,#28960,.T.);
#39691=ORIENTED_EDGE('',*,*,#28947,.F.);
#39692=ORIENTED_EDGE('',*,*,#28962,.F.);
#39693=ORIENTED_EDGE('',*,*,#25761,.T.);
#39694=ORIENTED_EDGE('',*,*,#28961,.T.);
#39695=ORIENTED_EDGE('',*,*,#28946,.F.);
#39696=ORIENTED_EDGE('',*,*,#28963,.F.);
#39697=ORIENTED_EDGE('',*,*,#25762,.T.);
#39698=ORIENTED_EDGE('',*,*,#28962,.T.);
#39699=ORIENTED_EDGE('',*,*,#28945,.F.);
#39700=ORIENTED_EDGE('',*,*,#28964,.F.);
#39701=ORIENTED_EDGE('',*,*,#25763,.T.);
#39702=ORIENTED_EDGE('',*,*,#28963,.T.);
#39703=ORIENTED_EDGE('',*,*,#28944,.F.);
#39704=ORIENTED_EDGE('',*,*,#28965,.F.);
#39705=ORIENTED_EDGE('',*,*,#25764,.T.);
#39706=ORIENTED_EDGE('',*,*,#28964,.T.);
#39707=ORIENTED_EDGE('',*,*,#28943,.F.);
#39708=ORIENTED_EDGE('',*,*,#28966,.F.);
#39709=ORIENTED_EDGE('',*,*,#25765,.T.);
#39710=ORIENTED_EDGE('',*,*,#28965,.T.);
#39711=ORIENTED_EDGE('',*,*,#28942,.F.);
#39712=ORIENTED_EDGE('',*,*,#28967,.F.);
#39713=ORIENTED_EDGE('',*,*,#25766,.T.);
#39714=ORIENTED_EDGE('',*,*,#28966,.T.);
#39715=ORIENTED_EDGE('',*,*,#26844,.T.);
#39716=ORIENTED_EDGE('',*,*,#25767,.T.);
#39717=ORIENTED_EDGE('',*,*,#28967,.T.);
#39718=ORIENTED_EDGE('',*,*,#28941,.F.);
#39719=ORIENTED_EDGE('',*,*,#28968,.F.);
#39720=ORIENTED_EDGE('',*,*,#27390,.T.);
#39721=ORIENTED_EDGE('',*,*,#27279,.T.);
#39722=ORIENTED_EDGE('',*,*,#28969,.F.);
#39723=ORIENTED_EDGE('',*,*,#28970,.F.);
#39724=ORIENTED_EDGE('',*,*,#25770,.T.);
#39725=ORIENTED_EDGE('',*,*,#26913,.T.);
#39726=ORIENTED_EDGE('',*,*,#28971,.F.);
#39727=ORIENTED_EDGE('',*,*,#28972,.F.);
#39728=ORIENTED_EDGE('',*,*,#25771,.T.);
#39729=ORIENTED_EDGE('',*,*,#28970,.T.);
#39730=ORIENTED_EDGE('',*,*,#28973,.F.);
#39731=ORIENTED_EDGE('',*,*,#28974,.F.);
#39732=ORIENTED_EDGE('',*,*,#25772,.T.);
#39733=ORIENTED_EDGE('',*,*,#28972,.T.);
#39734=ORIENTED_EDGE('',*,*,#28975,.F.);
#39735=ORIENTED_EDGE('',*,*,#28976,.F.);
#39736=ORIENTED_EDGE('',*,*,#25773,.T.);
#39737=ORIENTED_EDGE('',*,*,#28974,.T.);
#39738=ORIENTED_EDGE('',*,*,#28977,.F.);
#39739=ORIENTED_EDGE('',*,*,#28978,.F.);
#39740=ORIENTED_EDGE('',*,*,#25774,.T.);
#39741=ORIENTED_EDGE('',*,*,#28976,.T.);
#39742=ORIENTED_EDGE('',*,*,#28979,.F.);
#39743=ORIENTED_EDGE('',*,*,#28980,.F.);
#39744=ORIENTED_EDGE('',*,*,#25775,.T.);
#39745=ORIENTED_EDGE('',*,*,#28978,.T.);
#39746=ORIENTED_EDGE('',*,*,#28981,.F.);
#39747=ORIENTED_EDGE('',*,*,#28982,.F.);
#39748=ORIENTED_EDGE('',*,*,#25776,.T.);
#39749=ORIENTED_EDGE('',*,*,#28980,.T.);
#39750=ORIENTED_EDGE('',*,*,#28983,.F.);
#39751=ORIENTED_EDGE('',*,*,#28984,.F.);
#39752=ORIENTED_EDGE('',*,*,#25777,.T.);
#39753=ORIENTED_EDGE('',*,*,#28982,.T.);
#39754=ORIENTED_EDGE('',*,*,#28985,.F.);
#39755=ORIENTED_EDGE('',*,*,#28986,.F.);
#39756=ORIENTED_EDGE('',*,*,#25778,.T.);
#39757=ORIENTED_EDGE('',*,*,#28984,.T.);
#39758=ORIENTED_EDGE('',*,*,#28987,.F.);
#39759=ORIENTED_EDGE('',*,*,#28988,.F.);
#39760=ORIENTED_EDGE('',*,*,#25779,.T.);
#39761=ORIENTED_EDGE('',*,*,#28986,.T.);
#39762=ORIENTED_EDGE('',*,*,#28989,.F.);
#39763=ORIENTED_EDGE('',*,*,#28990,.F.);
#39764=ORIENTED_EDGE('',*,*,#25780,.T.);
#39765=ORIENTED_EDGE('',*,*,#28988,.T.);
#39766=ORIENTED_EDGE('',*,*,#28991,.F.);
#39767=ORIENTED_EDGE('',*,*,#28992,.F.);
#39768=ORIENTED_EDGE('',*,*,#25781,.T.);
#39769=ORIENTED_EDGE('',*,*,#28990,.T.);
#39770=ORIENTED_EDGE('',*,*,#28993,.F.);
#39771=ORIENTED_EDGE('',*,*,#27229,.F.);
#39772=ORIENTED_EDGE('',*,*,#25782,.T.);
#39773=ORIENTED_EDGE('',*,*,#28992,.T.);
#39774=ORIENTED_EDGE('',*,*,#27066,.T.);
#39775=ORIENTED_EDGE('',*,*,#27232,.F.);
#39776=ORIENTED_EDGE('',*,*,#27484,.F.);
#39777=ORIENTED_EDGE('',*,*,#25785,.F.);
#39778=ORIENTED_EDGE('',*,*,#27230,.T.);
#39779=ORIENTED_EDGE('',*,*,#28993,.T.);
#39780=ORIENTED_EDGE('',*,*,#28991,.T.);
#39781=ORIENTED_EDGE('',*,*,#28989,.T.);
#39782=ORIENTED_EDGE('',*,*,#28987,.T.);
#39783=ORIENTED_EDGE('',*,*,#28985,.T.);
#39784=ORIENTED_EDGE('',*,*,#28983,.T.);
#39785=ORIENTED_EDGE('',*,*,#28981,.T.);
#39786=ORIENTED_EDGE('',*,*,#28979,.T.);
#39787=ORIENTED_EDGE('',*,*,#28977,.T.);
#39788=ORIENTED_EDGE('',*,*,#28975,.T.);
#39789=ORIENTED_EDGE('',*,*,#28973,.T.);
#39790=ORIENTED_EDGE('',*,*,#28971,.T.);
#39791=ORIENTED_EDGE('',*,*,#28969,.T.);
#39792=ORIENTED_EDGE('',*,*,#26912,.T.);
#39793=ORIENTED_EDGE('',*,*,#28994,.F.);
#39794=ORIENTED_EDGE('',*,*,#28995,.T.);
#39795=ORIENTED_EDGE('',*,*,#28996,.T.);
#39796=ORIENTED_EDGE('',*,*,#28997,.T.);
#39797=ORIENTED_EDGE('',*,*,#28998,.T.);
#39798=ORIENTED_EDGE('',*,*,#28999,.T.);
#39799=ORIENTED_EDGE('',*,*,#29000,.T.);
#39800=ORIENTED_EDGE('',*,*,#29001,.T.);
#39801=ORIENTED_EDGE('',*,*,#29002,.T.);
#39802=ORIENTED_EDGE('',*,*,#29003,.T.);
#39803=ORIENTED_EDGE('',*,*,#29004,.T.);
#39804=ORIENTED_EDGE('',*,*,#29005,.T.);
#39805=ORIENTED_EDGE('',*,*,#29006,.T.);
#39806=ORIENTED_EDGE('',*,*,#29007,.T.);
#39807=ORIENTED_EDGE('',*,*,#29008,.T.);
#39808=ORIENTED_EDGE('',*,*,#25751,.T.);
#39809=ORIENTED_EDGE('',*,*,#27485,.T.);
#39810=ORIENTED_EDGE('',*,*,#29008,.F.);
#39811=ORIENTED_EDGE('',*,*,#29009,.F.);
#39812=ORIENTED_EDGE('',*,*,#25718,.T.);
#39813=ORIENTED_EDGE('',*,*,#25752,.T.);
#39814=ORIENTED_EDGE('',*,*,#29007,.F.);
#39815=ORIENTED_EDGE('',*,*,#29010,.F.);
#39816=ORIENTED_EDGE('',*,*,#25719,.T.);
#39817=ORIENTED_EDGE('',*,*,#29009,.T.);
#39818=ORIENTED_EDGE('',*,*,#29006,.F.);
#39819=ORIENTED_EDGE('',*,*,#29011,.F.);
#39820=ORIENTED_EDGE('',*,*,#25720,.T.);
#39821=ORIENTED_EDGE('',*,*,#29010,.T.);
#39822=ORIENTED_EDGE('',*,*,#29005,.F.);
#39823=ORIENTED_EDGE('',*,*,#29012,.F.);
#39824=ORIENTED_EDGE('',*,*,#25721,.T.);
#39825=ORIENTED_EDGE('',*,*,#29011,.T.);
#39826=ORIENTED_EDGE('',*,*,#29004,.F.);
#39827=ORIENTED_EDGE('',*,*,#29013,.F.);
#39828=ORIENTED_EDGE('',*,*,#25722,.T.);
#39829=ORIENTED_EDGE('',*,*,#29012,.T.);
#39830=ORIENTED_EDGE('',*,*,#29003,.F.);
#39831=ORIENTED_EDGE('',*,*,#29014,.F.);
#39832=ORIENTED_EDGE('',*,*,#25723,.T.);
#39833=ORIENTED_EDGE('',*,*,#29013,.T.);
#39834=ORIENTED_EDGE('',*,*,#29002,.F.);
#39835=ORIENTED_EDGE('',*,*,#29015,.F.);
#39836=ORIENTED_EDGE('',*,*,#25724,.T.);
#39837=ORIENTED_EDGE('',*,*,#29014,.T.);
#39838=ORIENTED_EDGE('',*,*,#29001,.F.);
#39839=ORIENTED_EDGE('',*,*,#29016,.F.);
#39840=ORIENTED_EDGE('',*,*,#25725,.T.);
#39841=ORIENTED_EDGE('',*,*,#29015,.T.);
#39842=ORIENTED_EDGE('',*,*,#29000,.F.);
#39843=ORIENTED_EDGE('',*,*,#29017,.F.);
#39844=ORIENTED_EDGE('',*,*,#25726,.T.);
#39845=ORIENTED_EDGE('',*,*,#29016,.T.);
#39846=ORIENTED_EDGE('',*,*,#28999,.F.);
#39847=ORIENTED_EDGE('',*,*,#29018,.F.);
#39848=ORIENTED_EDGE('',*,*,#25727,.T.);
#39849=ORIENTED_EDGE('',*,*,#29017,.T.);
#39850=ORIENTED_EDGE('',*,*,#28998,.F.);
#39851=ORIENTED_EDGE('',*,*,#29019,.F.);
#39852=ORIENTED_EDGE('',*,*,#25728,.T.);
#39853=ORIENTED_EDGE('',*,*,#29018,.T.);
#39854=ORIENTED_EDGE('',*,*,#28997,.F.);
#39855=ORIENTED_EDGE('',*,*,#29020,.F.);
#39856=ORIENTED_EDGE('',*,*,#25729,.T.);
#39857=ORIENTED_EDGE('',*,*,#29019,.T.);
#39858=ORIENTED_EDGE('',*,*,#28996,.F.);
#39859=ORIENTED_EDGE('',*,*,#29021,.F.);
#39860=ORIENTED_EDGE('',*,*,#25730,.T.);
#39861=ORIENTED_EDGE('',*,*,#29020,.T.);
#39862=ORIENTED_EDGE('',*,*,#26847,.T.);
#39863=ORIENTED_EDGE('',*,*,#25731,.T.);
#39864=ORIENTED_EDGE('',*,*,#29021,.T.);
#39865=ORIENTED_EDGE('',*,*,#28995,.F.);
#39866=ORIENTED_EDGE('',*,*,#29022,.F.);
#39867=ORIENTED_EDGE('',*,*,#27392,.T.);
#39868=ORIENTED_EDGE('',*,*,#27277,.T.);
#39869=ORIENTED_EDGE('',*,*,#29023,.F.);
#39870=ORIENTED_EDGE('',*,*,#29024,.F.);
#39871=ORIENTED_EDGE('',*,*,#25734,.T.);
#39872=ORIENTED_EDGE('',*,*,#26908,.T.);
#39873=ORIENTED_EDGE('',*,*,#29025,.F.);
#39874=ORIENTED_EDGE('',*,*,#29026,.F.);
#39875=ORIENTED_EDGE('',*,*,#25735,.T.);
#39876=ORIENTED_EDGE('',*,*,#29024,.T.);
#39877=ORIENTED_EDGE('',*,*,#29027,.F.);
#39878=ORIENTED_EDGE('',*,*,#29028,.F.);
#39879=ORIENTED_EDGE('',*,*,#25736,.T.);
#39880=ORIENTED_EDGE('',*,*,#29026,.T.);
#39881=ORIENTED_EDGE('',*,*,#29029,.F.);
#39882=ORIENTED_EDGE('',*,*,#29030,.F.);
#39883=ORIENTED_EDGE('',*,*,#25737,.T.);
#39884=ORIENTED_EDGE('',*,*,#29028,.T.);
#39885=ORIENTED_EDGE('',*,*,#29031,.F.);
#39886=ORIENTED_EDGE('',*,*,#29032,.F.);
#39887=ORIENTED_EDGE('',*,*,#25738,.T.);
#39888=ORIENTED_EDGE('',*,*,#29030,.T.);
#39889=ORIENTED_EDGE('',*,*,#29033,.F.);
#39890=ORIENTED_EDGE('',*,*,#29034,.F.);
#39891=ORIENTED_EDGE('',*,*,#25739,.T.);
#39892=ORIENTED_EDGE('',*,*,#29032,.T.);
#39893=ORIENTED_EDGE('',*,*,#29035,.F.);
#39894=ORIENTED_EDGE('',*,*,#29036,.F.);
#39895=ORIENTED_EDGE('',*,*,#25740,.T.);
#39896=ORIENTED_EDGE('',*,*,#29034,.T.);
#39897=ORIENTED_EDGE('',*,*,#29037,.F.);
#39898=ORIENTED_EDGE('',*,*,#29038,.F.);
#39899=ORIENTED_EDGE('',*,*,#25741,.T.);
#39900=ORIENTED_EDGE('',*,*,#29036,.T.);
#39901=ORIENTED_EDGE('',*,*,#29039,.F.);
#39902=ORIENTED_EDGE('',*,*,#29040,.F.);
#39903=ORIENTED_EDGE('',*,*,#25742,.T.);
#39904=ORIENTED_EDGE('',*,*,#29038,.T.);
#39905=ORIENTED_EDGE('',*,*,#29041,.F.);
#39906=ORIENTED_EDGE('',*,*,#29042,.F.);
#39907=ORIENTED_EDGE('',*,*,#25743,.T.);
#39908=ORIENTED_EDGE('',*,*,#29040,.T.);
#39909=ORIENTED_EDGE('',*,*,#29043,.F.);
#39910=ORIENTED_EDGE('',*,*,#29044,.F.);
#39911=ORIENTED_EDGE('',*,*,#25744,.T.);
#39912=ORIENTED_EDGE('',*,*,#29042,.T.);
#39913=ORIENTED_EDGE('',*,*,#29045,.F.);
#39914=ORIENTED_EDGE('',*,*,#29046,.F.);
#39915=ORIENTED_EDGE('',*,*,#25745,.T.);
#39916=ORIENTED_EDGE('',*,*,#29044,.T.);
#39917=ORIENTED_EDGE('',*,*,#29047,.F.);
#39918=ORIENTED_EDGE('',*,*,#27233,.F.);
#39919=ORIENTED_EDGE('',*,*,#25746,.T.);
#39920=ORIENTED_EDGE('',*,*,#29046,.T.);
#39921=ORIENTED_EDGE('',*,*,#27064,.T.);
#39922=ORIENTED_EDGE('',*,*,#27236,.F.);
#39923=ORIENTED_EDGE('',*,*,#27486,.F.);
#39924=ORIENTED_EDGE('',*,*,#25749,.F.);
#39925=ORIENTED_EDGE('',*,*,#27234,.T.);
#39926=ORIENTED_EDGE('',*,*,#29047,.T.);
#39927=ORIENTED_EDGE('',*,*,#29045,.T.);
#39928=ORIENTED_EDGE('',*,*,#29043,.T.);
#39929=ORIENTED_EDGE('',*,*,#29041,.T.);
#39930=ORIENTED_EDGE('',*,*,#29039,.T.);
#39931=ORIENTED_EDGE('',*,*,#29037,.T.);
#39932=ORIENTED_EDGE('',*,*,#29035,.T.);
#39933=ORIENTED_EDGE('',*,*,#29033,.T.);
#39934=ORIENTED_EDGE('',*,*,#29031,.T.);
#39935=ORIENTED_EDGE('',*,*,#29029,.T.);
#39936=ORIENTED_EDGE('',*,*,#29027,.T.);
#39937=ORIENTED_EDGE('',*,*,#29025,.T.);
#39938=ORIENTED_EDGE('',*,*,#29023,.T.);
#39939=ORIENTED_EDGE('',*,*,#26907,.T.);
#39940=ORIENTED_EDGE('',*,*,#29048,.F.);
#39941=ORIENTED_EDGE('',*,*,#29049,.T.);
#39942=ORIENTED_EDGE('',*,*,#29050,.T.);
#39943=ORIENTED_EDGE('',*,*,#29051,.T.);
#39944=ORIENTED_EDGE('',*,*,#29052,.T.);
#39945=ORIENTED_EDGE('',*,*,#29053,.T.);
#39946=ORIENTED_EDGE('',*,*,#29054,.T.);
#39947=ORIENTED_EDGE('',*,*,#29055,.T.);
#39948=ORIENTED_EDGE('',*,*,#29056,.T.);
#39949=ORIENTED_EDGE('',*,*,#29057,.T.);
#39950=ORIENTED_EDGE('',*,*,#29058,.T.);
#39951=ORIENTED_EDGE('',*,*,#29059,.T.);
#39952=ORIENTED_EDGE('',*,*,#29060,.T.);
#39953=ORIENTED_EDGE('',*,*,#29061,.T.);
#39954=ORIENTED_EDGE('',*,*,#29062,.T.);
#39955=ORIENTED_EDGE('',*,*,#25715,.T.);
#39956=ORIENTED_EDGE('',*,*,#27487,.T.);
#39957=ORIENTED_EDGE('',*,*,#29062,.F.);
#39958=ORIENTED_EDGE('',*,*,#29063,.F.);
#39959=ORIENTED_EDGE('',*,*,#25682,.T.);
#39960=ORIENTED_EDGE('',*,*,#25716,.T.);
#39961=ORIENTED_EDGE('',*,*,#29061,.F.);
#39962=ORIENTED_EDGE('',*,*,#29064,.F.);
#39963=ORIENTED_EDGE('',*,*,#25683,.T.);
#39964=ORIENTED_EDGE('',*,*,#29063,.T.);
#39965=ORIENTED_EDGE('',*,*,#29060,.F.);
#39966=ORIENTED_EDGE('',*,*,#29065,.F.);
#39967=ORIENTED_EDGE('',*,*,#25684,.T.);
#39968=ORIENTED_EDGE('',*,*,#29064,.T.);
#39969=ORIENTED_EDGE('',*,*,#29059,.F.);
#39970=ORIENTED_EDGE('',*,*,#29066,.F.);
#39971=ORIENTED_EDGE('',*,*,#25685,.T.);
#39972=ORIENTED_EDGE('',*,*,#29065,.T.);
#39973=ORIENTED_EDGE('',*,*,#29058,.F.);
#39974=ORIENTED_EDGE('',*,*,#29067,.F.);
#39975=ORIENTED_EDGE('',*,*,#25686,.T.);
#39976=ORIENTED_EDGE('',*,*,#29066,.T.);
#39977=ORIENTED_EDGE('',*,*,#29057,.F.);
#39978=ORIENTED_EDGE('',*,*,#29068,.F.);
#39979=ORIENTED_EDGE('',*,*,#25687,.T.);
#39980=ORIENTED_EDGE('',*,*,#29067,.T.);
#39981=ORIENTED_EDGE('',*,*,#29056,.F.);
#39982=ORIENTED_EDGE('',*,*,#29069,.F.);
#39983=ORIENTED_EDGE('',*,*,#25688,.T.);
#39984=ORIENTED_EDGE('',*,*,#29068,.T.);
#39985=ORIENTED_EDGE('',*,*,#29055,.F.);
#39986=ORIENTED_EDGE('',*,*,#29070,.F.);
#39987=ORIENTED_EDGE('',*,*,#25689,.T.);
#39988=ORIENTED_EDGE('',*,*,#29069,.T.);
#39989=ORIENTED_EDGE('',*,*,#29054,.F.);
#39990=ORIENTED_EDGE('',*,*,#29071,.F.);
#39991=ORIENTED_EDGE('',*,*,#25690,.T.);
#39992=ORIENTED_EDGE('',*,*,#29070,.T.);
#39993=ORIENTED_EDGE('',*,*,#29053,.F.);
#39994=ORIENTED_EDGE('',*,*,#29072,.F.);
#39995=ORIENTED_EDGE('',*,*,#25691,.T.);
#39996=ORIENTED_EDGE('',*,*,#29071,.T.);
#39997=ORIENTED_EDGE('',*,*,#29052,.F.);
#39998=ORIENTED_EDGE('',*,*,#29073,.F.);
#39999=ORIENTED_EDGE('',*,*,#25692,.T.);
#40000=ORIENTED_EDGE('',*,*,#29072,.T.);
#40001=ORIENTED_EDGE('',*,*,#29051,.F.);
#40002=ORIENTED_EDGE('',*,*,#29074,.F.);
#40003=ORIENTED_EDGE('',*,*,#25693,.T.);
#40004=ORIENTED_EDGE('',*,*,#29073,.T.);
#40005=ORIENTED_EDGE('',*,*,#29050,.F.);
#40006=ORIENTED_EDGE('',*,*,#29075,.F.);
#40007=ORIENTED_EDGE('',*,*,#25694,.T.);
#40008=ORIENTED_EDGE('',*,*,#29074,.T.);
#40009=ORIENTED_EDGE('',*,*,#26850,.T.);
#40010=ORIENTED_EDGE('',*,*,#25695,.T.);
#40011=ORIENTED_EDGE('',*,*,#29075,.T.);
#40012=ORIENTED_EDGE('',*,*,#29049,.F.);
#40013=ORIENTED_EDGE('',*,*,#29076,.F.);
#40014=ORIENTED_EDGE('',*,*,#27394,.T.);
#40015=ORIENTED_EDGE('',*,*,#27275,.T.);
#40016=ORIENTED_EDGE('',*,*,#29077,.F.);
#40017=ORIENTED_EDGE('',*,*,#29078,.F.);
#40018=ORIENTED_EDGE('',*,*,#25698,.T.);
#40019=ORIENTED_EDGE('',*,*,#26903,.T.);
#40020=ORIENTED_EDGE('',*,*,#29079,.F.);
#40021=ORIENTED_EDGE('',*,*,#29080,.F.);
#40022=ORIENTED_EDGE('',*,*,#25699,.T.);
#40023=ORIENTED_EDGE('',*,*,#29078,.T.);
#40024=ORIENTED_EDGE('',*,*,#29081,.F.);
#40025=ORIENTED_EDGE('',*,*,#29082,.F.);
#40026=ORIENTED_EDGE('',*,*,#25700,.T.);
#40027=ORIENTED_EDGE('',*,*,#29080,.T.);
#40028=ORIENTED_EDGE('',*,*,#29083,.F.);
#40029=ORIENTED_EDGE('',*,*,#29084,.F.);
#40030=ORIENTED_EDGE('',*,*,#25701,.T.);
#40031=ORIENTED_EDGE('',*,*,#29082,.T.);
#40032=ORIENTED_EDGE('',*,*,#29085,.F.);
#40033=ORIENTED_EDGE('',*,*,#29086,.F.);
#40034=ORIENTED_EDGE('',*,*,#25702,.T.);
#40035=ORIENTED_EDGE('',*,*,#29084,.T.);
#40036=ORIENTED_EDGE('',*,*,#29087,.F.);
#40037=ORIENTED_EDGE('',*,*,#29088,.F.);
#40038=ORIENTED_EDGE('',*,*,#25703,.T.);
#40039=ORIENTED_EDGE('',*,*,#29086,.T.);
#40040=ORIENTED_EDGE('',*,*,#29089,.F.);
#40041=ORIENTED_EDGE('',*,*,#29090,.F.);
#40042=ORIENTED_EDGE('',*,*,#25704,.T.);
#40043=ORIENTED_EDGE('',*,*,#29088,.T.);
#40044=ORIENTED_EDGE('',*,*,#29091,.F.);
#40045=ORIENTED_EDGE('',*,*,#29092,.F.);
#40046=ORIENTED_EDGE('',*,*,#25705,.T.);
#40047=ORIENTED_EDGE('',*,*,#29090,.T.);
#40048=ORIENTED_EDGE('',*,*,#29093,.F.);
#40049=ORIENTED_EDGE('',*,*,#29094,.F.);
#40050=ORIENTED_EDGE('',*,*,#25706,.T.);
#40051=ORIENTED_EDGE('',*,*,#29092,.T.);
#40052=ORIENTED_EDGE('',*,*,#29095,.F.);
#40053=ORIENTED_EDGE('',*,*,#29096,.F.);
#40054=ORIENTED_EDGE('',*,*,#25707,.T.);
#40055=ORIENTED_EDGE('',*,*,#29094,.T.);
#40056=ORIENTED_EDGE('',*,*,#29097,.F.);
#40057=ORIENTED_EDGE('',*,*,#29098,.F.);
#40058=ORIENTED_EDGE('',*,*,#25708,.T.);
#40059=ORIENTED_EDGE('',*,*,#29096,.T.);
#40060=ORIENTED_EDGE('',*,*,#29099,.F.);
#40061=ORIENTED_EDGE('',*,*,#29100,.F.);
#40062=ORIENTED_EDGE('',*,*,#25709,.T.);
#40063=ORIENTED_EDGE('',*,*,#29098,.T.);
#40064=ORIENTED_EDGE('',*,*,#29101,.F.);
#40065=ORIENTED_EDGE('',*,*,#27237,.F.);
#40066=ORIENTED_EDGE('',*,*,#25710,.T.);
#40067=ORIENTED_EDGE('',*,*,#29100,.T.);
#40068=ORIENTED_EDGE('',*,*,#27062,.T.);
#40069=ORIENTED_EDGE('',*,*,#27240,.F.);
#40070=ORIENTED_EDGE('',*,*,#27488,.F.);
#40071=ORIENTED_EDGE('',*,*,#25713,.F.);
#40072=ORIENTED_EDGE('',*,*,#27238,.T.);
#40073=ORIENTED_EDGE('',*,*,#29101,.T.);
#40074=ORIENTED_EDGE('',*,*,#29099,.T.);
#40075=ORIENTED_EDGE('',*,*,#29097,.T.);
#40076=ORIENTED_EDGE('',*,*,#29095,.T.);
#40077=ORIENTED_EDGE('',*,*,#29093,.T.);
#40078=ORIENTED_EDGE('',*,*,#29091,.T.);
#40079=ORIENTED_EDGE('',*,*,#29089,.T.);
#40080=ORIENTED_EDGE('',*,*,#29087,.T.);
#40081=ORIENTED_EDGE('',*,*,#29085,.T.);
#40082=ORIENTED_EDGE('',*,*,#29083,.T.);
#40083=ORIENTED_EDGE('',*,*,#29081,.T.);
#40084=ORIENTED_EDGE('',*,*,#29079,.T.);
#40085=ORIENTED_EDGE('',*,*,#29077,.T.);
#40086=ORIENTED_EDGE('',*,*,#26902,.T.);
#40087=ORIENTED_EDGE('',*,*,#29102,.F.);
#40088=ORIENTED_EDGE('',*,*,#29103,.T.);
#40089=ORIENTED_EDGE('',*,*,#29104,.T.);
#40090=ORIENTED_EDGE('',*,*,#29105,.T.);
#40091=ORIENTED_EDGE('',*,*,#29106,.T.);
#40092=ORIENTED_EDGE('',*,*,#29107,.T.);
#40093=ORIENTED_EDGE('',*,*,#29108,.T.);
#40094=ORIENTED_EDGE('',*,*,#29109,.T.);
#40095=ORIENTED_EDGE('',*,*,#29110,.T.);
#40096=ORIENTED_EDGE('',*,*,#29111,.T.);
#40097=ORIENTED_EDGE('',*,*,#29112,.T.);
#40098=ORIENTED_EDGE('',*,*,#29113,.T.);
#40099=ORIENTED_EDGE('',*,*,#29114,.T.);
#40100=ORIENTED_EDGE('',*,*,#29115,.T.);
#40101=ORIENTED_EDGE('',*,*,#29116,.T.);
#40102=ORIENTED_EDGE('',*,*,#25679,.T.);
#40103=ORIENTED_EDGE('',*,*,#27489,.T.);
#40104=ORIENTED_EDGE('',*,*,#29116,.F.);
#40105=ORIENTED_EDGE('',*,*,#29117,.F.);
#40106=ORIENTED_EDGE('',*,*,#25646,.T.);
#40107=ORIENTED_EDGE('',*,*,#25680,.T.);
#40108=ORIENTED_EDGE('',*,*,#29115,.F.);
#40109=ORIENTED_EDGE('',*,*,#29118,.F.);
#40110=ORIENTED_EDGE('',*,*,#25647,.T.);
#40111=ORIENTED_EDGE('',*,*,#29117,.T.);
#40112=ORIENTED_EDGE('',*,*,#29114,.F.);
#40113=ORIENTED_EDGE('',*,*,#29119,.F.);
#40114=ORIENTED_EDGE('',*,*,#25648,.T.);
#40115=ORIENTED_EDGE('',*,*,#29118,.T.);
#40116=ORIENTED_EDGE('',*,*,#29113,.F.);
#40117=ORIENTED_EDGE('',*,*,#29120,.F.);
#40118=ORIENTED_EDGE('',*,*,#25649,.T.);
#40119=ORIENTED_EDGE('',*,*,#29119,.T.);
#40120=ORIENTED_EDGE('',*,*,#29112,.F.);
#40121=ORIENTED_EDGE('',*,*,#29121,.F.);
#40122=ORIENTED_EDGE('',*,*,#25650,.T.);
#40123=ORIENTED_EDGE('',*,*,#29120,.T.);
#40124=ORIENTED_EDGE('',*,*,#29111,.F.);
#40125=ORIENTED_EDGE('',*,*,#29122,.F.);
#40126=ORIENTED_EDGE('',*,*,#25651,.T.);
#40127=ORIENTED_EDGE('',*,*,#29121,.T.);
#40128=ORIENTED_EDGE('',*,*,#29110,.F.);
#40129=ORIENTED_EDGE('',*,*,#29123,.F.);
#40130=ORIENTED_EDGE('',*,*,#25652,.T.);
#40131=ORIENTED_EDGE('',*,*,#29122,.T.);
#40132=ORIENTED_EDGE('',*,*,#29109,.F.);
#40133=ORIENTED_EDGE('',*,*,#29124,.F.);
#40134=ORIENTED_EDGE('',*,*,#25653,.T.);
#40135=ORIENTED_EDGE('',*,*,#29123,.T.);
#40136=ORIENTED_EDGE('',*,*,#29108,.F.);
#40137=ORIENTED_EDGE('',*,*,#29125,.F.);
#40138=ORIENTED_EDGE('',*,*,#25654,.T.);
#40139=ORIENTED_EDGE('',*,*,#29124,.T.);
#40140=ORIENTED_EDGE('',*,*,#29107,.F.);
#40141=ORIENTED_EDGE('',*,*,#29126,.F.);
#40142=ORIENTED_EDGE('',*,*,#25655,.T.);
#40143=ORIENTED_EDGE('',*,*,#29125,.T.);
#40144=ORIENTED_EDGE('',*,*,#29106,.F.);
#40145=ORIENTED_EDGE('',*,*,#29127,.F.);
#40146=ORIENTED_EDGE('',*,*,#25656,.T.);
#40147=ORIENTED_EDGE('',*,*,#29126,.T.);
#40148=ORIENTED_EDGE('',*,*,#29105,.F.);
#40149=ORIENTED_EDGE('',*,*,#29128,.F.);
#40150=ORIENTED_EDGE('',*,*,#25657,.T.);
#40151=ORIENTED_EDGE('',*,*,#29127,.T.);
#40152=ORIENTED_EDGE('',*,*,#29104,.F.);
#40153=ORIENTED_EDGE('',*,*,#29129,.F.);
#40154=ORIENTED_EDGE('',*,*,#25658,.T.);
#40155=ORIENTED_EDGE('',*,*,#29128,.T.);
#40156=ORIENTED_EDGE('',*,*,#26853,.T.);
#40157=ORIENTED_EDGE('',*,*,#25659,.T.);
#40158=ORIENTED_EDGE('',*,*,#29129,.T.);
#40159=ORIENTED_EDGE('',*,*,#29103,.F.);
#40160=ORIENTED_EDGE('',*,*,#29130,.F.);
#40161=ORIENTED_EDGE('',*,*,#27396,.T.);
#40162=ORIENTED_EDGE('',*,*,#27273,.T.);
#40163=ORIENTED_EDGE('',*,*,#29131,.F.);
#40164=ORIENTED_EDGE('',*,*,#29132,.F.);
#40165=ORIENTED_EDGE('',*,*,#25662,.T.);
#40166=ORIENTED_EDGE('',*,*,#26898,.T.);
#40167=ORIENTED_EDGE('',*,*,#29133,.F.);
#40168=ORIENTED_EDGE('',*,*,#29134,.F.);
#40169=ORIENTED_EDGE('',*,*,#25663,.T.);
#40170=ORIENTED_EDGE('',*,*,#29132,.T.);
#40171=ORIENTED_EDGE('',*,*,#29135,.F.);
#40172=ORIENTED_EDGE('',*,*,#29136,.F.);
#40173=ORIENTED_EDGE('',*,*,#25664,.T.);
#40174=ORIENTED_EDGE('',*,*,#29134,.T.);
#40175=ORIENTED_EDGE('',*,*,#29137,.F.);
#40176=ORIENTED_EDGE('',*,*,#29138,.F.);
#40177=ORIENTED_EDGE('',*,*,#25665,.T.);
#40178=ORIENTED_EDGE('',*,*,#29136,.T.);
#40179=ORIENTED_EDGE('',*,*,#29139,.F.);
#40180=ORIENTED_EDGE('',*,*,#29140,.F.);
#40181=ORIENTED_EDGE('',*,*,#25666,.T.);
#40182=ORIENTED_EDGE('',*,*,#29138,.T.);
#40183=ORIENTED_EDGE('',*,*,#29141,.F.);
#40184=ORIENTED_EDGE('',*,*,#29142,.F.);
#40185=ORIENTED_EDGE('',*,*,#25667,.T.);
#40186=ORIENTED_EDGE('',*,*,#29140,.T.);
#40187=ORIENTED_EDGE('',*,*,#29143,.F.);
#40188=ORIENTED_EDGE('',*,*,#29144,.F.);
#40189=ORIENTED_EDGE('',*,*,#25668,.T.);
#40190=ORIENTED_EDGE('',*,*,#29142,.T.);
#40191=ORIENTED_EDGE('',*,*,#29145,.F.);
#40192=ORIENTED_EDGE('',*,*,#29146,.F.);
#40193=ORIENTED_EDGE('',*,*,#25669,.T.);
#40194=ORIENTED_EDGE('',*,*,#29144,.T.);
#40195=ORIENTED_EDGE('',*,*,#29147,.F.);
#40196=ORIENTED_EDGE('',*,*,#29148,.F.);
#40197=ORIENTED_EDGE('',*,*,#25670,.T.);
#40198=ORIENTED_EDGE('',*,*,#29146,.T.);
#40199=ORIENTED_EDGE('',*,*,#29149,.F.);
#40200=ORIENTED_EDGE('',*,*,#29150,.F.);
#40201=ORIENTED_EDGE('',*,*,#25671,.T.);
#40202=ORIENTED_EDGE('',*,*,#29148,.T.);
#40203=ORIENTED_EDGE('',*,*,#29151,.F.);
#40204=ORIENTED_EDGE('',*,*,#29152,.F.);
#40205=ORIENTED_EDGE('',*,*,#25672,.T.);
#40206=ORIENTED_EDGE('',*,*,#29150,.T.);
#40207=ORIENTED_EDGE('',*,*,#29153,.F.);
#40208=ORIENTED_EDGE('',*,*,#29154,.F.);
#40209=ORIENTED_EDGE('',*,*,#25673,.T.);
#40210=ORIENTED_EDGE('',*,*,#29152,.T.);
#40211=ORIENTED_EDGE('',*,*,#29155,.F.);
#40212=ORIENTED_EDGE('',*,*,#27241,.F.);
#40213=ORIENTED_EDGE('',*,*,#25674,.T.);
#40214=ORIENTED_EDGE('',*,*,#29154,.T.);
#40215=ORIENTED_EDGE('',*,*,#27060,.T.);
#40216=ORIENTED_EDGE('',*,*,#27244,.F.);
#40217=ORIENTED_EDGE('',*,*,#27490,.F.);
#40218=ORIENTED_EDGE('',*,*,#25677,.F.);
#40219=ORIENTED_EDGE('',*,*,#27242,.T.);
#40220=ORIENTED_EDGE('',*,*,#29155,.T.);
#40221=ORIENTED_EDGE('',*,*,#29153,.T.);
#40222=ORIENTED_EDGE('',*,*,#29151,.T.);
#40223=ORIENTED_EDGE('',*,*,#29149,.T.);
#40224=ORIENTED_EDGE('',*,*,#29147,.T.);
#40225=ORIENTED_EDGE('',*,*,#29145,.T.);
#40226=ORIENTED_EDGE('',*,*,#29143,.T.);
#40227=ORIENTED_EDGE('',*,*,#29141,.T.);
#40228=ORIENTED_EDGE('',*,*,#29139,.T.);
#40229=ORIENTED_EDGE('',*,*,#29137,.T.);
#40230=ORIENTED_EDGE('',*,*,#29135,.T.);
#40231=ORIENTED_EDGE('',*,*,#29133,.T.);
#40232=ORIENTED_EDGE('',*,*,#29131,.T.);
#40233=ORIENTED_EDGE('',*,*,#26897,.T.);
#40234=ORIENTED_EDGE('',*,*,#29156,.F.);
#40235=ORIENTED_EDGE('',*,*,#29157,.T.);
#40236=ORIENTED_EDGE('',*,*,#29158,.T.);
#40237=ORIENTED_EDGE('',*,*,#29159,.T.);
#40238=ORIENTED_EDGE('',*,*,#29160,.T.);
#40239=ORIENTED_EDGE('',*,*,#29161,.T.);
#40240=ORIENTED_EDGE('',*,*,#29162,.T.);
#40241=ORIENTED_EDGE('',*,*,#29163,.T.);
#40242=ORIENTED_EDGE('',*,*,#29164,.T.);
#40243=ORIENTED_EDGE('',*,*,#29165,.T.);
#40244=ORIENTED_EDGE('',*,*,#29166,.T.);
#40245=ORIENTED_EDGE('',*,*,#29167,.T.);
#40246=ORIENTED_EDGE('',*,*,#29168,.T.);
#40247=ORIENTED_EDGE('',*,*,#29169,.T.);
#40248=ORIENTED_EDGE('',*,*,#29170,.T.);
#40249=ORIENTED_EDGE('',*,*,#25643,.T.);
#40250=ORIENTED_EDGE('',*,*,#27491,.T.);
#40251=ORIENTED_EDGE('',*,*,#29170,.F.);
#40252=ORIENTED_EDGE('',*,*,#29171,.F.);
#40253=ORIENTED_EDGE('',*,*,#25610,.T.);
#40254=ORIENTED_EDGE('',*,*,#25644,.T.);
#40255=ORIENTED_EDGE('',*,*,#29169,.F.);
#40256=ORIENTED_EDGE('',*,*,#29172,.F.);
#40257=ORIENTED_EDGE('',*,*,#25611,.T.);
#40258=ORIENTED_EDGE('',*,*,#29171,.T.);
#40259=ORIENTED_EDGE('',*,*,#29168,.F.);
#40260=ORIENTED_EDGE('',*,*,#29173,.F.);
#40261=ORIENTED_EDGE('',*,*,#25612,.T.);
#40262=ORIENTED_EDGE('',*,*,#29172,.T.);
#40263=ORIENTED_EDGE('',*,*,#29167,.F.);
#40264=ORIENTED_EDGE('',*,*,#29174,.F.);
#40265=ORIENTED_EDGE('',*,*,#25613,.T.);
#40266=ORIENTED_EDGE('',*,*,#29173,.T.);
#40267=ORIENTED_EDGE('',*,*,#29166,.F.);
#40268=ORIENTED_EDGE('',*,*,#29175,.F.);
#40269=ORIENTED_EDGE('',*,*,#25614,.T.);
#40270=ORIENTED_EDGE('',*,*,#29174,.T.);
#40271=ORIENTED_EDGE('',*,*,#29165,.F.);
#40272=ORIENTED_EDGE('',*,*,#29176,.F.);
#40273=ORIENTED_EDGE('',*,*,#25615,.T.);
#40274=ORIENTED_EDGE('',*,*,#29175,.T.);
#40275=ORIENTED_EDGE('',*,*,#29164,.F.);
#40276=ORIENTED_EDGE('',*,*,#29177,.F.);
#40277=ORIENTED_EDGE('',*,*,#25616,.T.);
#40278=ORIENTED_EDGE('',*,*,#29176,.T.);
#40279=ORIENTED_EDGE('',*,*,#29163,.F.);
#40280=ORIENTED_EDGE('',*,*,#29178,.F.);
#40281=ORIENTED_EDGE('',*,*,#25617,.T.);
#40282=ORIENTED_EDGE('',*,*,#29177,.T.);
#40283=ORIENTED_EDGE('',*,*,#29162,.F.);
#40284=ORIENTED_EDGE('',*,*,#29179,.F.);
#40285=ORIENTED_EDGE('',*,*,#25618,.T.);
#40286=ORIENTED_EDGE('',*,*,#29178,.T.);
#40287=ORIENTED_EDGE('',*,*,#29161,.F.);
#40288=ORIENTED_EDGE('',*,*,#29180,.F.);
#40289=ORIENTED_EDGE('',*,*,#25619,.T.);
#40290=ORIENTED_EDGE('',*,*,#29179,.T.);
#40291=ORIENTED_EDGE('',*,*,#29160,.F.);
#40292=ORIENTED_EDGE('',*,*,#29181,.F.);
#40293=ORIENTED_EDGE('',*,*,#25620,.T.);
#40294=ORIENTED_EDGE('',*,*,#29180,.T.);
#40295=ORIENTED_EDGE('',*,*,#29159,.F.);
#40296=ORIENTED_EDGE('',*,*,#29182,.F.);
#40297=ORIENTED_EDGE('',*,*,#25621,.T.);
#40298=ORIENTED_EDGE('',*,*,#29181,.T.);
#40299=ORIENTED_EDGE('',*,*,#29158,.F.);
#40300=ORIENTED_EDGE('',*,*,#29183,.F.);
#40301=ORIENTED_EDGE('',*,*,#25622,.T.);
#40302=ORIENTED_EDGE('',*,*,#29182,.T.);
#40303=ORIENTED_EDGE('',*,*,#26856,.T.);
#40304=ORIENTED_EDGE('',*,*,#25623,.T.);
#40305=ORIENTED_EDGE('',*,*,#29183,.T.);
#40306=ORIENTED_EDGE('',*,*,#29157,.F.);
#40307=ORIENTED_EDGE('',*,*,#29184,.F.);
#40308=ORIENTED_EDGE('',*,*,#27398,.T.);
#40309=ORIENTED_EDGE('',*,*,#27271,.T.);
#40310=ORIENTED_EDGE('',*,*,#29185,.F.);
#40311=ORIENTED_EDGE('',*,*,#29186,.F.);
#40312=ORIENTED_EDGE('',*,*,#25626,.T.);
#40313=ORIENTED_EDGE('',*,*,#26893,.T.);
#40314=ORIENTED_EDGE('',*,*,#29187,.F.);
#40315=ORIENTED_EDGE('',*,*,#29188,.F.);
#40316=ORIENTED_EDGE('',*,*,#25627,.T.);
#40317=ORIENTED_EDGE('',*,*,#29186,.T.);
#40318=ORIENTED_EDGE('',*,*,#29189,.F.);
#40319=ORIENTED_EDGE('',*,*,#29190,.F.);
#40320=ORIENTED_EDGE('',*,*,#25628,.T.);
#40321=ORIENTED_EDGE('',*,*,#29188,.T.);
#40322=ORIENTED_EDGE('',*,*,#29191,.F.);
#40323=ORIENTED_EDGE('',*,*,#29192,.F.);
#40324=ORIENTED_EDGE('',*,*,#25629,.T.);
#40325=ORIENTED_EDGE('',*,*,#29190,.T.);
#40326=ORIENTED_EDGE('',*,*,#29193,.F.);
#40327=ORIENTED_EDGE('',*,*,#29194,.F.);
#40328=ORIENTED_EDGE('',*,*,#25630,.T.);
#40329=ORIENTED_EDGE('',*,*,#29192,.T.);
#40330=ORIENTED_EDGE('',*,*,#29195,.F.);
#40331=ORIENTED_EDGE('',*,*,#29196,.F.);
#40332=ORIENTED_EDGE('',*,*,#25631,.T.);
#40333=ORIENTED_EDGE('',*,*,#29194,.T.);
#40334=ORIENTED_EDGE('',*,*,#29197,.F.);
#40335=ORIENTED_EDGE('',*,*,#29198,.F.);
#40336=ORIENTED_EDGE('',*,*,#25632,.T.);
#40337=ORIENTED_EDGE('',*,*,#29196,.T.);
#40338=ORIENTED_EDGE('',*,*,#29199,.F.);
#40339=ORIENTED_EDGE('',*,*,#29200,.F.);
#40340=ORIENTED_EDGE('',*,*,#25633,.T.);
#40341=ORIENTED_EDGE('',*,*,#29198,.T.);
#40342=ORIENTED_EDGE('',*,*,#29201,.F.);
#40343=ORIENTED_EDGE('',*,*,#29202,.F.);
#40344=ORIENTED_EDGE('',*,*,#25634,.T.);
#40345=ORIENTED_EDGE('',*,*,#29200,.T.);
#40346=ORIENTED_EDGE('',*,*,#29203,.F.);
#40347=ORIENTED_EDGE('',*,*,#29204,.F.);
#40348=ORIENTED_EDGE('',*,*,#25635,.T.);
#40349=ORIENTED_EDGE('',*,*,#29202,.T.);
#40350=ORIENTED_EDGE('',*,*,#29205,.F.);
#40351=ORIENTED_EDGE('',*,*,#29206,.F.);
#40352=ORIENTED_EDGE('',*,*,#25636,.T.);
#40353=ORIENTED_EDGE('',*,*,#29204,.T.);
#40354=ORIENTED_EDGE('',*,*,#29207,.F.);
#40355=ORIENTED_EDGE('',*,*,#29208,.F.);
#40356=ORIENTED_EDGE('',*,*,#25637,.T.);
#40357=ORIENTED_EDGE('',*,*,#29206,.T.);
#40358=ORIENTED_EDGE('',*,*,#29209,.F.);
#40359=ORIENTED_EDGE('',*,*,#27245,.F.);
#40360=ORIENTED_EDGE('',*,*,#25638,.T.);
#40361=ORIENTED_EDGE('',*,*,#29208,.T.);
#40362=ORIENTED_EDGE('',*,*,#27058,.T.);
#40363=ORIENTED_EDGE('',*,*,#27248,.F.);
#40364=ORIENTED_EDGE('',*,*,#27492,.F.);
#40365=ORIENTED_EDGE('',*,*,#25641,.F.);
#40366=ORIENTED_EDGE('',*,*,#27246,.T.);
#40367=ORIENTED_EDGE('',*,*,#29209,.T.);
#40368=ORIENTED_EDGE('',*,*,#29207,.T.);
#40369=ORIENTED_EDGE('',*,*,#29205,.T.);
#40370=ORIENTED_EDGE('',*,*,#29203,.T.);
#40371=ORIENTED_EDGE('',*,*,#29201,.T.);
#40372=ORIENTED_EDGE('',*,*,#29199,.T.);
#40373=ORIENTED_EDGE('',*,*,#29197,.T.);
#40374=ORIENTED_EDGE('',*,*,#29195,.T.);
#40375=ORIENTED_EDGE('',*,*,#29193,.T.);
#40376=ORIENTED_EDGE('',*,*,#29191,.T.);
#40377=ORIENTED_EDGE('',*,*,#29189,.T.);
#40378=ORIENTED_EDGE('',*,*,#29187,.T.);
#40379=ORIENTED_EDGE('',*,*,#29185,.T.);
#40380=ORIENTED_EDGE('',*,*,#26892,.T.);
#40381=ORIENTED_EDGE('',*,*,#29210,.F.);
#40382=ORIENTED_EDGE('',*,*,#29211,.T.);
#40383=ORIENTED_EDGE('',*,*,#29212,.T.);
#40384=ORIENTED_EDGE('',*,*,#29213,.T.);
#40385=ORIENTED_EDGE('',*,*,#29214,.T.);
#40386=ORIENTED_EDGE('',*,*,#29215,.T.);
#40387=ORIENTED_EDGE('',*,*,#29216,.T.);
#40388=ORIENTED_EDGE('',*,*,#29217,.T.);
#40389=ORIENTED_EDGE('',*,*,#29218,.T.);
#40390=ORIENTED_EDGE('',*,*,#29219,.T.);
#40391=ORIENTED_EDGE('',*,*,#29220,.T.);
#40392=ORIENTED_EDGE('',*,*,#29221,.T.);
#40393=ORIENTED_EDGE('',*,*,#29222,.T.);
#40394=ORIENTED_EDGE('',*,*,#29223,.T.);
#40395=ORIENTED_EDGE('',*,*,#29224,.T.);
#40396=ORIENTED_EDGE('',*,*,#25607,.T.);
#40397=ORIENTED_EDGE('',*,*,#27493,.T.);
#40398=ORIENTED_EDGE('',*,*,#29224,.F.);
#40399=ORIENTED_EDGE('',*,*,#29225,.F.);
#40400=ORIENTED_EDGE('',*,*,#25574,.T.);
#40401=ORIENTED_EDGE('',*,*,#25608,.T.);
#40402=ORIENTED_EDGE('',*,*,#29223,.F.);
#40403=ORIENTED_EDGE('',*,*,#29226,.F.);
#40404=ORIENTED_EDGE('',*,*,#25575,.T.);
#40405=ORIENTED_EDGE('',*,*,#29225,.T.);
#40406=ORIENTED_EDGE('',*,*,#29222,.F.);
#40407=ORIENTED_EDGE('',*,*,#29227,.F.);
#40408=ORIENTED_EDGE('',*,*,#25576,.T.);
#40409=ORIENTED_EDGE('',*,*,#29226,.T.);
#40410=ORIENTED_EDGE('',*,*,#29221,.F.);
#40411=ORIENTED_EDGE('',*,*,#29228,.F.);
#40412=ORIENTED_EDGE('',*,*,#25577,.T.);
#40413=ORIENTED_EDGE('',*,*,#29227,.T.);
#40414=ORIENTED_EDGE('',*,*,#29220,.F.);
#40415=ORIENTED_EDGE('',*,*,#29229,.F.);
#40416=ORIENTED_EDGE('',*,*,#25578,.T.);
#40417=ORIENTED_EDGE('',*,*,#29228,.T.);
#40418=ORIENTED_EDGE('',*,*,#29219,.F.);
#40419=ORIENTED_EDGE('',*,*,#29230,.F.);
#40420=ORIENTED_EDGE('',*,*,#25579,.T.);
#40421=ORIENTED_EDGE('',*,*,#29229,.T.);
#40422=ORIENTED_EDGE('',*,*,#29218,.F.);
#40423=ORIENTED_EDGE('',*,*,#29231,.F.);
#40424=ORIENTED_EDGE('',*,*,#25580,.T.);
#40425=ORIENTED_EDGE('',*,*,#29230,.T.);
#40426=ORIENTED_EDGE('',*,*,#29217,.F.);
#40427=ORIENTED_EDGE('',*,*,#29232,.F.);
#40428=ORIENTED_EDGE('',*,*,#25581,.T.);
#40429=ORIENTED_EDGE('',*,*,#29231,.T.);
#40430=ORIENTED_EDGE('',*,*,#29216,.F.);
#40431=ORIENTED_EDGE('',*,*,#29233,.F.);
#40432=ORIENTED_EDGE('',*,*,#25582,.T.);
#40433=ORIENTED_EDGE('',*,*,#29232,.T.);
#40434=ORIENTED_EDGE('',*,*,#29215,.F.);
#40435=ORIENTED_EDGE('',*,*,#29234,.F.);
#40436=ORIENTED_EDGE('',*,*,#25583,.T.);
#40437=ORIENTED_EDGE('',*,*,#29233,.T.);
#40438=ORIENTED_EDGE('',*,*,#29214,.F.);
#40439=ORIENTED_EDGE('',*,*,#29235,.F.);
#40440=ORIENTED_EDGE('',*,*,#25584,.T.);
#40441=ORIENTED_EDGE('',*,*,#29234,.T.);
#40442=ORIENTED_EDGE('',*,*,#29213,.F.);
#40443=ORIENTED_EDGE('',*,*,#29236,.F.);
#40444=ORIENTED_EDGE('',*,*,#25585,.T.);
#40445=ORIENTED_EDGE('',*,*,#29235,.T.);
#40446=ORIENTED_EDGE('',*,*,#29212,.F.);
#40447=ORIENTED_EDGE('',*,*,#29237,.F.);
#40448=ORIENTED_EDGE('',*,*,#25586,.T.);
#40449=ORIENTED_EDGE('',*,*,#29236,.T.);
#40450=ORIENTED_EDGE('',*,*,#26859,.T.);
#40451=ORIENTED_EDGE('',*,*,#25587,.T.);
#40452=ORIENTED_EDGE('',*,*,#29237,.T.);
#40453=ORIENTED_EDGE('',*,*,#29211,.F.);
#40454=ORIENTED_EDGE('',*,*,#29238,.F.);
#40455=ORIENTED_EDGE('',*,*,#27400,.T.);
#40456=ORIENTED_EDGE('',*,*,#27269,.T.);
#40457=ORIENTED_EDGE('',*,*,#29239,.F.);
#40458=ORIENTED_EDGE('',*,*,#29240,.F.);
#40459=ORIENTED_EDGE('',*,*,#25590,.T.);
#40460=ORIENTED_EDGE('',*,*,#26888,.T.);
#40461=ORIENTED_EDGE('',*,*,#29241,.F.);
#40462=ORIENTED_EDGE('',*,*,#29242,.F.);
#40463=ORIENTED_EDGE('',*,*,#25591,.T.);
#40464=ORIENTED_EDGE('',*,*,#29240,.T.);
#40465=ORIENTED_EDGE('',*,*,#29243,.F.);
#40466=ORIENTED_EDGE('',*,*,#29244,.F.);
#40467=ORIENTED_EDGE('',*,*,#25592,.T.);
#40468=ORIENTED_EDGE('',*,*,#29242,.T.);
#40469=ORIENTED_EDGE('',*,*,#29245,.F.);
#40470=ORIENTED_EDGE('',*,*,#29246,.F.);
#40471=ORIENTED_EDGE('',*,*,#25593,.T.);
#40472=ORIENTED_EDGE('',*,*,#29244,.T.);
#40473=ORIENTED_EDGE('',*,*,#29247,.F.);
#40474=ORIENTED_EDGE('',*,*,#29248,.F.);
#40475=ORIENTED_EDGE('',*,*,#25594,.T.);
#40476=ORIENTED_EDGE('',*,*,#29246,.T.);
#40477=ORIENTED_EDGE('',*,*,#29249,.F.);
#40478=ORIENTED_EDGE('',*,*,#29250,.F.);
#40479=ORIENTED_EDGE('',*,*,#25595,.T.);
#40480=ORIENTED_EDGE('',*,*,#29248,.T.);
#40481=ORIENTED_EDGE('',*,*,#29251,.F.);
#40482=ORIENTED_EDGE('',*,*,#29252,.F.);
#40483=ORIENTED_EDGE('',*,*,#25596,.T.);
#40484=ORIENTED_EDGE('',*,*,#29250,.T.);
#40485=ORIENTED_EDGE('',*,*,#29253,.F.);
#40486=ORIENTED_EDGE('',*,*,#29254,.F.);
#40487=ORIENTED_EDGE('',*,*,#25597,.T.);
#40488=ORIENTED_EDGE('',*,*,#29252,.T.);
#40489=ORIENTED_EDGE('',*,*,#29255,.F.);
#40490=ORIENTED_EDGE('',*,*,#29256,.F.);
#40491=ORIENTED_EDGE('',*,*,#25598,.T.);
#40492=ORIENTED_EDGE('',*,*,#29254,.T.);
#40493=ORIENTED_EDGE('',*,*,#29257,.F.);
#40494=ORIENTED_EDGE('',*,*,#29258,.F.);
#40495=ORIENTED_EDGE('',*,*,#25599,.T.);
#40496=ORIENTED_EDGE('',*,*,#29256,.T.);
#40497=ORIENTED_EDGE('',*,*,#29259,.F.);
#40498=ORIENTED_EDGE('',*,*,#29260,.F.);
#40499=ORIENTED_EDGE('',*,*,#25600,.T.);
#40500=ORIENTED_EDGE('',*,*,#29258,.T.);
#40501=ORIENTED_EDGE('',*,*,#29261,.F.);
#40502=ORIENTED_EDGE('',*,*,#29262,.F.);
#40503=ORIENTED_EDGE('',*,*,#25601,.T.);
#40504=ORIENTED_EDGE('',*,*,#29260,.T.);
#40505=ORIENTED_EDGE('',*,*,#29263,.F.);
#40506=ORIENTED_EDGE('',*,*,#27249,.F.);
#40507=ORIENTED_EDGE('',*,*,#25602,.T.);
#40508=ORIENTED_EDGE('',*,*,#29262,.T.);
#40509=ORIENTED_EDGE('',*,*,#27056,.T.);
#40510=ORIENTED_EDGE('',*,*,#27252,.F.);
#40511=ORIENTED_EDGE('',*,*,#27494,.F.);
#40512=ORIENTED_EDGE('',*,*,#25605,.F.);
#40513=ORIENTED_EDGE('',*,*,#27250,.T.);
#40514=ORIENTED_EDGE('',*,*,#29263,.T.);
#40515=ORIENTED_EDGE('',*,*,#29261,.T.);
#40516=ORIENTED_EDGE('',*,*,#29259,.T.);
#40517=ORIENTED_EDGE('',*,*,#29257,.T.);
#40518=ORIENTED_EDGE('',*,*,#29255,.T.);
#40519=ORIENTED_EDGE('',*,*,#29253,.T.);
#40520=ORIENTED_EDGE('',*,*,#29251,.T.);
#40521=ORIENTED_EDGE('',*,*,#29249,.T.);
#40522=ORIENTED_EDGE('',*,*,#29247,.T.);
#40523=ORIENTED_EDGE('',*,*,#29245,.T.);
#40524=ORIENTED_EDGE('',*,*,#29243,.T.);
#40525=ORIENTED_EDGE('',*,*,#29241,.T.);
#40526=ORIENTED_EDGE('',*,*,#29239,.T.);
#40527=ORIENTED_EDGE('',*,*,#26887,.T.);
#40528=ORIENTED_EDGE('',*,*,#29264,.F.);
#40529=ORIENTED_EDGE('',*,*,#29265,.T.);
#40530=ORIENTED_EDGE('',*,*,#29266,.T.);
#40531=ORIENTED_EDGE('',*,*,#29267,.T.);
#40532=ORIENTED_EDGE('',*,*,#29268,.T.);
#40533=ORIENTED_EDGE('',*,*,#29269,.T.);
#40534=ORIENTED_EDGE('',*,*,#29270,.T.);
#40535=ORIENTED_EDGE('',*,*,#29271,.T.);
#40536=ORIENTED_EDGE('',*,*,#29272,.T.);
#40537=ORIENTED_EDGE('',*,*,#29273,.T.);
#40538=ORIENTED_EDGE('',*,*,#29274,.T.);
#40539=ORIENTED_EDGE('',*,*,#29275,.T.);
#40540=ORIENTED_EDGE('',*,*,#29276,.T.);
#40541=ORIENTED_EDGE('',*,*,#29277,.T.);
#40542=ORIENTED_EDGE('',*,*,#29278,.T.);
#40543=ORIENTED_EDGE('',*,*,#25571,.T.);
#40544=ORIENTED_EDGE('',*,*,#27495,.T.);
#40545=ORIENTED_EDGE('',*,*,#29278,.F.);
#40546=ORIENTED_EDGE('',*,*,#29279,.F.);
#40547=ORIENTED_EDGE('',*,*,#25538,.T.);
#40548=ORIENTED_EDGE('',*,*,#25572,.T.);
#40549=ORIENTED_EDGE('',*,*,#29277,.F.);
#40550=ORIENTED_EDGE('',*,*,#29280,.F.);
#40551=ORIENTED_EDGE('',*,*,#25539,.T.);
#40552=ORIENTED_EDGE('',*,*,#29279,.T.);
#40553=ORIENTED_EDGE('',*,*,#29276,.F.);
#40554=ORIENTED_EDGE('',*,*,#29281,.F.);
#40555=ORIENTED_EDGE('',*,*,#25540,.T.);
#40556=ORIENTED_EDGE('',*,*,#29280,.T.);
#40557=ORIENTED_EDGE('',*,*,#29275,.F.);
#40558=ORIENTED_EDGE('',*,*,#29282,.F.);
#40559=ORIENTED_EDGE('',*,*,#25541,.T.);
#40560=ORIENTED_EDGE('',*,*,#29281,.T.);
#40561=ORIENTED_EDGE('',*,*,#29274,.F.);
#40562=ORIENTED_EDGE('',*,*,#29283,.F.);
#40563=ORIENTED_EDGE('',*,*,#25542,.T.);
#40564=ORIENTED_EDGE('',*,*,#29282,.T.);
#40565=ORIENTED_EDGE('',*,*,#29273,.F.);
#40566=ORIENTED_EDGE('',*,*,#29284,.F.);
#40567=ORIENTED_EDGE('',*,*,#25543,.T.);
#40568=ORIENTED_EDGE('',*,*,#29283,.T.);
#40569=ORIENTED_EDGE('',*,*,#29272,.F.);
#40570=ORIENTED_EDGE('',*,*,#29285,.F.);
#40571=ORIENTED_EDGE('',*,*,#25544,.T.);
#40572=ORIENTED_EDGE('',*,*,#29284,.T.);
#40573=ORIENTED_EDGE('',*,*,#29271,.F.);
#40574=ORIENTED_EDGE('',*,*,#29286,.F.);
#40575=ORIENTED_EDGE('',*,*,#25545,.T.);
#40576=ORIENTED_EDGE('',*,*,#29285,.T.);
#40577=ORIENTED_EDGE('',*,*,#29270,.F.);
#40578=ORIENTED_EDGE('',*,*,#29287,.F.);
#40579=ORIENTED_EDGE('',*,*,#25546,.T.);
#40580=ORIENTED_EDGE('',*,*,#29286,.T.);
#40581=ORIENTED_EDGE('',*,*,#29269,.F.);
#40582=ORIENTED_EDGE('',*,*,#29288,.F.);
#40583=ORIENTED_EDGE('',*,*,#25547,.T.);
#40584=ORIENTED_EDGE('',*,*,#29287,.T.);
#40585=ORIENTED_EDGE('',*,*,#29268,.F.);
#40586=ORIENTED_EDGE('',*,*,#29289,.F.);
#40587=ORIENTED_EDGE('',*,*,#25548,.T.);
#40588=ORIENTED_EDGE('',*,*,#29288,.T.);
#40589=ORIENTED_EDGE('',*,*,#29267,.F.);
#40590=ORIENTED_EDGE('',*,*,#29290,.F.);
#40591=ORIENTED_EDGE('',*,*,#25549,.T.);
#40592=ORIENTED_EDGE('',*,*,#29289,.T.);
#40593=ORIENTED_EDGE('',*,*,#29266,.F.);
#40594=ORIENTED_EDGE('',*,*,#29291,.F.);
#40595=ORIENTED_EDGE('',*,*,#25550,.T.);
#40596=ORIENTED_EDGE('',*,*,#29290,.T.);
#40597=ORIENTED_EDGE('',*,*,#26862,.T.);
#40598=ORIENTED_EDGE('',*,*,#25551,.T.);
#40599=ORIENTED_EDGE('',*,*,#29291,.T.);
#40600=ORIENTED_EDGE('',*,*,#29265,.F.);
#40601=ORIENTED_EDGE('',*,*,#29292,.F.);
#40602=ORIENTED_EDGE('',*,*,#27402,.T.);
#40603=ORIENTED_EDGE('',*,*,#27267,.T.);
#40604=ORIENTED_EDGE('',*,*,#29293,.F.);
#40605=ORIENTED_EDGE('',*,*,#29294,.F.);
#40606=ORIENTED_EDGE('',*,*,#25554,.T.);
#40607=ORIENTED_EDGE('',*,*,#26883,.T.);
#40608=ORIENTED_EDGE('',*,*,#29295,.F.);
#40609=ORIENTED_EDGE('',*,*,#29296,.F.);
#40610=ORIENTED_EDGE('',*,*,#25555,.T.);
#40611=ORIENTED_EDGE('',*,*,#29294,.T.);
#40612=ORIENTED_EDGE('',*,*,#29297,.F.);
#40613=ORIENTED_EDGE('',*,*,#29298,.F.);
#40614=ORIENTED_EDGE('',*,*,#25556,.T.);
#40615=ORIENTED_EDGE('',*,*,#29296,.T.);
#40616=ORIENTED_EDGE('',*,*,#29299,.F.);
#40617=ORIENTED_EDGE('',*,*,#29300,.F.);
#40618=ORIENTED_EDGE('',*,*,#25557,.T.);
#40619=ORIENTED_EDGE('',*,*,#29298,.T.);
#40620=ORIENTED_EDGE('',*,*,#29301,.F.);
#40621=ORIENTED_EDGE('',*,*,#29302,.F.);
#40622=ORIENTED_EDGE('',*,*,#25558,.T.);
#40623=ORIENTED_EDGE('',*,*,#29300,.T.);
#40624=ORIENTED_EDGE('',*,*,#29303,.F.);
#40625=ORIENTED_EDGE('',*,*,#29304,.F.);
#40626=ORIENTED_EDGE('',*,*,#25559,.T.);
#40627=ORIENTED_EDGE('',*,*,#29302,.T.);
#40628=ORIENTED_EDGE('',*,*,#29305,.F.);
#40629=ORIENTED_EDGE('',*,*,#29306,.F.);
#40630=ORIENTED_EDGE('',*,*,#25560,.T.);
#40631=ORIENTED_EDGE('',*,*,#29304,.T.);
#40632=ORIENTED_EDGE('',*,*,#29307,.F.);
#40633=ORIENTED_EDGE('',*,*,#29308,.F.);
#40634=ORIENTED_EDGE('',*,*,#25561,.T.);
#40635=ORIENTED_EDGE('',*,*,#29306,.T.);
#40636=ORIENTED_EDGE('',*,*,#29309,.F.);
#40637=ORIENTED_EDGE('',*,*,#29310,.F.);
#40638=ORIENTED_EDGE('',*,*,#25562,.T.);
#40639=ORIENTED_EDGE('',*,*,#29308,.T.);
#40640=ORIENTED_EDGE('',*,*,#29311,.F.);
#40641=ORIENTED_EDGE('',*,*,#29312,.F.);
#40642=ORIENTED_EDGE('',*,*,#25563,.T.);
#40643=ORIENTED_EDGE('',*,*,#29310,.T.);
#40644=ORIENTED_EDGE('',*,*,#29313,.F.);
#40645=ORIENTED_EDGE('',*,*,#29314,.F.);
#40646=ORIENTED_EDGE('',*,*,#25564,.T.);
#40647=ORIENTED_EDGE('',*,*,#29312,.T.);
#40648=ORIENTED_EDGE('',*,*,#29315,.F.);
#40649=ORIENTED_EDGE('',*,*,#29316,.F.);
#40650=ORIENTED_EDGE('',*,*,#25565,.T.);
#40651=ORIENTED_EDGE('',*,*,#29314,.T.);
#40652=ORIENTED_EDGE('',*,*,#29317,.F.);
#40653=ORIENTED_EDGE('',*,*,#27253,.F.);
#40654=ORIENTED_EDGE('',*,*,#25566,.T.);
#40655=ORIENTED_EDGE('',*,*,#29316,.T.);
#40656=ORIENTED_EDGE('',*,*,#27054,.T.);
#40657=ORIENTED_EDGE('',*,*,#27256,.F.);
#40658=ORIENTED_EDGE('',*,*,#27496,.F.);
#40659=ORIENTED_EDGE('',*,*,#25569,.F.);
#40660=ORIENTED_EDGE('',*,*,#27254,.T.);
#40661=ORIENTED_EDGE('',*,*,#29317,.T.);
#40662=ORIENTED_EDGE('',*,*,#29315,.T.);
#40663=ORIENTED_EDGE('',*,*,#29313,.T.);
#40664=ORIENTED_EDGE('',*,*,#29311,.T.);
#40665=ORIENTED_EDGE('',*,*,#29309,.T.);
#40666=ORIENTED_EDGE('',*,*,#29307,.T.);
#40667=ORIENTED_EDGE('',*,*,#29305,.T.);
#40668=ORIENTED_EDGE('',*,*,#29303,.T.);
#40669=ORIENTED_EDGE('',*,*,#29301,.T.);
#40670=ORIENTED_EDGE('',*,*,#29299,.T.);
#40671=ORIENTED_EDGE('',*,*,#29297,.T.);
#40672=ORIENTED_EDGE('',*,*,#29295,.T.);
#40673=ORIENTED_EDGE('',*,*,#29293,.T.);
#40674=ORIENTED_EDGE('',*,*,#26882,.T.);
#40675=ORIENTED_EDGE('',*,*,#29318,.F.);
#40676=ORIENTED_EDGE('',*,*,#29319,.T.);
#40677=ORIENTED_EDGE('',*,*,#29320,.T.);
#40678=ORIENTED_EDGE('',*,*,#29321,.T.);
#40679=ORIENTED_EDGE('',*,*,#29322,.T.);
#40680=ORIENTED_EDGE('',*,*,#29323,.T.);
#40681=ORIENTED_EDGE('',*,*,#29324,.T.);
#40682=ORIENTED_EDGE('',*,*,#29325,.T.);
#40683=ORIENTED_EDGE('',*,*,#29326,.T.);
#40684=ORIENTED_EDGE('',*,*,#29327,.T.);
#40685=ORIENTED_EDGE('',*,*,#29328,.T.);
#40686=ORIENTED_EDGE('',*,*,#29329,.T.);
#40687=ORIENTED_EDGE('',*,*,#29330,.T.);
#40688=ORIENTED_EDGE('',*,*,#29331,.T.);
#40689=ORIENTED_EDGE('',*,*,#29332,.T.);
#40690=ORIENTED_EDGE('',*,*,#25535,.T.);
#40691=ORIENTED_EDGE('',*,*,#27497,.T.);
#40692=ORIENTED_EDGE('',*,*,#29332,.F.);
#40693=ORIENTED_EDGE('',*,*,#29333,.F.);
#40694=ORIENTED_EDGE('',*,*,#25502,.T.);
#40695=ORIENTED_EDGE('',*,*,#25536,.T.);
#40696=ORIENTED_EDGE('',*,*,#29331,.F.);
#40697=ORIENTED_EDGE('',*,*,#29334,.F.);
#40698=ORIENTED_EDGE('',*,*,#25503,.T.);
#40699=ORIENTED_EDGE('',*,*,#29333,.T.);
#40700=ORIENTED_EDGE('',*,*,#29330,.F.);
#40701=ORIENTED_EDGE('',*,*,#29335,.F.);
#40702=ORIENTED_EDGE('',*,*,#25504,.T.);
#40703=ORIENTED_EDGE('',*,*,#29334,.T.);
#40704=ORIENTED_EDGE('',*,*,#29329,.F.);
#40705=ORIENTED_EDGE('',*,*,#29336,.F.);
#40706=ORIENTED_EDGE('',*,*,#25505,.T.);
#40707=ORIENTED_EDGE('',*,*,#29335,.T.);
#40708=ORIENTED_EDGE('',*,*,#29328,.F.);
#40709=ORIENTED_EDGE('',*,*,#29337,.F.);
#40710=ORIENTED_EDGE('',*,*,#25506,.T.);
#40711=ORIENTED_EDGE('',*,*,#29336,.T.);
#40712=ORIENTED_EDGE('',*,*,#29327,.F.);
#40713=ORIENTED_EDGE('',*,*,#29338,.F.);
#40714=ORIENTED_EDGE('',*,*,#25507,.T.);
#40715=ORIENTED_EDGE('',*,*,#29337,.T.);
#40716=ORIENTED_EDGE('',*,*,#29326,.F.);
#40717=ORIENTED_EDGE('',*,*,#29339,.F.);
#40718=ORIENTED_EDGE('',*,*,#25508,.T.);
#40719=ORIENTED_EDGE('',*,*,#29338,.T.);
#40720=ORIENTED_EDGE('',*,*,#29325,.F.);
#40721=ORIENTED_EDGE('',*,*,#29340,.F.);
#40722=ORIENTED_EDGE('',*,*,#25509,.T.);
#40723=ORIENTED_EDGE('',*,*,#29339,.T.);
#40724=ORIENTED_EDGE('',*,*,#29324,.F.);
#40725=ORIENTED_EDGE('',*,*,#29341,.F.);
#40726=ORIENTED_EDGE('',*,*,#25510,.T.);
#40727=ORIENTED_EDGE('',*,*,#29340,.T.);
#40728=ORIENTED_EDGE('',*,*,#29323,.F.);
#40729=ORIENTED_EDGE('',*,*,#29342,.F.);
#40730=ORIENTED_EDGE('',*,*,#25511,.T.);
#40731=ORIENTED_EDGE('',*,*,#29341,.T.);
#40732=ORIENTED_EDGE('',*,*,#29322,.F.);
#40733=ORIENTED_EDGE('',*,*,#29343,.F.);
#40734=ORIENTED_EDGE('',*,*,#25512,.T.);
#40735=ORIENTED_EDGE('',*,*,#29342,.T.);
#40736=ORIENTED_EDGE('',*,*,#29321,.F.);
#40737=ORIENTED_EDGE('',*,*,#29344,.F.);
#40738=ORIENTED_EDGE('',*,*,#25513,.T.);
#40739=ORIENTED_EDGE('',*,*,#29343,.T.);
#40740=ORIENTED_EDGE('',*,*,#29320,.F.);
#40741=ORIENTED_EDGE('',*,*,#29345,.F.);
#40742=ORIENTED_EDGE('',*,*,#25514,.T.);
#40743=ORIENTED_EDGE('',*,*,#29344,.T.);
#40744=ORIENTED_EDGE('',*,*,#26865,.T.);
#40745=ORIENTED_EDGE('',*,*,#25515,.T.);
#40746=ORIENTED_EDGE('',*,*,#29345,.T.);
#40747=ORIENTED_EDGE('',*,*,#29319,.F.);
#40748=ORIENTED_EDGE('',*,*,#29346,.F.);
#40749=ORIENTED_EDGE('',*,*,#27404,.T.);
#40750=ORIENTED_EDGE('',*,*,#27265,.T.);
#40751=ORIENTED_EDGE('',*,*,#29347,.F.);
#40752=ORIENTED_EDGE('',*,*,#29348,.F.);
#40753=ORIENTED_EDGE('',*,*,#25518,.T.);
#40754=ORIENTED_EDGE('',*,*,#26878,.T.);
#40755=ORIENTED_EDGE('',*,*,#29349,.F.);
#40756=ORIENTED_EDGE('',*,*,#29350,.F.);
#40757=ORIENTED_EDGE('',*,*,#25519,.T.);
#40758=ORIENTED_EDGE('',*,*,#29348,.T.);
#40759=ORIENTED_EDGE('',*,*,#29351,.F.);
#40760=ORIENTED_EDGE('',*,*,#29352,.F.);
#40761=ORIENTED_EDGE('',*,*,#25520,.T.);
#40762=ORIENTED_EDGE('',*,*,#29350,.T.);
#40763=ORIENTED_EDGE('',*,*,#29353,.F.);
#40764=ORIENTED_EDGE('',*,*,#29354,.F.);
#40765=ORIENTED_EDGE('',*,*,#25521,.T.);
#40766=ORIENTED_EDGE('',*,*,#29352,.T.);
#40767=ORIENTED_EDGE('',*,*,#29355,.F.);
#40768=ORIENTED_EDGE('',*,*,#29356,.F.);
#40769=ORIENTED_EDGE('',*,*,#25522,.T.);
#40770=ORIENTED_EDGE('',*,*,#29354,.T.);
#40771=ORIENTED_EDGE('',*,*,#29357,.F.);
#40772=ORIENTED_EDGE('',*,*,#29358,.F.);
#40773=ORIENTED_EDGE('',*,*,#25523,.T.);
#40774=ORIENTED_EDGE('',*,*,#29356,.T.);
#40775=ORIENTED_EDGE('',*,*,#29359,.F.);
#40776=ORIENTED_EDGE('',*,*,#29360,.F.);
#40777=ORIENTED_EDGE('',*,*,#25524,.T.);
#40778=ORIENTED_EDGE('',*,*,#29358,.T.);
#40779=ORIENTED_EDGE('',*,*,#29361,.F.);
#40780=ORIENTED_EDGE('',*,*,#29362,.F.);
#40781=ORIENTED_EDGE('',*,*,#25525,.T.);
#40782=ORIENTED_EDGE('',*,*,#29360,.T.);
#40783=ORIENTED_EDGE('',*,*,#29363,.F.);
#40784=ORIENTED_EDGE('',*,*,#29364,.F.);
#40785=ORIENTED_EDGE('',*,*,#25526,.T.);
#40786=ORIENTED_EDGE('',*,*,#29362,.T.);
#40787=ORIENTED_EDGE('',*,*,#29365,.F.);
#40788=ORIENTED_EDGE('',*,*,#29366,.F.);
#40789=ORIENTED_EDGE('',*,*,#25527,.T.);
#40790=ORIENTED_EDGE('',*,*,#29364,.T.);
#40791=ORIENTED_EDGE('',*,*,#29367,.F.);
#40792=ORIENTED_EDGE('',*,*,#29368,.F.);
#40793=ORIENTED_EDGE('',*,*,#25528,.T.);
#40794=ORIENTED_EDGE('',*,*,#29366,.T.);
#40795=ORIENTED_EDGE('',*,*,#29369,.F.);
#40796=ORIENTED_EDGE('',*,*,#29370,.F.);
#40797=ORIENTED_EDGE('',*,*,#25529,.T.);
#40798=ORIENTED_EDGE('',*,*,#29368,.T.);
#40799=ORIENTED_EDGE('',*,*,#29371,.F.);
#40800=ORIENTED_EDGE('',*,*,#27257,.F.);
#40801=ORIENTED_EDGE('',*,*,#25530,.T.);
#40802=ORIENTED_EDGE('',*,*,#29370,.T.);
#40803=ORIENTED_EDGE('',*,*,#27052,.T.);
#40804=ORIENTED_EDGE('',*,*,#27260,.F.);
#40805=ORIENTED_EDGE('',*,*,#27498,.F.);
#40806=ORIENTED_EDGE('',*,*,#25533,.F.);
#40807=ORIENTED_EDGE('',*,*,#27258,.T.);
#40808=ORIENTED_EDGE('',*,*,#29371,.T.);
#40809=ORIENTED_EDGE('',*,*,#29369,.T.);
#40810=ORIENTED_EDGE('',*,*,#29367,.T.);
#40811=ORIENTED_EDGE('',*,*,#29365,.T.);
#40812=ORIENTED_EDGE('',*,*,#29363,.T.);
#40813=ORIENTED_EDGE('',*,*,#29361,.T.);
#40814=ORIENTED_EDGE('',*,*,#29359,.T.);
#40815=ORIENTED_EDGE('',*,*,#29357,.T.);
#40816=ORIENTED_EDGE('',*,*,#29355,.T.);
#40817=ORIENTED_EDGE('',*,*,#29353,.T.);
#40818=ORIENTED_EDGE('',*,*,#29351,.T.);
#40819=ORIENTED_EDGE('',*,*,#29349,.T.);
#40820=ORIENTED_EDGE('',*,*,#29347,.T.);
#40821=ORIENTED_EDGE('',*,*,#26877,.T.);
#40822=ORIENTED_EDGE('',*,*,#29372,.F.);
#40823=ORIENTED_EDGE('',*,*,#29373,.T.);
#40824=ORIENTED_EDGE('',*,*,#29374,.T.);
#40825=ORIENTED_EDGE('',*,*,#29375,.T.);
#40826=ORIENTED_EDGE('',*,*,#29376,.T.);
#40827=ORIENTED_EDGE('',*,*,#29377,.T.);
#40828=ORIENTED_EDGE('',*,*,#29378,.T.);
#40829=ORIENTED_EDGE('',*,*,#29379,.T.);
#40830=ORIENTED_EDGE('',*,*,#29380,.T.);
#40831=ORIENTED_EDGE('',*,*,#29381,.T.);
#40832=ORIENTED_EDGE('',*,*,#29382,.T.);
#40833=ORIENTED_EDGE('',*,*,#29383,.T.);
#40834=ORIENTED_EDGE('',*,*,#29384,.T.);
#40835=ORIENTED_EDGE('',*,*,#29385,.T.);
#40836=ORIENTED_EDGE('',*,*,#29386,.T.);
#40837=ORIENTED_EDGE('',*,*,#25499,.T.);
#40838=ORIENTED_EDGE('',*,*,#27499,.T.);
#40839=ORIENTED_EDGE('',*,*,#29387,.F.);
#40840=ORIENTED_EDGE('',*,*,#29388,.F.);
#40841=ORIENTED_EDGE('',*,*,#25482,.T.);
#40842=ORIENTED_EDGE('',*,*,#26873,.T.);
#40843=ORIENTED_EDGE('',*,*,#29389,.F.);
#40844=ORIENTED_EDGE('',*,*,#29390,.F.);
#40845=ORIENTED_EDGE('',*,*,#25483,.T.);
#40846=ORIENTED_EDGE('',*,*,#29388,.T.);
#40847=ORIENTED_EDGE('',*,*,#29391,.F.);
#40848=ORIENTED_EDGE('',*,*,#29392,.F.);
#40849=ORIENTED_EDGE('',*,*,#25484,.T.);
#40850=ORIENTED_EDGE('',*,*,#29390,.T.);
#40851=ORIENTED_EDGE('',*,*,#29393,.F.);
#40852=ORIENTED_EDGE('',*,*,#29394,.F.);
#40853=ORIENTED_EDGE('',*,*,#25485,.T.);
#40854=ORIENTED_EDGE('',*,*,#29392,.T.);
#40855=ORIENTED_EDGE('',*,*,#29395,.F.);
#40856=ORIENTED_EDGE('',*,*,#29396,.F.);
#40857=ORIENTED_EDGE('',*,*,#25486,.T.);
#40858=ORIENTED_EDGE('',*,*,#29394,.T.);
#40859=ORIENTED_EDGE('',*,*,#29397,.F.);
#40860=ORIENTED_EDGE('',*,*,#29398,.F.);
#40861=ORIENTED_EDGE('',*,*,#25487,.T.);
#40862=ORIENTED_EDGE('',*,*,#29396,.T.);
#40863=ORIENTED_EDGE('',*,*,#29399,.F.);
#40864=ORIENTED_EDGE('',*,*,#29400,.F.);
#40865=ORIENTED_EDGE('',*,*,#25488,.T.);
#40866=ORIENTED_EDGE('',*,*,#29398,.T.);
#40867=ORIENTED_EDGE('',*,*,#29401,.F.);
#40868=ORIENTED_EDGE('',*,*,#29402,.F.);
#40869=ORIENTED_EDGE('',*,*,#25489,.T.);
#40870=ORIENTED_EDGE('',*,*,#29400,.T.);
#40871=ORIENTED_EDGE('',*,*,#29403,.F.);
#40872=ORIENTED_EDGE('',*,*,#29404,.F.);
#40873=ORIENTED_EDGE('',*,*,#25490,.T.);
#40874=ORIENTED_EDGE('',*,*,#29402,.T.);
#40875=ORIENTED_EDGE('',*,*,#29405,.F.);
#40876=ORIENTED_EDGE('',*,*,#29406,.F.);
#40877=ORIENTED_EDGE('',*,*,#25491,.T.);
#40878=ORIENTED_EDGE('',*,*,#29404,.T.);
#40879=ORIENTED_EDGE('',*,*,#29407,.F.);
#40880=ORIENTED_EDGE('',*,*,#29408,.F.);
#40881=ORIENTED_EDGE('',*,*,#25492,.T.);
#40882=ORIENTED_EDGE('',*,*,#29406,.T.);
#40883=ORIENTED_EDGE('',*,*,#29409,.F.);
#40884=ORIENTED_EDGE('',*,*,#29410,.F.);
#40885=ORIENTED_EDGE('',*,*,#25493,.T.);
#40886=ORIENTED_EDGE('',*,*,#29408,.T.);
#40887=ORIENTED_EDGE('',*,*,#29411,.F.);
#40888=ORIENTED_EDGE('',*,*,#29412,.F.);
#40889=ORIENTED_EDGE('',*,*,#25494,.T.);
#40890=ORIENTED_EDGE('',*,*,#29410,.T.);
#40891=ORIENTED_EDGE('',*,*,#25464,.T.);
#40892=ORIENTED_EDGE('',*,*,#25495,.T.);
#40893=ORIENTED_EDGE('',*,*,#29412,.T.);
#40894=ORIENTED_EDGE('',*,*,#29413,.F.);
#40895=ORIENTED_EDGE('',*,*,#27500,.F.);
#40896=ORIENTED_EDGE('',*,*,#27261,.T.);
#40897=ORIENTED_EDGE('',*,*,#27049,.T.);
#40898=ORIENTED_EDGE('',*,*,#29386,.F.);
#40899=ORIENTED_EDGE('',*,*,#29414,.F.);
#40900=ORIENTED_EDGE('',*,*,#25466,.T.);
#40901=ORIENTED_EDGE('',*,*,#25500,.T.);
#40902=ORIENTED_EDGE('',*,*,#29385,.F.);
#40903=ORIENTED_EDGE('',*,*,#29415,.F.);
#40904=ORIENTED_EDGE('',*,*,#25467,.T.);
#40905=ORIENTED_EDGE('',*,*,#29414,.T.);
#40906=ORIENTED_EDGE('',*,*,#29384,.F.);
#40907=ORIENTED_EDGE('',*,*,#29416,.F.);
#40908=ORIENTED_EDGE('',*,*,#25468,.T.);
#40909=ORIENTED_EDGE('',*,*,#29415,.T.);
#40910=ORIENTED_EDGE('',*,*,#29383,.F.);
#40911=ORIENTED_EDGE('',*,*,#29417,.F.);
#40912=ORIENTED_EDGE('',*,*,#25469,.T.);
#40913=ORIENTED_EDGE('',*,*,#29416,.T.);
#40914=ORIENTED_EDGE('',*,*,#29382,.F.);
#40915=ORIENTED_EDGE('',*,*,#29418,.F.);
#40916=ORIENTED_EDGE('',*,*,#25470,.T.);
#40917=ORIENTED_EDGE('',*,*,#29417,.T.);
#40918=ORIENTED_EDGE('',*,*,#29381,.F.);
#40919=ORIENTED_EDGE('',*,*,#29419,.F.);
#40920=ORIENTED_EDGE('',*,*,#25471,.T.);
#40921=ORIENTED_EDGE('',*,*,#29418,.T.);
#40922=ORIENTED_EDGE('',*,*,#29380,.F.);
#40923=ORIENTED_EDGE('',*,*,#29420,.F.);
#40924=ORIENTED_EDGE('',*,*,#25472,.T.);
#40925=ORIENTED_EDGE('',*,*,#29419,.T.);
#40926=ORIENTED_EDGE('',*,*,#29379,.F.);
#40927=ORIENTED_EDGE('',*,*,#29421,.F.);
#40928=ORIENTED_EDGE('',*,*,#25473,.T.);
#40929=ORIENTED_EDGE('',*,*,#29420,.T.);
#40930=ORIENTED_EDGE('',*,*,#29378,.F.);
#40931=ORIENTED_EDGE('',*,*,#29422,.F.);
#40932=ORIENTED_EDGE('',*,*,#25474,.T.);
#40933=ORIENTED_EDGE('',*,*,#29421,.T.);
#40934=ORIENTED_EDGE('',*,*,#29377,.F.);
#40935=ORIENTED_EDGE('',*,*,#29423,.F.);
#40936=ORIENTED_EDGE('',*,*,#25475,.T.);
#40937=ORIENTED_EDGE('',*,*,#29422,.T.);
#40938=ORIENTED_EDGE('',*,*,#29376,.F.);
#40939=ORIENTED_EDGE('',*,*,#29424,.F.);
#40940=ORIENTED_EDGE('',*,*,#25476,.T.);
#40941=ORIENTED_EDGE('',*,*,#29423,.T.);
#40942=ORIENTED_EDGE('',*,*,#29375,.F.);
#40943=ORIENTED_EDGE('',*,*,#29425,.F.);
#40944=ORIENTED_EDGE('',*,*,#25477,.T.);
#40945=ORIENTED_EDGE('',*,*,#29424,.T.);
#40946=ORIENTED_EDGE('',*,*,#29374,.F.);
#40947=ORIENTED_EDGE('',*,*,#29426,.F.);
#40948=ORIENTED_EDGE('',*,*,#25478,.T.);
#40949=ORIENTED_EDGE('',*,*,#29425,.T.);
#40950=ORIENTED_EDGE('',*,*,#26868,.T.);
#40951=ORIENTED_EDGE('',*,*,#25479,.T.);
#40952=ORIENTED_EDGE('',*,*,#29426,.T.);
#40953=ORIENTED_EDGE('',*,*,#29373,.F.);
#40954=ORIENTED_EDGE('',*,*,#29427,.F.);
#40955=ORIENTED_EDGE('',*,*,#27406,.T.);
#40956=ORIENTED_EDGE('',*,*,#27263,.T.);
#40957=ORIENTED_EDGE('',*,*,#27435,.T.);
#40958=ORIENTED_EDGE('',*,*,#29428,.T.);
#40959=ORIENTED_EDGE('',*,*,#26871,.T.);
#40960=ORIENTED_EDGE('',*,*,#27407,.T.);
#40961=ORIENTED_EDGE('',*,*,#29427,.T.);
#40962=ORIENTED_EDGE('',*,*,#29372,.T.);
#40963=ORIENTED_EDGE('',*,*,#26876,.T.);
#40964=ORIENTED_EDGE('',*,*,#27405,.T.);
#40965=ORIENTED_EDGE('',*,*,#29346,.T.);
#40966=ORIENTED_EDGE('',*,*,#29318,.T.);
#40967=ORIENTED_EDGE('',*,*,#26881,.T.);
#40968=ORIENTED_EDGE('',*,*,#27403,.T.);
#40969=ORIENTED_EDGE('',*,*,#29292,.T.);
#40970=ORIENTED_EDGE('',*,*,#29264,.T.);
#40971=ORIENTED_EDGE('',*,*,#26886,.T.);
#40972=ORIENTED_EDGE('',*,*,#27401,.T.);
#40973=ORIENTED_EDGE('',*,*,#29238,.T.);
#40974=ORIENTED_EDGE('',*,*,#29210,.T.);
#40975=ORIENTED_EDGE('',*,*,#26891,.T.);
#40976=ORIENTED_EDGE('',*,*,#27399,.T.);
#40977=ORIENTED_EDGE('',*,*,#29184,.T.);
#40978=ORIENTED_EDGE('',*,*,#29156,.T.);
#40979=ORIENTED_EDGE('',*,*,#26896,.T.);
#40980=ORIENTED_EDGE('',*,*,#27397,.T.);
#40981=ORIENTED_EDGE('',*,*,#29130,.T.);
#40982=ORIENTED_EDGE('',*,*,#29102,.T.);
#40983=ORIENTED_EDGE('',*,*,#26901,.T.);
#40984=ORIENTED_EDGE('',*,*,#27395,.T.);
#40985=ORIENTED_EDGE('',*,*,#29076,.T.);
#40986=ORIENTED_EDGE('',*,*,#29048,.T.);
#40987=ORIENTED_EDGE('',*,*,#26906,.T.);
#40988=ORIENTED_EDGE('',*,*,#27393,.T.);
#40989=ORIENTED_EDGE('',*,*,#29022,.T.);
#40990=ORIENTED_EDGE('',*,*,#28994,.T.);
#40991=ORIENTED_EDGE('',*,*,#26911,.T.);
#40992=ORIENTED_EDGE('',*,*,#27391,.T.);
#40993=ORIENTED_EDGE('',*,*,#28968,.T.);
#40994=ORIENTED_EDGE('',*,*,#28940,.T.);
#40995=ORIENTED_EDGE('',*,*,#26916,.T.);
#40996=ORIENTED_EDGE('',*,*,#27389,.T.);
#40997=ORIENTED_EDGE('',*,*,#28914,.T.);
#40998=ORIENTED_EDGE('',*,*,#28886,.T.);
#40999=ORIENTED_EDGE('',*,*,#26921,.T.);
#41000=ORIENTED_EDGE('',*,*,#27387,.T.);
#41001=ORIENTED_EDGE('',*,*,#28860,.T.);
#41002=ORIENTED_EDGE('',*,*,#28832,.T.);
#41003=ORIENTED_EDGE('',*,*,#26926,.T.);
#41004=ORIENTED_EDGE('',*,*,#27385,.T.);
#41005=ORIENTED_EDGE('',*,*,#28806,.T.);
#41006=ORIENTED_EDGE('',*,*,#28778,.T.);
#41007=ORIENTED_EDGE('',*,*,#26931,.T.);
#41008=ORIENTED_EDGE('',*,*,#27383,.T.);
#41009=ORIENTED_EDGE('',*,*,#28752,.T.);
#41010=ORIENTED_EDGE('',*,*,#28724,.T.);
#41011=ORIENTED_EDGE('',*,*,#26936,.T.);
#41012=ORIENTED_EDGE('',*,*,#27381,.T.);
#41013=ORIENTED_EDGE('',*,*,#28698,.T.);
#41014=ORIENTED_EDGE('',*,*,#28670,.T.);
#41015=ORIENTED_EDGE('',*,*,#26941,.T.);
#41016=ORIENTED_EDGE('',*,*,#27379,.T.);
#41017=ORIENTED_EDGE('',*,*,#28644,.T.);
#41018=ORIENTED_EDGE('',*,*,#28616,.T.);
#41019=ORIENTED_EDGE('',*,*,#26946,.T.);
#41020=ORIENTED_EDGE('',*,*,#27377,.T.);
#41021=ORIENTED_EDGE('',*,*,#28590,.T.);
#41022=ORIENTED_EDGE('',*,*,#28562,.T.);
#41023=ORIENTED_EDGE('',*,*,#26951,.T.);
#41024=ORIENTED_EDGE('',*,*,#27375,.T.);
#41025=ORIENTED_EDGE('',*,*,#28536,.T.);
#41026=ORIENTED_EDGE('',*,*,#28508,.T.);
#41027=ORIENTED_EDGE('',*,*,#26956,.T.);
#41028=ORIENTED_EDGE('',*,*,#27373,.T.);
#41029=ORIENTED_EDGE('',*,*,#28482,.T.);
#41030=ORIENTED_EDGE('',*,*,#28454,.T.);
#41031=ORIENTED_EDGE('',*,*,#26961,.T.);
#41032=ORIENTED_EDGE('',*,*,#27371,.T.);
#41033=ORIENTED_EDGE('',*,*,#29429,.T.);
#41034=ORIENTED_EDGE('',*,*,#29430,.F.);
#41035=ORIENTED_EDGE('',*,*,#29429,.F.);
#41036=ORIENTED_EDGE('',*,*,#27370,.T.);
#41037=ORIENTED_EDGE('',*,*,#28428,.T.);
#41038=ORIENTED_EDGE('',*,*,#28400,.T.);
#41039=ORIENTED_EDGE('',*,*,#26966,.T.);
#41040=ORIENTED_EDGE('',*,*,#27368,.T.);
#41041=ORIENTED_EDGE('',*,*,#28374,.T.);
#41042=ORIENTED_EDGE('',*,*,#28346,.T.);
#41043=ORIENTED_EDGE('',*,*,#26971,.T.);
#41044=ORIENTED_EDGE('',*,*,#27366,.T.);
#41045=ORIENTED_EDGE('',*,*,#28320,.T.);
#41046=ORIENTED_EDGE('',*,*,#28292,.T.);
#41047=ORIENTED_EDGE('',*,*,#26976,.T.);
#41048=ORIENTED_EDGE('',*,*,#27364,.T.);
#41049=ORIENTED_EDGE('',*,*,#28266,.T.);
#41050=ORIENTED_EDGE('',*,*,#28238,.T.);
#41051=ORIENTED_EDGE('',*,*,#26981,.T.);
#41052=ORIENTED_EDGE('',*,*,#27362,.T.);
#41053=ORIENTED_EDGE('',*,*,#28212,.T.);
#41054=ORIENTED_EDGE('',*,*,#28184,.T.);
#41055=ORIENTED_EDGE('',*,*,#26986,.T.);
#41056=ORIENTED_EDGE('',*,*,#27360,.T.);
#41057=ORIENTED_EDGE('',*,*,#28158,.T.);
#41058=ORIENTED_EDGE('',*,*,#28130,.T.);
#41059=ORIENTED_EDGE('',*,*,#26991,.T.);
#41060=ORIENTED_EDGE('',*,*,#27358,.T.);
#41061=ORIENTED_EDGE('',*,*,#28104,.T.);
#41062=ORIENTED_EDGE('',*,*,#28076,.T.);
#41063=ORIENTED_EDGE('',*,*,#26996,.T.);
#41064=ORIENTED_EDGE('',*,*,#27356,.T.);
#41065=ORIENTED_EDGE('',*,*,#28050,.T.);
#41066=ORIENTED_EDGE('',*,*,#28022,.T.);
#41067=ORIENTED_EDGE('',*,*,#27001,.T.);
#41068=ORIENTED_EDGE('',*,*,#27354,.T.);
#41069=ORIENTED_EDGE('',*,*,#27996,.T.);
#41070=ORIENTED_EDGE('',*,*,#27968,.T.);
#41071=ORIENTED_EDGE('',*,*,#27006,.T.);
#41072=ORIENTED_EDGE('',*,*,#27352,.T.);
#41073=ORIENTED_EDGE('',*,*,#27942,.T.);
#41074=ORIENTED_EDGE('',*,*,#27914,.T.);
#41075=ORIENTED_EDGE('',*,*,#27011,.T.);
#41076=ORIENTED_EDGE('',*,*,#27350,.T.);
#41077=ORIENTED_EDGE('',*,*,#27888,.T.);
#41078=ORIENTED_EDGE('',*,*,#27860,.T.);
#41079=ORIENTED_EDGE('',*,*,#27016,.T.);
#41080=ORIENTED_EDGE('',*,*,#27348,.T.);
#41081=ORIENTED_EDGE('',*,*,#27834,.T.);
#41082=ORIENTED_EDGE('',*,*,#27806,.T.);
#41083=ORIENTED_EDGE('',*,*,#27021,.T.);
#41084=ORIENTED_EDGE('',*,*,#27346,.T.);
#41085=ORIENTED_EDGE('',*,*,#27780,.T.);
#41086=ORIENTED_EDGE('',*,*,#27752,.T.);
#41087=ORIENTED_EDGE('',*,*,#27026,.T.);
#41088=ORIENTED_EDGE('',*,*,#27344,.T.);
#41089=ORIENTED_EDGE('',*,*,#27726,.T.);
#41090=ORIENTED_EDGE('',*,*,#27698,.T.);
#41091=ORIENTED_EDGE('',*,*,#27031,.T.);
#41092=ORIENTED_EDGE('',*,*,#27342,.T.);
#41093=ORIENTED_EDGE('',*,*,#27672,.T.);
#41094=ORIENTED_EDGE('',*,*,#27644,.T.);
#41095=ORIENTED_EDGE('',*,*,#27036,.T.);
#41096=ORIENTED_EDGE('',*,*,#27340,.T.);
#41097=ORIENTED_EDGE('',*,*,#27618,.T.);
#41098=ORIENTED_EDGE('',*,*,#27590,.T.);
#41099=ORIENTED_EDGE('',*,*,#27041,.T.);
#41100=ORIENTED_EDGE('',*,*,#27338,.T.);
#41101=ORIENTED_EDGE('',*,*,#27564,.T.);
#41102=ORIENTED_EDGE('',*,*,#27536,.T.);
#41103=ORIENTED_EDGE('',*,*,#27046,.T.);
#41104=ORIENTED_EDGE('',*,*,#27336,.T.);
#41105=ORIENTED_EDGE('',*,*,#29431,.T.);
#41106=ORIENTED_EDGE('',*,*,#29432,.T.);
#41107=ORIENTED_EDGE('',*,*,#29433,.T.);
#41108=ORIENTED_EDGE('',*,*,#29434,.T.);
#41109=ORIENTED_EDGE('',*,*,#29432,.F.);
#41110=ORIENTED_EDGE('',*,*,#29433,.F.);
#41111=ORIENTED_EDGE('',*,*,#29434,.F.);
#41112=ORIENTED_EDGE('',*,*,#29435,.T.);
#41113=ORIENTED_EDGE('',*,*,#29436,.F.);
#41114=ORIENTED_EDGE('',*,*,#29437,.F.);
#41115=ORIENTED_EDGE('',*,*,#29435,.F.);
#41116=ORIENTED_EDGE('',*,*,#29431,.F.);
#41117=ORIENTED_EDGE('',*,*,#27462,.F.);
#41118=ORIENTED_EDGE('',*,*,#29436,.T.);
#41119=ORIENTED_EDGE('',*,*,#29437,.T.);
#41120=ORIENTED_EDGE('',*,*,#29438,.T.);
#41121=ORIENTED_EDGE('',*,*,#29439,.T.);
#41122=ORIENTED_EDGE('',*,*,#29440,.T.);
#41123=ORIENTED_EDGE('',*,*,#29438,.F.);
#41124=ORIENTED_EDGE('',*,*,#29440,.F.);
#41125=ORIENTED_EDGE('',*,*,#29441,.T.);
#41126=ORIENTED_EDGE('',*,*,#29442,.T.);
#41127=ORIENTED_EDGE('',*,*,#29441,.F.);
#41128=ORIENTED_EDGE('',*,*,#29439,.F.);
#41129=ORIENTED_EDGE('',*,*,#29443,.T.);
#41130=ORIENTED_EDGE('',*,*,#29444,.T.);
#41131=ORIENTED_EDGE('',*,*,#29445,.T.);
#41132=ORIENTED_EDGE('',*,*,#29444,.F.);
#41133=ORIENTED_EDGE('',*,*,#29446,.T.);
#41134=ORIENTED_EDGE('',*,*,#29443,.F.);
#41135=ORIENTED_EDGE('',*,*,#29447,.T.);
#41136=ORIENTED_EDGE('',*,*,#29448,.F.);
#41137=ORIENTED_EDGE('',*,*,#29449,.F.);
#41138=ORIENTED_EDGE('',*,*,#29447,.F.);
#41139=ORIENTED_EDGE('',*,*,#29446,.F.);
#41140=ORIENTED_EDGE('',*,*,#29450,.F.);
#41141=ORIENTED_EDGE('',*,*,#29445,.F.);
#41142=ORIENTED_EDGE('',*,*,#29451,.T.);
#41143=ORIENTED_EDGE('',*,*,#29452,.T.);
#41144=ORIENTED_EDGE('',*,*,#29448,.T.);
#41145=ORIENTED_EDGE('',*,*,#29449,.T.);
#41146=ORIENTED_EDGE('',*,*,#29452,.F.);
#41147=ORIENTED_EDGE('',*,*,#29453,.T.);
#41148=ORIENTED_EDGE('',*,*,#29451,.F.);
#41149=ORIENTED_EDGE('',*,*,#26759,.T.);
#41150=ORIENTED_EDGE('',*,*,#27501,.T.);
#41151=ORIENTED_EDGE('',*,*,#29413,.T.);
#41152=ORIENTED_EDGE('',*,*,#29411,.T.);
#41153=ORIENTED_EDGE('',*,*,#29409,.T.);
#41154=ORIENTED_EDGE('',*,*,#29407,.T.);
#41155=ORIENTED_EDGE('',*,*,#29405,.T.);
#41156=ORIENTED_EDGE('',*,*,#29403,.T.);
#41157=ORIENTED_EDGE('',*,*,#29401,.T.);
#41158=ORIENTED_EDGE('',*,*,#29399,.T.);
#41159=ORIENTED_EDGE('',*,*,#29397,.T.);
#41160=ORIENTED_EDGE('',*,*,#29395,.T.);
#41161=ORIENTED_EDGE('',*,*,#29393,.T.);
#41162=ORIENTED_EDGE('',*,*,#29391,.T.);
#41163=ORIENTED_EDGE('',*,*,#29389,.T.);
#41164=ORIENTED_EDGE('',*,*,#29387,.T.);
#41165=ORIENTED_EDGE('',*,*,#26872,.T.);
#41166=ORIENTED_EDGE('',*,*,#29428,.F.);
#41167=ORIENTED_EDGE('',*,*,#27434,.T.);
#41168=ORIENTED_EDGE('',*,*,#27432,.T.);
#41169=ORIENTED_EDGE('',*,*,#27430,.T.);
#41170=ORIENTED_EDGE('',*,*,#27428,.T.);
#41171=ORIENTED_EDGE('',*,*,#27426,.T.);
#41172=ORIENTED_EDGE('',*,*,#27424,.T.);
#41173=ORIENTED_EDGE('',*,*,#27422,.T.);
#41174=ORIENTED_EDGE('',*,*,#27420,.T.);
#41175=ORIENTED_EDGE('',*,*,#27418,.T.);
#41176=ORIENTED_EDGE('',*,*,#27416,.T.);
#41177=ORIENTED_EDGE('',*,*,#27414,.T.);
#41178=ORIENTED_EDGE('',*,*,#27412,.T.);
#41179=ORIENTED_EDGE('',*,*,#27410,.T.);
#41180=ORIENTED_EDGE('',*,*,#27408,.T.);
#41181=ORIENTED_EDGE('',*,*,#29454,.F.);
#41182=ORIENTED_EDGE('',*,*,#29430,.T.);
#41183=ORIENTED_EDGE('',*,*,#29455,.F.);
#41184=ORIENTED_EDGE('',*,*,#29456,.T.);
#41185=ORIENTED_EDGE('',*,*,#29454,.T.);
#41186=ORIENTED_EDGE('',*,*,#29456,.F.);
#41187=ORIENTED_EDGE('',*,*,#29457,.F.);
#41188=ORIENTED_EDGE('',*,*,#29458,.T.);
#41189=ORIENTED_EDGE('',*,*,#29455,.T.);
#41190=ORIENTED_EDGE('',*,*,#29458,.F.);
#41191=ORIENTED_EDGE('',*,*,#29453,.F.);
#41192=ORIENTED_EDGE('',*,*,#29459,.T.);
#41193=ORIENTED_EDGE('',*,*,#29457,.T.);
#41194=ORIENTED_EDGE('',*,*,#29459,.F.);
#41195=ORIENTED_EDGE('',*,*,#29460,.F.);
#41196=ORIENTED_EDGE('',*,*,#29461,.T.);
#41197=ORIENTED_EDGE('',*,*,#29450,.T.);
#41198=ORIENTED_EDGE('',*,*,#29461,.F.);
#41199=ORIENTED_EDGE('',*,*,#29442,.F.);
#41200=ORIENTED_EDGE('',*,*,#29462,.T.);
#41201=ORIENTED_EDGE('',*,*,#29460,.T.);
#41202=ORIENTED_EDGE('',*,*,#29462,.F.);
#41203=ORIENTED_EDGE('',*,*,#29463,.F.);
#41204=ORIENTED_EDGE('',*,*,#29464,.F.);
#41205=ORIENTED_EDGE('',*,*,#29465,.F.);
#41206=ORIENTED_EDGE('',*,*,#29466,.F.);
#41207=ORIENTED_EDGE('',*,*,#29467,.F.);
#41208=ORIENTED_EDGE('',*,*,#29468,.F.);
#41209=ORIENTED_EDGE('',*,*,#29469,.F.);
#41210=ORIENTED_EDGE('',*,*,#29470,.F.);
#41211=ORIENTED_EDGE('',*,*,#29471,.F.);
#41212=ORIENTED_EDGE('',*,*,#29472,.F.);
#41213=ORIENTED_EDGE('',*,*,#29473,.T.);
#41214=ORIENTED_EDGE('',*,*,#29474,.F.);
#41215=ORIENTED_EDGE('',*,*,#29475,.F.);
#41216=ORIENTED_EDGE('',*,*,#29465,.T.);
#41217=ORIENTED_EDGE('',*,*,#29476,.F.);
#41218=ORIENTED_EDGE('',*,*,#29473,.F.);
#41219=ORIENTED_EDGE('',*,*,#29468,.T.);
#41220=ORIENTED_EDGE('',*,*,#29477,.T.);
#41221=ORIENTED_EDGE('',*,*,#29478,.T.);
#41222=ORIENTED_EDGE('',*,*,#29479,.F.);
#41223=ORIENTED_EDGE('',*,*,#29469,.T.);
#41224=ORIENTED_EDGE('',*,*,#29480,.F.);
#41225=ORIENTED_EDGE('',*,*,#29481,.T.);
#41226=ORIENTED_EDGE('',*,*,#29482,.T.);
#41227=ORIENTED_EDGE('',*,*,#29483,.T.);
#41228=ORIENTED_EDGE('',*,*,#29484,.T.);
#41229=ORIENTED_EDGE('',*,*,#29485,.T.);
#41230=ORIENTED_EDGE('',*,*,#29486,.T.);
#41231=ORIENTED_EDGE('',*,*,#29487,.T.);
#41232=ORIENTED_EDGE('',*,*,#29488,.T.);
#41233=ORIENTED_EDGE('',*,*,#29489,.T.);
#41234=ORIENTED_EDGE('',*,*,#29490,.T.);
#41235=ORIENTED_EDGE('',*,*,#29491,.T.);
#41236=ORIENTED_EDGE('',*,*,#29492,.T.);
#41237=ORIENTED_EDGE('',*,*,#29493,.T.);
#41238=ORIENTED_EDGE('',*,*,#29494,.T.);
#41239=ORIENTED_EDGE('',*,*,#29495,.T.);
#41240=ORIENTED_EDGE('',*,*,#29496,.T.);
#41241=ORIENTED_EDGE('',*,*,#29497,.T.);
#41242=ORIENTED_EDGE('',*,*,#29498,.T.);
#41243=ORIENTED_EDGE('',*,*,#29499,.T.);
#41244=ORIENTED_EDGE('',*,*,#29500,.T.);
#41245=ORIENTED_EDGE('',*,*,#29501,.T.);
#41246=ORIENTED_EDGE('',*,*,#29502,.T.);
#41247=ORIENTED_EDGE('',*,*,#29503,.T.);
#41248=ORIENTED_EDGE('',*,*,#29504,.T.);
#41249=ORIENTED_EDGE('',*,*,#29505,.T.);
#41250=ORIENTED_EDGE('',*,*,#29506,.T.);
#41251=ORIENTED_EDGE('',*,*,#29507,.T.);
#41252=ORIENTED_EDGE('',*,*,#29508,.T.);
#41253=ORIENTED_EDGE('',*,*,#29509,.T.);
#41254=ORIENTED_EDGE('',*,*,#29510,.T.);
#41255=ORIENTED_EDGE('',*,*,#29511,.T.);
#41256=ORIENTED_EDGE('',*,*,#29512,.T.);
#41257=ORIENTED_EDGE('',*,*,#29513,.T.);
#41258=ORIENTED_EDGE('',*,*,#29514,.T.);
#41259=ORIENTED_EDGE('',*,*,#29515,.T.);
#41260=ORIENTED_EDGE('',*,*,#29516,.T.);
#41261=ORIENTED_EDGE('',*,*,#29517,.T.);
#41262=ORIENTED_EDGE('',*,*,#29518,.T.);
#41263=ORIENTED_EDGE('',*,*,#29519,.T.);
#41264=ORIENTED_EDGE('',*,*,#29520,.T.);
#41265=ORIENTED_EDGE('',*,*,#29521,.T.);
#41266=ORIENTED_EDGE('',*,*,#29522,.T.);
#41267=ORIENTED_EDGE('',*,*,#29523,.T.);
#41268=ORIENTED_EDGE('',*,*,#29524,.T.);
#41269=ORIENTED_EDGE('',*,*,#29525,.T.);
#41270=ORIENTED_EDGE('',*,*,#29526,.T.);
#41271=ORIENTED_EDGE('',*,*,#29466,.T.);
#41272=ORIENTED_EDGE('',*,*,#29475,.T.);
#41273=ORIENTED_EDGE('',*,*,#29472,.T.);
#41274=ORIENTED_EDGE('',*,*,#29527,.F.);
#41275=ORIENTED_EDGE('',*,*,#29528,.T.);
#41276=ORIENTED_EDGE('',*,*,#29529,.T.);
#41277=ORIENTED_EDGE('',*,*,#29530,.T.);
#41278=ORIENTED_EDGE('',*,*,#29531,.F.);
#41279=ORIENTED_EDGE('',*,*,#29532,.T.);
#41280=ORIENTED_EDGE('',*,*,#29533,.T.);
#41281=ORIENTED_EDGE('',*,*,#29534,.T.);
#41282=ORIENTED_EDGE('',*,*,#29535,.F.);
#41283=ORIENTED_EDGE('',*,*,#29536,.T.);
#41284=ORIENTED_EDGE('',*,*,#29471,.T.);
#41285=ORIENTED_EDGE('',*,*,#29537,.F.);
#41286=ORIENTED_EDGE('',*,*,#29538,.T.);
#41287=ORIENTED_EDGE('',*,*,#29539,.T.);
#41288=ORIENTED_EDGE('',*,*,#29540,.T.);
#41289=ORIENTED_EDGE('',*,*,#29541,.F.);
#41290=ORIENTED_EDGE('',*,*,#29542,.T.);
#41291=ORIENTED_EDGE('',*,*,#29543,.T.);
#41292=ORIENTED_EDGE('',*,*,#29544,.T.);
#41293=ORIENTED_EDGE('',*,*,#29545,.F.);
#41294=ORIENTED_EDGE('',*,*,#29546,.T.);
#41295=ORIENTED_EDGE('',*,*,#29547,.T.);
#41296=ORIENTED_EDGE('',*,*,#29548,.T.);
#41297=ORIENTED_EDGE('',*,*,#29549,.F.);
#41298=ORIENTED_EDGE('',*,*,#29550,.T.);
#41299=ORIENTED_EDGE('',*,*,#29551,.T.);
#41300=ORIENTED_EDGE('',*,*,#29552,.T.);
#41301=ORIENTED_EDGE('',*,*,#29553,.F.);
#41302=ORIENTED_EDGE('',*,*,#29554,.T.);
#41303=ORIENTED_EDGE('',*,*,#29555,.T.);
#41304=ORIENTED_EDGE('',*,*,#29556,.T.);
#41305=ORIENTED_EDGE('',*,*,#29557,.F.);
#41306=ORIENTED_EDGE('',*,*,#29558,.T.);
#41307=ORIENTED_EDGE('',*,*,#29559,.T.);
#41308=ORIENTED_EDGE('',*,*,#29560,.T.);
#41309=ORIENTED_EDGE('',*,*,#29561,.F.);
#41310=ORIENTED_EDGE('',*,*,#29562,.T.);
#41311=ORIENTED_EDGE('',*,*,#29563,.T.);
#41312=ORIENTED_EDGE('',*,*,#29564,.T.);
#41313=ORIENTED_EDGE('',*,*,#29565,.F.);
#41314=ORIENTED_EDGE('',*,*,#29566,.T.);
#41315=ORIENTED_EDGE('',*,*,#29567,.T.);
#41316=ORIENTED_EDGE('',*,*,#29568,.T.);
#41317=ORIENTED_EDGE('',*,*,#29569,.F.);
#41318=ORIENTED_EDGE('',*,*,#29570,.T.);
#41319=ORIENTED_EDGE('',*,*,#29571,.T.);
#41320=ORIENTED_EDGE('',*,*,#29572,.T.);
#41321=ORIENTED_EDGE('',*,*,#29573,.F.);
#41322=ORIENTED_EDGE('',*,*,#29574,.T.);
#41323=ORIENTED_EDGE('',*,*,#29575,.T.);
#41324=ORIENTED_EDGE('',*,*,#29576,.T.);
#41325=ORIENTED_EDGE('',*,*,#29577,.F.);
#41326=ORIENTED_EDGE('',*,*,#29578,.T.);
#41327=ORIENTED_EDGE('',*,*,#29579,.T.);
#41328=ORIENTED_EDGE('',*,*,#29580,.T.);
#41329=ORIENTED_EDGE('',*,*,#29581,.F.);
#41330=ORIENTED_EDGE('',*,*,#29582,.T.);
#41331=ORIENTED_EDGE('',*,*,#29527,.T.);
#41332=ORIENTED_EDGE('',*,*,#29467,.T.);
#41333=ORIENTED_EDGE('',*,*,#29535,.T.);
#41334=ORIENTED_EDGE('',*,*,#29583,.T.);
#41335=ORIENTED_EDGE('',*,*,#29584,.F.);
#41336=ORIENTED_EDGE('',*,*,#29585,.T.);
#41337=ORIENTED_EDGE('',*,*,#29586,.T.);
#41338=ORIENTED_EDGE('',*,*,#29587,.T.);
#41339=ORIENTED_EDGE('',*,*,#29588,.F.);
#41340=ORIENTED_EDGE('',*,*,#29589,.T.);
#41341=ORIENTED_EDGE('',*,*,#29590,.T.);
#41342=ORIENTED_EDGE('',*,*,#29591,.T.);
#41343=ORIENTED_EDGE('',*,*,#29592,.F.);
#41344=ORIENTED_EDGE('',*,*,#29593,.T.);
#41345=ORIENTED_EDGE('',*,*,#29594,.T.);
#41346=ORIENTED_EDGE('',*,*,#29595,.T.);
#41347=ORIENTED_EDGE('',*,*,#29596,.F.);
#41348=ORIENTED_EDGE('',*,*,#29597,.T.);
#41349=ORIENTED_EDGE('',*,*,#29598,.T.);
#41350=ORIENTED_EDGE('',*,*,#29599,.T.);
#41351=ORIENTED_EDGE('',*,*,#29600,.F.);
#41352=ORIENTED_EDGE('',*,*,#29601,.T.);
#41353=ORIENTED_EDGE('',*,*,#29602,.T.);
#41354=ORIENTED_EDGE('',*,*,#29603,.T.);
#41355=ORIENTED_EDGE('',*,*,#29604,.F.);
#41356=ORIENTED_EDGE('',*,*,#29605,.T.);
#41357=ORIENTED_EDGE('',*,*,#29606,.T.);
#41358=ORIENTED_EDGE('',*,*,#29607,.T.);
#41359=ORIENTED_EDGE('',*,*,#29608,.F.);
#41360=ORIENTED_EDGE('',*,*,#29609,.T.);
#41361=ORIENTED_EDGE('',*,*,#29610,.T.);
#41362=ORIENTED_EDGE('',*,*,#29611,.T.);
#41363=ORIENTED_EDGE('',*,*,#29612,.F.);
#41364=ORIENTED_EDGE('',*,*,#29613,.T.);
#41365=ORIENTED_EDGE('',*,*,#29614,.T.);
#41366=ORIENTED_EDGE('',*,*,#29615,.T.);
#41367=ORIENTED_EDGE('',*,*,#29616,.F.);
#41368=ORIENTED_EDGE('',*,*,#29617,.T.);
#41369=ORIENTED_EDGE('',*,*,#29618,.T.);
#41370=ORIENTED_EDGE('',*,*,#29619,.T.);
#41371=ORIENTED_EDGE('',*,*,#29620,.F.);
#41372=ORIENTED_EDGE('',*,*,#29621,.T.);
#41373=ORIENTED_EDGE('',*,*,#29622,.T.);
#41374=ORIENTED_EDGE('',*,*,#29623,.T.);
#41375=ORIENTED_EDGE('',*,*,#29624,.F.);
#41376=ORIENTED_EDGE('',*,*,#29625,.T.);
#41377=ORIENTED_EDGE('',*,*,#29626,.T.);
#41378=ORIENTED_EDGE('',*,*,#29627,.T.);
#41379=ORIENTED_EDGE('',*,*,#29477,.F.);
#41380=ORIENTED_EDGE('',*,*,#29481,.F.);
#41381=ORIENTED_EDGE('',*,*,#29628,.F.);
#41382=ORIENTED_EDGE('',*,*,#29629,.F.);
#41383=ORIENTED_EDGE('',*,*,#29528,.F.);
#41384=ORIENTED_EDGE('',*,*,#29582,.F.);
#41385=ORIENTED_EDGE('',*,*,#29630,.F.);
#41386=ORIENTED_EDGE('',*,*,#29631,.F.);
#41387=ORIENTED_EDGE('',*,*,#29632,.F.);
#41388=ORIENTED_EDGE('',*,*,#29633,.F.);
#41389=ORIENTED_EDGE('',*,*,#29530,.F.);
#41390=ORIENTED_EDGE('',*,*,#29634,.T.);
#41391=ORIENTED_EDGE('',*,*,#29635,.F.);
#41392=ORIENTED_EDGE('',*,*,#29529,.F.);
#41393=ORIENTED_EDGE('',*,*,#29629,.T.);
#41394=ORIENTED_EDGE('',*,*,#29636,.F.);
#41395=ORIENTED_EDGE('',*,*,#29634,.F.);
#41396=ORIENTED_EDGE('',*,*,#29631,.T.);
#41397=ORIENTED_EDGE('',*,*,#29637,.F.);
#41398=ORIENTED_EDGE('',*,*,#29638,.T.);
#41399=ORIENTED_EDGE('',*,*,#29639,.T.);
#41400=ORIENTED_EDGE('',*,*,#29640,.T.);
#41401=ORIENTED_EDGE('',*,*,#29641,.T.);
#41402=ORIENTED_EDGE('',*,*,#29642,.T.);
#41403=ORIENTED_EDGE('',*,*,#29643,.T.);
#41404=ORIENTED_EDGE('',*,*,#29644,.T.);
#41405=ORIENTED_EDGE('',*,*,#29645,.T.);
#41406=ORIENTED_EDGE('',*,*,#29646,.T.);
#41407=ORIENTED_EDGE('',*,*,#29647,.T.);
#41408=ORIENTED_EDGE('',*,*,#29648,.T.);
#41409=ORIENTED_EDGE('',*,*,#29649,.T.);
#41410=ORIENTED_EDGE('',*,*,#29650,.T.);
#41411=ORIENTED_EDGE('',*,*,#29651,.T.);
#41412=ORIENTED_EDGE('',*,*,#29652,.T.);
#41413=ORIENTED_EDGE('',*,*,#29653,.T.);
#41414=ORIENTED_EDGE('',*,*,#29654,.T.);
#41415=ORIENTED_EDGE('',*,*,#29655,.T.);
#41416=ORIENTED_EDGE('',*,*,#29656,.T.);
#41417=ORIENTED_EDGE('',*,*,#29657,.T.);
#41418=ORIENTED_EDGE('',*,*,#29658,.T.);
#41419=ORIENTED_EDGE('',*,*,#29659,.T.);
#41420=ORIENTED_EDGE('',*,*,#29660,.T.);
#41421=ORIENTED_EDGE('',*,*,#29661,.T.);
#41422=ORIENTED_EDGE('',*,*,#29662,.T.);
#41423=ORIENTED_EDGE('',*,*,#29663,.T.);
#41424=ORIENTED_EDGE('',*,*,#29664,.T.);
#41425=ORIENTED_EDGE('',*,*,#29665,.T.);
#41426=ORIENTED_EDGE('',*,*,#29666,.T.);
#41427=ORIENTED_EDGE('',*,*,#29667,.T.);
#41428=ORIENTED_EDGE('',*,*,#29668,.T.);
#41429=ORIENTED_EDGE('',*,*,#29669,.T.);
#41430=ORIENTED_EDGE('',*,*,#29670,.T.);
#41431=ORIENTED_EDGE('',*,*,#29671,.T.);
#41432=ORIENTED_EDGE('',*,*,#29672,.T.);
#41433=ORIENTED_EDGE('',*,*,#29673,.T.);
#41434=ORIENTED_EDGE('',*,*,#29674,.T.);
#41435=ORIENTED_EDGE('',*,*,#29675,.T.);
#41436=ORIENTED_EDGE('',*,*,#29676,.T.);
#41437=ORIENTED_EDGE('',*,*,#29677,.T.);
#41438=ORIENTED_EDGE('',*,*,#29678,.T.);
#41439=ORIENTED_EDGE('',*,*,#29679,.T.);
#41440=ORIENTED_EDGE('',*,*,#29680,.T.);
#41441=ORIENTED_EDGE('',*,*,#29681,.T.);
#41442=ORIENTED_EDGE('',*,*,#29682,.T.);
#41443=ORIENTED_EDGE('',*,*,#29683,.T.);
#41444=ORIENTED_EDGE('',*,*,#29463,.T.);
#41445=ORIENTED_EDGE('',*,*,#29479,.T.);
#41446=ORIENTED_EDGE('',*,*,#29684,.T.);
#41447=ORIENTED_EDGE('',*,*,#29685,.T.);
#41448=ORIENTED_EDGE('',*,*,#29686,.T.);
#41449=ORIENTED_EDGE('',*,*,#29687,.T.);
#41450=ORIENTED_EDGE('',*,*,#29688,.T.);
#41451=ORIENTED_EDGE('',*,*,#29689,.T.);
#41452=ORIENTED_EDGE('',*,*,#29690,.T.);
#41453=ORIENTED_EDGE('',*,*,#29691,.T.);
#41454=ORIENTED_EDGE('',*,*,#29692,.T.);
#41455=ORIENTED_EDGE('',*,*,#29693,.T.);
#41456=ORIENTED_EDGE('',*,*,#29694,.T.);
#41457=ORIENTED_EDGE('',*,*,#29695,.T.);
#41458=ORIENTED_EDGE('',*,*,#29696,.T.);
#41459=ORIENTED_EDGE('',*,*,#29697,.T.);
#41460=ORIENTED_EDGE('',*,*,#29698,.T.);
#41461=ORIENTED_EDGE('',*,*,#29699,.T.);
#41462=ORIENTED_EDGE('',*,*,#29700,.T.);
#41463=ORIENTED_EDGE('',*,*,#29701,.T.);
#41464=ORIENTED_EDGE('',*,*,#29702,.T.);
#41465=ORIENTED_EDGE('',*,*,#29703,.T.);
#41466=ORIENTED_EDGE('',*,*,#29704,.T.);
#41467=ORIENTED_EDGE('',*,*,#29705,.T.);
#41468=ORIENTED_EDGE('',*,*,#29706,.T.);
#41469=ORIENTED_EDGE('',*,*,#29707,.T.);
#41470=ORIENTED_EDGE('',*,*,#29708,.T.);
#41471=ORIENTED_EDGE('',*,*,#29709,.T.);
#41472=ORIENTED_EDGE('',*,*,#29710,.T.);
#41473=ORIENTED_EDGE('',*,*,#29711,.T.);
#41474=ORIENTED_EDGE('',*,*,#29712,.T.);
#41475=ORIENTED_EDGE('',*,*,#29713,.T.);
#41476=ORIENTED_EDGE('',*,*,#29714,.T.);
#41477=ORIENTED_EDGE('',*,*,#29715,.T.);
#41478=ORIENTED_EDGE('',*,*,#29716,.T.);
#41479=ORIENTED_EDGE('',*,*,#29717,.T.);
#41480=ORIENTED_EDGE('',*,*,#29718,.T.);
#41481=ORIENTED_EDGE('',*,*,#29719,.T.);
#41482=ORIENTED_EDGE('',*,*,#29720,.T.);
#41483=ORIENTED_EDGE('',*,*,#29721,.T.);
#41484=ORIENTED_EDGE('',*,*,#29722,.T.);
#41485=ORIENTED_EDGE('',*,*,#29723,.T.);
#41486=ORIENTED_EDGE('',*,*,#29724,.T.);
#41487=ORIENTED_EDGE('',*,*,#29725,.T.);
#41488=ORIENTED_EDGE('',*,*,#29726,.T.);
#41489=ORIENTED_EDGE('',*,*,#29727,.T.);
#41490=ORIENTED_EDGE('',*,*,#29728,.T.);
#41491=ORIENTED_EDGE('',*,*,#29729,.F.);
#41492=ORIENTED_EDGE('',*,*,#29630,.T.);
#41493=ORIENTED_EDGE('',*,*,#29581,.T.);
#41494=ORIENTED_EDGE('',*,*,#29730,.T.);
#41495=ORIENTED_EDGE('',*,*,#29482,.F.);
#41496=ORIENTED_EDGE('',*,*,#29633,.T.);
#41497=ORIENTED_EDGE('',*,*,#29731,.F.);
#41498=ORIENTED_EDGE('',*,*,#29732,.T.);
#41499=ORIENTED_EDGE('',*,*,#29733,.T.);
#41500=ORIENTED_EDGE('',*,*,#29734,.T.);
#41501=ORIENTED_EDGE('',*,*,#29735,.F.);
#41502=ORIENTED_EDGE('',*,*,#29736,.T.);
#41503=ORIENTED_EDGE('',*,*,#29737,.T.);
#41504=ORIENTED_EDGE('',*,*,#29738,.T.);
#41505=ORIENTED_EDGE('',*,*,#29739,.F.);
#41506=ORIENTED_EDGE('',*,*,#29740,.T.);
#41507=ORIENTED_EDGE('',*,*,#29741,.T.);
#41508=ORIENTED_EDGE('',*,*,#29742,.T.);
#41509=ORIENTED_EDGE('',*,*,#29743,.F.);
#41510=ORIENTED_EDGE('',*,*,#29744,.T.);
#41511=ORIENTED_EDGE('',*,*,#29745,.T.);
#41512=ORIENTED_EDGE('',*,*,#29746,.T.);
#41513=ORIENTED_EDGE('',*,*,#29747,.F.);
#41514=ORIENTED_EDGE('',*,*,#29748,.T.);
#41515=ORIENTED_EDGE('',*,*,#29749,.T.);
#41516=ORIENTED_EDGE('',*,*,#29750,.T.);
#41517=ORIENTED_EDGE('',*,*,#29751,.F.);
#41518=ORIENTED_EDGE('',*,*,#29752,.T.);
#41519=ORIENTED_EDGE('',*,*,#29753,.T.);
#41520=ORIENTED_EDGE('',*,*,#29754,.T.);
#41521=ORIENTED_EDGE('',*,*,#29755,.F.);
#41522=ORIENTED_EDGE('',*,*,#29756,.T.);
#41523=ORIENTED_EDGE('',*,*,#29757,.T.);
#41524=ORIENTED_EDGE('',*,*,#29758,.T.);
#41525=ORIENTED_EDGE('',*,*,#29759,.F.);
#41526=ORIENTED_EDGE('',*,*,#29760,.T.);
#41527=ORIENTED_EDGE('',*,*,#29761,.T.);
#41528=ORIENTED_EDGE('',*,*,#29762,.T.);
#41529=ORIENTED_EDGE('',*,*,#29763,.F.);
#41530=ORIENTED_EDGE('',*,*,#29764,.T.);
#41531=ORIENTED_EDGE('',*,*,#29765,.T.);
#41532=ORIENTED_EDGE('',*,*,#29766,.T.);
#41533=ORIENTED_EDGE('',*,*,#29767,.F.);
#41534=ORIENTED_EDGE('',*,*,#29768,.T.);
#41535=ORIENTED_EDGE('',*,*,#29769,.T.);
#41536=ORIENTED_EDGE('',*,*,#29770,.T.);
#41537=ORIENTED_EDGE('',*,*,#29771,.F.);
#41538=ORIENTED_EDGE('',*,*,#29772,.T.);
#41539=ORIENTED_EDGE('',*,*,#29773,.T.);
#41540=ORIENTED_EDGE('',*,*,#29774,.T.);
#41541=ORIENTED_EDGE('',*,*,#29775,.F.);
#41542=ORIENTED_EDGE('',*,*,#29776,.T.);
#41543=ORIENTED_EDGE('',*,*,#29531,.T.);
#41544=ORIENTED_EDGE('',*,*,#29638,.F.);
#41545=ORIENTED_EDGE('',*,*,#29777,.F.);
#41546=ORIENTED_EDGE('',*,*,#29778,.F.);
#41547=ORIENTED_EDGE('',*,*,#29532,.F.);
#41548=ORIENTED_EDGE('',*,*,#29776,.F.);
#41549=ORIENTED_EDGE('',*,*,#29779,.F.);
#41550=ORIENTED_EDGE('',*,*,#29728,.F.);
#41551=ORIENTED_EDGE('',*,*,#29780,.F.);
#41552=ORIENTED_EDGE('',*,*,#29583,.F.);
#41553=ORIENTED_EDGE('',*,*,#29534,.F.);
#41554=ORIENTED_EDGE('',*,*,#29781,.T.);
#41555=ORIENTED_EDGE('',*,*,#29782,.F.);
#41556=ORIENTED_EDGE('',*,*,#29533,.F.);
#41557=ORIENTED_EDGE('',*,*,#29778,.T.);
#41558=ORIENTED_EDGE('',*,*,#29783,.F.);
#41559=ORIENTED_EDGE('',*,*,#29781,.F.);
#41560=ORIENTED_EDGE('',*,*,#29779,.T.);
#41561=ORIENTED_EDGE('',*,*,#29775,.T.);
#41562=ORIENTED_EDGE('',*,*,#29784,.T.);
#41563=ORIENTED_EDGE('',*,*,#29639,.F.);
#41564=ORIENTED_EDGE('',*,*,#29785,.F.);
#41565=ORIENTED_EDGE('',*,*,#29786,.F.);
#41566=ORIENTED_EDGE('',*,*,#29787,.F.);
#41567=ORIENTED_EDGE('',*,*,#29788,.F.);
#41568=ORIENTED_EDGE('',*,*,#29789,.F.);
#41569=ORIENTED_EDGE('',*,*,#29790,.F.);
#41570=ORIENTED_EDGE('',*,*,#29791,.F.);
#41571=ORIENTED_EDGE('',*,*,#29792,.F.);
#41572=ORIENTED_EDGE('',*,*,#29793,.F.);
#41573=ORIENTED_EDGE('',*,*,#29794,.F.);
#41574=ORIENTED_EDGE('',*,*,#29795,.F.);
#41575=ORIENTED_EDGE('',*,*,#29796,.F.);
#41576=ORIENTED_EDGE('',*,*,#29797,.F.);
#41577=ORIENTED_EDGE('',*,*,#29798,.F.);
#41578=ORIENTED_EDGE('',*,*,#29799,.F.);
#41579=ORIENTED_EDGE('',*,*,#29800,.F.);
#41580=ORIENTED_EDGE('',*,*,#29801,.F.);
#41581=ORIENTED_EDGE('',*,*,#29802,.F.);
#41582=ORIENTED_EDGE('',*,*,#29803,.F.);
#41583=ORIENTED_EDGE('',*,*,#29804,.F.);
#41584=ORIENTED_EDGE('',*,*,#29805,.F.);
#41585=ORIENTED_EDGE('',*,*,#29806,.F.);
#41586=ORIENTED_EDGE('',*,*,#29807,.F.);
#41587=ORIENTED_EDGE('',*,*,#29808,.F.);
#41588=ORIENTED_EDGE('',*,*,#29809,.F.);
#41589=ORIENTED_EDGE('',*,*,#29810,.F.);
#41590=ORIENTED_EDGE('',*,*,#29811,.F.);
#41591=ORIENTED_EDGE('',*,*,#29812,.F.);
#41592=ORIENTED_EDGE('',*,*,#29813,.F.);
#41593=ORIENTED_EDGE('',*,*,#29814,.F.);
#41594=ORIENTED_EDGE('',*,*,#29815,.F.);
#41595=ORIENTED_EDGE('',*,*,#29816,.F.);
#41596=ORIENTED_EDGE('',*,*,#29817,.F.);
#41597=ORIENTED_EDGE('',*,*,#29818,.F.);
#41598=ORIENTED_EDGE('',*,*,#29819,.F.);
#41599=ORIENTED_EDGE('',*,*,#29820,.F.);
#41600=ORIENTED_EDGE('',*,*,#29821,.F.);
#41601=ORIENTED_EDGE('',*,*,#29822,.F.);
#41602=ORIENTED_EDGE('',*,*,#29823,.F.);
#41603=ORIENTED_EDGE('',*,*,#29824,.F.);
#41604=ORIENTED_EDGE('',*,*,#29825,.F.);
#41605=ORIENTED_EDGE('',*,*,#29826,.F.);
#41606=ORIENTED_EDGE('',*,*,#29827,.F.);
#41607=ORIENTED_EDGE('',*,*,#29828,.F.);
#41608=ORIENTED_EDGE('',*,*,#29829,.F.);
#41609=ORIENTED_EDGE('',*,*,#29830,.F.);
#41610=ORIENTED_EDGE('',*,*,#29831,.F.);
#41611=ORIENTED_EDGE('',*,*,#29832,.F.);
#41612=ORIENTED_EDGE('',*,*,#29833,.F.);
#41613=ORIENTED_EDGE('',*,*,#29834,.F.);
#41614=ORIENTED_EDGE('',*,*,#29835,.F.);
#41615=ORIENTED_EDGE('',*,*,#29836,.F.);
#41616=ORIENTED_EDGE('',*,*,#29837,.F.);
#41617=ORIENTED_EDGE('',*,*,#29838,.F.);
#41618=ORIENTED_EDGE('',*,*,#29839,.F.);
#41619=ORIENTED_EDGE('',*,*,#29840,.F.);
#41620=ORIENTED_EDGE('',*,*,#29841,.F.);
#41621=ORIENTED_EDGE('',*,*,#29842,.F.);
#41622=ORIENTED_EDGE('',*,*,#29843,.F.);
#41623=ORIENTED_EDGE('',*,*,#29844,.F.);
#41624=ORIENTED_EDGE('',*,*,#29845,.F.);
#41625=ORIENTED_EDGE('',*,*,#29846,.F.);
#41626=ORIENTED_EDGE('',*,*,#29847,.F.);
#41627=ORIENTED_EDGE('',*,*,#29848,.F.);
#41628=ORIENTED_EDGE('',*,*,#29849,.F.);
#41629=ORIENTED_EDGE('',*,*,#29850,.F.);
#41630=ORIENTED_EDGE('',*,*,#29851,.F.);
#41631=ORIENTED_EDGE('',*,*,#29852,.F.);
#41632=ORIENTED_EDGE('',*,*,#29853,.F.);
#41633=ORIENTED_EDGE('',*,*,#29854,.F.);
#41634=ORIENTED_EDGE('',*,*,#29855,.F.);
#41635=ORIENTED_EDGE('',*,*,#29856,.F.);
#41636=ORIENTED_EDGE('',*,*,#29857,.F.);
#41637=ORIENTED_EDGE('',*,*,#29858,.F.);
#41638=ORIENTED_EDGE('',*,*,#29859,.F.);
#41639=ORIENTED_EDGE('',*,*,#29860,.F.);
#41640=ORIENTED_EDGE('',*,*,#29861,.F.);
#41641=ORIENTED_EDGE('',*,*,#29862,.F.);
#41642=ORIENTED_EDGE('',*,*,#29863,.F.);
#41643=ORIENTED_EDGE('',*,*,#29864,.F.);
#41644=ORIENTED_EDGE('',*,*,#29865,.F.);
#41645=ORIENTED_EDGE('',*,*,#29866,.F.);
#41646=ORIENTED_EDGE('',*,*,#29867,.F.);
#41647=ORIENTED_EDGE('',*,*,#29868,.F.);
#41648=ORIENTED_EDGE('',*,*,#29869,.F.);
#41649=ORIENTED_EDGE('',*,*,#29870,.F.);
#41650=ORIENTED_EDGE('',*,*,#29871,.F.);
#41651=ORIENTED_EDGE('',*,*,#29872,.F.);
#41652=ORIENTED_EDGE('',*,*,#29873,.F.);
#41653=ORIENTED_EDGE('',*,*,#29874,.F.);
#41654=ORIENTED_EDGE('',*,*,#29875,.F.);
#41655=ORIENTED_EDGE('',*,*,#29876,.F.);
#41656=ORIENTED_EDGE('',*,*,#29877,.F.);
#41657=ORIENTED_EDGE('',*,*,#29878,.F.);
#41658=ORIENTED_EDGE('',*,*,#29879,.F.);
#41659=ORIENTED_EDGE('',*,*,#29880,.F.);
#41660=ORIENTED_EDGE('',*,*,#29881,.F.);
#41661=ORIENTED_EDGE('',*,*,#29882,.F.);
#41662=ORIENTED_EDGE('',*,*,#29883,.F.);
#41663=ORIENTED_EDGE('',*,*,#29884,.F.);
#41664=ORIENTED_EDGE('',*,*,#29885,.F.);
#41665=ORIENTED_EDGE('',*,*,#29886,.F.);
#41666=ORIENTED_EDGE('',*,*,#29887,.F.);
#41667=ORIENTED_EDGE('',*,*,#29888,.F.);
#41668=ORIENTED_EDGE('',*,*,#29889,.F.);
#41669=ORIENTED_EDGE('',*,*,#29890,.F.);
#41670=ORIENTED_EDGE('',*,*,#29891,.F.);
#41671=ORIENTED_EDGE('',*,*,#29892,.F.);
#41672=ORIENTED_EDGE('',*,*,#29893,.F.);
#41673=ORIENTED_EDGE('',*,*,#29894,.F.);
#41674=ORIENTED_EDGE('',*,*,#29895,.F.);
#41675=ORIENTED_EDGE('',*,*,#29896,.F.);
#41676=ORIENTED_EDGE('',*,*,#29897,.F.);
#41677=ORIENTED_EDGE('',*,*,#29898,.F.);
#41678=ORIENTED_EDGE('',*,*,#29899,.F.);
#41679=ORIENTED_EDGE('',*,*,#29900,.F.);
#41680=ORIENTED_EDGE('',*,*,#29901,.F.);
#41681=ORIENTED_EDGE('',*,*,#29902,.F.);
#41682=ORIENTED_EDGE('',*,*,#29903,.F.);
#41683=ORIENTED_EDGE('',*,*,#29904,.F.);
#41684=ORIENTED_EDGE('',*,*,#29905,.F.);
#41685=ORIENTED_EDGE('',*,*,#29906,.F.);
#41686=ORIENTED_EDGE('',*,*,#29907,.F.);
#41687=ORIENTED_EDGE('',*,*,#29908,.F.);
#41688=ORIENTED_EDGE('',*,*,#29909,.F.);
#41689=ORIENTED_EDGE('',*,*,#29910,.F.);
#41690=ORIENTED_EDGE('',*,*,#29911,.F.);
#41691=ORIENTED_EDGE('',*,*,#29912,.F.);
#41692=ORIENTED_EDGE('',*,*,#29913,.F.);
#41693=ORIENTED_EDGE('',*,*,#29914,.F.);
#41694=ORIENTED_EDGE('',*,*,#29915,.F.);
#41695=ORIENTED_EDGE('',*,*,#29916,.F.);
#41696=ORIENTED_EDGE('',*,*,#29915,.T.);
#41697=ORIENTED_EDGE('',*,*,#29917,.F.);
#41698=ORIENTED_EDGE('',*,*,#29918,.T.);
#41699=ORIENTED_EDGE('',*,*,#29919,.T.);
#41700=ORIENTED_EDGE('',*,*,#29920,.T.);
#41701=ORIENTED_EDGE('',*,*,#29585,.F.);
#41702=ORIENTED_EDGE('',*,*,#29921,.F.);
#41703=ORIENTED_EDGE('',*,*,#29726,.F.);
#41704=ORIENTED_EDGE('',*,*,#29922,.T.);
#41705=ORIENTED_EDGE('',*,*,#29923,.F.);
#41706=ORIENTED_EDGE('',*,*,#29914,.T.);
#41707=ORIENTED_EDGE('',*,*,#29924,.F.);
#41708=ORIENTED_EDGE('',*,*,#29925,.T.);
#41709=ORIENTED_EDGE('',*,*,#29917,.T.);
#41710=ORIENTED_EDGE('',*,*,#29911,.T.);
#41711=ORIENTED_EDGE('',*,*,#29926,.F.);
#41712=ORIENTED_EDGE('',*,*,#29927,.T.);
#41713=ORIENTED_EDGE('',*,*,#29928,.T.);
#41714=ORIENTED_EDGE('',*,*,#29929,.T.);
#41715=ORIENTED_EDGE('',*,*,#29589,.F.);
#41716=ORIENTED_EDGE('',*,*,#29930,.F.);
#41717=ORIENTED_EDGE('',*,*,#29722,.F.);
#41718=ORIENTED_EDGE('',*,*,#29931,.T.);
#41719=ORIENTED_EDGE('',*,*,#29932,.F.);
#41720=ORIENTED_EDGE('',*,*,#29910,.T.);
#41721=ORIENTED_EDGE('',*,*,#29933,.F.);
#41722=ORIENTED_EDGE('',*,*,#29934,.T.);
#41723=ORIENTED_EDGE('',*,*,#29926,.T.);
#41724=ORIENTED_EDGE('',*,*,#29907,.T.);
#41725=ORIENTED_EDGE('',*,*,#29935,.F.);
#41726=ORIENTED_EDGE('',*,*,#29936,.T.);
#41727=ORIENTED_EDGE('',*,*,#29937,.T.);
#41728=ORIENTED_EDGE('',*,*,#29938,.T.);
#41729=ORIENTED_EDGE('',*,*,#29593,.F.);
#41730=ORIENTED_EDGE('',*,*,#29939,.F.);
#41731=ORIENTED_EDGE('',*,*,#29718,.F.);
#41732=ORIENTED_EDGE('',*,*,#29940,.T.);
#41733=ORIENTED_EDGE('',*,*,#29941,.F.);
#41734=ORIENTED_EDGE('',*,*,#29906,.T.);
#41735=ORIENTED_EDGE('',*,*,#29942,.F.);
#41736=ORIENTED_EDGE('',*,*,#29943,.T.);
#41737=ORIENTED_EDGE('',*,*,#29935,.T.);
#41738=ORIENTED_EDGE('',*,*,#29903,.T.);
#41739=ORIENTED_EDGE('',*,*,#29944,.F.);
#41740=ORIENTED_EDGE('',*,*,#29945,.T.);
#41741=ORIENTED_EDGE('',*,*,#29946,.T.);
#41742=ORIENTED_EDGE('',*,*,#29947,.T.);
#41743=ORIENTED_EDGE('',*,*,#29597,.F.);
#41744=ORIENTED_EDGE('',*,*,#29948,.F.);
#41745=ORIENTED_EDGE('',*,*,#29714,.F.);
#41746=ORIENTED_EDGE('',*,*,#29949,.T.);
#41747=ORIENTED_EDGE('',*,*,#29950,.F.);
#41748=ORIENTED_EDGE('',*,*,#29902,.T.);
#41749=ORIENTED_EDGE('',*,*,#29951,.F.);
#41750=ORIENTED_EDGE('',*,*,#29952,.T.);
#41751=ORIENTED_EDGE('',*,*,#29944,.T.);
#41752=ORIENTED_EDGE('',*,*,#29899,.T.);
#41753=ORIENTED_EDGE('',*,*,#29953,.F.);
#41754=ORIENTED_EDGE('',*,*,#29954,.T.);
#41755=ORIENTED_EDGE('',*,*,#29955,.T.);
#41756=ORIENTED_EDGE('',*,*,#29956,.T.);
#41757=ORIENTED_EDGE('',*,*,#29601,.F.);
#41758=ORIENTED_EDGE('',*,*,#29957,.F.);
#41759=ORIENTED_EDGE('',*,*,#29710,.F.);
#41760=ORIENTED_EDGE('',*,*,#29958,.T.);
#41761=ORIENTED_EDGE('',*,*,#29959,.F.);
#41762=ORIENTED_EDGE('',*,*,#29898,.T.);
#41763=ORIENTED_EDGE('',*,*,#29960,.F.);
#41764=ORIENTED_EDGE('',*,*,#29961,.T.);
#41765=ORIENTED_EDGE('',*,*,#29953,.T.);
#41766=ORIENTED_EDGE('',*,*,#29895,.T.);
#41767=ORIENTED_EDGE('',*,*,#29962,.F.);
#41768=ORIENTED_EDGE('',*,*,#29963,.T.);
#41769=ORIENTED_EDGE('',*,*,#29964,.T.);
#41770=ORIENTED_EDGE('',*,*,#29965,.T.);
#41771=ORIENTED_EDGE('',*,*,#29605,.F.);
#41772=ORIENTED_EDGE('',*,*,#29966,.F.);
#41773=ORIENTED_EDGE('',*,*,#29706,.F.);
#41774=ORIENTED_EDGE('',*,*,#29967,.T.);
#41775=ORIENTED_EDGE('',*,*,#29968,.F.);
#41776=ORIENTED_EDGE('',*,*,#29894,.T.);
#41777=ORIENTED_EDGE('',*,*,#29969,.F.);
#41778=ORIENTED_EDGE('',*,*,#29970,.T.);
#41779=ORIENTED_EDGE('',*,*,#29962,.T.);
#41780=ORIENTED_EDGE('',*,*,#29891,.T.);
#41781=ORIENTED_EDGE('',*,*,#29971,.F.);
#41782=ORIENTED_EDGE('',*,*,#29972,.T.);
#41783=ORIENTED_EDGE('',*,*,#29973,.T.);
#41784=ORIENTED_EDGE('',*,*,#29974,.T.);
#41785=ORIENTED_EDGE('',*,*,#29609,.F.);
#41786=ORIENTED_EDGE('',*,*,#29975,.F.);
#41787=ORIENTED_EDGE('',*,*,#29702,.F.);
#41788=ORIENTED_EDGE('',*,*,#29976,.T.);
#41789=ORIENTED_EDGE('',*,*,#29977,.F.);
#41790=ORIENTED_EDGE('',*,*,#29890,.T.);
#41791=ORIENTED_EDGE('',*,*,#29978,.F.);
#41792=ORIENTED_EDGE('',*,*,#29979,.T.);
#41793=ORIENTED_EDGE('',*,*,#29971,.T.);
#41794=ORIENTED_EDGE('',*,*,#29887,.T.);
#41795=ORIENTED_EDGE('',*,*,#29980,.F.);
#41796=ORIENTED_EDGE('',*,*,#29981,.T.);
#41797=ORIENTED_EDGE('',*,*,#29982,.T.);
#41798=ORIENTED_EDGE('',*,*,#29983,.T.);
#41799=ORIENTED_EDGE('',*,*,#29613,.F.);
#41800=ORIENTED_EDGE('',*,*,#29984,.F.);
#41801=ORIENTED_EDGE('',*,*,#29698,.F.);
#41802=ORIENTED_EDGE('',*,*,#29985,.T.);
#41803=ORIENTED_EDGE('',*,*,#29986,.F.);
#41804=ORIENTED_EDGE('',*,*,#29886,.T.);
#41805=ORIENTED_EDGE('',*,*,#29987,.F.);
#41806=ORIENTED_EDGE('',*,*,#29988,.T.);
#41807=ORIENTED_EDGE('',*,*,#29980,.T.);
#41808=ORIENTED_EDGE('',*,*,#29883,.T.);
#41809=ORIENTED_EDGE('',*,*,#29989,.F.);
#41810=ORIENTED_EDGE('',*,*,#29990,.T.);
#41811=ORIENTED_EDGE('',*,*,#29991,.T.);
#41812=ORIENTED_EDGE('',*,*,#29992,.T.);
#41813=ORIENTED_EDGE('',*,*,#29617,.F.);
#41814=ORIENTED_EDGE('',*,*,#29993,.F.);
#41815=ORIENTED_EDGE('',*,*,#29694,.F.);
#41816=ORIENTED_EDGE('',*,*,#29994,.T.);
#41817=ORIENTED_EDGE('',*,*,#29995,.F.);
#41818=ORIENTED_EDGE('',*,*,#29882,.T.);
#41819=ORIENTED_EDGE('',*,*,#29996,.F.);
#41820=ORIENTED_EDGE('',*,*,#29997,.T.);
#41821=ORIENTED_EDGE('',*,*,#29989,.T.);
#41822=ORIENTED_EDGE('',*,*,#29879,.T.);
#41823=ORIENTED_EDGE('',*,*,#29998,.F.);
#41824=ORIENTED_EDGE('',*,*,#29999,.T.);
#41825=ORIENTED_EDGE('',*,*,#30000,.T.);
#41826=ORIENTED_EDGE('',*,*,#30001,.T.);
#41827=ORIENTED_EDGE('',*,*,#29621,.F.);
#41828=ORIENTED_EDGE('',*,*,#30002,.F.);
#41829=ORIENTED_EDGE('',*,*,#29690,.F.);
#41830=ORIENTED_EDGE('',*,*,#30003,.T.);
#41831=ORIENTED_EDGE('',*,*,#30004,.F.);
#41832=ORIENTED_EDGE('',*,*,#29878,.T.);
#41833=ORIENTED_EDGE('',*,*,#30005,.F.);
#41834=ORIENTED_EDGE('',*,*,#30006,.T.);
#41835=ORIENTED_EDGE('',*,*,#29998,.T.);
#41836=ORIENTED_EDGE('',*,*,#29875,.T.);
#41837=ORIENTED_EDGE('',*,*,#30007,.F.);
#41838=ORIENTED_EDGE('',*,*,#30008,.T.);
#41839=ORIENTED_EDGE('',*,*,#30009,.T.);
#41840=ORIENTED_EDGE('',*,*,#30010,.T.);
#41841=ORIENTED_EDGE('',*,*,#29625,.F.);
#41842=ORIENTED_EDGE('',*,*,#30011,.F.);
#41843=ORIENTED_EDGE('',*,*,#29686,.F.);
#41844=ORIENTED_EDGE('',*,*,#30012,.T.);
#41845=ORIENTED_EDGE('',*,*,#30013,.F.);
#41846=ORIENTED_EDGE('',*,*,#29874,.T.);
#41847=ORIENTED_EDGE('',*,*,#30014,.F.);
#41848=ORIENTED_EDGE('',*,*,#30015,.T.);
#41849=ORIENTED_EDGE('',*,*,#30007,.T.);
#41850=ORIENTED_EDGE('',*,*,#29871,.T.);
#41851=ORIENTED_EDGE('',*,*,#30016,.F.);
#41852=ORIENTED_EDGE('',*,*,#30017,.T.);
#41853=ORIENTED_EDGE('',*,*,#30018,.T.);
#41854=ORIENTED_EDGE('',*,*,#30019,.T.);
#41855=ORIENTED_EDGE('',*,*,#29538,.F.);
#41856=ORIENTED_EDGE('',*,*,#30020,.F.);
#41857=ORIENTED_EDGE('',*,*,#29525,.F.);
#41858=ORIENTED_EDGE('',*,*,#30021,.T.);
#41859=ORIENTED_EDGE('',*,*,#30022,.F.);
#41860=ORIENTED_EDGE('',*,*,#29870,.T.);
#41861=ORIENTED_EDGE('',*,*,#30023,.F.);
#41862=ORIENTED_EDGE('',*,*,#30024,.T.);
#41863=ORIENTED_EDGE('',*,*,#30016,.T.);
#41864=ORIENTED_EDGE('',*,*,#29867,.T.);
#41865=ORIENTED_EDGE('',*,*,#30025,.F.);
#41866=ORIENTED_EDGE('',*,*,#30026,.T.);
#41867=ORIENTED_EDGE('',*,*,#30027,.T.);
#41868=ORIENTED_EDGE('',*,*,#30028,.T.);
#41869=ORIENTED_EDGE('',*,*,#29542,.F.);
#41870=ORIENTED_EDGE('',*,*,#30029,.F.);
#41871=ORIENTED_EDGE('',*,*,#29521,.F.);
#41872=ORIENTED_EDGE('',*,*,#30030,.T.);
#41873=ORIENTED_EDGE('',*,*,#30031,.F.);
#41874=ORIENTED_EDGE('',*,*,#29866,.T.);
#41875=ORIENTED_EDGE('',*,*,#30032,.F.);
#41876=ORIENTED_EDGE('',*,*,#30033,.T.);
#41877=ORIENTED_EDGE('',*,*,#30025,.T.);
#41878=ORIENTED_EDGE('',*,*,#29863,.T.);
#41879=ORIENTED_EDGE('',*,*,#30034,.F.);
#41880=ORIENTED_EDGE('',*,*,#30035,.T.);
#41881=ORIENTED_EDGE('',*,*,#30036,.T.);
#41882=ORIENTED_EDGE('',*,*,#30037,.T.);
#41883=ORIENTED_EDGE('',*,*,#29546,.F.);
#41884=ORIENTED_EDGE('',*,*,#30038,.F.);
#41885=ORIENTED_EDGE('',*,*,#29517,.F.);
#41886=ORIENTED_EDGE('',*,*,#30039,.T.);
#41887=ORIENTED_EDGE('',*,*,#30040,.F.);
#41888=ORIENTED_EDGE('',*,*,#29862,.T.);
#41889=ORIENTED_EDGE('',*,*,#30041,.F.);
#41890=ORIENTED_EDGE('',*,*,#30042,.T.);
#41891=ORIENTED_EDGE('',*,*,#30034,.T.);
#41892=ORIENTED_EDGE('',*,*,#29859,.T.);
#41893=ORIENTED_EDGE('',*,*,#30043,.F.);
#41894=ORIENTED_EDGE('',*,*,#30044,.T.);
#41895=ORIENTED_EDGE('',*,*,#30045,.T.);
#41896=ORIENTED_EDGE('',*,*,#30046,.T.);
#41897=ORIENTED_EDGE('',*,*,#29550,.F.);
#41898=ORIENTED_EDGE('',*,*,#30047,.F.);
#41899=ORIENTED_EDGE('',*,*,#29513,.F.);
#41900=ORIENTED_EDGE('',*,*,#30048,.T.);
#41901=ORIENTED_EDGE('',*,*,#30049,.F.);
#41902=ORIENTED_EDGE('',*,*,#29858,.T.);
#41903=ORIENTED_EDGE('',*,*,#30050,.F.);
#41904=ORIENTED_EDGE('',*,*,#30051,.T.);
#41905=ORIENTED_EDGE('',*,*,#30043,.T.);
#41906=ORIENTED_EDGE('',*,*,#29855,.T.);
#41907=ORIENTED_EDGE('',*,*,#30052,.F.);
#41908=ORIENTED_EDGE('',*,*,#30053,.T.);
#41909=ORIENTED_EDGE('',*,*,#30054,.T.);
#41910=ORIENTED_EDGE('',*,*,#30055,.T.);
#41911=ORIENTED_EDGE('',*,*,#29554,.F.);
#41912=ORIENTED_EDGE('',*,*,#30056,.F.);
#41913=ORIENTED_EDGE('',*,*,#29509,.F.);
#41914=ORIENTED_EDGE('',*,*,#30057,.T.);
#41915=ORIENTED_EDGE('',*,*,#30058,.F.);
#41916=ORIENTED_EDGE('',*,*,#29854,.T.);
#41917=ORIENTED_EDGE('',*,*,#30059,.F.);
#41918=ORIENTED_EDGE('',*,*,#30060,.T.);
#41919=ORIENTED_EDGE('',*,*,#30052,.T.);
#41920=ORIENTED_EDGE('',*,*,#29851,.T.);
#41921=ORIENTED_EDGE('',*,*,#30061,.F.);
#41922=ORIENTED_EDGE('',*,*,#30062,.T.);
#41923=ORIENTED_EDGE('',*,*,#30063,.T.);
#41924=ORIENTED_EDGE('',*,*,#30064,.T.);
#41925=ORIENTED_EDGE('',*,*,#29558,.F.);
#41926=ORIENTED_EDGE('',*,*,#30065,.F.);
#41927=ORIENTED_EDGE('',*,*,#29505,.F.);
#41928=ORIENTED_EDGE('',*,*,#30066,.T.);
#41929=ORIENTED_EDGE('',*,*,#30067,.F.);
#41930=ORIENTED_EDGE('',*,*,#29850,.T.);
#41931=ORIENTED_EDGE('',*,*,#30068,.F.);
#41932=ORIENTED_EDGE('',*,*,#30069,.T.);
#41933=ORIENTED_EDGE('',*,*,#30061,.T.);
#41934=ORIENTED_EDGE('',*,*,#29847,.T.);
#41935=ORIENTED_EDGE('',*,*,#30070,.F.);
#41936=ORIENTED_EDGE('',*,*,#30071,.T.);
#41937=ORIENTED_EDGE('',*,*,#30072,.T.);
#41938=ORIENTED_EDGE('',*,*,#30073,.T.);
#41939=ORIENTED_EDGE('',*,*,#29562,.F.);
#41940=ORIENTED_EDGE('',*,*,#30074,.F.);
#41941=ORIENTED_EDGE('',*,*,#29501,.F.);
#41942=ORIENTED_EDGE('',*,*,#30075,.T.);
#41943=ORIENTED_EDGE('',*,*,#30076,.F.);
#41944=ORIENTED_EDGE('',*,*,#29846,.T.);
#41945=ORIENTED_EDGE('',*,*,#30077,.F.);
#41946=ORIENTED_EDGE('',*,*,#30078,.T.);
#41947=ORIENTED_EDGE('',*,*,#30070,.T.);
#41948=ORIENTED_EDGE('',*,*,#29843,.T.);
#41949=ORIENTED_EDGE('',*,*,#30079,.F.);
#41950=ORIENTED_EDGE('',*,*,#30080,.T.);
#41951=ORIENTED_EDGE('',*,*,#30081,.T.);
#41952=ORIENTED_EDGE('',*,*,#30082,.T.);
#41953=ORIENTED_EDGE('',*,*,#29566,.F.);
#41954=ORIENTED_EDGE('',*,*,#30083,.F.);
#41955=ORIENTED_EDGE('',*,*,#29497,.F.);
#41956=ORIENTED_EDGE('',*,*,#30084,.T.);
#41957=ORIENTED_EDGE('',*,*,#30085,.F.);
#41958=ORIENTED_EDGE('',*,*,#29842,.T.);
#41959=ORIENTED_EDGE('',*,*,#30086,.F.);
#41960=ORIENTED_EDGE('',*,*,#30087,.T.);
#41961=ORIENTED_EDGE('',*,*,#30079,.T.);
#41962=ORIENTED_EDGE('',*,*,#29839,.T.);
#41963=ORIENTED_EDGE('',*,*,#30088,.F.);
#41964=ORIENTED_EDGE('',*,*,#30089,.T.);
#41965=ORIENTED_EDGE('',*,*,#30090,.T.);
#41966=ORIENTED_EDGE('',*,*,#30091,.T.);
#41967=ORIENTED_EDGE('',*,*,#29570,.F.);
#41968=ORIENTED_EDGE('',*,*,#30092,.F.);
#41969=ORIENTED_EDGE('',*,*,#29493,.F.);
#41970=ORIENTED_EDGE('',*,*,#30093,.T.);
#41971=ORIENTED_EDGE('',*,*,#30094,.F.);
#41972=ORIENTED_EDGE('',*,*,#29838,.T.);
#41973=ORIENTED_EDGE('',*,*,#30095,.F.);
#41974=ORIENTED_EDGE('',*,*,#30096,.T.);
#41975=ORIENTED_EDGE('',*,*,#30088,.T.);
#41976=ORIENTED_EDGE('',*,*,#29835,.T.);
#41977=ORIENTED_EDGE('',*,*,#30097,.F.);
#41978=ORIENTED_EDGE('',*,*,#30098,.T.);
#41979=ORIENTED_EDGE('',*,*,#30099,.T.);
#41980=ORIENTED_EDGE('',*,*,#30100,.T.);
#41981=ORIENTED_EDGE('',*,*,#29574,.F.);
#41982=ORIENTED_EDGE('',*,*,#30101,.F.);
#41983=ORIENTED_EDGE('',*,*,#29489,.F.);
#41984=ORIENTED_EDGE('',*,*,#30102,.T.);
#41985=ORIENTED_EDGE('',*,*,#30103,.F.);
#41986=ORIENTED_EDGE('',*,*,#29834,.T.);
#41987=ORIENTED_EDGE('',*,*,#30104,.F.);
#41988=ORIENTED_EDGE('',*,*,#30105,.T.);
#41989=ORIENTED_EDGE('',*,*,#30097,.T.);
#41990=ORIENTED_EDGE('',*,*,#29831,.T.);
#41991=ORIENTED_EDGE('',*,*,#30106,.F.);
#41992=ORIENTED_EDGE('',*,*,#30107,.T.);
#41993=ORIENTED_EDGE('',*,*,#30108,.T.);
#41994=ORIENTED_EDGE('',*,*,#30109,.T.);
#41995=ORIENTED_EDGE('',*,*,#29578,.F.);
#41996=ORIENTED_EDGE('',*,*,#30110,.F.);
#41997=ORIENTED_EDGE('',*,*,#29485,.F.);
#41998=ORIENTED_EDGE('',*,*,#30111,.T.);
#41999=ORIENTED_EDGE('',*,*,#30112,.F.);
#42000=ORIENTED_EDGE('',*,*,#29830,.T.);
#42001=ORIENTED_EDGE('',*,*,#30113,.F.);
#42002=ORIENTED_EDGE('',*,*,#30114,.T.);
#42003=ORIENTED_EDGE('',*,*,#30106,.T.);
#42004=ORIENTED_EDGE('',*,*,#29827,.T.);
#42005=ORIENTED_EDGE('',*,*,#30115,.F.);
#42006=ORIENTED_EDGE('',*,*,#30116,.T.);
#42007=ORIENTED_EDGE('',*,*,#30117,.T.);
#42008=ORIENTED_EDGE('',*,*,#30118,.T.);
#42009=ORIENTED_EDGE('',*,*,#29732,.F.);
#42010=ORIENTED_EDGE('',*,*,#30119,.F.);
#42011=ORIENTED_EDGE('',*,*,#29682,.F.);
#42012=ORIENTED_EDGE('',*,*,#30120,.T.);
#42013=ORIENTED_EDGE('',*,*,#30121,.F.);
#42014=ORIENTED_EDGE('',*,*,#29826,.T.);
#42015=ORIENTED_EDGE('',*,*,#30122,.F.);
#42016=ORIENTED_EDGE('',*,*,#30123,.T.);
#42017=ORIENTED_EDGE('',*,*,#30115,.T.);
#42018=ORIENTED_EDGE('',*,*,#29823,.T.);
#42019=ORIENTED_EDGE('',*,*,#30124,.F.);
#42020=ORIENTED_EDGE('',*,*,#30125,.T.);
#42021=ORIENTED_EDGE('',*,*,#30126,.T.);
#42022=ORIENTED_EDGE('',*,*,#30127,.T.);
#42023=ORIENTED_EDGE('',*,*,#29736,.F.);
#42024=ORIENTED_EDGE('',*,*,#30128,.F.);
#42025=ORIENTED_EDGE('',*,*,#29678,.F.);
#42026=ORIENTED_EDGE('',*,*,#30129,.T.);
#42027=ORIENTED_EDGE('',*,*,#30130,.F.);
#42028=ORIENTED_EDGE('',*,*,#29822,.T.);
#42029=ORIENTED_EDGE('',*,*,#30131,.F.);
#42030=ORIENTED_EDGE('',*,*,#30132,.T.);
#42031=ORIENTED_EDGE('',*,*,#30124,.T.);
#42032=ORIENTED_EDGE('',*,*,#29819,.T.);
#42033=ORIENTED_EDGE('',*,*,#30133,.F.);
#42034=ORIENTED_EDGE('',*,*,#30134,.T.);
#42035=ORIENTED_EDGE('',*,*,#30135,.T.);
#42036=ORIENTED_EDGE('',*,*,#30136,.T.);
#42037=ORIENTED_EDGE('',*,*,#29740,.F.);
#42038=ORIENTED_EDGE('',*,*,#30137,.F.);
#42039=ORIENTED_EDGE('',*,*,#29674,.F.);
#42040=ORIENTED_EDGE('',*,*,#30138,.T.);
#42041=ORIENTED_EDGE('',*,*,#30139,.F.);
#42042=ORIENTED_EDGE('',*,*,#29818,.T.);
#42043=ORIENTED_EDGE('',*,*,#30140,.F.);
#42044=ORIENTED_EDGE('',*,*,#30141,.T.);
#42045=ORIENTED_EDGE('',*,*,#30133,.T.);
#42046=ORIENTED_EDGE('',*,*,#29815,.T.);
#42047=ORIENTED_EDGE('',*,*,#30142,.F.);
#42048=ORIENTED_EDGE('',*,*,#30143,.T.);
#42049=ORIENTED_EDGE('',*,*,#30144,.T.);
#42050=ORIENTED_EDGE('',*,*,#30145,.T.);
#42051=ORIENTED_EDGE('',*,*,#29744,.F.);
#42052=ORIENTED_EDGE('',*,*,#30146,.F.);
#42053=ORIENTED_EDGE('',*,*,#29670,.F.);
#42054=ORIENTED_EDGE('',*,*,#30147,.T.);
#42055=ORIENTED_EDGE('',*,*,#30148,.F.);
#42056=ORIENTED_EDGE('',*,*,#29814,.T.);
#42057=ORIENTED_EDGE('',*,*,#30149,.F.);
#42058=ORIENTED_EDGE('',*,*,#30150,.T.);
#42059=ORIENTED_EDGE('',*,*,#30142,.T.);
#42060=ORIENTED_EDGE('',*,*,#29811,.T.);
#42061=ORIENTED_EDGE('',*,*,#30151,.F.);
#42062=ORIENTED_EDGE('',*,*,#30152,.T.);
#42063=ORIENTED_EDGE('',*,*,#30153,.T.);
#42064=ORIENTED_EDGE('',*,*,#30154,.T.);
#42065=ORIENTED_EDGE('',*,*,#29748,.F.);
#42066=ORIENTED_EDGE('',*,*,#30155,.F.);
#42067=ORIENTED_EDGE('',*,*,#29666,.F.);
#42068=ORIENTED_EDGE('',*,*,#30156,.T.);
#42069=ORIENTED_EDGE('',*,*,#30157,.F.);
#42070=ORIENTED_EDGE('',*,*,#29810,.T.);
#42071=ORIENTED_EDGE('',*,*,#30158,.F.);
#42072=ORIENTED_EDGE('',*,*,#30159,.T.);
#42073=ORIENTED_EDGE('',*,*,#30151,.T.);
#42074=ORIENTED_EDGE('',*,*,#29807,.T.);
#42075=ORIENTED_EDGE('',*,*,#30160,.F.);
#42076=ORIENTED_EDGE('',*,*,#30161,.T.);
#42077=ORIENTED_EDGE('',*,*,#30162,.T.);
#42078=ORIENTED_EDGE('',*,*,#30163,.T.);
#42079=ORIENTED_EDGE('',*,*,#29752,.F.);
#42080=ORIENTED_EDGE('',*,*,#30164,.F.);
#42081=ORIENTED_EDGE('',*,*,#29662,.F.);
#42082=ORIENTED_EDGE('',*,*,#30165,.T.);
#42083=ORIENTED_EDGE('',*,*,#30166,.F.);
#42084=ORIENTED_EDGE('',*,*,#29806,.T.);
#42085=ORIENTED_EDGE('',*,*,#30167,.F.);
#42086=ORIENTED_EDGE('',*,*,#30168,.T.);
#42087=ORIENTED_EDGE('',*,*,#30160,.T.);
#42088=ORIENTED_EDGE('',*,*,#29803,.T.);
#42089=ORIENTED_EDGE('',*,*,#30169,.F.);
#42090=ORIENTED_EDGE('',*,*,#30170,.T.);
#42091=ORIENTED_EDGE('',*,*,#30171,.T.);
#42092=ORIENTED_EDGE('',*,*,#30172,.T.);
#42093=ORIENTED_EDGE('',*,*,#29756,.F.);
#42094=ORIENTED_EDGE('',*,*,#30173,.F.);
#42095=ORIENTED_EDGE('',*,*,#29658,.F.);
#42096=ORIENTED_EDGE('',*,*,#30174,.T.);
#42097=ORIENTED_EDGE('',*,*,#30175,.F.);
#42098=ORIENTED_EDGE('',*,*,#29802,.T.);
#42099=ORIENTED_EDGE('',*,*,#30176,.F.);
#42100=ORIENTED_EDGE('',*,*,#30177,.T.);
#42101=ORIENTED_EDGE('',*,*,#30169,.T.);
#42102=ORIENTED_EDGE('',*,*,#29799,.T.);
#42103=ORIENTED_EDGE('',*,*,#30178,.F.);
#42104=ORIENTED_EDGE('',*,*,#30179,.T.);
#42105=ORIENTED_EDGE('',*,*,#30180,.T.);
#42106=ORIENTED_EDGE('',*,*,#30181,.T.);
#42107=ORIENTED_EDGE('',*,*,#29760,.F.);
#42108=ORIENTED_EDGE('',*,*,#30182,.F.);
#42109=ORIENTED_EDGE('',*,*,#29654,.F.);
#42110=ORIENTED_EDGE('',*,*,#30183,.T.);
#42111=ORIENTED_EDGE('',*,*,#30184,.F.);
#42112=ORIENTED_EDGE('',*,*,#29798,.T.);
#42113=ORIENTED_EDGE('',*,*,#30185,.F.);
#42114=ORIENTED_EDGE('',*,*,#30186,.T.);
#42115=ORIENTED_EDGE('',*,*,#30178,.T.);
#42116=ORIENTED_EDGE('',*,*,#29795,.T.);
#42117=ORIENTED_EDGE('',*,*,#30187,.F.);
#42118=ORIENTED_EDGE('',*,*,#30188,.T.);
#42119=ORIENTED_EDGE('',*,*,#30189,.T.);
#42120=ORIENTED_EDGE('',*,*,#30190,.T.);
#42121=ORIENTED_EDGE('',*,*,#29764,.F.);
#42122=ORIENTED_EDGE('',*,*,#30191,.F.);
#42123=ORIENTED_EDGE('',*,*,#29650,.F.);
#42124=ORIENTED_EDGE('',*,*,#30192,.T.);
#42125=ORIENTED_EDGE('',*,*,#30193,.F.);
#42126=ORIENTED_EDGE('',*,*,#29794,.T.);
#42127=ORIENTED_EDGE('',*,*,#30194,.F.);
#42128=ORIENTED_EDGE('',*,*,#30195,.T.);
#42129=ORIENTED_EDGE('',*,*,#30187,.T.);
#42130=ORIENTED_EDGE('',*,*,#29791,.T.);
#42131=ORIENTED_EDGE('',*,*,#30196,.F.);
#42132=ORIENTED_EDGE('',*,*,#30197,.T.);
#42133=ORIENTED_EDGE('',*,*,#30198,.T.);
#42134=ORIENTED_EDGE('',*,*,#30199,.T.);
#42135=ORIENTED_EDGE('',*,*,#29768,.F.);
#42136=ORIENTED_EDGE('',*,*,#30200,.F.);
#42137=ORIENTED_EDGE('',*,*,#29646,.F.);
#42138=ORIENTED_EDGE('',*,*,#30201,.T.);
#42139=ORIENTED_EDGE('',*,*,#30202,.F.);
#42140=ORIENTED_EDGE('',*,*,#29790,.T.);
#42141=ORIENTED_EDGE('',*,*,#30203,.F.);
#42142=ORIENTED_EDGE('',*,*,#30204,.T.);
#42143=ORIENTED_EDGE('',*,*,#30196,.T.);
#42144=ORIENTED_EDGE('',*,*,#29787,.T.);
#42145=ORIENTED_EDGE('',*,*,#30205,.F.);
#42146=ORIENTED_EDGE('',*,*,#30206,.T.);
#42147=ORIENTED_EDGE('',*,*,#30207,.T.);
#42148=ORIENTED_EDGE('',*,*,#30208,.T.);
#42149=ORIENTED_EDGE('',*,*,#29772,.F.);
#42150=ORIENTED_EDGE('',*,*,#30209,.F.);
#42151=ORIENTED_EDGE('',*,*,#29642,.F.);
#42152=ORIENTED_EDGE('',*,*,#30210,.T.);
#42153=ORIENTED_EDGE('',*,*,#30211,.F.);
#42154=ORIENTED_EDGE('',*,*,#29786,.T.);
#42155=ORIENTED_EDGE('',*,*,#30212,.F.);
#42156=ORIENTED_EDGE('',*,*,#30213,.T.);
#42157=ORIENTED_EDGE('',*,*,#30205,.T.);
#42158=ORIENTED_EDGE('',*,*,#30206,.F.);
#42159=ORIENTED_EDGE('',*,*,#30213,.F.);
#42160=ORIENTED_EDGE('',*,*,#30214,.F.);
#42161=ORIENTED_EDGE('',*,*,#30215,.F.);
#42162=ORIENTED_EDGE('',*,*,#30197,.F.);
#42163=ORIENTED_EDGE('',*,*,#30204,.F.);
#42164=ORIENTED_EDGE('',*,*,#30216,.F.);
#42165=ORIENTED_EDGE('',*,*,#30217,.F.);
#42166=ORIENTED_EDGE('',*,*,#30188,.F.);
#42167=ORIENTED_EDGE('',*,*,#30195,.F.);
#42168=ORIENTED_EDGE('',*,*,#30218,.F.);
#42169=ORIENTED_EDGE('',*,*,#30219,.F.);
#42170=ORIENTED_EDGE('',*,*,#30179,.F.);
#42171=ORIENTED_EDGE('',*,*,#30186,.F.);
#42172=ORIENTED_EDGE('',*,*,#30220,.F.);
#42173=ORIENTED_EDGE('',*,*,#30221,.F.);
#42174=ORIENTED_EDGE('',*,*,#30170,.F.);
#42175=ORIENTED_EDGE('',*,*,#30177,.F.);
#42176=ORIENTED_EDGE('',*,*,#30222,.F.);
#42177=ORIENTED_EDGE('',*,*,#30223,.F.);
#42178=ORIENTED_EDGE('',*,*,#30161,.F.);
#42179=ORIENTED_EDGE('',*,*,#30168,.F.);
#42180=ORIENTED_EDGE('',*,*,#30224,.F.);
#42181=ORIENTED_EDGE('',*,*,#30225,.F.);
#42182=ORIENTED_EDGE('',*,*,#30152,.F.);
#42183=ORIENTED_EDGE('',*,*,#30159,.F.);
#42184=ORIENTED_EDGE('',*,*,#30226,.F.);
#42185=ORIENTED_EDGE('',*,*,#30227,.F.);
#42186=ORIENTED_EDGE('',*,*,#30143,.F.);
#42187=ORIENTED_EDGE('',*,*,#30150,.F.);
#42188=ORIENTED_EDGE('',*,*,#30228,.F.);
#42189=ORIENTED_EDGE('',*,*,#30229,.F.);
#42190=ORIENTED_EDGE('',*,*,#30134,.F.);
#42191=ORIENTED_EDGE('',*,*,#30141,.F.);
#42192=ORIENTED_EDGE('',*,*,#30230,.F.);
#42193=ORIENTED_EDGE('',*,*,#30231,.F.);
#42194=ORIENTED_EDGE('',*,*,#30125,.F.);
#42195=ORIENTED_EDGE('',*,*,#30132,.F.);
#42196=ORIENTED_EDGE('',*,*,#30232,.F.);
#42197=ORIENTED_EDGE('',*,*,#30233,.F.);
#42198=ORIENTED_EDGE('',*,*,#30116,.F.);
#42199=ORIENTED_EDGE('',*,*,#30123,.F.);
#42200=ORIENTED_EDGE('',*,*,#30234,.F.);
#42201=ORIENTED_EDGE('',*,*,#30235,.F.);
#42202=ORIENTED_EDGE('',*,*,#30107,.F.);
#42203=ORIENTED_EDGE('',*,*,#30114,.F.);
#42204=ORIENTED_EDGE('',*,*,#30236,.F.);
#42205=ORIENTED_EDGE('',*,*,#30237,.F.);
#42206=ORIENTED_EDGE('',*,*,#30098,.F.);
#42207=ORIENTED_EDGE('',*,*,#30105,.F.);
#42208=ORIENTED_EDGE('',*,*,#30238,.F.);
#42209=ORIENTED_EDGE('',*,*,#30239,.F.);
#42210=ORIENTED_EDGE('',*,*,#30089,.F.);
#42211=ORIENTED_EDGE('',*,*,#30096,.F.);
#42212=ORIENTED_EDGE('',*,*,#30240,.F.);
#42213=ORIENTED_EDGE('',*,*,#30241,.F.);
#42214=ORIENTED_EDGE('',*,*,#30080,.F.);
#42215=ORIENTED_EDGE('',*,*,#30087,.F.);
#42216=ORIENTED_EDGE('',*,*,#30242,.F.);
#42217=ORIENTED_EDGE('',*,*,#30243,.F.);
#42218=ORIENTED_EDGE('',*,*,#30071,.F.);
#42219=ORIENTED_EDGE('',*,*,#30078,.F.);
#42220=ORIENTED_EDGE('',*,*,#30244,.F.);
#42221=ORIENTED_EDGE('',*,*,#30245,.F.);
#42222=ORIENTED_EDGE('',*,*,#30062,.F.);
#42223=ORIENTED_EDGE('',*,*,#30069,.F.);
#42224=ORIENTED_EDGE('',*,*,#30246,.F.);
#42225=ORIENTED_EDGE('',*,*,#30247,.F.);
#42226=ORIENTED_EDGE('',*,*,#30053,.F.);
#42227=ORIENTED_EDGE('',*,*,#30060,.F.);
#42228=ORIENTED_EDGE('',*,*,#30248,.F.);
#42229=ORIENTED_EDGE('',*,*,#30249,.F.);
#42230=ORIENTED_EDGE('',*,*,#30044,.F.);
#42231=ORIENTED_EDGE('',*,*,#30051,.F.);
#42232=ORIENTED_EDGE('',*,*,#30250,.F.);
#42233=ORIENTED_EDGE('',*,*,#30251,.F.);
#42234=ORIENTED_EDGE('',*,*,#30035,.F.);
#42235=ORIENTED_EDGE('',*,*,#30042,.F.);
#42236=ORIENTED_EDGE('',*,*,#30252,.F.);
#42237=ORIENTED_EDGE('',*,*,#30253,.F.);
#42238=ORIENTED_EDGE('',*,*,#30026,.F.);
#42239=ORIENTED_EDGE('',*,*,#30033,.F.);
#42240=ORIENTED_EDGE('',*,*,#30254,.F.);
#42241=ORIENTED_EDGE('',*,*,#30255,.F.);
#42242=ORIENTED_EDGE('',*,*,#30017,.F.);
#42243=ORIENTED_EDGE('',*,*,#30024,.F.);
#42244=ORIENTED_EDGE('',*,*,#30256,.F.);
#42245=ORIENTED_EDGE('',*,*,#30257,.F.);
#42246=ORIENTED_EDGE('',*,*,#30008,.F.);
#42247=ORIENTED_EDGE('',*,*,#30015,.F.);
#42248=ORIENTED_EDGE('',*,*,#30258,.F.);
#42249=ORIENTED_EDGE('',*,*,#30259,.F.);
#42250=ORIENTED_EDGE('',*,*,#29999,.F.);
#42251=ORIENTED_EDGE('',*,*,#30006,.F.);
#42252=ORIENTED_EDGE('',*,*,#30260,.F.);
#42253=ORIENTED_EDGE('',*,*,#30261,.F.);
#42254=ORIENTED_EDGE('',*,*,#29990,.F.);
#42255=ORIENTED_EDGE('',*,*,#29997,.F.);
#42256=ORIENTED_EDGE('',*,*,#30262,.F.);
#42257=ORIENTED_EDGE('',*,*,#30263,.F.);
#42258=ORIENTED_EDGE('',*,*,#29981,.F.);
#42259=ORIENTED_EDGE('',*,*,#29988,.F.);
#42260=ORIENTED_EDGE('',*,*,#30264,.F.);
#42261=ORIENTED_EDGE('',*,*,#30265,.F.);
#42262=ORIENTED_EDGE('',*,*,#29972,.F.);
#42263=ORIENTED_EDGE('',*,*,#29979,.F.);
#42264=ORIENTED_EDGE('',*,*,#30266,.F.);
#42265=ORIENTED_EDGE('',*,*,#30267,.F.);
#42266=ORIENTED_EDGE('',*,*,#29963,.F.);
#42267=ORIENTED_EDGE('',*,*,#29970,.F.);
#42268=ORIENTED_EDGE('',*,*,#30268,.F.);
#42269=ORIENTED_EDGE('',*,*,#30269,.F.);
#42270=ORIENTED_EDGE('',*,*,#29954,.F.);
#42271=ORIENTED_EDGE('',*,*,#29961,.F.);
#42272=ORIENTED_EDGE('',*,*,#30270,.F.);
#42273=ORIENTED_EDGE('',*,*,#30271,.F.);
#42274=ORIENTED_EDGE('',*,*,#29945,.F.);
#42275=ORIENTED_EDGE('',*,*,#29952,.F.);
#42276=ORIENTED_EDGE('',*,*,#30272,.F.);
#42277=ORIENTED_EDGE('',*,*,#30273,.F.);
#42278=ORIENTED_EDGE('',*,*,#29936,.F.);
#42279=ORIENTED_EDGE('',*,*,#29943,.F.);
#42280=ORIENTED_EDGE('',*,*,#30274,.F.);
#42281=ORIENTED_EDGE('',*,*,#30275,.F.);
#42282=ORIENTED_EDGE('',*,*,#29927,.F.);
#42283=ORIENTED_EDGE('',*,*,#29934,.F.);
#42284=ORIENTED_EDGE('',*,*,#30276,.F.);
#42285=ORIENTED_EDGE('',*,*,#30277,.F.);
#42286=ORIENTED_EDGE('',*,*,#29918,.F.);
#42287=ORIENTED_EDGE('',*,*,#29925,.F.);
#42288=ORIENTED_EDGE('',*,*,#30278,.F.);
#42289=ORIENTED_EDGE('',*,*,#30279,.F.);
#42290=ORIENTED_EDGE('',*,*,#29913,.T.);
#42291=ORIENTED_EDGE('',*,*,#30280,.F.);
#42292=ORIENTED_EDGE('',*,*,#30281,.F.);
#42293=ORIENTED_EDGE('',*,*,#29724,.F.);
#42294=ORIENTED_EDGE('',*,*,#30282,.F.);
#42295=ORIENTED_EDGE('',*,*,#29587,.F.);
#42296=ORIENTED_EDGE('',*,*,#30283,.F.);
#42297=ORIENTED_EDGE('',*,*,#30284,.T.);
#42298=ORIENTED_EDGE('',*,*,#30278,.T.);
#42299=ORIENTED_EDGE('',*,*,#29924,.T.);
#42300=ORIENTED_EDGE('',*,*,#29909,.T.);
#42301=ORIENTED_EDGE('',*,*,#30285,.F.);
#42302=ORIENTED_EDGE('',*,*,#30286,.F.);
#42303=ORIENTED_EDGE('',*,*,#29720,.F.);
#42304=ORIENTED_EDGE('',*,*,#30287,.F.);
#42305=ORIENTED_EDGE('',*,*,#29591,.F.);
#42306=ORIENTED_EDGE('',*,*,#30288,.F.);
#42307=ORIENTED_EDGE('',*,*,#30289,.T.);
#42308=ORIENTED_EDGE('',*,*,#30276,.T.);
#42309=ORIENTED_EDGE('',*,*,#29933,.T.);
#42310=ORIENTED_EDGE('',*,*,#29905,.T.);
#42311=ORIENTED_EDGE('',*,*,#30290,.F.);
#42312=ORIENTED_EDGE('',*,*,#30291,.F.);
#42313=ORIENTED_EDGE('',*,*,#29716,.F.);
#42314=ORIENTED_EDGE('',*,*,#30292,.F.);
#42315=ORIENTED_EDGE('',*,*,#29595,.F.);
#42316=ORIENTED_EDGE('',*,*,#30293,.F.);
#42317=ORIENTED_EDGE('',*,*,#30294,.T.);
#42318=ORIENTED_EDGE('',*,*,#30274,.T.);
#42319=ORIENTED_EDGE('',*,*,#29942,.T.);
#42320=ORIENTED_EDGE('',*,*,#29901,.T.);
#42321=ORIENTED_EDGE('',*,*,#30295,.F.);
#42322=ORIENTED_EDGE('',*,*,#30296,.F.);
#42323=ORIENTED_EDGE('',*,*,#29712,.F.);
#42324=ORIENTED_EDGE('',*,*,#30297,.F.);
#42325=ORIENTED_EDGE('',*,*,#29599,.F.);
#42326=ORIENTED_EDGE('',*,*,#30298,.F.);
#42327=ORIENTED_EDGE('',*,*,#30299,.T.);
#42328=ORIENTED_EDGE('',*,*,#30272,.T.);
#42329=ORIENTED_EDGE('',*,*,#29951,.T.);
#42330=ORIENTED_EDGE('',*,*,#29897,.T.);
#42331=ORIENTED_EDGE('',*,*,#30300,.F.);
#42332=ORIENTED_EDGE('',*,*,#30301,.F.);
#42333=ORIENTED_EDGE('',*,*,#29708,.F.);
#42334=ORIENTED_EDGE('',*,*,#30302,.F.);
#42335=ORIENTED_EDGE('',*,*,#29603,.F.);
#42336=ORIENTED_EDGE('',*,*,#30303,.F.);
#42337=ORIENTED_EDGE('',*,*,#30304,.T.);
#42338=ORIENTED_EDGE('',*,*,#30270,.T.);
#42339=ORIENTED_EDGE('',*,*,#29960,.T.);
#42340=ORIENTED_EDGE('',*,*,#29893,.T.);
#42341=ORIENTED_EDGE('',*,*,#30305,.F.);
#42342=ORIENTED_EDGE('',*,*,#30306,.F.);
#42343=ORIENTED_EDGE('',*,*,#29704,.F.);
#42344=ORIENTED_EDGE('',*,*,#30307,.F.);
#42345=ORIENTED_EDGE('',*,*,#29607,.F.);
#42346=ORIENTED_EDGE('',*,*,#30308,.F.);
#42347=ORIENTED_EDGE('',*,*,#30309,.T.);
#42348=ORIENTED_EDGE('',*,*,#30268,.T.);
#42349=ORIENTED_EDGE('',*,*,#29969,.T.);
#42350=ORIENTED_EDGE('',*,*,#29889,.T.);
#42351=ORIENTED_EDGE('',*,*,#30310,.F.);
#42352=ORIENTED_EDGE('',*,*,#30311,.F.);
#42353=ORIENTED_EDGE('',*,*,#29700,.F.);
#42354=ORIENTED_EDGE('',*,*,#30312,.F.);
#42355=ORIENTED_EDGE('',*,*,#29611,.F.);
#42356=ORIENTED_EDGE('',*,*,#30313,.F.);
#42357=ORIENTED_EDGE('',*,*,#30314,.T.);
#42358=ORIENTED_EDGE('',*,*,#30266,.T.);
#42359=ORIENTED_EDGE('',*,*,#29978,.T.);
#42360=ORIENTED_EDGE('',*,*,#29885,.T.);
#42361=ORIENTED_EDGE('',*,*,#30315,.F.);
#42362=ORIENTED_EDGE('',*,*,#30316,.F.);
#42363=ORIENTED_EDGE('',*,*,#29696,.F.);
#42364=ORIENTED_EDGE('',*,*,#30317,.F.);
#42365=ORIENTED_EDGE('',*,*,#29615,.F.);
#42366=ORIENTED_EDGE('',*,*,#30318,.F.);
#42367=ORIENTED_EDGE('',*,*,#30319,.T.);
#42368=ORIENTED_EDGE('',*,*,#30264,.T.);
#42369=ORIENTED_EDGE('',*,*,#29987,.T.);
#42370=ORIENTED_EDGE('',*,*,#29881,.T.);
#42371=ORIENTED_EDGE('',*,*,#30320,.F.);
#42372=ORIENTED_EDGE('',*,*,#30321,.F.);
#42373=ORIENTED_EDGE('',*,*,#29692,.F.);
#42374=ORIENTED_EDGE('',*,*,#30322,.F.);
#42375=ORIENTED_EDGE('',*,*,#29619,.F.);
#42376=ORIENTED_EDGE('',*,*,#30323,.F.);
#42377=ORIENTED_EDGE('',*,*,#30324,.T.);
#42378=ORIENTED_EDGE('',*,*,#30262,.T.);
#42379=ORIENTED_EDGE('',*,*,#29996,.T.);
#42380=ORIENTED_EDGE('',*,*,#29877,.T.);
#42381=ORIENTED_EDGE('',*,*,#30325,.F.);
#42382=ORIENTED_EDGE('',*,*,#30326,.F.);
#42383=ORIENTED_EDGE('',*,*,#29688,.F.);
#42384=ORIENTED_EDGE('',*,*,#30327,.F.);
#42385=ORIENTED_EDGE('',*,*,#29623,.F.);
#42386=ORIENTED_EDGE('',*,*,#30328,.F.);
#42387=ORIENTED_EDGE('',*,*,#30329,.T.);
#42388=ORIENTED_EDGE('',*,*,#30260,.T.);
#42389=ORIENTED_EDGE('',*,*,#30005,.T.);
#42390=ORIENTED_EDGE('',*,*,#29873,.T.);
#42391=ORIENTED_EDGE('',*,*,#30330,.F.);
#42392=ORIENTED_EDGE('',*,*,#30331,.F.);
#42393=ORIENTED_EDGE('',*,*,#29684,.F.);
#42394=ORIENTED_EDGE('',*,*,#29478,.F.);
#42395=ORIENTED_EDGE('',*,*,#29627,.F.);
#42396=ORIENTED_EDGE('',*,*,#30332,.F.);
#42397=ORIENTED_EDGE('',*,*,#30333,.T.);
#42398=ORIENTED_EDGE('',*,*,#30258,.T.);
#42399=ORIENTED_EDGE('',*,*,#30014,.T.);
#42400=ORIENTED_EDGE('',*,*,#29869,.T.);
#42401=ORIENTED_EDGE('',*,*,#30334,.F.);
#42402=ORIENTED_EDGE('',*,*,#30335,.F.);
#42403=ORIENTED_EDGE('',*,*,#29523,.F.);
#42404=ORIENTED_EDGE('',*,*,#30336,.F.);
#42405=ORIENTED_EDGE('',*,*,#29540,.F.);
#42406=ORIENTED_EDGE('',*,*,#30337,.F.);
#42407=ORIENTED_EDGE('',*,*,#30338,.T.);
#42408=ORIENTED_EDGE('',*,*,#30256,.T.);
#42409=ORIENTED_EDGE('',*,*,#30023,.T.);
#42410=ORIENTED_EDGE('',*,*,#29865,.T.);
#42411=ORIENTED_EDGE('',*,*,#30339,.F.);
#42412=ORIENTED_EDGE('',*,*,#30340,.F.);
#42413=ORIENTED_EDGE('',*,*,#29519,.F.);
#42414=ORIENTED_EDGE('',*,*,#30341,.F.);
#42415=ORIENTED_EDGE('',*,*,#29544,.F.);
#42416=ORIENTED_EDGE('',*,*,#30342,.F.);
#42417=ORIENTED_EDGE('',*,*,#30343,.T.);
#42418=ORIENTED_EDGE('',*,*,#30254,.T.);
#42419=ORIENTED_EDGE('',*,*,#30032,.T.);
#42420=ORIENTED_EDGE('',*,*,#29861,.T.);
#42421=ORIENTED_EDGE('',*,*,#30344,.F.);
#42422=ORIENTED_EDGE('',*,*,#30345,.F.);
#42423=ORIENTED_EDGE('',*,*,#29515,.F.);
#42424=ORIENTED_EDGE('',*,*,#30346,.F.);
#42425=ORIENTED_EDGE('',*,*,#29548,.F.);
#42426=ORIENTED_EDGE('',*,*,#30347,.F.);
#42427=ORIENTED_EDGE('',*,*,#30348,.T.);
#42428=ORIENTED_EDGE('',*,*,#30252,.T.);
#42429=ORIENTED_EDGE('',*,*,#30041,.T.);
#42430=ORIENTED_EDGE('',*,*,#29857,.T.);
#42431=ORIENTED_EDGE('',*,*,#30349,.F.);
#42432=ORIENTED_EDGE('',*,*,#30350,.F.);
#42433=ORIENTED_EDGE('',*,*,#29511,.F.);
#42434=ORIENTED_EDGE('',*,*,#30351,.F.);
#42435=ORIENTED_EDGE('',*,*,#29552,.F.);
#42436=ORIENTED_EDGE('',*,*,#30352,.F.);
#42437=ORIENTED_EDGE('',*,*,#30353,.T.);
#42438=ORIENTED_EDGE('',*,*,#30250,.T.);
#42439=ORIENTED_EDGE('',*,*,#30050,.T.);
#42440=ORIENTED_EDGE('',*,*,#29853,.T.);
#42441=ORIENTED_EDGE('',*,*,#30354,.F.);
#42442=ORIENTED_EDGE('',*,*,#30355,.F.);
#42443=ORIENTED_EDGE('',*,*,#29507,.F.);
#42444=ORIENTED_EDGE('',*,*,#30356,.F.);
#42445=ORIENTED_EDGE('',*,*,#29556,.F.);
#42446=ORIENTED_EDGE('',*,*,#30357,.F.);
#42447=ORIENTED_EDGE('',*,*,#30358,.T.);
#42448=ORIENTED_EDGE('',*,*,#30248,.T.);
#42449=ORIENTED_EDGE('',*,*,#30059,.T.);
#42450=ORIENTED_EDGE('',*,*,#29849,.T.);
#42451=ORIENTED_EDGE('',*,*,#30359,.F.);
#42452=ORIENTED_EDGE('',*,*,#30360,.F.);
#42453=ORIENTED_EDGE('',*,*,#29503,.F.);
#42454=ORIENTED_EDGE('',*,*,#30361,.F.);
#42455=ORIENTED_EDGE('',*,*,#29560,.F.);
#42456=ORIENTED_EDGE('',*,*,#30362,.F.);
#42457=ORIENTED_EDGE('',*,*,#30363,.T.);
#42458=ORIENTED_EDGE('',*,*,#30246,.T.);
#42459=ORIENTED_EDGE('',*,*,#30068,.T.);
#42460=ORIENTED_EDGE('',*,*,#29845,.T.);
#42461=ORIENTED_EDGE('',*,*,#30364,.F.);
#42462=ORIENTED_EDGE('',*,*,#30365,.F.);
#42463=ORIENTED_EDGE('',*,*,#29499,.F.);
#42464=ORIENTED_EDGE('',*,*,#30366,.F.);
#42465=ORIENTED_EDGE('',*,*,#29564,.F.);
#42466=ORIENTED_EDGE('',*,*,#30367,.F.);
#42467=ORIENTED_EDGE('',*,*,#30368,.T.);
#42468=ORIENTED_EDGE('',*,*,#30244,.T.);
#42469=ORIENTED_EDGE('',*,*,#30077,.T.);
#42470=ORIENTED_EDGE('',*,*,#29841,.T.);
#42471=ORIENTED_EDGE('',*,*,#30369,.F.);
#42472=ORIENTED_EDGE('',*,*,#30370,.F.);
#42473=ORIENTED_EDGE('',*,*,#29495,.F.);
#42474=ORIENTED_EDGE('',*,*,#30371,.F.);
#42475=ORIENTED_EDGE('',*,*,#29568,.F.);
#42476=ORIENTED_EDGE('',*,*,#30372,.F.);
#42477=ORIENTED_EDGE('',*,*,#30373,.T.);
#42478=ORIENTED_EDGE('',*,*,#30242,.T.);
#42479=ORIENTED_EDGE('',*,*,#30086,.T.);
#42480=ORIENTED_EDGE('',*,*,#29837,.T.);
#42481=ORIENTED_EDGE('',*,*,#30374,.F.);
#42482=ORIENTED_EDGE('',*,*,#30375,.F.);
#42483=ORIENTED_EDGE('',*,*,#29491,.F.);
#42484=ORIENTED_EDGE('',*,*,#30376,.F.);
#42485=ORIENTED_EDGE('',*,*,#29572,.F.);
#42486=ORIENTED_EDGE('',*,*,#30377,.F.);
#42487=ORIENTED_EDGE('',*,*,#30378,.T.);
#42488=ORIENTED_EDGE('',*,*,#30240,.T.);
#42489=ORIENTED_EDGE('',*,*,#30095,.T.);
#42490=ORIENTED_EDGE('',*,*,#29833,.T.);
#42491=ORIENTED_EDGE('',*,*,#30379,.F.);
#42492=ORIENTED_EDGE('',*,*,#30380,.F.);
#42493=ORIENTED_EDGE('',*,*,#29487,.F.);
#42494=ORIENTED_EDGE('',*,*,#30381,.F.);
#42495=ORIENTED_EDGE('',*,*,#29576,.F.);
#42496=ORIENTED_EDGE('',*,*,#30382,.F.);
#42497=ORIENTED_EDGE('',*,*,#30383,.T.);
#42498=ORIENTED_EDGE('',*,*,#30238,.T.);
#42499=ORIENTED_EDGE('',*,*,#30104,.T.);
#42500=ORIENTED_EDGE('',*,*,#29829,.T.);
#42501=ORIENTED_EDGE('',*,*,#30384,.F.);
#42502=ORIENTED_EDGE('',*,*,#30385,.F.);
#42503=ORIENTED_EDGE('',*,*,#29483,.F.);
#42504=ORIENTED_EDGE('',*,*,#29730,.F.);
#42505=ORIENTED_EDGE('',*,*,#29580,.F.);
#42506=ORIENTED_EDGE('',*,*,#30386,.F.);
#42507=ORIENTED_EDGE('',*,*,#30387,.T.);
#42508=ORIENTED_EDGE('',*,*,#30236,.T.);
#42509=ORIENTED_EDGE('',*,*,#30113,.T.);
#42510=ORIENTED_EDGE('',*,*,#29825,.T.);
#42511=ORIENTED_EDGE('',*,*,#30388,.F.);
#42512=ORIENTED_EDGE('',*,*,#30389,.F.);
#42513=ORIENTED_EDGE('',*,*,#29680,.F.);
#42514=ORIENTED_EDGE('',*,*,#30390,.F.);
#42515=ORIENTED_EDGE('',*,*,#29734,.F.);
#42516=ORIENTED_EDGE('',*,*,#30391,.F.);
#42517=ORIENTED_EDGE('',*,*,#30392,.T.);
#42518=ORIENTED_EDGE('',*,*,#30234,.T.);
#42519=ORIENTED_EDGE('',*,*,#30122,.T.);
#42520=ORIENTED_EDGE('',*,*,#29821,.T.);
#42521=ORIENTED_EDGE('',*,*,#30393,.F.);
#42522=ORIENTED_EDGE('',*,*,#30394,.F.);
#42523=ORIENTED_EDGE('',*,*,#29676,.F.);
#42524=ORIENTED_EDGE('',*,*,#30395,.F.);
#42525=ORIENTED_EDGE('',*,*,#29738,.F.);
#42526=ORIENTED_EDGE('',*,*,#30396,.F.);
#42527=ORIENTED_EDGE('',*,*,#30397,.T.);
#42528=ORIENTED_EDGE('',*,*,#30232,.T.);
#42529=ORIENTED_EDGE('',*,*,#30131,.T.);
#42530=ORIENTED_EDGE('',*,*,#29817,.T.);
#42531=ORIENTED_EDGE('',*,*,#30398,.F.);
#42532=ORIENTED_EDGE('',*,*,#30399,.F.);
#42533=ORIENTED_EDGE('',*,*,#29672,.F.);
#42534=ORIENTED_EDGE('',*,*,#30400,.F.);
#42535=ORIENTED_EDGE('',*,*,#29742,.F.);
#42536=ORIENTED_EDGE('',*,*,#30401,.F.);
#42537=ORIENTED_EDGE('',*,*,#30402,.T.);
#42538=ORIENTED_EDGE('',*,*,#30230,.T.);
#42539=ORIENTED_EDGE('',*,*,#30140,.T.);
#42540=ORIENTED_EDGE('',*,*,#29813,.T.);
#42541=ORIENTED_EDGE('',*,*,#30403,.F.);
#42542=ORIENTED_EDGE('',*,*,#30404,.F.);
#42543=ORIENTED_EDGE('',*,*,#29668,.F.);
#42544=ORIENTED_EDGE('',*,*,#30405,.F.);
#42545=ORIENTED_EDGE('',*,*,#29746,.F.);
#42546=ORIENTED_EDGE('',*,*,#30406,.F.);
#42547=ORIENTED_EDGE('',*,*,#30407,.T.);
#42548=ORIENTED_EDGE('',*,*,#30228,.T.);
#42549=ORIENTED_EDGE('',*,*,#30149,.T.);
#42550=ORIENTED_EDGE('',*,*,#29809,.T.);
#42551=ORIENTED_EDGE('',*,*,#30408,.F.);
#42552=ORIENTED_EDGE('',*,*,#30409,.F.);
#42553=ORIENTED_EDGE('',*,*,#29664,.F.);
#42554=ORIENTED_EDGE('',*,*,#30410,.F.);
#42555=ORIENTED_EDGE('',*,*,#29750,.F.);
#42556=ORIENTED_EDGE('',*,*,#30411,.F.);
#42557=ORIENTED_EDGE('',*,*,#30412,.T.);
#42558=ORIENTED_EDGE('',*,*,#30226,.T.);
#42559=ORIENTED_EDGE('',*,*,#30158,.T.);
#42560=ORIENTED_EDGE('',*,*,#29805,.T.);
#42561=ORIENTED_EDGE('',*,*,#30413,.F.);
#42562=ORIENTED_EDGE('',*,*,#30414,.F.);
#42563=ORIENTED_EDGE('',*,*,#29660,.F.);
#42564=ORIENTED_EDGE('',*,*,#30415,.F.);
#42565=ORIENTED_EDGE('',*,*,#29754,.F.);
#42566=ORIENTED_EDGE('',*,*,#30416,.F.);
#42567=ORIENTED_EDGE('',*,*,#30417,.T.);
#42568=ORIENTED_EDGE('',*,*,#30224,.T.);
#42569=ORIENTED_EDGE('',*,*,#30167,.T.);
#42570=ORIENTED_EDGE('',*,*,#29801,.T.);
#42571=ORIENTED_EDGE('',*,*,#30418,.F.);
#42572=ORIENTED_EDGE('',*,*,#30419,.F.);
#42573=ORIENTED_EDGE('',*,*,#29656,.F.);
#42574=ORIENTED_EDGE('',*,*,#30420,.F.);
#42575=ORIENTED_EDGE('',*,*,#29758,.F.);
#42576=ORIENTED_EDGE('',*,*,#30421,.F.);
#42577=ORIENTED_EDGE('',*,*,#30422,.T.);
#42578=ORIENTED_EDGE('',*,*,#30222,.T.);
#42579=ORIENTED_EDGE('',*,*,#30176,.T.);
#42580=ORIENTED_EDGE('',*,*,#29797,.T.);
#42581=ORIENTED_EDGE('',*,*,#30423,.F.);
#42582=ORIENTED_EDGE('',*,*,#30424,.F.);
#42583=ORIENTED_EDGE('',*,*,#29652,.F.);
#42584=ORIENTED_EDGE('',*,*,#30425,.F.);
#42585=ORIENTED_EDGE('',*,*,#29762,.F.);
#42586=ORIENTED_EDGE('',*,*,#30426,.F.);
#42587=ORIENTED_EDGE('',*,*,#30427,.T.);
#42588=ORIENTED_EDGE('',*,*,#30220,.T.);
#42589=ORIENTED_EDGE('',*,*,#30185,.T.);
#42590=ORIENTED_EDGE('',*,*,#29793,.T.);
#42591=ORIENTED_EDGE('',*,*,#30428,.F.);
#42592=ORIENTED_EDGE('',*,*,#30429,.F.);
#42593=ORIENTED_EDGE('',*,*,#29648,.F.);
#42594=ORIENTED_EDGE('',*,*,#30430,.F.);
#42595=ORIENTED_EDGE('',*,*,#29766,.F.);
#42596=ORIENTED_EDGE('',*,*,#30431,.F.);
#42597=ORIENTED_EDGE('',*,*,#30432,.T.);
#42598=ORIENTED_EDGE('',*,*,#30218,.T.);
#42599=ORIENTED_EDGE('',*,*,#30194,.T.);
#42600=ORIENTED_EDGE('',*,*,#29789,.T.);
#42601=ORIENTED_EDGE('',*,*,#30433,.F.);
#42602=ORIENTED_EDGE('',*,*,#30434,.F.);
#42603=ORIENTED_EDGE('',*,*,#29644,.F.);
#42604=ORIENTED_EDGE('',*,*,#30435,.F.);
#42605=ORIENTED_EDGE('',*,*,#29770,.F.);
#42606=ORIENTED_EDGE('',*,*,#30436,.F.);
#42607=ORIENTED_EDGE('',*,*,#30437,.T.);
#42608=ORIENTED_EDGE('',*,*,#30216,.T.);
#42609=ORIENTED_EDGE('',*,*,#30203,.T.);
#42610=ORIENTED_EDGE('',*,*,#29785,.T.);
#42611=ORIENTED_EDGE('',*,*,#30438,.F.);
#42612=ORIENTED_EDGE('',*,*,#30439,.F.);
#42613=ORIENTED_EDGE('',*,*,#29640,.F.);
#42614=ORIENTED_EDGE('',*,*,#29784,.F.);
#42615=ORIENTED_EDGE('',*,*,#29774,.F.);
#42616=ORIENTED_EDGE('',*,*,#30440,.F.);
#42617=ORIENTED_EDGE('',*,*,#30441,.T.);
#42618=ORIENTED_EDGE('',*,*,#30214,.T.);
#42619=ORIENTED_EDGE('',*,*,#30212,.T.);
#42620=ORIENTED_EDGE('',*,*,#29586,.F.);
#42621=ORIENTED_EDGE('',*,*,#29920,.F.);
#42622=ORIENTED_EDGE('',*,*,#30442,.T.);
#42623=ORIENTED_EDGE('',*,*,#30283,.T.);
#42624=ORIENTED_EDGE('',*,*,#29725,.F.);
#42625=ORIENTED_EDGE('',*,*,#30281,.T.);
#42626=ORIENTED_EDGE('',*,*,#30443,.F.);
#42627=ORIENTED_EDGE('',*,*,#29922,.F.);
#42628=ORIENTED_EDGE('',*,*,#29916,.T.);
#42629=ORIENTED_EDGE('',*,*,#29923,.T.);
#42630=ORIENTED_EDGE('',*,*,#30443,.T.);
#42631=ORIENTED_EDGE('',*,*,#30280,.T.);
#42632=ORIENTED_EDGE('',*,*,#30279,.T.);
#42633=ORIENTED_EDGE('',*,*,#30284,.F.);
#42634=ORIENTED_EDGE('',*,*,#30442,.F.);
#42635=ORIENTED_EDGE('',*,*,#29919,.F.);
#42636=ORIENTED_EDGE('',*,*,#30282,.T.);
#42637=ORIENTED_EDGE('',*,*,#29723,.F.);
#42638=ORIENTED_EDGE('',*,*,#29930,.T.);
#42639=ORIENTED_EDGE('',*,*,#29588,.T.);
#42640=ORIENTED_EDGE('',*,*,#29780,.T.);
#42641=ORIENTED_EDGE('',*,*,#29727,.F.);
#42642=ORIENTED_EDGE('',*,*,#29921,.T.);
#42643=ORIENTED_EDGE('',*,*,#29584,.T.);
#42644=ORIENTED_EDGE('',*,*,#29590,.F.);
#42645=ORIENTED_EDGE('',*,*,#29929,.F.);
#42646=ORIENTED_EDGE('',*,*,#30444,.T.);
#42647=ORIENTED_EDGE('',*,*,#30288,.T.);
#42648=ORIENTED_EDGE('',*,*,#29721,.F.);
#42649=ORIENTED_EDGE('',*,*,#30286,.T.);
#42650=ORIENTED_EDGE('',*,*,#30445,.F.);
#42651=ORIENTED_EDGE('',*,*,#29931,.F.);
#42652=ORIENTED_EDGE('',*,*,#29912,.T.);
#42653=ORIENTED_EDGE('',*,*,#29932,.T.);
#42654=ORIENTED_EDGE('',*,*,#30445,.T.);
#42655=ORIENTED_EDGE('',*,*,#30285,.T.);
#42656=ORIENTED_EDGE('',*,*,#30277,.T.);
#42657=ORIENTED_EDGE('',*,*,#30289,.F.);
#42658=ORIENTED_EDGE('',*,*,#30444,.F.);
#42659=ORIENTED_EDGE('',*,*,#29928,.F.);
#42660=ORIENTED_EDGE('',*,*,#30287,.T.);
#42661=ORIENTED_EDGE('',*,*,#29719,.F.);
#42662=ORIENTED_EDGE('',*,*,#29939,.T.);
#42663=ORIENTED_EDGE('',*,*,#29592,.T.);
#42664=ORIENTED_EDGE('',*,*,#29594,.F.);
#42665=ORIENTED_EDGE('',*,*,#29938,.F.);
#42666=ORIENTED_EDGE('',*,*,#30446,.T.);
#42667=ORIENTED_EDGE('',*,*,#30293,.T.);
#42668=ORIENTED_EDGE('',*,*,#29717,.F.);
#42669=ORIENTED_EDGE('',*,*,#30291,.T.);
#42670=ORIENTED_EDGE('',*,*,#30447,.F.);
#42671=ORIENTED_EDGE('',*,*,#29940,.F.);
#42672=ORIENTED_EDGE('',*,*,#29908,.T.);
#42673=ORIENTED_EDGE('',*,*,#29941,.T.);
#42674=ORIENTED_EDGE('',*,*,#30447,.T.);
#42675=ORIENTED_EDGE('',*,*,#30290,.T.);
#42676=ORIENTED_EDGE('',*,*,#30275,.T.);
#42677=ORIENTED_EDGE('',*,*,#30294,.F.);
#42678=ORIENTED_EDGE('',*,*,#30446,.F.);
#42679=ORIENTED_EDGE('',*,*,#29937,.F.);
#42680=ORIENTED_EDGE('',*,*,#30292,.T.);
#42681=ORIENTED_EDGE('',*,*,#29715,.F.);
#42682=ORIENTED_EDGE('',*,*,#29948,.T.);
#42683=ORIENTED_EDGE('',*,*,#29596,.T.);
#42684=ORIENTED_EDGE('',*,*,#29598,.F.);
#42685=ORIENTED_EDGE('',*,*,#29947,.F.);
#42686=ORIENTED_EDGE('',*,*,#30448,.T.);
#42687=ORIENTED_EDGE('',*,*,#30298,.T.);
#42688=ORIENTED_EDGE('',*,*,#29713,.F.);
#42689=ORIENTED_EDGE('',*,*,#30296,.T.);
#42690=ORIENTED_EDGE('',*,*,#30449,.F.);
#42691=ORIENTED_EDGE('',*,*,#29949,.F.);
#42692=ORIENTED_EDGE('',*,*,#29904,.T.);
#42693=ORIENTED_EDGE('',*,*,#29950,.T.);
#42694=ORIENTED_EDGE('',*,*,#30449,.T.);
#42695=ORIENTED_EDGE('',*,*,#30295,.T.);
#42696=ORIENTED_EDGE('',*,*,#30273,.T.);
#42697=ORIENTED_EDGE('',*,*,#30299,.F.);
#42698=ORIENTED_EDGE('',*,*,#30448,.F.);
#42699=ORIENTED_EDGE('',*,*,#29946,.F.);
#42700=ORIENTED_EDGE('',*,*,#30297,.T.);
#42701=ORIENTED_EDGE('',*,*,#29711,.F.);
#42702=ORIENTED_EDGE('',*,*,#29957,.T.);
#42703=ORIENTED_EDGE('',*,*,#29600,.T.);
#42704=ORIENTED_EDGE('',*,*,#29602,.F.);
#42705=ORIENTED_EDGE('',*,*,#29956,.F.);
#42706=ORIENTED_EDGE('',*,*,#30450,.T.);
#42707=ORIENTED_EDGE('',*,*,#30303,.T.);
#42708=ORIENTED_EDGE('',*,*,#29709,.F.);
#42709=ORIENTED_EDGE('',*,*,#30301,.T.);
#42710=ORIENTED_EDGE('',*,*,#30451,.F.);
#42711=ORIENTED_EDGE('',*,*,#29958,.F.);
#42712=ORIENTED_EDGE('',*,*,#29900,.T.);
#42713=ORIENTED_EDGE('',*,*,#29959,.T.);
#42714=ORIENTED_EDGE('',*,*,#30451,.T.);
#42715=ORIENTED_EDGE('',*,*,#30300,.T.);
#42716=ORIENTED_EDGE('',*,*,#30271,.T.);
#42717=ORIENTED_EDGE('',*,*,#30304,.F.);
#42718=ORIENTED_EDGE('',*,*,#30450,.F.);
#42719=ORIENTED_EDGE('',*,*,#29955,.F.);
#42720=ORIENTED_EDGE('',*,*,#30302,.T.);
#42721=ORIENTED_EDGE('',*,*,#29707,.F.);
#42722=ORIENTED_EDGE('',*,*,#29966,.T.);
#42723=ORIENTED_EDGE('',*,*,#29604,.T.);
#42724=ORIENTED_EDGE('',*,*,#29606,.F.);
#42725=ORIENTED_EDGE('',*,*,#29965,.F.);
#42726=ORIENTED_EDGE('',*,*,#30452,.T.);
#42727=ORIENTED_EDGE('',*,*,#30308,.T.);
#42728=ORIENTED_EDGE('',*,*,#29705,.F.);
#42729=ORIENTED_EDGE('',*,*,#30306,.T.);
#42730=ORIENTED_EDGE('',*,*,#30453,.F.);
#42731=ORIENTED_EDGE('',*,*,#29967,.F.);
#42732=ORIENTED_EDGE('',*,*,#29896,.T.);
#42733=ORIENTED_EDGE('',*,*,#29968,.T.);
#42734=ORIENTED_EDGE('',*,*,#30453,.T.);
#42735=ORIENTED_EDGE('',*,*,#30305,.T.);
#42736=ORIENTED_EDGE('',*,*,#30269,.T.);
#42737=ORIENTED_EDGE('',*,*,#30309,.F.);
#42738=ORIENTED_EDGE('',*,*,#30452,.F.);
#42739=ORIENTED_EDGE('',*,*,#29964,.F.);
#42740=ORIENTED_EDGE('',*,*,#30307,.T.);
#42741=ORIENTED_EDGE('',*,*,#29703,.F.);
#42742=ORIENTED_EDGE('',*,*,#29975,.T.);
#42743=ORIENTED_EDGE('',*,*,#29608,.T.);
#42744=ORIENTED_EDGE('',*,*,#29610,.F.);
#42745=ORIENTED_EDGE('',*,*,#29974,.F.);
#42746=ORIENTED_EDGE('',*,*,#30454,.T.);
#42747=ORIENTED_EDGE('',*,*,#30313,.T.);
#42748=ORIENTED_EDGE('',*,*,#29701,.F.);
#42749=ORIENTED_EDGE('',*,*,#30311,.T.);
#42750=ORIENTED_EDGE('',*,*,#30455,.F.);
#42751=ORIENTED_EDGE('',*,*,#29976,.F.);
#42752=ORIENTED_EDGE('',*,*,#29892,.T.);
#42753=ORIENTED_EDGE('',*,*,#29977,.T.);
#42754=ORIENTED_EDGE('',*,*,#30455,.T.);
#42755=ORIENTED_EDGE('',*,*,#30310,.T.);
#42756=ORIENTED_EDGE('',*,*,#30267,.T.);
#42757=ORIENTED_EDGE('',*,*,#30314,.F.);
#42758=ORIENTED_EDGE('',*,*,#30454,.F.);
#42759=ORIENTED_EDGE('',*,*,#29973,.F.);
#42760=ORIENTED_EDGE('',*,*,#30312,.T.);
#42761=ORIENTED_EDGE('',*,*,#29699,.F.);
#42762=ORIENTED_EDGE('',*,*,#29984,.T.);
#42763=ORIENTED_EDGE('',*,*,#29612,.T.);
#42764=ORIENTED_EDGE('',*,*,#29614,.F.);
#42765=ORIENTED_EDGE('',*,*,#29983,.F.);
#42766=ORIENTED_EDGE('',*,*,#30456,.T.);
#42767=ORIENTED_EDGE('',*,*,#30318,.T.);
#42768=ORIENTED_EDGE('',*,*,#29697,.F.);
#42769=ORIENTED_EDGE('',*,*,#30316,.T.);
#42770=ORIENTED_EDGE('',*,*,#30457,.F.);
#42771=ORIENTED_EDGE('',*,*,#29985,.F.);
#42772=ORIENTED_EDGE('',*,*,#29888,.T.);
#42773=ORIENTED_EDGE('',*,*,#29986,.T.);
#42774=ORIENTED_EDGE('',*,*,#30457,.T.);
#42775=ORIENTED_EDGE('',*,*,#30315,.T.);
#42776=ORIENTED_EDGE('',*,*,#30265,.T.);
#42777=ORIENTED_EDGE('',*,*,#30319,.F.);
#42778=ORIENTED_EDGE('',*,*,#30456,.F.);
#42779=ORIENTED_EDGE('',*,*,#29982,.F.);
#42780=ORIENTED_EDGE('',*,*,#30317,.T.);
#42781=ORIENTED_EDGE('',*,*,#29695,.F.);
#42782=ORIENTED_EDGE('',*,*,#29993,.T.);
#42783=ORIENTED_EDGE('',*,*,#29616,.T.);
#42784=ORIENTED_EDGE('',*,*,#29618,.F.);
#42785=ORIENTED_EDGE('',*,*,#29992,.F.);
#42786=ORIENTED_EDGE('',*,*,#30458,.T.);
#42787=ORIENTED_EDGE('',*,*,#30323,.T.);
#42788=ORIENTED_EDGE('',*,*,#29693,.F.);
#42789=ORIENTED_EDGE('',*,*,#30321,.T.);
#42790=ORIENTED_EDGE('',*,*,#30459,.F.);
#42791=ORIENTED_EDGE('',*,*,#29994,.F.);
#42792=ORIENTED_EDGE('',*,*,#29884,.T.);
#42793=ORIENTED_EDGE('',*,*,#29995,.T.);
#42794=ORIENTED_EDGE('',*,*,#30459,.T.);
#42795=ORIENTED_EDGE('',*,*,#30320,.T.);
#42796=ORIENTED_EDGE('',*,*,#30263,.T.);
#42797=ORIENTED_EDGE('',*,*,#30324,.F.);
#42798=ORIENTED_EDGE('',*,*,#30458,.F.);
#42799=ORIENTED_EDGE('',*,*,#29991,.F.);
#42800=ORIENTED_EDGE('',*,*,#30322,.T.);
#42801=ORIENTED_EDGE('',*,*,#29691,.F.);
#42802=ORIENTED_EDGE('',*,*,#30002,.T.);
#42803=ORIENTED_EDGE('',*,*,#29620,.T.);
#42804=ORIENTED_EDGE('',*,*,#29622,.F.);
#42805=ORIENTED_EDGE('',*,*,#30001,.F.);
#42806=ORIENTED_EDGE('',*,*,#30460,.T.);
#42807=ORIENTED_EDGE('',*,*,#30328,.T.);
#42808=ORIENTED_EDGE('',*,*,#29689,.F.);
#42809=ORIENTED_EDGE('',*,*,#30326,.T.);
#42810=ORIENTED_EDGE('',*,*,#30461,.F.);
#42811=ORIENTED_EDGE('',*,*,#30003,.F.);
#42812=ORIENTED_EDGE('',*,*,#29880,.T.);
#42813=ORIENTED_EDGE('',*,*,#30004,.T.);
#42814=ORIENTED_EDGE('',*,*,#30461,.T.);
#42815=ORIENTED_EDGE('',*,*,#30325,.T.);
#42816=ORIENTED_EDGE('',*,*,#30261,.T.);
#42817=ORIENTED_EDGE('',*,*,#30329,.F.);
#42818=ORIENTED_EDGE('',*,*,#30460,.F.);
#42819=ORIENTED_EDGE('',*,*,#30000,.F.);
#42820=ORIENTED_EDGE('',*,*,#30327,.T.);
#42821=ORIENTED_EDGE('',*,*,#29687,.F.);
#42822=ORIENTED_EDGE('',*,*,#30011,.T.);
#42823=ORIENTED_EDGE('',*,*,#29624,.T.);
#42824=ORIENTED_EDGE('',*,*,#29626,.F.);
#42825=ORIENTED_EDGE('',*,*,#30010,.F.);
#42826=ORIENTED_EDGE('',*,*,#30462,.T.);
#42827=ORIENTED_EDGE('',*,*,#30332,.T.);
#42828=ORIENTED_EDGE('',*,*,#29685,.F.);
#42829=ORIENTED_EDGE('',*,*,#30331,.T.);
#42830=ORIENTED_EDGE('',*,*,#30463,.F.);
#42831=ORIENTED_EDGE('',*,*,#30012,.F.);
#42832=ORIENTED_EDGE('',*,*,#29876,.T.);
#42833=ORIENTED_EDGE('',*,*,#30013,.T.);
#42834=ORIENTED_EDGE('',*,*,#30463,.T.);
#42835=ORIENTED_EDGE('',*,*,#30330,.T.);
#42836=ORIENTED_EDGE('',*,*,#30259,.T.);
#42837=ORIENTED_EDGE('',*,*,#30333,.F.);
#42838=ORIENTED_EDGE('',*,*,#30462,.F.);
#42839=ORIENTED_EDGE('',*,*,#30009,.F.);
#42840=ORIENTED_EDGE('',*,*,#29470,.T.);
#42841=ORIENTED_EDGE('',*,*,#29526,.F.);
#42842=ORIENTED_EDGE('',*,*,#30020,.T.);
#42843=ORIENTED_EDGE('',*,*,#29537,.T.);
#42844=ORIENTED_EDGE('',*,*,#29539,.F.);
#42845=ORIENTED_EDGE('',*,*,#30019,.F.);
#42846=ORIENTED_EDGE('',*,*,#30464,.T.);
#42847=ORIENTED_EDGE('',*,*,#30337,.T.);
#42848=ORIENTED_EDGE('',*,*,#29524,.F.);
#42849=ORIENTED_EDGE('',*,*,#30335,.T.);
#42850=ORIENTED_EDGE('',*,*,#30465,.F.);
#42851=ORIENTED_EDGE('',*,*,#30021,.F.);
#42852=ORIENTED_EDGE('',*,*,#29872,.T.);
#42853=ORIENTED_EDGE('',*,*,#30022,.T.);
#42854=ORIENTED_EDGE('',*,*,#30465,.T.);
#42855=ORIENTED_EDGE('',*,*,#30334,.T.);
#42856=ORIENTED_EDGE('',*,*,#30257,.T.);
#42857=ORIENTED_EDGE('',*,*,#30338,.F.);
#42858=ORIENTED_EDGE('',*,*,#30464,.F.);
#42859=ORIENTED_EDGE('',*,*,#30018,.F.);
#42860=ORIENTED_EDGE('',*,*,#30336,.T.);
#42861=ORIENTED_EDGE('',*,*,#29522,.F.);
#42862=ORIENTED_EDGE('',*,*,#30029,.T.);
#42863=ORIENTED_EDGE('',*,*,#29541,.T.);
#42864=ORIENTED_EDGE('',*,*,#29543,.F.);
#42865=ORIENTED_EDGE('',*,*,#30028,.F.);
#42866=ORIENTED_EDGE('',*,*,#30466,.T.);
#42867=ORIENTED_EDGE('',*,*,#30342,.T.);
#42868=ORIENTED_EDGE('',*,*,#29520,.F.);
#42869=ORIENTED_EDGE('',*,*,#30340,.T.);
#42870=ORIENTED_EDGE('',*,*,#30467,.F.);
#42871=ORIENTED_EDGE('',*,*,#30030,.F.);
#42872=ORIENTED_EDGE('',*,*,#29868,.T.);
#42873=ORIENTED_EDGE('',*,*,#30031,.T.);
#42874=ORIENTED_EDGE('',*,*,#30467,.T.);
#42875=ORIENTED_EDGE('',*,*,#30339,.T.);
#42876=ORIENTED_EDGE('',*,*,#30255,.T.);
#42877=ORIENTED_EDGE('',*,*,#30343,.F.);
#42878=ORIENTED_EDGE('',*,*,#30466,.F.);
#42879=ORIENTED_EDGE('',*,*,#30027,.F.);
#42880=ORIENTED_EDGE('',*,*,#30341,.T.);
#42881=ORIENTED_EDGE('',*,*,#29518,.F.);
#42882=ORIENTED_EDGE('',*,*,#30038,.T.);
#42883=ORIENTED_EDGE('',*,*,#29545,.T.);
#42884=ORIENTED_EDGE('',*,*,#29547,.F.);
#42885=ORIENTED_EDGE('',*,*,#30037,.F.);
#42886=ORIENTED_EDGE('',*,*,#30468,.T.);
#42887=ORIENTED_EDGE('',*,*,#30347,.T.);
#42888=ORIENTED_EDGE('',*,*,#29516,.F.);
#42889=ORIENTED_EDGE('',*,*,#30345,.T.);
#42890=ORIENTED_EDGE('',*,*,#30469,.F.);
#42891=ORIENTED_EDGE('',*,*,#30039,.F.);
#42892=ORIENTED_EDGE('',*,*,#29864,.T.);
#42893=ORIENTED_EDGE('',*,*,#30040,.T.);
#42894=ORIENTED_EDGE('',*,*,#30469,.T.);
#42895=ORIENTED_EDGE('',*,*,#30344,.T.);
#42896=ORIENTED_EDGE('',*,*,#30253,.T.);
#42897=ORIENTED_EDGE('',*,*,#30348,.F.);
#42898=ORIENTED_EDGE('',*,*,#30468,.F.);
#42899=ORIENTED_EDGE('',*,*,#30036,.F.);
#42900=ORIENTED_EDGE('',*,*,#30346,.T.);
#42901=ORIENTED_EDGE('',*,*,#29514,.F.);
#42902=ORIENTED_EDGE('',*,*,#30047,.T.);
#42903=ORIENTED_EDGE('',*,*,#29549,.T.);
#42904=ORIENTED_EDGE('',*,*,#29551,.F.);
#42905=ORIENTED_EDGE('',*,*,#30046,.F.);
#42906=ORIENTED_EDGE('',*,*,#30470,.T.);
#42907=ORIENTED_EDGE('',*,*,#30352,.T.);
#42908=ORIENTED_EDGE('',*,*,#29512,.F.);
#42909=ORIENTED_EDGE('',*,*,#30350,.T.);
#42910=ORIENTED_EDGE('',*,*,#30471,.F.);
#42911=ORIENTED_EDGE('',*,*,#30048,.F.);
#42912=ORIENTED_EDGE('',*,*,#29860,.T.);
#42913=ORIENTED_EDGE('',*,*,#30049,.T.);
#42914=ORIENTED_EDGE('',*,*,#30471,.T.);
#42915=ORIENTED_EDGE('',*,*,#30349,.T.);
#42916=ORIENTED_EDGE('',*,*,#30251,.T.);
#42917=ORIENTED_EDGE('',*,*,#30353,.F.);
#42918=ORIENTED_EDGE('',*,*,#30470,.F.);
#42919=ORIENTED_EDGE('',*,*,#30045,.F.);
#42920=ORIENTED_EDGE('',*,*,#30351,.T.);
#42921=ORIENTED_EDGE('',*,*,#29510,.F.);
#42922=ORIENTED_EDGE('',*,*,#30056,.T.);
#42923=ORIENTED_EDGE('',*,*,#29553,.T.);
#42924=ORIENTED_EDGE('',*,*,#29555,.F.);
#42925=ORIENTED_EDGE('',*,*,#30055,.F.);
#42926=ORIENTED_EDGE('',*,*,#30472,.T.);
#42927=ORIENTED_EDGE('',*,*,#30357,.T.);
#42928=ORIENTED_EDGE('',*,*,#29508,.F.);
#42929=ORIENTED_EDGE('',*,*,#30355,.T.);
#42930=ORIENTED_EDGE('',*,*,#30473,.F.);
#42931=ORIENTED_EDGE('',*,*,#30057,.F.);
#42932=ORIENTED_EDGE('',*,*,#29856,.T.);
#42933=ORIENTED_EDGE('',*,*,#30058,.T.);
#42934=ORIENTED_EDGE('',*,*,#30473,.T.);
#42935=ORIENTED_EDGE('',*,*,#30354,.T.);
#42936=ORIENTED_EDGE('',*,*,#30249,.T.);
#42937=ORIENTED_EDGE('',*,*,#30358,.F.);
#42938=ORIENTED_EDGE('',*,*,#30472,.F.);
#42939=ORIENTED_EDGE('',*,*,#30054,.F.);
#42940=ORIENTED_EDGE('',*,*,#30356,.T.);
#42941=ORIENTED_EDGE('',*,*,#29506,.F.);
#42942=ORIENTED_EDGE('',*,*,#30065,.T.);
#42943=ORIENTED_EDGE('',*,*,#29557,.T.);
#42944=ORIENTED_EDGE('',*,*,#29559,.F.);
#42945=ORIENTED_EDGE('',*,*,#30064,.F.);
#42946=ORIENTED_EDGE('',*,*,#30474,.T.);
#42947=ORIENTED_EDGE('',*,*,#30362,.T.);
#42948=ORIENTED_EDGE('',*,*,#29504,.F.);
#42949=ORIENTED_EDGE('',*,*,#30360,.T.);
#42950=ORIENTED_EDGE('',*,*,#30475,.F.);
#42951=ORIENTED_EDGE('',*,*,#30066,.F.);
#42952=ORIENTED_EDGE('',*,*,#29852,.T.);
#42953=ORIENTED_EDGE('',*,*,#30067,.T.);
#42954=ORIENTED_EDGE('',*,*,#30475,.T.);
#42955=ORIENTED_EDGE('',*,*,#30359,.T.);
#42956=ORIENTED_EDGE('',*,*,#30247,.T.);
#42957=ORIENTED_EDGE('',*,*,#30363,.F.);
#42958=ORIENTED_EDGE('',*,*,#30474,.F.);
#42959=ORIENTED_EDGE('',*,*,#30063,.F.);
#42960=ORIENTED_EDGE('',*,*,#30361,.T.);
#42961=ORIENTED_EDGE('',*,*,#29502,.F.);
#42962=ORIENTED_EDGE('',*,*,#30074,.T.);
#42963=ORIENTED_EDGE('',*,*,#29561,.T.);
#42964=ORIENTED_EDGE('',*,*,#29563,.F.);
#42965=ORIENTED_EDGE('',*,*,#30073,.F.);
#42966=ORIENTED_EDGE('',*,*,#30476,.T.);
#42967=ORIENTED_EDGE('',*,*,#30367,.T.);
#42968=ORIENTED_EDGE('',*,*,#29500,.F.);
#42969=ORIENTED_EDGE('',*,*,#30365,.T.);
#42970=ORIENTED_EDGE('',*,*,#30477,.F.);
#42971=ORIENTED_EDGE('',*,*,#30075,.F.);
#42972=ORIENTED_EDGE('',*,*,#29848,.T.);
#42973=ORIENTED_EDGE('',*,*,#30076,.T.);
#42974=ORIENTED_EDGE('',*,*,#30477,.T.);
#42975=ORIENTED_EDGE('',*,*,#30364,.T.);
#42976=ORIENTED_EDGE('',*,*,#30245,.T.);
#42977=ORIENTED_EDGE('',*,*,#30368,.F.);
#42978=ORIENTED_EDGE('',*,*,#30476,.F.);
#42979=ORIENTED_EDGE('',*,*,#30072,.F.);
#42980=ORIENTED_EDGE('',*,*,#30366,.T.);
#42981=ORIENTED_EDGE('',*,*,#29498,.F.);
#42982=ORIENTED_EDGE('',*,*,#30083,.T.);
#42983=ORIENTED_EDGE('',*,*,#29565,.T.);
#42984=ORIENTED_EDGE('',*,*,#29567,.F.);
#42985=ORIENTED_EDGE('',*,*,#30082,.F.);
#42986=ORIENTED_EDGE('',*,*,#30478,.T.);
#42987=ORIENTED_EDGE('',*,*,#30372,.T.);
#42988=ORIENTED_EDGE('',*,*,#29496,.F.);
#42989=ORIENTED_EDGE('',*,*,#30370,.T.);
#42990=ORIENTED_EDGE('',*,*,#30479,.F.);
#42991=ORIENTED_EDGE('',*,*,#30084,.F.);
#42992=ORIENTED_EDGE('',*,*,#29844,.T.);
#42993=ORIENTED_EDGE('',*,*,#30085,.T.);
#42994=ORIENTED_EDGE('',*,*,#30479,.T.);
#42995=ORIENTED_EDGE('',*,*,#30369,.T.);
#42996=ORIENTED_EDGE('',*,*,#30243,.T.);
#42997=ORIENTED_EDGE('',*,*,#30373,.F.);
#42998=ORIENTED_EDGE('',*,*,#30478,.F.);
#42999=ORIENTED_EDGE('',*,*,#30081,.F.);
#43000=ORIENTED_EDGE('',*,*,#30371,.T.);
#43001=ORIENTED_EDGE('',*,*,#29494,.F.);
#43002=ORIENTED_EDGE('',*,*,#30092,.T.);
#43003=ORIENTED_EDGE('',*,*,#29569,.T.);
#43004=ORIENTED_EDGE('',*,*,#29571,.F.);
#43005=ORIENTED_EDGE('',*,*,#30091,.F.);
#43006=ORIENTED_EDGE('',*,*,#30480,.T.);
#43007=ORIENTED_EDGE('',*,*,#30377,.T.);
#43008=ORIENTED_EDGE('',*,*,#29492,.F.);
#43009=ORIENTED_EDGE('',*,*,#30375,.T.);
#43010=ORIENTED_EDGE('',*,*,#30481,.F.);
#43011=ORIENTED_EDGE('',*,*,#30093,.F.);
#43012=ORIENTED_EDGE('',*,*,#29840,.T.);
#43013=ORIENTED_EDGE('',*,*,#30094,.T.);
#43014=ORIENTED_EDGE('',*,*,#30481,.T.);
#43015=ORIENTED_EDGE('',*,*,#30374,.T.);
#43016=ORIENTED_EDGE('',*,*,#30241,.T.);
#43017=ORIENTED_EDGE('',*,*,#30378,.F.);
#43018=ORIENTED_EDGE('',*,*,#30480,.F.);
#43019=ORIENTED_EDGE('',*,*,#30090,.F.);
#43020=ORIENTED_EDGE('',*,*,#30376,.T.);
#43021=ORIENTED_EDGE('',*,*,#29490,.F.);
#43022=ORIENTED_EDGE('',*,*,#30101,.T.);
#43023=ORIENTED_EDGE('',*,*,#29573,.T.);
#43024=ORIENTED_EDGE('',*,*,#29575,.F.);
#43025=ORIENTED_EDGE('',*,*,#30100,.F.);
#43026=ORIENTED_EDGE('',*,*,#30482,.T.);
#43027=ORIENTED_EDGE('',*,*,#30382,.T.);
#43028=ORIENTED_EDGE('',*,*,#29488,.F.);
#43029=ORIENTED_EDGE('',*,*,#30380,.T.);
#43030=ORIENTED_EDGE('',*,*,#30483,.F.);
#43031=ORIENTED_EDGE('',*,*,#30102,.F.);
#43032=ORIENTED_EDGE('',*,*,#29836,.T.);
#43033=ORIENTED_EDGE('',*,*,#30103,.T.);
#43034=ORIENTED_EDGE('',*,*,#30483,.T.);
#43035=ORIENTED_EDGE('',*,*,#30379,.T.);
#43036=ORIENTED_EDGE('',*,*,#30239,.T.);
#43037=ORIENTED_EDGE('',*,*,#30383,.F.);
#43038=ORIENTED_EDGE('',*,*,#30482,.F.);
#43039=ORIENTED_EDGE('',*,*,#30099,.F.);
#43040=ORIENTED_EDGE('',*,*,#30381,.T.);
#43041=ORIENTED_EDGE('',*,*,#29486,.F.);
#43042=ORIENTED_EDGE('',*,*,#30110,.T.);
#43043=ORIENTED_EDGE('',*,*,#29577,.T.);
#43044=ORIENTED_EDGE('',*,*,#29579,.F.);
#43045=ORIENTED_EDGE('',*,*,#30109,.F.);
#43046=ORIENTED_EDGE('',*,*,#30484,.T.);
#43047=ORIENTED_EDGE('',*,*,#30386,.T.);
#43048=ORIENTED_EDGE('',*,*,#29484,.F.);
#43049=ORIENTED_EDGE('',*,*,#30385,.T.);
#43050=ORIENTED_EDGE('',*,*,#30485,.F.);
#43051=ORIENTED_EDGE('',*,*,#30111,.F.);
#43052=ORIENTED_EDGE('',*,*,#29832,.T.);
#43053=ORIENTED_EDGE('',*,*,#30112,.T.);
#43054=ORIENTED_EDGE('',*,*,#30485,.T.);
#43055=ORIENTED_EDGE('',*,*,#30384,.T.);
#43056=ORIENTED_EDGE('',*,*,#30237,.T.);
#43057=ORIENTED_EDGE('',*,*,#30387,.F.);
#43058=ORIENTED_EDGE('',*,*,#30484,.F.);
#43059=ORIENTED_EDGE('',*,*,#30108,.F.);
#43060=ORIENTED_EDGE('',*,*,#29632,.T.);
#43061=ORIENTED_EDGE('',*,*,#29683,.F.);
#43062=ORIENTED_EDGE('',*,*,#30119,.T.);
#43063=ORIENTED_EDGE('',*,*,#29731,.T.);
#43064=ORIENTED_EDGE('',*,*,#29733,.F.);
#43065=ORIENTED_EDGE('',*,*,#30118,.F.);
#43066=ORIENTED_EDGE('',*,*,#30486,.T.);
#43067=ORIENTED_EDGE('',*,*,#30391,.T.);
#43068=ORIENTED_EDGE('',*,*,#29681,.F.);
#43069=ORIENTED_EDGE('',*,*,#30389,.T.);
#43070=ORIENTED_EDGE('',*,*,#30487,.F.);
#43071=ORIENTED_EDGE('',*,*,#30120,.F.);
#43072=ORIENTED_EDGE('',*,*,#29828,.T.);
#43073=ORIENTED_EDGE('',*,*,#30121,.T.);
#43074=ORIENTED_EDGE('',*,*,#30487,.T.);
#43075=ORIENTED_EDGE('',*,*,#30388,.T.);
#43076=ORIENTED_EDGE('',*,*,#30235,.T.);
#43077=ORIENTED_EDGE('',*,*,#30392,.F.);
#43078=ORIENTED_EDGE('',*,*,#30486,.F.);
#43079=ORIENTED_EDGE('',*,*,#30117,.F.);
#43080=ORIENTED_EDGE('',*,*,#30390,.T.);
#43081=ORIENTED_EDGE('',*,*,#29679,.F.);
#43082=ORIENTED_EDGE('',*,*,#30128,.T.);
#43083=ORIENTED_EDGE('',*,*,#29735,.T.);
#43084=ORIENTED_EDGE('',*,*,#29737,.F.);
#43085=ORIENTED_EDGE('',*,*,#30127,.F.);
#43086=ORIENTED_EDGE('',*,*,#30488,.T.);
#43087=ORIENTED_EDGE('',*,*,#30396,.T.);
#43088=ORIENTED_EDGE('',*,*,#29677,.F.);
#43089=ORIENTED_EDGE('',*,*,#30394,.T.);
#43090=ORIENTED_EDGE('',*,*,#30489,.F.);
#43091=ORIENTED_EDGE('',*,*,#30129,.F.);
#43092=ORIENTED_EDGE('',*,*,#29824,.T.);
#43093=ORIENTED_EDGE('',*,*,#30130,.T.);
#43094=ORIENTED_EDGE('',*,*,#30489,.T.);
#43095=ORIENTED_EDGE('',*,*,#30393,.T.);
#43096=ORIENTED_EDGE('',*,*,#30233,.T.);
#43097=ORIENTED_EDGE('',*,*,#30397,.F.);
#43098=ORIENTED_EDGE('',*,*,#30488,.F.);
#43099=ORIENTED_EDGE('',*,*,#30126,.F.);
#43100=ORIENTED_EDGE('',*,*,#30395,.T.);
#43101=ORIENTED_EDGE('',*,*,#29675,.F.);
#43102=ORIENTED_EDGE('',*,*,#30137,.T.);
#43103=ORIENTED_EDGE('',*,*,#29739,.T.);
#43104=ORIENTED_EDGE('',*,*,#29741,.F.);
#43105=ORIENTED_EDGE('',*,*,#30136,.F.);
#43106=ORIENTED_EDGE('',*,*,#30490,.T.);
#43107=ORIENTED_EDGE('',*,*,#30401,.T.);
#43108=ORIENTED_EDGE('',*,*,#29673,.F.);
#43109=ORIENTED_EDGE('',*,*,#30399,.T.);
#43110=ORIENTED_EDGE('',*,*,#30491,.F.);
#43111=ORIENTED_EDGE('',*,*,#30138,.F.);
#43112=ORIENTED_EDGE('',*,*,#29820,.T.);
#43113=ORIENTED_EDGE('',*,*,#30139,.T.);
#43114=ORIENTED_EDGE('',*,*,#30491,.T.);
#43115=ORIENTED_EDGE('',*,*,#30398,.T.);
#43116=ORIENTED_EDGE('',*,*,#30231,.T.);
#43117=ORIENTED_EDGE('',*,*,#30402,.F.);
#43118=ORIENTED_EDGE('',*,*,#30490,.F.);
#43119=ORIENTED_EDGE('',*,*,#30135,.F.);
#43120=ORIENTED_EDGE('',*,*,#30400,.T.);
#43121=ORIENTED_EDGE('',*,*,#29671,.F.);
#43122=ORIENTED_EDGE('',*,*,#30146,.T.);
#43123=ORIENTED_EDGE('',*,*,#29743,.T.);
#43124=ORIENTED_EDGE('',*,*,#29745,.F.);
#43125=ORIENTED_EDGE('',*,*,#30145,.F.);
#43126=ORIENTED_EDGE('',*,*,#30492,.T.);
#43127=ORIENTED_EDGE('',*,*,#30406,.T.);
#43128=ORIENTED_EDGE('',*,*,#29669,.F.);
#43129=ORIENTED_EDGE('',*,*,#30404,.T.);
#43130=ORIENTED_EDGE('',*,*,#30493,.F.);
#43131=ORIENTED_EDGE('',*,*,#30147,.F.);
#43132=ORIENTED_EDGE('',*,*,#29816,.T.);
#43133=ORIENTED_EDGE('',*,*,#30148,.T.);
#43134=ORIENTED_EDGE('',*,*,#30493,.T.);
#43135=ORIENTED_EDGE('',*,*,#30403,.T.);
#43136=ORIENTED_EDGE('',*,*,#30229,.T.);
#43137=ORIENTED_EDGE('',*,*,#30407,.F.);
#43138=ORIENTED_EDGE('',*,*,#30492,.F.);
#43139=ORIENTED_EDGE('',*,*,#30144,.F.);
#43140=ORIENTED_EDGE('',*,*,#30405,.T.);
#43141=ORIENTED_EDGE('',*,*,#29667,.F.);
#43142=ORIENTED_EDGE('',*,*,#30155,.T.);
#43143=ORIENTED_EDGE('',*,*,#29747,.T.);
#43144=ORIENTED_EDGE('',*,*,#29749,.F.);
#43145=ORIENTED_EDGE('',*,*,#30154,.F.);
#43146=ORIENTED_EDGE('',*,*,#30494,.T.);
#43147=ORIENTED_EDGE('',*,*,#30411,.T.);
#43148=ORIENTED_EDGE('',*,*,#29665,.F.);
#43149=ORIENTED_EDGE('',*,*,#30409,.T.);
#43150=ORIENTED_EDGE('',*,*,#30495,.F.);
#43151=ORIENTED_EDGE('',*,*,#30156,.F.);
#43152=ORIENTED_EDGE('',*,*,#29812,.T.);
#43153=ORIENTED_EDGE('',*,*,#30157,.T.);
#43154=ORIENTED_EDGE('',*,*,#30495,.T.);
#43155=ORIENTED_EDGE('',*,*,#30408,.T.);
#43156=ORIENTED_EDGE('',*,*,#30227,.T.);
#43157=ORIENTED_EDGE('',*,*,#30412,.F.);
#43158=ORIENTED_EDGE('',*,*,#30494,.F.);
#43159=ORIENTED_EDGE('',*,*,#30153,.F.);
#43160=ORIENTED_EDGE('',*,*,#30410,.T.);
#43161=ORIENTED_EDGE('',*,*,#29663,.F.);
#43162=ORIENTED_EDGE('',*,*,#30164,.T.);
#43163=ORIENTED_EDGE('',*,*,#29751,.T.);
#43164=ORIENTED_EDGE('',*,*,#29753,.F.);
#43165=ORIENTED_EDGE('',*,*,#30163,.F.);
#43166=ORIENTED_EDGE('',*,*,#30496,.T.);
#43167=ORIENTED_EDGE('',*,*,#30416,.T.);
#43168=ORIENTED_EDGE('',*,*,#29661,.F.);
#43169=ORIENTED_EDGE('',*,*,#30414,.T.);
#43170=ORIENTED_EDGE('',*,*,#30497,.F.);
#43171=ORIENTED_EDGE('',*,*,#30165,.F.);
#43172=ORIENTED_EDGE('',*,*,#29808,.T.);
#43173=ORIENTED_EDGE('',*,*,#30166,.T.);
#43174=ORIENTED_EDGE('',*,*,#30497,.T.);
#43175=ORIENTED_EDGE('',*,*,#30413,.T.);
#43176=ORIENTED_EDGE('',*,*,#30225,.T.);
#43177=ORIENTED_EDGE('',*,*,#30417,.F.);
#43178=ORIENTED_EDGE('',*,*,#30496,.F.);
#43179=ORIENTED_EDGE('',*,*,#30162,.F.);
#43180=ORIENTED_EDGE('',*,*,#30415,.T.);
#43181=ORIENTED_EDGE('',*,*,#29659,.F.);
#43182=ORIENTED_EDGE('',*,*,#30173,.T.);
#43183=ORIENTED_EDGE('',*,*,#29755,.T.);
#43184=ORIENTED_EDGE('',*,*,#29757,.F.);
#43185=ORIENTED_EDGE('',*,*,#30172,.F.);
#43186=ORIENTED_EDGE('',*,*,#30498,.T.);
#43187=ORIENTED_EDGE('',*,*,#30421,.T.);
#43188=ORIENTED_EDGE('',*,*,#29657,.F.);
#43189=ORIENTED_EDGE('',*,*,#30419,.T.);
#43190=ORIENTED_EDGE('',*,*,#30499,.F.);
#43191=ORIENTED_EDGE('',*,*,#30174,.F.);
#43192=ORIENTED_EDGE('',*,*,#29804,.T.);
#43193=ORIENTED_EDGE('',*,*,#30175,.T.);
#43194=ORIENTED_EDGE('',*,*,#30499,.T.);
#43195=ORIENTED_EDGE('',*,*,#30418,.T.);
#43196=ORIENTED_EDGE('',*,*,#30223,.T.);
#43197=ORIENTED_EDGE('',*,*,#30422,.F.);
#43198=ORIENTED_EDGE('',*,*,#30498,.F.);
#43199=ORIENTED_EDGE('',*,*,#30171,.F.);
#43200=ORIENTED_EDGE('',*,*,#30420,.T.);
#43201=ORIENTED_EDGE('',*,*,#29655,.F.);
#43202=ORIENTED_EDGE('',*,*,#30182,.T.);
#43203=ORIENTED_EDGE('',*,*,#29759,.T.);
#43204=ORIENTED_EDGE('',*,*,#29761,.F.);
#43205=ORIENTED_EDGE('',*,*,#30181,.F.);
#43206=ORIENTED_EDGE('',*,*,#30500,.T.);
#43207=ORIENTED_EDGE('',*,*,#30426,.T.);
#43208=ORIENTED_EDGE('',*,*,#29653,.F.);
#43209=ORIENTED_EDGE('',*,*,#30424,.T.);
#43210=ORIENTED_EDGE('',*,*,#30501,.F.);
#43211=ORIENTED_EDGE('',*,*,#30183,.F.);
#43212=ORIENTED_EDGE('',*,*,#29800,.T.);
#43213=ORIENTED_EDGE('',*,*,#30184,.T.);
#43214=ORIENTED_EDGE('',*,*,#30501,.T.);
#43215=ORIENTED_EDGE('',*,*,#30423,.T.);
#43216=ORIENTED_EDGE('',*,*,#30221,.T.);
#43217=ORIENTED_EDGE('',*,*,#30427,.F.);
#43218=ORIENTED_EDGE('',*,*,#30500,.F.);
#43219=ORIENTED_EDGE('',*,*,#30180,.F.);
#43220=ORIENTED_EDGE('',*,*,#30425,.T.);
#43221=ORIENTED_EDGE('',*,*,#29651,.F.);
#43222=ORIENTED_EDGE('',*,*,#30191,.T.);
#43223=ORIENTED_EDGE('',*,*,#29763,.T.);
#43224=ORIENTED_EDGE('',*,*,#29765,.F.);
#43225=ORIENTED_EDGE('',*,*,#30190,.F.);
#43226=ORIENTED_EDGE('',*,*,#30502,.T.);
#43227=ORIENTED_EDGE('',*,*,#30431,.T.);
#43228=ORIENTED_EDGE('',*,*,#29649,.F.);
#43229=ORIENTED_EDGE('',*,*,#30429,.T.);
#43230=ORIENTED_EDGE('',*,*,#30503,.F.);
#43231=ORIENTED_EDGE('',*,*,#30192,.F.);
#43232=ORIENTED_EDGE('',*,*,#29796,.T.);
#43233=ORIENTED_EDGE('',*,*,#30193,.T.);
#43234=ORIENTED_EDGE('',*,*,#30503,.T.);
#43235=ORIENTED_EDGE('',*,*,#30428,.T.);
#43236=ORIENTED_EDGE('',*,*,#30219,.T.);
#43237=ORIENTED_EDGE('',*,*,#30432,.F.);
#43238=ORIENTED_EDGE('',*,*,#30502,.F.);
#43239=ORIENTED_EDGE('',*,*,#30189,.F.);
#43240=ORIENTED_EDGE('',*,*,#30430,.T.);
#43241=ORIENTED_EDGE('',*,*,#29647,.F.);
#43242=ORIENTED_EDGE('',*,*,#30200,.T.);
#43243=ORIENTED_EDGE('',*,*,#29767,.T.);
#43244=ORIENTED_EDGE('',*,*,#29769,.F.);
#43245=ORIENTED_EDGE('',*,*,#30199,.F.);
#43246=ORIENTED_EDGE('',*,*,#30504,.T.);
#43247=ORIENTED_EDGE('',*,*,#30436,.T.);
#43248=ORIENTED_EDGE('',*,*,#29645,.F.);
#43249=ORIENTED_EDGE('',*,*,#30434,.T.);
#43250=ORIENTED_EDGE('',*,*,#30505,.F.);
#43251=ORIENTED_EDGE('',*,*,#30201,.F.);
#43252=ORIENTED_EDGE('',*,*,#29792,.T.);
#43253=ORIENTED_EDGE('',*,*,#30202,.T.);
#43254=ORIENTED_EDGE('',*,*,#30505,.T.);
#43255=ORIENTED_EDGE('',*,*,#30433,.T.);
#43256=ORIENTED_EDGE('',*,*,#30217,.T.);
#43257=ORIENTED_EDGE('',*,*,#30437,.F.);
#43258=ORIENTED_EDGE('',*,*,#30504,.F.);
#43259=ORIENTED_EDGE('',*,*,#30198,.F.);
#43260=ORIENTED_EDGE('',*,*,#30435,.T.);
#43261=ORIENTED_EDGE('',*,*,#29643,.F.);
#43262=ORIENTED_EDGE('',*,*,#30209,.T.);
#43263=ORIENTED_EDGE('',*,*,#29771,.T.);
#43264=ORIENTED_EDGE('',*,*,#29773,.F.);
#43265=ORIENTED_EDGE('',*,*,#30208,.F.);
#43266=ORIENTED_EDGE('',*,*,#30506,.T.);
#43267=ORIENTED_EDGE('',*,*,#30440,.T.);
#43268=ORIENTED_EDGE('',*,*,#29641,.F.);
#43269=ORIENTED_EDGE('',*,*,#30439,.T.);
#43270=ORIENTED_EDGE('',*,*,#30507,.F.);
#43271=ORIENTED_EDGE('',*,*,#30210,.F.);
#43272=ORIENTED_EDGE('',*,*,#29788,.T.);
#43273=ORIENTED_EDGE('',*,*,#30211,.T.);
#43274=ORIENTED_EDGE('',*,*,#30507,.T.);
#43275=ORIENTED_EDGE('',*,*,#30438,.T.);
#43276=ORIENTED_EDGE('',*,*,#30215,.T.);
#43277=ORIENTED_EDGE('',*,*,#30441,.F.);
#43278=ORIENTED_EDGE('',*,*,#30506,.F.);
#43279=ORIENTED_EDGE('',*,*,#30207,.F.);
#43280=ORIENTED_EDGE('',*,*,#30508,.T.);
#43281=ORIENTED_EDGE('',*,*,#30509,.T.);
#43282=ORIENTED_EDGE('',*,*,#30510,.T.);
#43283=ORIENTED_EDGE('',*,*,#30509,.F.);
#43284=ORIENTED_EDGE('',*,*,#30511,.T.);
#43285=ORIENTED_EDGE('',*,*,#30510,.F.);
#43286=ORIENTED_EDGE('',*,*,#30512,.F.);
#43287=ORIENTED_EDGE('',*,*,#30513,.T.);
#43288=ORIENTED_EDGE('',*,*,#30514,.T.);
#43289=ORIENTED_EDGE('',*,*,#30511,.F.);
#43290=ORIENTED_EDGE('',*,*,#30508,.F.);
#43291=ORIENTED_EDGE('',*,*,#30514,.F.);
#43292=ORIENTED_EDGE('',*,*,#30515,.T.);
#43293=ORIENTED_EDGE('',*,*,#30516,.T.);
#43294=ORIENTED_EDGE('',*,*,#30517,.T.);
#43295=ORIENTED_EDGE('',*,*,#30518,.T.);
#43296=ORIENTED_EDGE('',*,*,#30516,.F.);
#43297=ORIENTED_EDGE('',*,*,#30515,.F.);
#43298=ORIENTED_EDGE('',*,*,#30519,.F.);
#43299=ORIENTED_EDGE('',*,*,#30517,.F.);
#43300=ORIENTED_EDGE('',*,*,#30518,.F.);
#43301=ORIENTED_EDGE('',*,*,#30520,.T.);
#43302=ORIENTED_EDGE('',*,*,#29536,.F.);
#43303=ORIENTED_EDGE('',*,*,#30520,.F.);
#43304=ORIENTED_EDGE('',*,*,#30512,.T.);
#43305=ORIENTED_EDGE('',*,*,#30521,.T.);
#43306=ORIENTED_EDGE('',*,*,#30522,.T.);
#43307=ORIENTED_EDGE('',*,*,#30523,.T.);
#43308=ORIENTED_EDGE('',*,*,#30521,.F.);
#43309=ORIENTED_EDGE('',*,*,#30524,.F.);
#43310=ORIENTED_EDGE('',*,*,#30525,.T.);
#43311=ORIENTED_EDGE('',*,*,#30522,.F.);
#43312=ORIENTED_EDGE('',*,*,#30523,.F.);
#43313=ORIENTED_EDGE('',*,*,#30525,.F.);
#43314=ORIENTED_EDGE('',*,*,#30526,.T.);
#43315=ORIENTED_EDGE('',*,*,#30527,.T.);
#43316=ORIENTED_EDGE('',*,*,#30519,.T.);
#43317=ORIENTED_EDGE('',*,*,#30527,.F.);
#43318=ORIENTED_EDGE('',*,*,#30528,.T.);
#43319=ORIENTED_EDGE('',*,*,#30526,.F.);
#43320=ORIENTED_EDGE('',*,*,#30529,.T.);
#43321=ORIENTED_EDGE('',*,*,#30530,.T.);
#43322=ORIENTED_EDGE('',*,*,#30529,.F.);
#43323=ORIENTED_EDGE('',*,*,#30528,.F.);
#43324=ORIENTED_EDGE('',*,*,#30531,.T.);
#43325=ORIENTED_EDGE('',*,*,#30532,.T.);
#43326=ORIENTED_EDGE('',*,*,#30533,.F.);
#43327=ORIENTED_EDGE('',*,*,#30532,.F.);
#43328=ORIENTED_EDGE('',*,*,#30533,.T.);
#43329=ORIENTED_EDGE('',*,*,#30534,.T.);
#43330=ORIENTED_EDGE('',*,*,#30535,.F.);
#43331=ORIENTED_EDGE('',*,*,#30534,.F.);
#43332=ORIENTED_EDGE('',*,*,#30530,.F.);
#43333=ORIENTED_EDGE('',*,*,#30535,.T.);
#43334=ORIENTED_EDGE('',*,*,#29464,.T.);
#43335=ORIENTED_EDGE('',*,*,#29729,.T.);
#43336=ORIENTED_EDGE('',*,*,#29782,.T.);
#43337=ORIENTED_EDGE('',*,*,#29783,.T.);
#43338=ORIENTED_EDGE('',*,*,#29777,.T.);
#43339=ORIENTED_EDGE('',*,*,#29637,.T.);
#43340=ORIENTED_EDGE('',*,*,#29635,.T.);
#43341=ORIENTED_EDGE('',*,*,#29636,.T.);
#43342=ORIENTED_EDGE('',*,*,#29628,.T.);
#43343=ORIENTED_EDGE('',*,*,#29480,.T.);
#43344=ORIENTED_EDGE('',*,*,#29474,.T.);
#43345=ORIENTED_EDGE('',*,*,#29476,.T.);
#43346=ORIENTED_EDGE('',*,*,#30513,.F.);
#43347=ORIENTED_EDGE('',*,*,#30524,.T.);
#43348=ORIENTED_EDGE('',*,*,#30536,.F.);
#43349=ORIENTED_EDGE('',*,*,#30536,.T.);
#43350=ORIENTED_EDGE('',*,*,#30537,.T.);
#43351=ORIENTED_EDGE('',*,*,#30531,.F.);
#43352=ORIENTED_EDGE('',*,*,#30537,.F.);
#43353=ORIENTED_EDGE('',*,*,#30538,.T.);
#43354=ORIENTED_EDGE('',*,*,#30539,.T.);
#43355=ORIENTED_EDGE('',*,*,#30540,.T.);
#43356=ORIENTED_EDGE('',*,*,#30539,.F.);
#43357=ORIENTED_EDGE('',*,*,#30541,.T.);
#43358=ORIENTED_EDGE('',*,*,#30542,.F.);
#43359=ORIENTED_EDGE('',*,*,#30543,.T.);
#43360=ORIENTED_EDGE('',*,*,#30544,.T.);
#43361=ORIENTED_EDGE('',*,*,#30545,.T.);
#43362=ORIENTED_EDGE('',*,*,#30546,.T.);
#43363=ORIENTED_EDGE('',*,*,#30547,.F.);
#43364=ORIENTED_EDGE('',*,*,#30538,.F.);
#43365=ORIENTED_EDGE('',*,*,#30548,.F.);
#43366=ORIENTED_EDGE('',*,*,#30549,.T.);
#43367=ORIENTED_EDGE('',*,*,#30540,.F.);
#43368=ORIENTED_EDGE('',*,*,#30549,.F.);
#43369=ORIENTED_EDGE('',*,*,#30542,.T.);
#43370=ORIENTED_EDGE('',*,*,#30550,.T.);
#43371=ORIENTED_EDGE('',*,*,#30551,.T.);
#43372=ORIENTED_EDGE('',*,*,#30550,.F.);
#43373=ORIENTED_EDGE('',*,*,#30552,.F.);
#43374=ORIENTED_EDGE('',*,*,#30553,.T.);
#43375=ORIENTED_EDGE('',*,*,#30551,.F.);
#43376=ORIENTED_EDGE('',*,*,#30553,.F.);
#43377=ORIENTED_EDGE('',*,*,#30554,.F.);
#43378=ORIENTED_EDGE('',*,*,#30555,.T.);
#43379=ORIENTED_EDGE('',*,*,#30556,.F.);
#43380=ORIENTED_EDGE('',*,*,#30555,.F.);
#43381=ORIENTED_EDGE('',*,*,#30557,.F.);
#43382=ORIENTED_EDGE('',*,*,#30558,.T.);
#43383=ORIENTED_EDGE('',*,*,#30559,.F.);
#43384=ORIENTED_EDGE('',*,*,#30558,.F.);
#43385=ORIENTED_EDGE('',*,*,#30560,.F.);
#43386=ORIENTED_EDGE('',*,*,#30561,.T.);
#43387=ORIENTED_EDGE('',*,*,#30562,.F.);
#43388=ORIENTED_EDGE('',*,*,#30561,.F.);
#43389=ORIENTED_EDGE('',*,*,#30563,.F.);
#43390=ORIENTED_EDGE('',*,*,#30564,.T.);
#43391=ORIENTED_EDGE('',*,*,#30565,.F.);
#43392=ORIENTED_EDGE('',*,*,#30564,.F.);
#43393=ORIENTED_EDGE('',*,*,#30566,.F.);
#43394=ORIENTED_EDGE('',*,*,#30567,.T.);
#43395=ORIENTED_EDGE('',*,*,#30543,.F.);
#43396=ORIENTED_EDGE('',*,*,#30567,.F.);
#43397=ORIENTED_EDGE('',*,*,#30566,.T.);
#43398=ORIENTED_EDGE('',*,*,#30562,.T.);
#43399=ORIENTED_EDGE('',*,*,#30568,.F.);
#43400=ORIENTED_EDGE('',*,*,#30569,.T.);
#43401=ORIENTED_EDGE('',*,*,#30544,.F.);
#43402=ORIENTED_EDGE('',*,*,#30569,.F.);
#43403=ORIENTED_EDGE('',*,*,#30568,.T.);
#43404=ORIENTED_EDGE('',*,*,#30559,.T.);
#43405=ORIENTED_EDGE('',*,*,#30570,.F.);
#43406=ORIENTED_EDGE('',*,*,#30571,.T.);
#43407=ORIENTED_EDGE('',*,*,#30545,.F.);
#43408=ORIENTED_EDGE('',*,*,#30571,.F.);
#43409=ORIENTED_EDGE('',*,*,#30570,.T.);
#43410=ORIENTED_EDGE('',*,*,#30556,.T.);
#43411=ORIENTED_EDGE('',*,*,#30572,.F.);
#43412=ORIENTED_EDGE('',*,*,#30573,.T.);
#43413=ORIENTED_EDGE('',*,*,#30546,.F.);
#43414=ORIENTED_EDGE('',*,*,#30573,.F.);
#43415=ORIENTED_EDGE('',*,*,#30572,.T.);
#43416=ORIENTED_EDGE('',*,*,#30565,.T.);
#43417=ORIENTED_EDGE('',*,*,#30574,.T.);
#43418=ORIENTED_EDGE('',*,*,#30575,.T.);
#43419=ORIENTED_EDGE('',*,*,#30574,.F.);
#43420=ORIENTED_EDGE('',*,*,#30575,.F.);
#43421=ORIENTED_EDGE('',*,*,#30576,.T.);
#43422=ORIENTED_EDGE('',*,*,#30577,.T.);
#43423=ORIENTED_EDGE('',*,*,#30576,.F.);
#43424=ORIENTED_EDGE('',*,*,#30577,.F.);
#43425=ORIENTED_EDGE('',*,*,#30578,.T.);
#43426=ORIENTED_EDGE('',*,*,#30579,.F.);
#43427=ORIENTED_EDGE('',*,*,#30578,.F.);
#43428=ORIENTED_EDGE('',*,*,#30547,.T.);
#43429=ORIENTED_EDGE('',*,*,#30580,.T.);
#43430=ORIENTED_EDGE('',*,*,#30581,.T.);
#43431=ORIENTED_EDGE('',*,*,#30582,.T.);
#43432=ORIENTED_EDGE('',*,*,#30580,.F.);
#43433=ORIENTED_EDGE('',*,*,#30583,.F.);
#43434=ORIENTED_EDGE('',*,*,#30584,.T.);
#43435=ORIENTED_EDGE('',*,*,#30581,.F.);
#43436=ORIENTED_EDGE('',*,*,#30582,.F.);
#43437=ORIENTED_EDGE('',*,*,#30584,.F.);
#43438=ORIENTED_EDGE('',*,*,#30585,.F.);
#43439=ORIENTED_EDGE('',*,*,#30586,.F.);
#43440=ORIENTED_EDGE('',*,*,#30587,.T.);
#43441=ORIENTED_EDGE('',*,*,#30585,.T.);
#43442=ORIENTED_EDGE('',*,*,#30587,.F.);
#43443=ORIENTED_EDGE('',*,*,#30588,.F.);
#43444=ORIENTED_EDGE('',*,*,#30589,.T.);
#43445=ORIENTED_EDGE('',*,*,#30586,.T.);
#43446=ORIENTED_EDGE('',*,*,#30589,.F.);
#43447=ORIENTED_EDGE('',*,*,#30590,.F.);
#43448=ORIENTED_EDGE('',*,*,#30588,.T.);
#43449=ORIENTED_EDGE('',*,*,#30548,.T.);
#43450=ORIENTED_EDGE('',*,*,#30563,.T.);
#43451=ORIENTED_EDGE('',*,*,#30560,.T.);
#43452=ORIENTED_EDGE('',*,*,#30557,.T.);
#43453=ORIENTED_EDGE('',*,*,#30554,.T.);
#43454=ORIENTED_EDGE('',*,*,#30552,.T.);
#43455=ORIENTED_EDGE('',*,*,#30591,.F.);
#43456=ORIENTED_EDGE('',*,*,#30592,.T.);
#43457=ORIENTED_EDGE('',*,*,#30590,.T.);
#43458=ORIENTED_EDGE('',*,*,#30592,.F.);
#43459=ORIENTED_EDGE('',*,*,#30593,.F.);
#43460=ORIENTED_EDGE('',*,*,#30594,.T.);
#43461=ORIENTED_EDGE('',*,*,#30591,.T.);
#43462=ORIENTED_EDGE('',*,*,#30594,.F.);
#43463=ORIENTED_EDGE('',*,*,#30541,.F.);
#43464=ORIENTED_EDGE('',*,*,#30595,.T.);
#43465=ORIENTED_EDGE('',*,*,#30593,.T.);
#43466=ORIENTED_EDGE('',*,*,#30595,.F.);
#43467=ORIENTED_EDGE('',*,*,#30583,.T.);
#43468=ORIENTED_EDGE('',*,*,#30596,.F.);
#43469=ORIENTED_EDGE('',*,*,#30597,.F.);
#43470=ORIENTED_EDGE('',*,*,#30598,.T.);
#43471=ORIENTED_EDGE('',*,*,#30596,.T.);
#43472=ORIENTED_EDGE('',*,*,#30598,.F.);
#43473=ORIENTED_EDGE('',*,*,#30599,.F.);
#43474=ORIENTED_EDGE('',*,*,#30600,.T.);
#43475=ORIENTED_EDGE('',*,*,#30597,.T.);
#43476=ORIENTED_EDGE('',*,*,#30600,.F.);
#43477=ORIENTED_EDGE('',*,*,#30599,.T.);
#43478=ORIENTED_EDGE('',*,*,#30579,.T.);
#43479=ORIENTED_EDGE('',*,*,#30601,.F.);
#43480=ORIENTED_EDGE('',*,*,#30602,.T.);
#43481=ORIENTED_EDGE('',*,*,#30603,.T.);
#43482=ORIENTED_EDGE('',*,*,#30604,.F.);
#43483=ORIENTED_EDGE('',*,*,#30605,.F.);
#43484=ORIENTED_EDGE('',*,*,#30606,.T.);
#43485=ORIENTED_EDGE('',*,*,#30607,.T.);
#43486=ORIENTED_EDGE('',*,*,#30602,.F.);
#43487=ORIENTED_EDGE('',*,*,#30608,.F.);
#43488=ORIENTED_EDGE('',*,*,#30609,.T.);
#43489=ORIENTED_EDGE('',*,*,#30610,.T.);
#43490=ORIENTED_EDGE('',*,*,#30606,.F.);
#43491=ORIENTED_EDGE('',*,*,#30611,.F.);
#43492=ORIENTED_EDGE('',*,*,#30612,.T.);
#43493=ORIENTED_EDGE('',*,*,#30613,.T.);
#43494=ORIENTED_EDGE('',*,*,#30609,.F.);
#43495=ORIENTED_EDGE('',*,*,#30614,.F.);
#43496=ORIENTED_EDGE('',*,*,#30615,.T.);
#43497=ORIENTED_EDGE('',*,*,#30616,.T.);
#43498=ORIENTED_EDGE('',*,*,#30612,.F.);
#43499=ORIENTED_EDGE('',*,*,#30617,.F.);
#43500=ORIENTED_EDGE('',*,*,#30618,.T.);
#43501=ORIENTED_EDGE('',*,*,#30619,.T.);
#43502=ORIENTED_EDGE('',*,*,#30615,.F.);
#43503=ORIENTED_EDGE('',*,*,#30620,.F.);
#43504=ORIENTED_EDGE('',*,*,#30621,.T.);
#43505=ORIENTED_EDGE('',*,*,#30622,.T.);
#43506=ORIENTED_EDGE('',*,*,#30618,.F.);
#43507=ORIENTED_EDGE('',*,*,#30623,.F.);
#43508=ORIENTED_EDGE('',*,*,#30624,.T.);
#43509=ORIENTED_EDGE('',*,*,#30625,.T.);
#43510=ORIENTED_EDGE('',*,*,#30621,.F.);
#43511=ORIENTED_EDGE('',*,*,#30626,.F.);
#43512=ORIENTED_EDGE('',*,*,#30627,.T.);
#43513=ORIENTED_EDGE('',*,*,#30628,.T.);
#43514=ORIENTED_EDGE('',*,*,#30624,.F.);
#43515=ORIENTED_EDGE('',*,*,#30629,.F.);
#43516=ORIENTED_EDGE('',*,*,#30630,.T.);
#43517=ORIENTED_EDGE('',*,*,#30631,.T.);
#43518=ORIENTED_EDGE('',*,*,#30627,.F.);
#43519=ORIENTED_EDGE('',*,*,#30632,.F.);
#43520=ORIENTED_EDGE('',*,*,#30633,.T.);
#43521=ORIENTED_EDGE('',*,*,#30634,.T.);
#43522=ORIENTED_EDGE('',*,*,#30630,.F.);
#43523=ORIENTED_EDGE('',*,*,#30635,.F.);
#43524=ORIENTED_EDGE('',*,*,#30604,.T.);
#43525=ORIENTED_EDGE('',*,*,#30636,.T.);
#43526=ORIENTED_EDGE('',*,*,#30633,.F.);
#43527=ORIENTED_EDGE('',*,*,#30636,.F.);
#43528=ORIENTED_EDGE('',*,*,#30603,.F.);
#43529=ORIENTED_EDGE('',*,*,#30607,.F.);
#43530=ORIENTED_EDGE('',*,*,#30610,.F.);
#43531=ORIENTED_EDGE('',*,*,#30613,.F.);
#43532=ORIENTED_EDGE('',*,*,#30616,.F.);
#43533=ORIENTED_EDGE('',*,*,#30619,.F.);
#43534=ORIENTED_EDGE('',*,*,#30622,.F.);
#43535=ORIENTED_EDGE('',*,*,#30625,.F.);
#43536=ORIENTED_EDGE('',*,*,#30628,.F.);
#43537=ORIENTED_EDGE('',*,*,#30631,.F.);
#43538=ORIENTED_EDGE('',*,*,#30634,.F.);
#43539=ORIENTED_EDGE('',*,*,#30637,.F.);
#43540=ORIENTED_EDGE('',*,*,#30638,.T.);
#43541=ORIENTED_EDGE('',*,*,#30639,.T.);
#43542=ORIENTED_EDGE('',*,*,#30640,.F.);
#43543=ORIENTED_EDGE('',*,*,#30641,.F.);
#43544=ORIENTED_EDGE('',*,*,#30642,.T.);
#43545=ORIENTED_EDGE('',*,*,#30643,.T.);
#43546=ORIENTED_EDGE('',*,*,#30638,.F.);
#43547=ORIENTED_EDGE('',*,*,#30644,.F.);
#43548=ORIENTED_EDGE('',*,*,#30645,.T.);
#43549=ORIENTED_EDGE('',*,*,#30646,.T.);
#43550=ORIENTED_EDGE('',*,*,#30642,.F.);
#43551=ORIENTED_EDGE('',*,*,#30647,.F.);
#43552=ORIENTED_EDGE('',*,*,#30640,.T.);
#43553=ORIENTED_EDGE('',*,*,#30648,.T.);
#43554=ORIENTED_EDGE('',*,*,#30645,.F.);
#43555=ORIENTED_EDGE('',*,*,#30648,.F.);
#43556=ORIENTED_EDGE('',*,*,#30639,.F.);
#43557=ORIENTED_EDGE('',*,*,#30643,.F.);
#43558=ORIENTED_EDGE('',*,*,#30646,.F.);
#43559=ORIENTED_EDGE('',*,*,#30649,.F.);
#43560=ORIENTED_EDGE('',*,*,#30650,.T.);
#43561=ORIENTED_EDGE('',*,*,#30651,.T.);
#43562=ORIENTED_EDGE('',*,*,#30652,.F.);
#43563=ORIENTED_EDGE('',*,*,#30653,.F.);
#43564=ORIENTED_EDGE('',*,*,#30654,.T.);
#43565=ORIENTED_EDGE('',*,*,#30655,.T.);
#43566=ORIENTED_EDGE('',*,*,#30650,.F.);
#43567=ORIENTED_EDGE('',*,*,#30656,.F.);
#43568=ORIENTED_EDGE('',*,*,#30657,.T.);
#43569=ORIENTED_EDGE('',*,*,#30658,.T.);
#43570=ORIENTED_EDGE('',*,*,#30654,.F.);
#43571=ORIENTED_EDGE('',*,*,#30659,.F.);
#43572=ORIENTED_EDGE('',*,*,#30660,.T.);
#43573=ORIENTED_EDGE('',*,*,#30661,.T.);
#43574=ORIENTED_EDGE('',*,*,#30657,.F.);
#43575=ORIENTED_EDGE('',*,*,#30662,.F.);
#43576=ORIENTED_EDGE('',*,*,#30663,.T.);
#43577=ORIENTED_EDGE('',*,*,#30664,.T.);
#43578=ORIENTED_EDGE('',*,*,#30660,.F.);
#43579=ORIENTED_EDGE('',*,*,#30665,.F.);
#43580=ORIENTED_EDGE('',*,*,#30666,.T.);
#43581=ORIENTED_EDGE('',*,*,#30667,.T.);
#43582=ORIENTED_EDGE('',*,*,#30663,.F.);
#43583=ORIENTED_EDGE('',*,*,#30668,.F.);
#43584=ORIENTED_EDGE('',*,*,#30669,.T.);
#43585=ORIENTED_EDGE('',*,*,#30670,.T.);
#43586=ORIENTED_EDGE('',*,*,#30666,.F.);
#43587=ORIENTED_EDGE('',*,*,#30671,.F.);
#43588=ORIENTED_EDGE('',*,*,#30672,.T.);
#43589=ORIENTED_EDGE('',*,*,#30673,.T.);
#43590=ORIENTED_EDGE('',*,*,#30669,.F.);
#43591=ORIENTED_EDGE('',*,*,#30674,.F.);
#43592=ORIENTED_EDGE('',*,*,#30675,.T.);
#43593=ORIENTED_EDGE('',*,*,#30676,.T.);
#43594=ORIENTED_EDGE('',*,*,#30672,.F.);
#43595=ORIENTED_EDGE('',*,*,#30677,.F.);
#43596=ORIENTED_EDGE('',*,*,#30678,.T.);
#43597=ORIENTED_EDGE('',*,*,#30679,.T.);
#43598=ORIENTED_EDGE('',*,*,#30675,.F.);
#43599=ORIENTED_EDGE('',*,*,#30680,.F.);
#43600=ORIENTED_EDGE('',*,*,#30681,.T.);
#43601=ORIENTED_EDGE('',*,*,#30682,.T.);
#43602=ORIENTED_EDGE('',*,*,#30678,.F.);
#43603=ORIENTED_EDGE('',*,*,#30683,.F.);
#43604=ORIENTED_EDGE('',*,*,#30684,.T.);
#43605=ORIENTED_EDGE('',*,*,#30685,.T.);
#43606=ORIENTED_EDGE('',*,*,#30681,.F.);
#43607=ORIENTED_EDGE('',*,*,#30686,.F.);
#43608=ORIENTED_EDGE('',*,*,#30687,.T.);
#43609=ORIENTED_EDGE('',*,*,#30688,.T.);
#43610=ORIENTED_EDGE('',*,*,#30684,.F.);
#43611=ORIENTED_EDGE('',*,*,#30689,.F.);
#43612=ORIENTED_EDGE('',*,*,#30690,.T.);
#43613=ORIENTED_EDGE('',*,*,#30691,.T.);
#43614=ORIENTED_EDGE('',*,*,#30687,.F.);
#43615=ORIENTED_EDGE('',*,*,#30692,.F.);
#43616=ORIENTED_EDGE('',*,*,#30693,.T.);
#43617=ORIENTED_EDGE('',*,*,#30694,.T.);
#43618=ORIENTED_EDGE('',*,*,#30690,.F.);
#43619=ORIENTED_EDGE('',*,*,#30695,.F.);
#43620=ORIENTED_EDGE('',*,*,#30696,.T.);
#43621=ORIENTED_EDGE('',*,*,#30697,.T.);
#43622=ORIENTED_EDGE('',*,*,#30693,.F.);
#43623=ORIENTED_EDGE('',*,*,#30698,.F.);
#43624=ORIENTED_EDGE('',*,*,#30699,.T.);
#43625=ORIENTED_EDGE('',*,*,#30700,.T.);
#43626=ORIENTED_EDGE('',*,*,#30696,.F.);
#43627=ORIENTED_EDGE('',*,*,#30701,.F.);
#43628=ORIENTED_EDGE('',*,*,#30702,.T.);
#43629=ORIENTED_EDGE('',*,*,#30703,.T.);
#43630=ORIENTED_EDGE('',*,*,#30699,.F.);
#43631=ORIENTED_EDGE('',*,*,#30704,.F.);
#43632=ORIENTED_EDGE('',*,*,#30705,.T.);
#43633=ORIENTED_EDGE('',*,*,#30706,.T.);
#43634=ORIENTED_EDGE('',*,*,#30702,.F.);
#43635=ORIENTED_EDGE('',*,*,#30707,.F.);
#43636=ORIENTED_EDGE('',*,*,#30708,.T.);
#43637=ORIENTED_EDGE('',*,*,#30709,.T.);
#43638=ORIENTED_EDGE('',*,*,#30705,.F.);
#43639=ORIENTED_EDGE('',*,*,#30710,.F.);
#43640=ORIENTED_EDGE('',*,*,#30711,.T.);
#43641=ORIENTED_EDGE('',*,*,#30712,.T.);
#43642=ORIENTED_EDGE('',*,*,#30708,.F.);
#43643=ORIENTED_EDGE('',*,*,#30713,.F.);
#43644=ORIENTED_EDGE('',*,*,#30714,.T.);
#43645=ORIENTED_EDGE('',*,*,#30715,.T.);
#43646=ORIENTED_EDGE('',*,*,#30711,.F.);
#43647=ORIENTED_EDGE('',*,*,#30716,.F.);
#43648=ORIENTED_EDGE('',*,*,#30717,.T.);
#43649=ORIENTED_EDGE('',*,*,#30718,.T.);
#43650=ORIENTED_EDGE('',*,*,#30714,.F.);
#43651=ORIENTED_EDGE('',*,*,#30719,.F.);
#43652=ORIENTED_EDGE('',*,*,#30720,.T.);
#43653=ORIENTED_EDGE('',*,*,#30721,.T.);
#43654=ORIENTED_EDGE('',*,*,#30717,.F.);
#43655=ORIENTED_EDGE('',*,*,#30722,.F.);
#43656=ORIENTED_EDGE('',*,*,#30723,.T.);
#43657=ORIENTED_EDGE('',*,*,#30724,.T.);
#43658=ORIENTED_EDGE('',*,*,#30720,.F.);
#43659=ORIENTED_EDGE('',*,*,#30725,.F.);
#43660=ORIENTED_EDGE('',*,*,#30726,.T.);
#43661=ORIENTED_EDGE('',*,*,#30727,.T.);
#43662=ORIENTED_EDGE('',*,*,#30723,.F.);
#43663=ORIENTED_EDGE('',*,*,#30728,.F.);
#43664=ORIENTED_EDGE('',*,*,#30729,.T.);
#43665=ORIENTED_EDGE('',*,*,#30730,.T.);
#43666=ORIENTED_EDGE('',*,*,#30726,.F.);
#43667=ORIENTED_EDGE('',*,*,#30731,.F.);
#43668=ORIENTED_EDGE('',*,*,#30732,.T.);
#43669=ORIENTED_EDGE('',*,*,#30733,.T.);
#43670=ORIENTED_EDGE('',*,*,#30729,.F.);
#43671=ORIENTED_EDGE('',*,*,#30734,.F.);
#43672=ORIENTED_EDGE('',*,*,#30735,.T.);
#43673=ORIENTED_EDGE('',*,*,#30736,.T.);
#43674=ORIENTED_EDGE('',*,*,#30732,.F.);
#43675=ORIENTED_EDGE('',*,*,#30737,.F.);
#43676=ORIENTED_EDGE('',*,*,#30738,.T.);
#43677=ORIENTED_EDGE('',*,*,#30739,.T.);
#43678=ORIENTED_EDGE('',*,*,#30735,.F.);
#43679=ORIENTED_EDGE('',*,*,#30740,.F.);
#43680=ORIENTED_EDGE('',*,*,#30741,.T.);
#43681=ORIENTED_EDGE('',*,*,#30742,.T.);
#43682=ORIENTED_EDGE('',*,*,#30738,.F.);
#43683=ORIENTED_EDGE('',*,*,#30743,.F.);
#43684=ORIENTED_EDGE('',*,*,#30744,.T.);
#43685=ORIENTED_EDGE('',*,*,#30745,.T.);
#43686=ORIENTED_EDGE('',*,*,#30741,.F.);
#43687=ORIENTED_EDGE('',*,*,#30746,.F.);
#43688=ORIENTED_EDGE('',*,*,#30747,.T.);
#43689=ORIENTED_EDGE('',*,*,#30748,.T.);
#43690=ORIENTED_EDGE('',*,*,#30744,.F.);
#43691=ORIENTED_EDGE('',*,*,#30749,.F.);
#43692=ORIENTED_EDGE('',*,*,#30750,.T.);
#43693=ORIENTED_EDGE('',*,*,#30751,.T.);
#43694=ORIENTED_EDGE('',*,*,#30747,.F.);
#43695=ORIENTED_EDGE('',*,*,#30752,.F.);
#43696=ORIENTED_EDGE('',*,*,#30652,.T.);
#43697=ORIENTED_EDGE('',*,*,#30753,.T.);
#43698=ORIENTED_EDGE('',*,*,#30750,.F.);
#43699=ORIENTED_EDGE('',*,*,#30753,.F.);
#43700=ORIENTED_EDGE('',*,*,#30651,.F.);
#43701=ORIENTED_EDGE('',*,*,#30655,.F.);
#43702=ORIENTED_EDGE('',*,*,#30658,.F.);
#43703=ORIENTED_EDGE('',*,*,#30661,.F.);
#43704=ORIENTED_EDGE('',*,*,#30664,.F.);
#43705=ORIENTED_EDGE('',*,*,#30667,.F.);
#43706=ORIENTED_EDGE('',*,*,#30670,.F.);
#43707=ORIENTED_EDGE('',*,*,#30673,.F.);
#43708=ORIENTED_EDGE('',*,*,#30676,.F.);
#43709=ORIENTED_EDGE('',*,*,#30679,.F.);
#43710=ORIENTED_EDGE('',*,*,#30682,.F.);
#43711=ORIENTED_EDGE('',*,*,#30685,.F.);
#43712=ORIENTED_EDGE('',*,*,#30688,.F.);
#43713=ORIENTED_EDGE('',*,*,#30691,.F.);
#43714=ORIENTED_EDGE('',*,*,#30694,.F.);
#43715=ORIENTED_EDGE('',*,*,#30697,.F.);
#43716=ORIENTED_EDGE('',*,*,#30700,.F.);
#43717=ORIENTED_EDGE('',*,*,#30703,.F.);
#43718=ORIENTED_EDGE('',*,*,#30706,.F.);
#43719=ORIENTED_EDGE('',*,*,#30709,.F.);
#43720=ORIENTED_EDGE('',*,*,#30712,.F.);
#43721=ORIENTED_EDGE('',*,*,#30715,.F.);
#43722=ORIENTED_EDGE('',*,*,#30718,.F.);
#43723=ORIENTED_EDGE('',*,*,#30721,.F.);
#43724=ORIENTED_EDGE('',*,*,#30724,.F.);
#43725=ORIENTED_EDGE('',*,*,#30727,.F.);
#43726=ORIENTED_EDGE('',*,*,#30730,.F.);
#43727=ORIENTED_EDGE('',*,*,#30733,.F.);
#43728=ORIENTED_EDGE('',*,*,#30736,.F.);
#43729=ORIENTED_EDGE('',*,*,#30739,.F.);
#43730=ORIENTED_EDGE('',*,*,#30742,.F.);
#43731=ORIENTED_EDGE('',*,*,#30745,.F.);
#43732=ORIENTED_EDGE('',*,*,#30748,.F.);
#43733=ORIENTED_EDGE('',*,*,#30751,.F.);
#43734=ORIENTED_EDGE('',*,*,#30754,.F.);
#43735=ORIENTED_EDGE('',*,*,#30755,.T.);
#43736=ORIENTED_EDGE('',*,*,#30756,.T.);
#43737=ORIENTED_EDGE('',*,*,#30757,.F.);
#43738=ORIENTED_EDGE('',*,*,#30758,.F.);
#43739=ORIENTED_EDGE('',*,*,#30759,.T.);
#43740=ORIENTED_EDGE('',*,*,#30760,.T.);
#43741=ORIENTED_EDGE('',*,*,#30755,.F.);
#43742=ORIENTED_EDGE('',*,*,#30761,.F.);
#43743=ORIENTED_EDGE('',*,*,#30762,.T.);
#43744=ORIENTED_EDGE('',*,*,#30763,.T.);
#43745=ORIENTED_EDGE('',*,*,#30759,.F.);
#43746=ORIENTED_EDGE('',*,*,#30764,.F.);
#43747=ORIENTED_EDGE('',*,*,#30765,.T.);
#43748=ORIENTED_EDGE('',*,*,#30766,.T.);
#43749=ORIENTED_EDGE('',*,*,#30762,.F.);
#43750=ORIENTED_EDGE('',*,*,#30767,.F.);
#43751=ORIENTED_EDGE('',*,*,#30768,.T.);
#43752=ORIENTED_EDGE('',*,*,#30769,.T.);
#43753=ORIENTED_EDGE('',*,*,#30765,.F.);
#43754=ORIENTED_EDGE('',*,*,#30770,.F.);
#43755=ORIENTED_EDGE('',*,*,#30771,.T.);
#43756=ORIENTED_EDGE('',*,*,#30772,.T.);
#43757=ORIENTED_EDGE('',*,*,#30768,.F.);
#43758=ORIENTED_EDGE('',*,*,#30773,.F.);
#43759=ORIENTED_EDGE('',*,*,#30774,.T.);
#43760=ORIENTED_EDGE('',*,*,#30775,.T.);
#43761=ORIENTED_EDGE('',*,*,#30771,.F.);
#43762=ORIENTED_EDGE('',*,*,#30776,.F.);
#43763=ORIENTED_EDGE('',*,*,#30777,.T.);
#43764=ORIENTED_EDGE('',*,*,#30778,.T.);
#43765=ORIENTED_EDGE('',*,*,#30774,.F.);
#43766=ORIENTED_EDGE('',*,*,#30779,.F.);
#43767=ORIENTED_EDGE('',*,*,#30780,.T.);
#43768=ORIENTED_EDGE('',*,*,#30781,.T.);
#43769=ORIENTED_EDGE('',*,*,#30777,.F.);
#43770=ORIENTED_EDGE('',*,*,#30782,.F.);
#43771=ORIENTED_EDGE('',*,*,#30783,.T.);
#43772=ORIENTED_EDGE('',*,*,#30784,.T.);
#43773=ORIENTED_EDGE('',*,*,#30780,.F.);
#43774=ORIENTED_EDGE('',*,*,#30785,.F.);
#43775=ORIENTED_EDGE('',*,*,#30786,.T.);
#43776=ORIENTED_EDGE('',*,*,#30787,.T.);
#43777=ORIENTED_EDGE('',*,*,#30783,.F.);
#43778=ORIENTED_EDGE('',*,*,#30788,.F.);
#43779=ORIENTED_EDGE('',*,*,#30789,.T.);
#43780=ORIENTED_EDGE('',*,*,#30790,.T.);
#43781=ORIENTED_EDGE('',*,*,#30786,.F.);
#43782=ORIENTED_EDGE('',*,*,#30791,.F.);
#43783=ORIENTED_EDGE('',*,*,#30792,.T.);
#43784=ORIENTED_EDGE('',*,*,#30793,.T.);
#43785=ORIENTED_EDGE('',*,*,#30789,.F.);
#43786=ORIENTED_EDGE('',*,*,#30794,.F.);
#43787=ORIENTED_EDGE('',*,*,#30795,.T.);
#43788=ORIENTED_EDGE('',*,*,#30796,.T.);
#43789=ORIENTED_EDGE('',*,*,#30792,.F.);
#43790=ORIENTED_EDGE('',*,*,#30797,.F.);
#43791=ORIENTED_EDGE('',*,*,#30798,.T.);
#43792=ORIENTED_EDGE('',*,*,#30799,.T.);
#43793=ORIENTED_EDGE('',*,*,#30795,.F.);
#43794=ORIENTED_EDGE('',*,*,#30800,.F.);
#43795=ORIENTED_EDGE('',*,*,#30801,.T.);
#43796=ORIENTED_EDGE('',*,*,#30802,.T.);
#43797=ORIENTED_EDGE('',*,*,#30798,.F.);
#43798=ORIENTED_EDGE('',*,*,#30803,.F.);
#43799=ORIENTED_EDGE('',*,*,#30804,.T.);
#43800=ORIENTED_EDGE('',*,*,#30805,.T.);
#43801=ORIENTED_EDGE('',*,*,#30801,.F.);
#43802=ORIENTED_EDGE('',*,*,#30806,.F.);
#43803=ORIENTED_EDGE('',*,*,#30807,.T.);
#43804=ORIENTED_EDGE('',*,*,#30808,.T.);
#43805=ORIENTED_EDGE('',*,*,#30804,.F.);
#43806=ORIENTED_EDGE('',*,*,#30809,.F.);
#43807=ORIENTED_EDGE('',*,*,#30810,.T.);
#43808=ORIENTED_EDGE('',*,*,#30811,.T.);
#43809=ORIENTED_EDGE('',*,*,#30807,.F.);
#43810=ORIENTED_EDGE('',*,*,#30812,.F.);
#43811=ORIENTED_EDGE('',*,*,#30813,.T.);
#43812=ORIENTED_EDGE('',*,*,#30814,.T.);
#43813=ORIENTED_EDGE('',*,*,#30810,.F.);
#43814=ORIENTED_EDGE('',*,*,#30815,.F.);
#43815=ORIENTED_EDGE('',*,*,#30816,.T.);
#43816=ORIENTED_EDGE('',*,*,#30817,.T.);
#43817=ORIENTED_EDGE('',*,*,#30813,.F.);
#43818=ORIENTED_EDGE('',*,*,#30818,.F.);
#43819=ORIENTED_EDGE('',*,*,#30757,.T.);
#43820=ORIENTED_EDGE('',*,*,#30819,.T.);
#43821=ORIENTED_EDGE('',*,*,#30816,.F.);
#43822=ORIENTED_EDGE('',*,*,#30819,.F.);
#43823=ORIENTED_EDGE('',*,*,#30756,.F.);
#43824=ORIENTED_EDGE('',*,*,#30760,.F.);
#43825=ORIENTED_EDGE('',*,*,#30763,.F.);
#43826=ORIENTED_EDGE('',*,*,#30766,.F.);
#43827=ORIENTED_EDGE('',*,*,#30769,.F.);
#43828=ORIENTED_EDGE('',*,*,#30772,.F.);
#43829=ORIENTED_EDGE('',*,*,#30775,.F.);
#43830=ORIENTED_EDGE('',*,*,#30778,.F.);
#43831=ORIENTED_EDGE('',*,*,#30781,.F.);
#43832=ORIENTED_EDGE('',*,*,#30784,.F.);
#43833=ORIENTED_EDGE('',*,*,#30787,.F.);
#43834=ORIENTED_EDGE('',*,*,#30790,.F.);
#43835=ORIENTED_EDGE('',*,*,#30793,.F.);
#43836=ORIENTED_EDGE('',*,*,#30796,.F.);
#43837=ORIENTED_EDGE('',*,*,#30799,.F.);
#43838=ORIENTED_EDGE('',*,*,#30802,.F.);
#43839=ORIENTED_EDGE('',*,*,#30805,.F.);
#43840=ORIENTED_EDGE('',*,*,#30808,.F.);
#43841=ORIENTED_EDGE('',*,*,#30811,.F.);
#43842=ORIENTED_EDGE('',*,*,#30814,.F.);
#43843=ORIENTED_EDGE('',*,*,#30817,.F.);
#43844=ORIENTED_EDGE('',*,*,#30820,.F.);
#43845=ORIENTED_EDGE('',*,*,#30821,.T.);
#43846=ORIENTED_EDGE('',*,*,#30822,.T.);
#43847=ORIENTED_EDGE('',*,*,#30823,.F.);
#43848=ORIENTED_EDGE('',*,*,#30824,.F.);
#43849=ORIENTED_EDGE('',*,*,#30825,.T.);
#43850=ORIENTED_EDGE('',*,*,#30826,.T.);
#43851=ORIENTED_EDGE('',*,*,#30821,.F.);
#43852=ORIENTED_EDGE('',*,*,#30827,.F.);
#43853=ORIENTED_EDGE('',*,*,#30828,.T.);
#43854=ORIENTED_EDGE('',*,*,#30829,.T.);
#43855=ORIENTED_EDGE('',*,*,#30825,.F.);
#43856=ORIENTED_EDGE('',*,*,#30830,.F.);
#43857=ORIENTED_EDGE('',*,*,#30831,.T.);
#43858=ORIENTED_EDGE('',*,*,#30832,.T.);
#43859=ORIENTED_EDGE('',*,*,#30828,.F.);
#43860=ORIENTED_EDGE('',*,*,#30833,.F.);
#43861=ORIENTED_EDGE('',*,*,#30834,.T.);
#43862=ORIENTED_EDGE('',*,*,#30835,.T.);
#43863=ORIENTED_EDGE('',*,*,#30831,.F.);
#43864=ORIENTED_EDGE('',*,*,#30836,.F.);
#43865=ORIENTED_EDGE('',*,*,#30823,.T.);
#43866=ORIENTED_EDGE('',*,*,#30837,.T.);
#43867=ORIENTED_EDGE('',*,*,#30834,.F.);
#43868=ORIENTED_EDGE('',*,*,#30837,.F.);
#43869=ORIENTED_EDGE('',*,*,#30822,.F.);
#43870=ORIENTED_EDGE('',*,*,#30826,.F.);
#43871=ORIENTED_EDGE('',*,*,#30829,.F.);
#43872=ORIENTED_EDGE('',*,*,#30832,.F.);
#43873=ORIENTED_EDGE('',*,*,#30835,.F.);
#43874=ORIENTED_EDGE('',*,*,#30838,.F.);
#43875=ORIENTED_EDGE('',*,*,#30839,.T.);
#43876=ORIENTED_EDGE('',*,*,#30840,.T.);
#43877=ORIENTED_EDGE('',*,*,#30841,.F.);
#43878=ORIENTED_EDGE('',*,*,#30842,.F.);
#43879=ORIENTED_EDGE('',*,*,#30843,.T.);
#43880=ORIENTED_EDGE('',*,*,#30844,.T.);
#43881=ORIENTED_EDGE('',*,*,#30839,.F.);
#43882=ORIENTED_EDGE('',*,*,#30845,.F.);
#43883=ORIENTED_EDGE('',*,*,#30846,.T.);
#43884=ORIENTED_EDGE('',*,*,#30847,.T.);
#43885=ORIENTED_EDGE('',*,*,#30843,.F.);
#43886=ORIENTED_EDGE('',*,*,#30848,.F.);
#43887=ORIENTED_EDGE('',*,*,#30849,.T.);
#43888=ORIENTED_EDGE('',*,*,#30850,.T.);
#43889=ORIENTED_EDGE('',*,*,#30846,.F.);
#43890=ORIENTED_EDGE('',*,*,#30851,.F.);
#43891=ORIENTED_EDGE('',*,*,#30852,.T.);
#43892=ORIENTED_EDGE('',*,*,#30853,.T.);
#43893=ORIENTED_EDGE('',*,*,#30849,.F.);
#43894=ORIENTED_EDGE('',*,*,#30854,.F.);
#43895=ORIENTED_EDGE('',*,*,#30855,.T.);
#43896=ORIENTED_EDGE('',*,*,#30856,.T.);
#43897=ORIENTED_EDGE('',*,*,#30852,.F.);
#43898=ORIENTED_EDGE('',*,*,#30857,.F.);
#43899=ORIENTED_EDGE('',*,*,#30858,.T.);
#43900=ORIENTED_EDGE('',*,*,#30859,.T.);
#43901=ORIENTED_EDGE('',*,*,#30855,.F.);
#43902=ORIENTED_EDGE('',*,*,#30860,.F.);
#43903=ORIENTED_EDGE('',*,*,#30841,.T.);
#43904=ORIENTED_EDGE('',*,*,#30861,.T.);
#43905=ORIENTED_EDGE('',*,*,#30858,.F.);
#43906=ORIENTED_EDGE('',*,*,#30861,.F.);
#43907=ORIENTED_EDGE('',*,*,#30840,.F.);
#43908=ORIENTED_EDGE('',*,*,#30844,.F.);
#43909=ORIENTED_EDGE('',*,*,#30847,.F.);
#43910=ORIENTED_EDGE('',*,*,#30850,.F.);
#43911=ORIENTED_EDGE('',*,*,#30853,.F.);
#43912=ORIENTED_EDGE('',*,*,#30856,.F.);
#43913=ORIENTED_EDGE('',*,*,#30859,.F.);
#43914=ORIENTED_EDGE('',*,*,#30862,.F.);
#43915=ORIENTED_EDGE('',*,*,#30863,.T.);
#43916=ORIENTED_EDGE('',*,*,#30864,.T.);
#43917=ORIENTED_EDGE('',*,*,#30865,.F.);
#43918=ORIENTED_EDGE('',*,*,#30866,.F.);
#43919=ORIENTED_EDGE('',*,*,#30867,.T.);
#43920=ORIENTED_EDGE('',*,*,#30868,.T.);
#43921=ORIENTED_EDGE('',*,*,#30863,.F.);
#43922=ORIENTED_EDGE('',*,*,#30869,.F.);
#43923=ORIENTED_EDGE('',*,*,#30870,.T.);
#43924=ORIENTED_EDGE('',*,*,#30871,.T.);
#43925=ORIENTED_EDGE('',*,*,#30867,.F.);
#43926=ORIENTED_EDGE('',*,*,#30872,.F.);
#43927=ORIENTED_EDGE('',*,*,#30873,.T.);
#43928=ORIENTED_EDGE('',*,*,#30874,.T.);
#43929=ORIENTED_EDGE('',*,*,#30870,.F.);
#43930=ORIENTED_EDGE('',*,*,#30875,.F.);
#43931=ORIENTED_EDGE('',*,*,#30876,.T.);
#43932=ORIENTED_EDGE('',*,*,#30877,.T.);
#43933=ORIENTED_EDGE('',*,*,#30873,.F.);
#43934=ORIENTED_EDGE('',*,*,#30878,.F.);
#43935=ORIENTED_EDGE('',*,*,#30879,.T.);
#43936=ORIENTED_EDGE('',*,*,#30880,.T.);
#43937=ORIENTED_EDGE('',*,*,#30876,.F.);
#43938=ORIENTED_EDGE('',*,*,#30881,.F.);
#43939=ORIENTED_EDGE('',*,*,#30882,.T.);
#43940=ORIENTED_EDGE('',*,*,#30883,.T.);
#43941=ORIENTED_EDGE('',*,*,#30879,.F.);
#43942=ORIENTED_EDGE('',*,*,#30884,.F.);
#43943=ORIENTED_EDGE('',*,*,#30885,.T.);
#43944=ORIENTED_EDGE('',*,*,#30886,.T.);
#43945=ORIENTED_EDGE('',*,*,#30882,.F.);
#43946=ORIENTED_EDGE('',*,*,#30887,.F.);
#43947=ORIENTED_EDGE('',*,*,#30888,.T.);
#43948=ORIENTED_EDGE('',*,*,#30889,.T.);
#43949=ORIENTED_EDGE('',*,*,#30885,.F.);
#43950=ORIENTED_EDGE('',*,*,#30890,.F.);
#43951=ORIENTED_EDGE('',*,*,#30891,.T.);
#43952=ORIENTED_EDGE('',*,*,#30892,.T.);
#43953=ORIENTED_EDGE('',*,*,#30888,.F.);
#43954=ORIENTED_EDGE('',*,*,#30893,.F.);
#43955=ORIENTED_EDGE('',*,*,#30894,.T.);
#43956=ORIENTED_EDGE('',*,*,#30895,.T.);
#43957=ORIENTED_EDGE('',*,*,#30891,.F.);
#43958=ORIENTED_EDGE('',*,*,#30896,.F.);
#43959=ORIENTED_EDGE('',*,*,#30897,.T.);
#43960=ORIENTED_EDGE('',*,*,#30898,.T.);
#43961=ORIENTED_EDGE('',*,*,#30894,.F.);
#43962=ORIENTED_EDGE('',*,*,#30899,.F.);
#43963=ORIENTED_EDGE('',*,*,#30900,.T.);
#43964=ORIENTED_EDGE('',*,*,#30901,.T.);
#43965=ORIENTED_EDGE('',*,*,#30897,.F.);
#43966=ORIENTED_EDGE('',*,*,#30902,.F.);
#43967=ORIENTED_EDGE('',*,*,#30903,.T.);
#43968=ORIENTED_EDGE('',*,*,#30904,.T.);
#43969=ORIENTED_EDGE('',*,*,#30900,.F.);
#43970=ORIENTED_EDGE('',*,*,#30905,.F.);
#43971=ORIENTED_EDGE('',*,*,#30906,.T.);
#43972=ORIENTED_EDGE('',*,*,#30907,.T.);
#43973=ORIENTED_EDGE('',*,*,#30903,.F.);
#43974=ORIENTED_EDGE('',*,*,#30908,.F.);
#43975=ORIENTED_EDGE('',*,*,#30909,.T.);
#43976=ORIENTED_EDGE('',*,*,#30910,.T.);
#43977=ORIENTED_EDGE('',*,*,#30906,.F.);
#43978=ORIENTED_EDGE('',*,*,#30911,.F.);
#43979=ORIENTED_EDGE('',*,*,#30865,.T.);
#43980=ORIENTED_EDGE('',*,*,#30912,.T.);
#43981=ORIENTED_EDGE('',*,*,#30909,.F.);
#43982=ORIENTED_EDGE('',*,*,#30912,.F.);
#43983=ORIENTED_EDGE('',*,*,#30864,.F.);
#43984=ORIENTED_EDGE('',*,*,#30868,.F.);
#43985=ORIENTED_EDGE('',*,*,#30871,.F.);
#43986=ORIENTED_EDGE('',*,*,#30874,.F.);
#43987=ORIENTED_EDGE('',*,*,#30877,.F.);
#43988=ORIENTED_EDGE('',*,*,#30880,.F.);
#43989=ORIENTED_EDGE('',*,*,#30883,.F.);
#43990=ORIENTED_EDGE('',*,*,#30886,.F.);
#43991=ORIENTED_EDGE('',*,*,#30889,.F.);
#43992=ORIENTED_EDGE('',*,*,#30892,.F.);
#43993=ORIENTED_EDGE('',*,*,#30895,.F.);
#43994=ORIENTED_EDGE('',*,*,#30898,.F.);
#43995=ORIENTED_EDGE('',*,*,#30901,.F.);
#43996=ORIENTED_EDGE('',*,*,#30904,.F.);
#43997=ORIENTED_EDGE('',*,*,#30907,.F.);
#43998=ORIENTED_EDGE('',*,*,#30910,.F.);
#43999=ORIENTED_EDGE('',*,*,#30913,.F.);
#44000=ORIENTED_EDGE('',*,*,#30914,.T.);
#44001=ORIENTED_EDGE('',*,*,#30915,.T.);
#44002=ORIENTED_EDGE('',*,*,#30916,.F.);
#44003=ORIENTED_EDGE('',*,*,#30917,.F.);
#44004=ORIENTED_EDGE('',*,*,#30918,.T.);
#44005=ORIENTED_EDGE('',*,*,#30919,.T.);
#44006=ORIENTED_EDGE('',*,*,#30914,.F.);
#44007=ORIENTED_EDGE('',*,*,#30920,.F.);
#44008=ORIENTED_EDGE('',*,*,#30921,.T.);
#44009=ORIENTED_EDGE('',*,*,#30922,.T.);
#44010=ORIENTED_EDGE('',*,*,#30918,.F.);
#44011=ORIENTED_EDGE('',*,*,#30923,.F.);
#44012=ORIENTED_EDGE('',*,*,#30924,.T.);
#44013=ORIENTED_EDGE('',*,*,#30925,.T.);
#44014=ORIENTED_EDGE('',*,*,#30921,.F.);
#44015=ORIENTED_EDGE('',*,*,#30926,.F.);
#44016=ORIENTED_EDGE('',*,*,#30927,.T.);
#44017=ORIENTED_EDGE('',*,*,#30928,.T.);
#44018=ORIENTED_EDGE('',*,*,#30924,.F.);
#44019=ORIENTED_EDGE('',*,*,#30929,.F.);
#44020=ORIENTED_EDGE('',*,*,#30930,.T.);
#44021=ORIENTED_EDGE('',*,*,#30931,.T.);
#44022=ORIENTED_EDGE('',*,*,#30927,.F.);
#44023=ORIENTED_EDGE('',*,*,#30932,.F.);
#44024=ORIENTED_EDGE('',*,*,#30933,.T.);
#44025=ORIENTED_EDGE('',*,*,#30934,.T.);
#44026=ORIENTED_EDGE('',*,*,#30930,.F.);
#44027=ORIENTED_EDGE('',*,*,#30935,.F.);
#44028=ORIENTED_EDGE('',*,*,#30936,.T.);
#44029=ORIENTED_EDGE('',*,*,#30937,.T.);
#44030=ORIENTED_EDGE('',*,*,#30933,.F.);
#44031=ORIENTED_EDGE('',*,*,#30938,.F.);
#44032=ORIENTED_EDGE('',*,*,#30939,.T.);
#44033=ORIENTED_EDGE('',*,*,#30940,.T.);
#44034=ORIENTED_EDGE('',*,*,#30936,.F.);
#44035=ORIENTED_EDGE('',*,*,#30941,.F.);
#44036=ORIENTED_EDGE('',*,*,#30942,.T.);
#44037=ORIENTED_EDGE('',*,*,#30943,.T.);
#44038=ORIENTED_EDGE('',*,*,#30939,.F.);
#44039=ORIENTED_EDGE('',*,*,#30944,.F.);
#44040=ORIENTED_EDGE('',*,*,#30945,.T.);
#44041=ORIENTED_EDGE('',*,*,#30946,.T.);
#44042=ORIENTED_EDGE('',*,*,#30942,.F.);
#44043=ORIENTED_EDGE('',*,*,#30947,.F.);
#44044=ORIENTED_EDGE('',*,*,#30948,.T.);
#44045=ORIENTED_EDGE('',*,*,#30949,.T.);
#44046=ORIENTED_EDGE('',*,*,#30945,.F.);
#44047=ORIENTED_EDGE('',*,*,#30950,.F.);
#44048=ORIENTED_EDGE('',*,*,#30951,.T.);
#44049=ORIENTED_EDGE('',*,*,#30952,.T.);
#44050=ORIENTED_EDGE('',*,*,#30948,.F.);
#44051=ORIENTED_EDGE('',*,*,#30953,.F.);
#44052=ORIENTED_EDGE('',*,*,#30954,.T.);
#44053=ORIENTED_EDGE('',*,*,#30955,.T.);
#44054=ORIENTED_EDGE('',*,*,#30951,.F.);
#44055=ORIENTED_EDGE('',*,*,#30956,.F.);
#44056=ORIENTED_EDGE('',*,*,#30957,.T.);
#44057=ORIENTED_EDGE('',*,*,#30958,.T.);
#44058=ORIENTED_EDGE('',*,*,#30954,.F.);
#44059=ORIENTED_EDGE('',*,*,#30959,.F.);
#44060=ORIENTED_EDGE('',*,*,#30960,.T.);
#44061=ORIENTED_EDGE('',*,*,#30961,.T.);
#44062=ORIENTED_EDGE('',*,*,#30957,.F.);
#44063=ORIENTED_EDGE('',*,*,#30962,.F.);
#44064=ORIENTED_EDGE('',*,*,#30963,.T.);
#44065=ORIENTED_EDGE('',*,*,#30964,.T.);
#44066=ORIENTED_EDGE('',*,*,#30960,.F.);
#44067=ORIENTED_EDGE('',*,*,#30965,.F.);
#44068=ORIENTED_EDGE('',*,*,#30966,.T.);
#44069=ORIENTED_EDGE('',*,*,#30967,.T.);
#44070=ORIENTED_EDGE('',*,*,#30963,.F.);
#44071=ORIENTED_EDGE('',*,*,#30968,.F.);
#44072=ORIENTED_EDGE('',*,*,#30916,.T.);
#44073=ORIENTED_EDGE('',*,*,#30969,.T.);
#44074=ORIENTED_EDGE('',*,*,#30966,.F.);
#44075=ORIENTED_EDGE('',*,*,#30969,.F.);
#44076=ORIENTED_EDGE('',*,*,#30915,.F.);
#44077=ORIENTED_EDGE('',*,*,#30919,.F.);
#44078=ORIENTED_EDGE('',*,*,#30922,.F.);
#44079=ORIENTED_EDGE('',*,*,#30925,.F.);
#44080=ORIENTED_EDGE('',*,*,#30928,.F.);
#44081=ORIENTED_EDGE('',*,*,#30931,.F.);
#44082=ORIENTED_EDGE('',*,*,#30934,.F.);
#44083=ORIENTED_EDGE('',*,*,#30937,.F.);
#44084=ORIENTED_EDGE('',*,*,#30940,.F.);
#44085=ORIENTED_EDGE('',*,*,#30943,.F.);
#44086=ORIENTED_EDGE('',*,*,#30946,.F.);
#44087=ORIENTED_EDGE('',*,*,#30949,.F.);
#44088=ORIENTED_EDGE('',*,*,#30952,.F.);
#44089=ORIENTED_EDGE('',*,*,#30955,.F.);
#44090=ORIENTED_EDGE('',*,*,#30958,.F.);
#44091=ORIENTED_EDGE('',*,*,#30961,.F.);
#44092=ORIENTED_EDGE('',*,*,#30964,.F.);
#44093=ORIENTED_EDGE('',*,*,#30967,.F.);
#44094=ORIENTED_EDGE('',*,*,#30970,.F.);
#44095=ORIENTED_EDGE('',*,*,#30971,.T.);
#44096=ORIENTED_EDGE('',*,*,#30972,.T.);
#44097=ORIENTED_EDGE('',*,*,#30973,.F.);
#44098=ORIENTED_EDGE('',*,*,#30974,.F.);
#44099=ORIENTED_EDGE('',*,*,#30975,.T.);
#44100=ORIENTED_EDGE('',*,*,#30976,.T.);
#44101=ORIENTED_EDGE('',*,*,#30971,.F.);
#44102=ORIENTED_EDGE('',*,*,#30977,.F.);
#44103=ORIENTED_EDGE('',*,*,#30978,.T.);
#44104=ORIENTED_EDGE('',*,*,#30979,.T.);
#44105=ORIENTED_EDGE('',*,*,#30975,.F.);
#44106=ORIENTED_EDGE('',*,*,#30980,.F.);
#44107=ORIENTED_EDGE('',*,*,#30981,.T.);
#44108=ORIENTED_EDGE('',*,*,#30982,.T.);
#44109=ORIENTED_EDGE('',*,*,#30978,.F.);
#44110=ORIENTED_EDGE('',*,*,#30983,.F.);
#44111=ORIENTED_EDGE('',*,*,#30984,.T.);
#44112=ORIENTED_EDGE('',*,*,#30985,.T.);
#44113=ORIENTED_EDGE('',*,*,#30981,.F.);
#44114=ORIENTED_EDGE('',*,*,#30986,.F.);
#44115=ORIENTED_EDGE('',*,*,#30987,.T.);
#44116=ORIENTED_EDGE('',*,*,#30988,.T.);
#44117=ORIENTED_EDGE('',*,*,#30984,.F.);
#44118=ORIENTED_EDGE('',*,*,#30989,.F.);
#44119=ORIENTED_EDGE('',*,*,#30990,.T.);
#44120=ORIENTED_EDGE('',*,*,#30991,.T.);
#44121=ORIENTED_EDGE('',*,*,#30987,.F.);
#44122=ORIENTED_EDGE('',*,*,#30992,.F.);
#44123=ORIENTED_EDGE('',*,*,#30973,.T.);
#44124=ORIENTED_EDGE('',*,*,#30993,.T.);
#44125=ORIENTED_EDGE('',*,*,#30990,.F.);
#44126=ORIENTED_EDGE('',*,*,#30993,.F.);
#44127=ORIENTED_EDGE('',*,*,#30972,.F.);
#44128=ORIENTED_EDGE('',*,*,#30976,.F.);
#44129=ORIENTED_EDGE('',*,*,#30979,.F.);
#44130=ORIENTED_EDGE('',*,*,#30982,.F.);
#44131=ORIENTED_EDGE('',*,*,#30985,.F.);
#44132=ORIENTED_EDGE('',*,*,#30988,.F.);
#44133=ORIENTED_EDGE('',*,*,#30991,.F.);
#44134=ORIENTED_EDGE('',*,*,#30994,.F.);
#44135=ORIENTED_EDGE('',*,*,#30995,.T.);
#44136=ORIENTED_EDGE('',*,*,#30996,.T.);
#44137=ORIENTED_EDGE('',*,*,#30997,.F.);
#44138=ORIENTED_EDGE('',*,*,#30998,.F.);
#44139=ORIENTED_EDGE('',*,*,#30999,.T.);
#44140=ORIENTED_EDGE('',*,*,#31000,.T.);
#44141=ORIENTED_EDGE('',*,*,#30995,.F.);
#44142=ORIENTED_EDGE('',*,*,#31001,.F.);
#44143=ORIENTED_EDGE('',*,*,#31002,.T.);
#44144=ORIENTED_EDGE('',*,*,#31003,.T.);
#44145=ORIENTED_EDGE('',*,*,#30999,.F.);
#44146=ORIENTED_EDGE('',*,*,#31004,.F.);
#44147=ORIENTED_EDGE('',*,*,#31005,.T.);
#44148=ORIENTED_EDGE('',*,*,#31006,.T.);
#44149=ORIENTED_EDGE('',*,*,#31002,.F.);
#44150=ORIENTED_EDGE('',*,*,#31007,.F.);
#44151=ORIENTED_EDGE('',*,*,#31008,.T.);
#44152=ORIENTED_EDGE('',*,*,#31009,.T.);
#44153=ORIENTED_EDGE('',*,*,#31005,.F.);
#44154=ORIENTED_EDGE('',*,*,#31010,.F.);
#44155=ORIENTED_EDGE('',*,*,#31011,.T.);
#44156=ORIENTED_EDGE('',*,*,#31012,.T.);
#44157=ORIENTED_EDGE('',*,*,#31008,.F.);
#44158=ORIENTED_EDGE('',*,*,#31013,.F.);
#44159=ORIENTED_EDGE('',*,*,#31014,.T.);
#44160=ORIENTED_EDGE('',*,*,#31015,.T.);
#44161=ORIENTED_EDGE('',*,*,#31011,.F.);
#44162=ORIENTED_EDGE('',*,*,#31016,.F.);
#44163=ORIENTED_EDGE('',*,*,#31017,.T.);
#44164=ORIENTED_EDGE('',*,*,#31018,.T.);
#44165=ORIENTED_EDGE('',*,*,#31014,.F.);
#44166=ORIENTED_EDGE('',*,*,#31019,.F.);
#44167=ORIENTED_EDGE('',*,*,#30997,.T.);
#44168=ORIENTED_EDGE('',*,*,#31020,.T.);
#44169=ORIENTED_EDGE('',*,*,#31017,.F.);
#44170=ORIENTED_EDGE('',*,*,#31020,.F.);
#44171=ORIENTED_EDGE('',*,*,#30996,.F.);
#44172=ORIENTED_EDGE('',*,*,#31000,.F.);
#44173=ORIENTED_EDGE('',*,*,#31003,.F.);
#44174=ORIENTED_EDGE('',*,*,#31006,.F.);
#44175=ORIENTED_EDGE('',*,*,#31009,.F.);
#44176=ORIENTED_EDGE('',*,*,#31012,.F.);
#44177=ORIENTED_EDGE('',*,*,#31015,.F.);
#44178=ORIENTED_EDGE('',*,*,#31018,.F.);
#44179=ORIENTED_EDGE('',*,*,#31021,.F.);
#44180=ORIENTED_EDGE('',*,*,#31022,.T.);
#44181=ORIENTED_EDGE('',*,*,#31023,.T.);
#44182=ORIENTED_EDGE('',*,*,#31024,.F.);
#44183=ORIENTED_EDGE('',*,*,#31025,.F.);
#44184=ORIENTED_EDGE('',*,*,#31026,.T.);
#44185=ORIENTED_EDGE('',*,*,#31027,.T.);
#44186=ORIENTED_EDGE('',*,*,#31022,.F.);
#44187=ORIENTED_EDGE('',*,*,#31028,.F.);
#44188=ORIENTED_EDGE('',*,*,#31029,.T.);
#44189=ORIENTED_EDGE('',*,*,#31030,.T.);
#44190=ORIENTED_EDGE('',*,*,#31026,.F.);
#44191=ORIENTED_EDGE('',*,*,#31031,.F.);
#44192=ORIENTED_EDGE('',*,*,#31032,.T.);
#44193=ORIENTED_EDGE('',*,*,#31033,.T.);
#44194=ORIENTED_EDGE('',*,*,#31029,.F.);
#44195=ORIENTED_EDGE('',*,*,#31034,.F.);
#44196=ORIENTED_EDGE('',*,*,#31035,.T.);
#44197=ORIENTED_EDGE('',*,*,#31036,.T.);
#44198=ORIENTED_EDGE('',*,*,#31032,.F.);
#44199=ORIENTED_EDGE('',*,*,#31037,.F.);
#44200=ORIENTED_EDGE('',*,*,#31038,.T.);
#44201=ORIENTED_EDGE('',*,*,#31039,.T.);
#44202=ORIENTED_EDGE('',*,*,#31035,.F.);
#44203=ORIENTED_EDGE('',*,*,#31040,.F.);
#44204=ORIENTED_EDGE('',*,*,#31041,.T.);
#44205=ORIENTED_EDGE('',*,*,#31042,.T.);
#44206=ORIENTED_EDGE('',*,*,#31038,.F.);
#44207=ORIENTED_EDGE('',*,*,#31043,.F.);
#44208=ORIENTED_EDGE('',*,*,#31044,.T.);
#44209=ORIENTED_EDGE('',*,*,#31045,.T.);
#44210=ORIENTED_EDGE('',*,*,#31041,.F.);
#44211=ORIENTED_EDGE('',*,*,#31046,.F.);
#44212=ORIENTED_EDGE('',*,*,#31047,.T.);
#44213=ORIENTED_EDGE('',*,*,#31048,.T.);
#44214=ORIENTED_EDGE('',*,*,#31044,.F.);
#44215=ORIENTED_EDGE('',*,*,#31049,.F.);
#44216=ORIENTED_EDGE('',*,*,#31050,.T.);
#44217=ORIENTED_EDGE('',*,*,#31051,.T.);
#44218=ORIENTED_EDGE('',*,*,#31047,.F.);
#44219=ORIENTED_EDGE('',*,*,#31052,.F.);
#44220=ORIENTED_EDGE('',*,*,#31053,.T.);
#44221=ORIENTED_EDGE('',*,*,#31054,.T.);
#44222=ORIENTED_EDGE('',*,*,#31050,.F.);
#44223=ORIENTED_EDGE('',*,*,#31055,.F.);
#44224=ORIENTED_EDGE('',*,*,#31024,.T.);
#44225=ORIENTED_EDGE('',*,*,#31056,.T.);
#44226=ORIENTED_EDGE('',*,*,#31053,.F.);
#44227=ORIENTED_EDGE('',*,*,#31056,.F.);
#44228=ORIENTED_EDGE('',*,*,#31023,.F.);
#44229=ORIENTED_EDGE('',*,*,#31027,.F.);
#44230=ORIENTED_EDGE('',*,*,#31030,.F.);
#44231=ORIENTED_EDGE('',*,*,#31033,.F.);
#44232=ORIENTED_EDGE('',*,*,#31036,.F.);
#44233=ORIENTED_EDGE('',*,*,#31039,.F.);
#44234=ORIENTED_EDGE('',*,*,#31042,.F.);
#44235=ORIENTED_EDGE('',*,*,#31045,.F.);
#44236=ORIENTED_EDGE('',*,*,#31048,.F.);
#44237=ORIENTED_EDGE('',*,*,#31051,.F.);
#44238=ORIENTED_EDGE('',*,*,#31054,.F.);
#44239=ORIENTED_EDGE('',*,*,#31057,.F.);
#44240=ORIENTED_EDGE('',*,*,#31058,.T.);
#44241=ORIENTED_EDGE('',*,*,#31059,.T.);
#44242=ORIENTED_EDGE('',*,*,#31060,.F.);
#44243=ORIENTED_EDGE('',*,*,#31061,.F.);
#44244=ORIENTED_EDGE('',*,*,#31062,.T.);
#44245=ORIENTED_EDGE('',*,*,#31063,.T.);
#44246=ORIENTED_EDGE('',*,*,#31058,.F.);
#44247=ORIENTED_EDGE('',*,*,#31064,.F.);
#44248=ORIENTED_EDGE('',*,*,#31065,.T.);
#44249=ORIENTED_EDGE('',*,*,#31066,.T.);
#44250=ORIENTED_EDGE('',*,*,#31062,.F.);
#44251=ORIENTED_EDGE('',*,*,#31067,.F.);
#44252=ORIENTED_EDGE('',*,*,#31068,.T.);
#44253=ORIENTED_EDGE('',*,*,#31069,.T.);
#44254=ORIENTED_EDGE('',*,*,#31065,.F.);
#44255=ORIENTED_EDGE('',*,*,#31070,.F.);
#44256=ORIENTED_EDGE('',*,*,#31071,.T.);
#44257=ORIENTED_EDGE('',*,*,#31072,.T.);
#44258=ORIENTED_EDGE('',*,*,#31068,.F.);
#44259=ORIENTED_EDGE('',*,*,#31073,.F.);
#44260=ORIENTED_EDGE('',*,*,#31074,.T.);
#44261=ORIENTED_EDGE('',*,*,#31075,.T.);
#44262=ORIENTED_EDGE('',*,*,#31071,.F.);
#44263=ORIENTED_EDGE('',*,*,#31076,.F.);
#44264=ORIENTED_EDGE('',*,*,#31077,.T.);
#44265=ORIENTED_EDGE('',*,*,#31078,.T.);
#44266=ORIENTED_EDGE('',*,*,#31074,.F.);
#44267=ORIENTED_EDGE('',*,*,#31079,.F.);
#44268=ORIENTED_EDGE('',*,*,#31080,.T.);
#44269=ORIENTED_EDGE('',*,*,#31081,.T.);
#44270=ORIENTED_EDGE('',*,*,#31077,.F.);
#44271=ORIENTED_EDGE('',*,*,#31082,.F.);
#44272=ORIENTED_EDGE('',*,*,#31060,.T.);
#44273=ORIENTED_EDGE('',*,*,#31083,.T.);
#44274=ORIENTED_EDGE('',*,*,#31080,.F.);
#44275=ORIENTED_EDGE('',*,*,#31083,.F.);
#44276=ORIENTED_EDGE('',*,*,#31059,.F.);
#44277=ORIENTED_EDGE('',*,*,#31063,.F.);
#44278=ORIENTED_EDGE('',*,*,#31066,.F.);
#44279=ORIENTED_EDGE('',*,*,#31069,.F.);
#44280=ORIENTED_EDGE('',*,*,#31072,.F.);
#44281=ORIENTED_EDGE('',*,*,#31075,.F.);
#44282=ORIENTED_EDGE('',*,*,#31078,.F.);
#44283=ORIENTED_EDGE('',*,*,#31081,.F.);
#44284=ORIENTED_EDGE('',*,*,#31084,.F.);
#44285=ORIENTED_EDGE('',*,*,#31085,.T.);
#44286=ORIENTED_EDGE('',*,*,#31086,.T.);
#44287=ORIENTED_EDGE('',*,*,#31087,.F.);
#44288=ORIENTED_EDGE('',*,*,#31088,.F.);
#44289=ORIENTED_EDGE('',*,*,#31089,.T.);
#44290=ORIENTED_EDGE('',*,*,#31090,.T.);
#44291=ORIENTED_EDGE('',*,*,#31085,.F.);
#44292=ORIENTED_EDGE('',*,*,#31091,.F.);
#44293=ORIENTED_EDGE('',*,*,#31092,.T.);
#44294=ORIENTED_EDGE('',*,*,#31093,.T.);
#44295=ORIENTED_EDGE('',*,*,#31089,.F.);
#44296=ORIENTED_EDGE('',*,*,#31094,.F.);
#44297=ORIENTED_EDGE('',*,*,#31087,.T.);
#44298=ORIENTED_EDGE('',*,*,#31095,.T.);
#44299=ORIENTED_EDGE('',*,*,#31092,.F.);
#44300=ORIENTED_EDGE('',*,*,#31095,.F.);
#44301=ORIENTED_EDGE('',*,*,#31086,.F.);
#44302=ORIENTED_EDGE('',*,*,#31090,.F.);
#44303=ORIENTED_EDGE('',*,*,#31093,.F.);
#44304=ORIENTED_EDGE('',*,*,#31096,.F.);
#44305=ORIENTED_EDGE('',*,*,#31097,.T.);
#44306=ORIENTED_EDGE('',*,*,#31098,.T.);
#44307=ORIENTED_EDGE('',*,*,#31099,.F.);
#44308=ORIENTED_EDGE('',*,*,#31100,.F.);
#44309=ORIENTED_EDGE('',*,*,#31101,.T.);
#44310=ORIENTED_EDGE('',*,*,#31102,.T.);
#44311=ORIENTED_EDGE('',*,*,#31097,.F.);
#44312=ORIENTED_EDGE('',*,*,#31103,.F.);
#44313=ORIENTED_EDGE('',*,*,#31104,.T.);
#44314=ORIENTED_EDGE('',*,*,#31105,.T.);
#44315=ORIENTED_EDGE('',*,*,#31101,.F.);
#44316=ORIENTED_EDGE('',*,*,#31106,.F.);
#44317=ORIENTED_EDGE('',*,*,#31107,.T.);
#44318=ORIENTED_EDGE('',*,*,#31108,.T.);
#44319=ORIENTED_EDGE('',*,*,#31104,.F.);
#44320=ORIENTED_EDGE('',*,*,#31109,.F.);
#44321=ORIENTED_EDGE('',*,*,#31110,.T.);
#44322=ORIENTED_EDGE('',*,*,#31111,.T.);
#44323=ORIENTED_EDGE('',*,*,#31107,.F.);
#44324=ORIENTED_EDGE('',*,*,#31112,.F.);
#44325=ORIENTED_EDGE('',*,*,#31113,.T.);
#44326=ORIENTED_EDGE('',*,*,#31114,.T.);
#44327=ORIENTED_EDGE('',*,*,#31110,.F.);
#44328=ORIENTED_EDGE('',*,*,#31115,.F.);
#44329=ORIENTED_EDGE('',*,*,#31116,.T.);
#44330=ORIENTED_EDGE('',*,*,#31117,.T.);
#44331=ORIENTED_EDGE('',*,*,#31113,.F.);
#44332=ORIENTED_EDGE('',*,*,#31118,.F.);
#44333=ORIENTED_EDGE('',*,*,#31119,.T.);
#44334=ORIENTED_EDGE('',*,*,#31120,.T.);
#44335=ORIENTED_EDGE('',*,*,#31116,.F.);
#44336=ORIENTED_EDGE('',*,*,#31121,.F.);
#44337=ORIENTED_EDGE('',*,*,#31122,.T.);
#44338=ORIENTED_EDGE('',*,*,#31123,.T.);
#44339=ORIENTED_EDGE('',*,*,#31119,.F.);
#44340=ORIENTED_EDGE('',*,*,#31124,.F.);
#44341=ORIENTED_EDGE('',*,*,#31125,.T.);
#44342=ORIENTED_EDGE('',*,*,#31126,.T.);
#44343=ORIENTED_EDGE('',*,*,#31122,.F.);
#44344=ORIENTED_EDGE('',*,*,#31127,.F.);
#44345=ORIENTED_EDGE('',*,*,#31128,.T.);
#44346=ORIENTED_EDGE('',*,*,#31129,.T.);
#44347=ORIENTED_EDGE('',*,*,#31125,.F.);
#44348=ORIENTED_EDGE('',*,*,#31130,.F.);
#44349=ORIENTED_EDGE('',*,*,#31131,.T.);
#44350=ORIENTED_EDGE('',*,*,#31132,.T.);
#44351=ORIENTED_EDGE('',*,*,#31128,.F.);
#44352=ORIENTED_EDGE('',*,*,#31133,.F.);
#44353=ORIENTED_EDGE('',*,*,#31134,.T.);
#44354=ORIENTED_EDGE('',*,*,#31135,.T.);
#44355=ORIENTED_EDGE('',*,*,#31131,.F.);
#44356=ORIENTED_EDGE('',*,*,#31136,.F.);
#44357=ORIENTED_EDGE('',*,*,#31137,.T.);
#44358=ORIENTED_EDGE('',*,*,#31138,.T.);
#44359=ORIENTED_EDGE('',*,*,#31134,.F.);
#44360=ORIENTED_EDGE('',*,*,#31139,.F.);
#44361=ORIENTED_EDGE('',*,*,#31140,.T.);
#44362=ORIENTED_EDGE('',*,*,#31141,.T.);
#44363=ORIENTED_EDGE('',*,*,#31137,.F.);
#44364=ORIENTED_EDGE('',*,*,#31142,.F.);
#44365=ORIENTED_EDGE('',*,*,#31143,.T.);
#44366=ORIENTED_EDGE('',*,*,#31144,.T.);
#44367=ORIENTED_EDGE('',*,*,#31140,.F.);
#44368=ORIENTED_EDGE('',*,*,#31145,.F.);
#44369=ORIENTED_EDGE('',*,*,#31146,.T.);
#44370=ORIENTED_EDGE('',*,*,#31147,.T.);
#44371=ORIENTED_EDGE('',*,*,#31143,.F.);
#44372=ORIENTED_EDGE('',*,*,#31148,.F.);
#44373=ORIENTED_EDGE('',*,*,#31149,.T.);
#44374=ORIENTED_EDGE('',*,*,#31150,.T.);
#44375=ORIENTED_EDGE('',*,*,#31146,.F.);
#44376=ORIENTED_EDGE('',*,*,#31151,.F.);
#44377=ORIENTED_EDGE('',*,*,#31152,.T.);
#44378=ORIENTED_EDGE('',*,*,#31153,.T.);
#44379=ORIENTED_EDGE('',*,*,#31149,.F.);
#44380=ORIENTED_EDGE('',*,*,#31154,.F.);
#44381=ORIENTED_EDGE('',*,*,#31155,.T.);
#44382=ORIENTED_EDGE('',*,*,#31156,.T.);
#44383=ORIENTED_EDGE('',*,*,#31152,.F.);
#44384=ORIENTED_EDGE('',*,*,#31157,.F.);
#44385=ORIENTED_EDGE('',*,*,#31158,.T.);
#44386=ORIENTED_EDGE('',*,*,#31159,.T.);
#44387=ORIENTED_EDGE('',*,*,#31155,.F.);
#44388=ORIENTED_EDGE('',*,*,#31160,.F.);
#44389=ORIENTED_EDGE('',*,*,#31099,.T.);
#44390=ORIENTED_EDGE('',*,*,#31161,.T.);
#44391=ORIENTED_EDGE('',*,*,#31158,.F.);
#44392=ORIENTED_EDGE('',*,*,#31161,.F.);
#44393=ORIENTED_EDGE('',*,*,#31098,.F.);
#44394=ORIENTED_EDGE('',*,*,#31102,.F.);
#44395=ORIENTED_EDGE('',*,*,#31105,.F.);
#44396=ORIENTED_EDGE('',*,*,#31108,.F.);
#44397=ORIENTED_EDGE('',*,*,#31111,.F.);
#44398=ORIENTED_EDGE('',*,*,#31114,.F.);
#44399=ORIENTED_EDGE('',*,*,#31117,.F.);
#44400=ORIENTED_EDGE('',*,*,#31120,.F.);
#44401=ORIENTED_EDGE('',*,*,#31123,.F.);
#44402=ORIENTED_EDGE('',*,*,#31126,.F.);
#44403=ORIENTED_EDGE('',*,*,#31129,.F.);
#44404=ORIENTED_EDGE('',*,*,#31132,.F.);
#44405=ORIENTED_EDGE('',*,*,#31135,.F.);
#44406=ORIENTED_EDGE('',*,*,#31138,.F.);
#44407=ORIENTED_EDGE('',*,*,#31141,.F.);
#44408=ORIENTED_EDGE('',*,*,#31144,.F.);
#44409=ORIENTED_EDGE('',*,*,#31147,.F.);
#44410=ORIENTED_EDGE('',*,*,#31150,.F.);
#44411=ORIENTED_EDGE('',*,*,#31153,.F.);
#44412=ORIENTED_EDGE('',*,*,#31156,.F.);
#44413=ORIENTED_EDGE('',*,*,#31159,.F.);
#44414=ORIENTED_EDGE('',*,*,#31162,.F.);
#44415=ORIENTED_EDGE('',*,*,#31163,.T.);
#44416=ORIENTED_EDGE('',*,*,#31164,.T.);
#44417=ORIENTED_EDGE('',*,*,#31165,.F.);
#44418=ORIENTED_EDGE('',*,*,#31166,.F.);
#44419=ORIENTED_EDGE('',*,*,#31167,.T.);
#44420=ORIENTED_EDGE('',*,*,#31168,.T.);
#44421=ORIENTED_EDGE('',*,*,#31163,.F.);
#44422=ORIENTED_EDGE('',*,*,#31169,.F.);
#44423=ORIENTED_EDGE('',*,*,#31170,.T.);
#44424=ORIENTED_EDGE('',*,*,#31171,.T.);
#44425=ORIENTED_EDGE('',*,*,#31167,.F.);
#44426=ORIENTED_EDGE('',*,*,#31172,.F.);
#44427=ORIENTED_EDGE('',*,*,#31173,.T.);
#44428=ORIENTED_EDGE('',*,*,#31174,.T.);
#44429=ORIENTED_EDGE('',*,*,#31170,.F.);
#44430=ORIENTED_EDGE('',*,*,#31175,.F.);
#44431=ORIENTED_EDGE('',*,*,#31176,.T.);
#44432=ORIENTED_EDGE('',*,*,#31177,.T.);
#44433=ORIENTED_EDGE('',*,*,#31173,.F.);
#44434=ORIENTED_EDGE('',*,*,#31178,.F.);
#44435=ORIENTED_EDGE('',*,*,#31179,.T.);
#44436=ORIENTED_EDGE('',*,*,#31180,.T.);
#44437=ORIENTED_EDGE('',*,*,#31176,.F.);
#44438=ORIENTED_EDGE('',*,*,#31181,.F.);
#44439=ORIENTED_EDGE('',*,*,#31182,.T.);
#44440=ORIENTED_EDGE('',*,*,#31183,.T.);
#44441=ORIENTED_EDGE('',*,*,#31179,.F.);
#44442=ORIENTED_EDGE('',*,*,#31184,.F.);
#44443=ORIENTED_EDGE('',*,*,#31185,.T.);
#44444=ORIENTED_EDGE('',*,*,#31186,.T.);
#44445=ORIENTED_EDGE('',*,*,#31182,.F.);
#44446=ORIENTED_EDGE('',*,*,#31187,.F.);
#44447=ORIENTED_EDGE('',*,*,#31188,.T.);
#44448=ORIENTED_EDGE('',*,*,#31189,.T.);
#44449=ORIENTED_EDGE('',*,*,#31185,.F.);
#44450=ORIENTED_EDGE('',*,*,#31190,.F.);
#44451=ORIENTED_EDGE('',*,*,#31191,.T.);
#44452=ORIENTED_EDGE('',*,*,#31192,.T.);
#44453=ORIENTED_EDGE('',*,*,#31188,.F.);
#44454=ORIENTED_EDGE('',*,*,#31193,.F.);
#44455=ORIENTED_EDGE('',*,*,#31165,.T.);
#44456=ORIENTED_EDGE('',*,*,#31194,.T.);
#44457=ORIENTED_EDGE('',*,*,#31191,.F.);
#44458=ORIENTED_EDGE('',*,*,#31194,.F.);
#44459=ORIENTED_EDGE('',*,*,#31164,.F.);
#44460=ORIENTED_EDGE('',*,*,#31168,.F.);
#44461=ORIENTED_EDGE('',*,*,#31171,.F.);
#44462=ORIENTED_EDGE('',*,*,#31174,.F.);
#44463=ORIENTED_EDGE('',*,*,#31177,.F.);
#44464=ORIENTED_EDGE('',*,*,#31180,.F.);
#44465=ORIENTED_EDGE('',*,*,#31183,.F.);
#44466=ORIENTED_EDGE('',*,*,#31186,.F.);
#44467=ORIENTED_EDGE('',*,*,#31189,.F.);
#44468=ORIENTED_EDGE('',*,*,#31192,.F.);
#44469=ORIENTED_EDGE('',*,*,#31195,.F.);
#44470=ORIENTED_EDGE('',*,*,#31196,.T.);
#44471=ORIENTED_EDGE('',*,*,#31197,.T.);
#44472=ORIENTED_EDGE('',*,*,#31198,.F.);
#44473=ORIENTED_EDGE('',*,*,#31199,.F.);
#44474=ORIENTED_EDGE('',*,*,#31200,.T.);
#44475=ORIENTED_EDGE('',*,*,#31201,.T.);
#44476=ORIENTED_EDGE('',*,*,#31196,.F.);
#44477=ORIENTED_EDGE('',*,*,#31202,.F.);
#44478=ORIENTED_EDGE('',*,*,#31203,.T.);
#44479=ORIENTED_EDGE('',*,*,#31204,.T.);
#44480=ORIENTED_EDGE('',*,*,#31200,.F.);
#44481=ORIENTED_EDGE('',*,*,#31205,.F.);
#44482=ORIENTED_EDGE('',*,*,#31206,.T.);
#44483=ORIENTED_EDGE('',*,*,#31207,.T.);
#44484=ORIENTED_EDGE('',*,*,#31203,.F.);
#44485=ORIENTED_EDGE('',*,*,#31208,.F.);
#44486=ORIENTED_EDGE('',*,*,#31209,.T.);
#44487=ORIENTED_EDGE('',*,*,#31210,.T.);
#44488=ORIENTED_EDGE('',*,*,#31206,.F.);
#44489=ORIENTED_EDGE('',*,*,#31211,.F.);
#44490=ORIENTED_EDGE('',*,*,#31212,.T.);
#44491=ORIENTED_EDGE('',*,*,#31213,.T.);
#44492=ORIENTED_EDGE('',*,*,#31209,.F.);
#44493=ORIENTED_EDGE('',*,*,#31214,.F.);
#44494=ORIENTED_EDGE('',*,*,#31215,.T.);
#44495=ORIENTED_EDGE('',*,*,#31216,.T.);
#44496=ORIENTED_EDGE('',*,*,#31212,.F.);
#44497=ORIENTED_EDGE('',*,*,#31217,.F.);
#44498=ORIENTED_EDGE('',*,*,#31218,.T.);
#44499=ORIENTED_EDGE('',*,*,#31219,.T.);
#44500=ORIENTED_EDGE('',*,*,#31215,.F.);
#44501=ORIENTED_EDGE('',*,*,#31220,.F.);
#44502=ORIENTED_EDGE('',*,*,#31221,.T.);
#44503=ORIENTED_EDGE('',*,*,#31222,.T.);
#44504=ORIENTED_EDGE('',*,*,#31218,.F.);
#44505=ORIENTED_EDGE('',*,*,#31223,.F.);
#44506=ORIENTED_EDGE('',*,*,#31224,.T.);
#44507=ORIENTED_EDGE('',*,*,#31225,.T.);
#44508=ORIENTED_EDGE('',*,*,#31221,.F.);
#44509=ORIENTED_EDGE('',*,*,#31226,.F.);
#44510=ORIENTED_EDGE('',*,*,#31227,.T.);
#44511=ORIENTED_EDGE('',*,*,#31228,.T.);
#44512=ORIENTED_EDGE('',*,*,#31224,.F.);
#44513=ORIENTED_EDGE('',*,*,#31229,.F.);
#44514=ORIENTED_EDGE('',*,*,#31230,.T.);
#44515=ORIENTED_EDGE('',*,*,#31231,.T.);
#44516=ORIENTED_EDGE('',*,*,#31227,.F.);
#44517=ORIENTED_EDGE('',*,*,#31232,.F.);
#44518=ORIENTED_EDGE('',*,*,#31233,.T.);
#44519=ORIENTED_EDGE('',*,*,#31234,.T.);
#44520=ORIENTED_EDGE('',*,*,#31230,.F.);
#44521=ORIENTED_EDGE('',*,*,#31235,.F.);
#44522=ORIENTED_EDGE('',*,*,#31236,.T.);
#44523=ORIENTED_EDGE('',*,*,#31237,.T.);
#44524=ORIENTED_EDGE('',*,*,#31233,.F.);
#44525=ORIENTED_EDGE('',*,*,#31238,.F.);
#44526=ORIENTED_EDGE('',*,*,#31198,.T.);
#44527=ORIENTED_EDGE('',*,*,#31239,.T.);
#44528=ORIENTED_EDGE('',*,*,#31236,.F.);
#44529=ORIENTED_EDGE('',*,*,#31239,.F.);
#44530=ORIENTED_EDGE('',*,*,#31197,.F.);
#44531=ORIENTED_EDGE('',*,*,#31201,.F.);
#44532=ORIENTED_EDGE('',*,*,#31204,.F.);
#44533=ORIENTED_EDGE('',*,*,#31207,.F.);
#44534=ORIENTED_EDGE('',*,*,#31210,.F.);
#44535=ORIENTED_EDGE('',*,*,#31213,.F.);
#44536=ORIENTED_EDGE('',*,*,#31216,.F.);
#44537=ORIENTED_EDGE('',*,*,#31219,.F.);
#44538=ORIENTED_EDGE('',*,*,#31222,.F.);
#44539=ORIENTED_EDGE('',*,*,#31225,.F.);
#44540=ORIENTED_EDGE('',*,*,#31228,.F.);
#44541=ORIENTED_EDGE('',*,*,#31231,.F.);
#44542=ORIENTED_EDGE('',*,*,#31234,.F.);
#44543=ORIENTED_EDGE('',*,*,#31237,.F.);
#44544=ORIENTED_EDGE('',*,*,#31240,.F.);
#44545=ORIENTED_EDGE('',*,*,#31241,.T.);
#44546=ORIENTED_EDGE('',*,*,#31242,.T.);
#44547=ORIENTED_EDGE('',*,*,#31243,.F.);
#44548=ORIENTED_EDGE('',*,*,#31244,.F.);
#44549=ORIENTED_EDGE('',*,*,#31245,.T.);
#44550=ORIENTED_EDGE('',*,*,#31246,.T.);
#44551=ORIENTED_EDGE('',*,*,#31241,.F.);
#44552=ORIENTED_EDGE('',*,*,#31247,.F.);
#44553=ORIENTED_EDGE('',*,*,#31248,.T.);
#44554=ORIENTED_EDGE('',*,*,#31249,.T.);
#44555=ORIENTED_EDGE('',*,*,#31245,.F.);
#44556=ORIENTED_EDGE('',*,*,#31250,.F.);
#44557=ORIENTED_EDGE('',*,*,#31251,.T.);
#44558=ORIENTED_EDGE('',*,*,#31252,.T.);
#44559=ORIENTED_EDGE('',*,*,#31248,.F.);
#44560=ORIENTED_EDGE('',*,*,#31253,.F.);
#44561=ORIENTED_EDGE('',*,*,#31254,.T.);
#44562=ORIENTED_EDGE('',*,*,#31255,.T.);
#44563=ORIENTED_EDGE('',*,*,#31251,.F.);
#44564=ORIENTED_EDGE('',*,*,#31256,.F.);
#44565=ORIENTED_EDGE('',*,*,#31257,.T.);
#44566=ORIENTED_EDGE('',*,*,#31258,.T.);
#44567=ORIENTED_EDGE('',*,*,#31254,.F.);
#44568=ORIENTED_EDGE('',*,*,#31259,.F.);
#44569=ORIENTED_EDGE('',*,*,#31260,.T.);
#44570=ORIENTED_EDGE('',*,*,#31261,.T.);
#44571=ORIENTED_EDGE('',*,*,#31257,.F.);
#44572=ORIENTED_EDGE('',*,*,#31262,.F.);
#44573=ORIENTED_EDGE('',*,*,#31263,.T.);
#44574=ORIENTED_EDGE('',*,*,#31264,.T.);
#44575=ORIENTED_EDGE('',*,*,#31260,.F.);
#44576=ORIENTED_EDGE('',*,*,#31265,.F.);
#44577=ORIENTED_EDGE('',*,*,#31266,.T.);
#44578=ORIENTED_EDGE('',*,*,#31267,.T.);
#44579=ORIENTED_EDGE('',*,*,#31263,.F.);
#44580=ORIENTED_EDGE('',*,*,#31268,.F.);
#44581=ORIENTED_EDGE('',*,*,#31269,.T.);
#44582=ORIENTED_EDGE('',*,*,#31270,.T.);
#44583=ORIENTED_EDGE('',*,*,#31266,.F.);
#44584=ORIENTED_EDGE('',*,*,#31271,.F.);
#44585=ORIENTED_EDGE('',*,*,#31272,.T.);
#44586=ORIENTED_EDGE('',*,*,#31273,.T.);
#44587=ORIENTED_EDGE('',*,*,#31269,.F.);
#44588=ORIENTED_EDGE('',*,*,#31274,.F.);
#44589=ORIENTED_EDGE('',*,*,#31243,.T.);
#44590=ORIENTED_EDGE('',*,*,#31275,.T.);
#44591=ORIENTED_EDGE('',*,*,#31272,.F.);
#44592=ORIENTED_EDGE('',*,*,#31275,.F.);
#44593=ORIENTED_EDGE('',*,*,#31242,.F.);
#44594=ORIENTED_EDGE('',*,*,#31246,.F.);
#44595=ORIENTED_EDGE('',*,*,#31249,.F.);
#44596=ORIENTED_EDGE('',*,*,#31252,.F.);
#44597=ORIENTED_EDGE('',*,*,#31255,.F.);
#44598=ORIENTED_EDGE('',*,*,#31258,.F.);
#44599=ORIENTED_EDGE('',*,*,#31261,.F.);
#44600=ORIENTED_EDGE('',*,*,#31264,.F.);
#44601=ORIENTED_EDGE('',*,*,#31267,.F.);
#44602=ORIENTED_EDGE('',*,*,#31270,.F.);
#44603=ORIENTED_EDGE('',*,*,#31273,.F.);
#44604=ORIENTED_EDGE('',*,*,#31276,.F.);
#44605=ORIENTED_EDGE('',*,*,#31277,.T.);
#44606=ORIENTED_EDGE('',*,*,#31278,.T.);
#44607=ORIENTED_EDGE('',*,*,#31279,.F.);
#44608=ORIENTED_EDGE('',*,*,#31280,.F.);
#44609=ORIENTED_EDGE('',*,*,#31281,.T.);
#44610=ORIENTED_EDGE('',*,*,#31282,.T.);
#44611=ORIENTED_EDGE('',*,*,#31277,.F.);
#44612=ORIENTED_EDGE('',*,*,#31283,.F.);
#44613=ORIENTED_EDGE('',*,*,#31284,.T.);
#44614=ORIENTED_EDGE('',*,*,#31285,.T.);
#44615=ORIENTED_EDGE('',*,*,#31281,.F.);
#44616=ORIENTED_EDGE('',*,*,#31286,.F.);
#44617=ORIENTED_EDGE('',*,*,#31279,.T.);
#44618=ORIENTED_EDGE('',*,*,#31287,.T.);
#44619=ORIENTED_EDGE('',*,*,#31284,.F.);
#44620=ORIENTED_EDGE('',*,*,#31287,.F.);
#44621=ORIENTED_EDGE('',*,*,#31278,.F.);
#44622=ORIENTED_EDGE('',*,*,#31282,.F.);
#44623=ORIENTED_EDGE('',*,*,#31285,.F.);
#44624=ORIENTED_EDGE('',*,*,#31288,.F.);
#44625=ORIENTED_EDGE('',*,*,#31289,.T.);
#44626=ORIENTED_EDGE('',*,*,#31290,.T.);
#44627=ORIENTED_EDGE('',*,*,#31291,.F.);
#44628=ORIENTED_EDGE('',*,*,#31292,.F.);
#44629=ORIENTED_EDGE('',*,*,#31293,.T.);
#44630=ORIENTED_EDGE('',*,*,#31294,.T.);
#44631=ORIENTED_EDGE('',*,*,#31289,.F.);
#44632=ORIENTED_EDGE('',*,*,#31295,.F.);
#44633=ORIENTED_EDGE('',*,*,#31296,.T.);
#44634=ORIENTED_EDGE('',*,*,#31297,.T.);
#44635=ORIENTED_EDGE('',*,*,#31293,.F.);
#44636=ORIENTED_EDGE('',*,*,#31298,.F.);
#44637=ORIENTED_EDGE('',*,*,#31299,.T.);
#44638=ORIENTED_EDGE('',*,*,#31300,.T.);
#44639=ORIENTED_EDGE('',*,*,#31296,.F.);
#44640=ORIENTED_EDGE('',*,*,#31301,.F.);
#44641=ORIENTED_EDGE('',*,*,#31302,.T.);
#44642=ORIENTED_EDGE('',*,*,#31303,.T.);
#44643=ORIENTED_EDGE('',*,*,#31299,.F.);
#44644=ORIENTED_EDGE('',*,*,#31304,.F.);
#44645=ORIENTED_EDGE('',*,*,#31305,.T.);
#44646=ORIENTED_EDGE('',*,*,#31306,.T.);
#44647=ORIENTED_EDGE('',*,*,#31302,.F.);
#44648=ORIENTED_EDGE('',*,*,#31307,.F.);
#44649=ORIENTED_EDGE('',*,*,#31308,.T.);
#44650=ORIENTED_EDGE('',*,*,#31309,.T.);
#44651=ORIENTED_EDGE('',*,*,#31305,.F.);
#44652=ORIENTED_EDGE('',*,*,#31310,.F.);
#44653=ORIENTED_EDGE('',*,*,#31311,.T.);
#44654=ORIENTED_EDGE('',*,*,#31312,.T.);
#44655=ORIENTED_EDGE('',*,*,#31308,.F.);
#44656=ORIENTED_EDGE('',*,*,#31313,.F.);
#44657=ORIENTED_EDGE('',*,*,#31314,.T.);
#44658=ORIENTED_EDGE('',*,*,#31315,.T.);
#44659=ORIENTED_EDGE('',*,*,#31311,.F.);
#44660=ORIENTED_EDGE('',*,*,#31316,.F.);
#44661=ORIENTED_EDGE('',*,*,#31317,.T.);
#44662=ORIENTED_EDGE('',*,*,#31318,.T.);
#44663=ORIENTED_EDGE('',*,*,#31314,.F.);
#44664=ORIENTED_EDGE('',*,*,#31319,.F.);
#44665=ORIENTED_EDGE('',*,*,#31291,.T.);
#44666=ORIENTED_EDGE('',*,*,#31320,.T.);
#44667=ORIENTED_EDGE('',*,*,#31317,.F.);
#44668=ORIENTED_EDGE('',*,*,#31320,.F.);
#44669=ORIENTED_EDGE('',*,*,#31290,.F.);
#44670=ORIENTED_EDGE('',*,*,#31294,.F.);
#44671=ORIENTED_EDGE('',*,*,#31297,.F.);
#44672=ORIENTED_EDGE('',*,*,#31300,.F.);
#44673=ORIENTED_EDGE('',*,*,#31303,.F.);
#44674=ORIENTED_EDGE('',*,*,#31306,.F.);
#44675=ORIENTED_EDGE('',*,*,#31309,.F.);
#44676=ORIENTED_EDGE('',*,*,#31312,.F.);
#44677=ORIENTED_EDGE('',*,*,#31315,.F.);
#44678=ORIENTED_EDGE('',*,*,#31318,.F.);
#44679=ORIENTED_EDGE('',*,*,#31321,.F.);
#44680=ORIENTED_EDGE('',*,*,#31322,.T.);
#44681=ORIENTED_EDGE('',*,*,#31323,.T.);
#44682=ORIENTED_EDGE('',*,*,#31324,.F.);
#44683=ORIENTED_EDGE('',*,*,#31325,.F.);
#44684=ORIENTED_EDGE('',*,*,#31326,.T.);
#44685=ORIENTED_EDGE('',*,*,#31327,.T.);
#44686=ORIENTED_EDGE('',*,*,#31322,.F.);
#44687=ORIENTED_EDGE('',*,*,#31328,.F.);
#44688=ORIENTED_EDGE('',*,*,#31329,.T.);
#44689=ORIENTED_EDGE('',*,*,#31330,.T.);
#44690=ORIENTED_EDGE('',*,*,#31326,.F.);
#44691=ORIENTED_EDGE('',*,*,#31331,.F.);
#44692=ORIENTED_EDGE('',*,*,#31332,.T.);
#44693=ORIENTED_EDGE('',*,*,#31333,.T.);
#44694=ORIENTED_EDGE('',*,*,#31329,.F.);
#44695=ORIENTED_EDGE('',*,*,#31334,.F.);
#44696=ORIENTED_EDGE('',*,*,#31335,.T.);
#44697=ORIENTED_EDGE('',*,*,#31336,.T.);
#44698=ORIENTED_EDGE('',*,*,#31332,.F.);
#44699=ORIENTED_EDGE('',*,*,#31337,.F.);
#44700=ORIENTED_EDGE('',*,*,#31338,.T.);
#44701=ORIENTED_EDGE('',*,*,#31339,.T.);
#44702=ORIENTED_EDGE('',*,*,#31335,.F.);
#44703=ORIENTED_EDGE('',*,*,#31340,.F.);
#44704=ORIENTED_EDGE('',*,*,#31341,.T.);
#44705=ORIENTED_EDGE('',*,*,#31342,.T.);
#44706=ORIENTED_EDGE('',*,*,#31338,.F.);
#44707=ORIENTED_EDGE('',*,*,#31343,.F.);
#44708=ORIENTED_EDGE('',*,*,#31344,.T.);
#44709=ORIENTED_EDGE('',*,*,#31345,.T.);
#44710=ORIENTED_EDGE('',*,*,#31341,.F.);
#44711=ORIENTED_EDGE('',*,*,#31346,.F.);
#44712=ORIENTED_EDGE('',*,*,#31347,.T.);
#44713=ORIENTED_EDGE('',*,*,#31348,.T.);
#44714=ORIENTED_EDGE('',*,*,#31344,.F.);
#44715=ORIENTED_EDGE('',*,*,#31349,.F.);
#44716=ORIENTED_EDGE('',*,*,#31350,.T.);
#44717=ORIENTED_EDGE('',*,*,#31351,.T.);
#44718=ORIENTED_EDGE('',*,*,#31347,.F.);
#44719=ORIENTED_EDGE('',*,*,#31352,.F.);
#44720=ORIENTED_EDGE('',*,*,#31353,.T.);
#44721=ORIENTED_EDGE('',*,*,#31354,.T.);
#44722=ORIENTED_EDGE('',*,*,#31350,.F.);
#44723=ORIENTED_EDGE('',*,*,#31355,.F.);
#44724=ORIENTED_EDGE('',*,*,#31324,.T.);
#44725=ORIENTED_EDGE('',*,*,#31356,.T.);
#44726=ORIENTED_EDGE('',*,*,#31353,.F.);
#44727=ORIENTED_EDGE('',*,*,#31356,.F.);
#44728=ORIENTED_EDGE('',*,*,#31323,.F.);
#44729=ORIENTED_EDGE('',*,*,#31327,.F.);
#44730=ORIENTED_EDGE('',*,*,#31330,.F.);
#44731=ORIENTED_EDGE('',*,*,#31333,.F.);
#44732=ORIENTED_EDGE('',*,*,#31336,.F.);
#44733=ORIENTED_EDGE('',*,*,#31339,.F.);
#44734=ORIENTED_EDGE('',*,*,#31342,.F.);
#44735=ORIENTED_EDGE('',*,*,#31345,.F.);
#44736=ORIENTED_EDGE('',*,*,#31348,.F.);
#44737=ORIENTED_EDGE('',*,*,#31351,.F.);
#44738=ORIENTED_EDGE('',*,*,#31354,.F.);
#44739=ORIENTED_EDGE('',*,*,#31357,.F.);
#44740=ORIENTED_EDGE('',*,*,#31358,.T.);
#44741=ORIENTED_EDGE('',*,*,#31359,.T.);
#44742=ORIENTED_EDGE('',*,*,#31360,.F.);
#44743=ORIENTED_EDGE('',*,*,#31361,.F.);
#44744=ORIENTED_EDGE('',*,*,#31362,.T.);
#44745=ORIENTED_EDGE('',*,*,#31363,.T.);
#44746=ORIENTED_EDGE('',*,*,#31358,.F.);
#44747=ORIENTED_EDGE('',*,*,#31364,.F.);
#44748=ORIENTED_EDGE('',*,*,#31365,.T.);
#44749=ORIENTED_EDGE('',*,*,#31366,.T.);
#44750=ORIENTED_EDGE('',*,*,#31362,.F.);
#44751=ORIENTED_EDGE('',*,*,#31367,.F.);
#44752=ORIENTED_EDGE('',*,*,#31368,.T.);
#44753=ORIENTED_EDGE('',*,*,#31369,.T.);
#44754=ORIENTED_EDGE('',*,*,#31365,.F.);
#44755=ORIENTED_EDGE('',*,*,#31370,.F.);
#44756=ORIENTED_EDGE('',*,*,#31371,.T.);
#44757=ORIENTED_EDGE('',*,*,#31372,.T.);
#44758=ORIENTED_EDGE('',*,*,#31368,.F.);
#44759=ORIENTED_EDGE('',*,*,#31373,.F.);
#44760=ORIENTED_EDGE('',*,*,#31360,.T.);
#44761=ORIENTED_EDGE('',*,*,#31374,.T.);
#44762=ORIENTED_EDGE('',*,*,#31371,.F.);
#44763=ORIENTED_EDGE('',*,*,#31374,.F.);
#44764=ORIENTED_EDGE('',*,*,#31359,.F.);
#44765=ORIENTED_EDGE('',*,*,#31363,.F.);
#44766=ORIENTED_EDGE('',*,*,#31366,.F.);
#44767=ORIENTED_EDGE('',*,*,#31369,.F.);
#44768=ORIENTED_EDGE('',*,*,#31372,.F.);
#44769=ORIENTED_EDGE('',*,*,#31375,.F.);
#44770=ORIENTED_EDGE('',*,*,#31376,.T.);
#44771=ORIENTED_EDGE('',*,*,#31377,.T.);
#44772=ORIENTED_EDGE('',*,*,#31378,.F.);
#44773=ORIENTED_EDGE('',*,*,#31379,.F.);
#44774=ORIENTED_EDGE('',*,*,#31380,.T.);
#44775=ORIENTED_EDGE('',*,*,#31381,.T.);
#44776=ORIENTED_EDGE('',*,*,#31376,.F.);
#44777=ORIENTED_EDGE('',*,*,#31382,.F.);
#44778=ORIENTED_EDGE('',*,*,#31383,.T.);
#44779=ORIENTED_EDGE('',*,*,#31384,.T.);
#44780=ORIENTED_EDGE('',*,*,#31380,.F.);
#44781=ORIENTED_EDGE('',*,*,#31385,.F.);
#44782=ORIENTED_EDGE('',*,*,#31386,.T.);
#44783=ORIENTED_EDGE('',*,*,#31387,.T.);
#44784=ORIENTED_EDGE('',*,*,#31383,.F.);
#44785=ORIENTED_EDGE('',*,*,#31388,.F.);
#44786=ORIENTED_EDGE('',*,*,#31389,.T.);
#44787=ORIENTED_EDGE('',*,*,#31390,.T.);
#44788=ORIENTED_EDGE('',*,*,#31386,.F.);
#44789=ORIENTED_EDGE('',*,*,#31391,.F.);
#44790=ORIENTED_EDGE('',*,*,#31392,.T.);
#44791=ORIENTED_EDGE('',*,*,#31393,.T.);
#44792=ORIENTED_EDGE('',*,*,#31389,.F.);
#44793=ORIENTED_EDGE('',*,*,#31394,.F.);
#44794=ORIENTED_EDGE('',*,*,#31395,.T.);
#44795=ORIENTED_EDGE('',*,*,#31396,.T.);
#44796=ORIENTED_EDGE('',*,*,#31392,.F.);
#44797=ORIENTED_EDGE('',*,*,#31397,.F.);
#44798=ORIENTED_EDGE('',*,*,#31398,.T.);
#44799=ORIENTED_EDGE('',*,*,#31399,.T.);
#44800=ORIENTED_EDGE('',*,*,#31395,.F.);
#44801=ORIENTED_EDGE('',*,*,#31400,.F.);
#44802=ORIENTED_EDGE('',*,*,#31401,.T.);
#44803=ORIENTED_EDGE('',*,*,#31402,.T.);
#44804=ORIENTED_EDGE('',*,*,#31398,.F.);
#44805=ORIENTED_EDGE('',*,*,#31403,.F.);
#44806=ORIENTED_EDGE('',*,*,#31404,.T.);
#44807=ORIENTED_EDGE('',*,*,#31405,.T.);
#44808=ORIENTED_EDGE('',*,*,#31401,.F.);
#44809=ORIENTED_EDGE('',*,*,#31406,.F.);
#44810=ORIENTED_EDGE('',*,*,#31407,.T.);
#44811=ORIENTED_EDGE('',*,*,#31408,.T.);
#44812=ORIENTED_EDGE('',*,*,#31404,.F.);
#44813=ORIENTED_EDGE('',*,*,#31409,.F.);
#44814=ORIENTED_EDGE('',*,*,#31378,.T.);
#44815=ORIENTED_EDGE('',*,*,#31410,.T.);
#44816=ORIENTED_EDGE('',*,*,#31407,.F.);
#44817=ORIENTED_EDGE('',*,*,#31410,.F.);
#44818=ORIENTED_EDGE('',*,*,#31377,.F.);
#44819=ORIENTED_EDGE('',*,*,#31381,.F.);
#44820=ORIENTED_EDGE('',*,*,#31384,.F.);
#44821=ORIENTED_EDGE('',*,*,#31387,.F.);
#44822=ORIENTED_EDGE('',*,*,#31390,.F.);
#44823=ORIENTED_EDGE('',*,*,#31393,.F.);
#44824=ORIENTED_EDGE('',*,*,#31396,.F.);
#44825=ORIENTED_EDGE('',*,*,#31399,.F.);
#44826=ORIENTED_EDGE('',*,*,#31402,.F.);
#44827=ORIENTED_EDGE('',*,*,#31405,.F.);
#44828=ORIENTED_EDGE('',*,*,#31408,.F.);
#44829=ORIENTED_EDGE('',*,*,#31411,.F.);
#44830=ORIENTED_EDGE('',*,*,#31412,.T.);
#44831=ORIENTED_EDGE('',*,*,#31413,.T.);
#44832=ORIENTED_EDGE('',*,*,#31414,.F.);
#44833=ORIENTED_EDGE('',*,*,#31415,.F.);
#44834=ORIENTED_EDGE('',*,*,#31416,.T.);
#44835=ORIENTED_EDGE('',*,*,#31417,.T.);
#44836=ORIENTED_EDGE('',*,*,#31412,.F.);
#44837=ORIENTED_EDGE('',*,*,#31418,.F.);
#44838=ORIENTED_EDGE('',*,*,#31419,.T.);
#44839=ORIENTED_EDGE('',*,*,#31420,.T.);
#44840=ORIENTED_EDGE('',*,*,#31416,.F.);
#44841=ORIENTED_EDGE('',*,*,#31421,.F.);
#44842=ORIENTED_EDGE('',*,*,#31422,.T.);
#44843=ORIENTED_EDGE('',*,*,#31423,.T.);
#44844=ORIENTED_EDGE('',*,*,#31419,.F.);
#44845=ORIENTED_EDGE('',*,*,#31424,.F.);
#44846=ORIENTED_EDGE('',*,*,#31425,.T.);
#44847=ORIENTED_EDGE('',*,*,#31426,.T.);
#44848=ORIENTED_EDGE('',*,*,#31422,.F.);
#44849=ORIENTED_EDGE('',*,*,#31427,.F.);
#44850=ORIENTED_EDGE('',*,*,#31428,.T.);
#44851=ORIENTED_EDGE('',*,*,#31429,.T.);
#44852=ORIENTED_EDGE('',*,*,#31425,.F.);
#44853=ORIENTED_EDGE('',*,*,#31430,.F.);
#44854=ORIENTED_EDGE('',*,*,#31431,.T.);
#44855=ORIENTED_EDGE('',*,*,#31432,.T.);
#44856=ORIENTED_EDGE('',*,*,#31428,.F.);
#44857=ORIENTED_EDGE('',*,*,#31433,.F.);
#44858=ORIENTED_EDGE('',*,*,#31434,.T.);
#44859=ORIENTED_EDGE('',*,*,#31435,.T.);
#44860=ORIENTED_EDGE('',*,*,#31431,.F.);
#44861=ORIENTED_EDGE('',*,*,#31436,.F.);
#44862=ORIENTED_EDGE('',*,*,#31437,.T.);
#44863=ORIENTED_EDGE('',*,*,#31438,.T.);
#44864=ORIENTED_EDGE('',*,*,#31434,.F.);
#44865=ORIENTED_EDGE('',*,*,#31439,.F.);
#44866=ORIENTED_EDGE('',*,*,#31440,.T.);
#44867=ORIENTED_EDGE('',*,*,#31441,.T.);
#44868=ORIENTED_EDGE('',*,*,#31437,.F.);
#44869=ORIENTED_EDGE('',*,*,#31442,.F.);
#44870=ORIENTED_EDGE('',*,*,#31443,.T.);
#44871=ORIENTED_EDGE('',*,*,#31444,.T.);
#44872=ORIENTED_EDGE('',*,*,#31440,.F.);
#44873=ORIENTED_EDGE('',*,*,#31445,.F.);
#44874=ORIENTED_EDGE('',*,*,#31446,.T.);
#44875=ORIENTED_EDGE('',*,*,#31447,.T.);
#44876=ORIENTED_EDGE('',*,*,#31443,.F.);
#44877=ORIENTED_EDGE('',*,*,#31448,.F.);
#44878=ORIENTED_EDGE('',*,*,#31449,.T.);
#44879=ORIENTED_EDGE('',*,*,#31450,.T.);
#44880=ORIENTED_EDGE('',*,*,#31446,.F.);
#44881=ORIENTED_EDGE('',*,*,#31451,.F.);
#44882=ORIENTED_EDGE('',*,*,#31452,.T.);
#44883=ORIENTED_EDGE('',*,*,#31453,.T.);
#44884=ORIENTED_EDGE('',*,*,#31449,.F.);
#44885=ORIENTED_EDGE('',*,*,#31454,.F.);
#44886=ORIENTED_EDGE('',*,*,#31455,.T.);
#44887=ORIENTED_EDGE('',*,*,#31456,.T.);
#44888=ORIENTED_EDGE('',*,*,#31452,.F.);
#44889=ORIENTED_EDGE('',*,*,#31457,.F.);
#44890=ORIENTED_EDGE('',*,*,#31458,.T.);
#44891=ORIENTED_EDGE('',*,*,#31459,.T.);
#44892=ORIENTED_EDGE('',*,*,#31455,.F.);
#44893=ORIENTED_EDGE('',*,*,#31460,.F.);
#44894=ORIENTED_EDGE('',*,*,#31461,.T.);
#44895=ORIENTED_EDGE('',*,*,#31462,.T.);
#44896=ORIENTED_EDGE('',*,*,#31458,.F.);
#44897=ORIENTED_EDGE('',*,*,#31463,.F.);
#44898=ORIENTED_EDGE('',*,*,#31464,.T.);
#44899=ORIENTED_EDGE('',*,*,#31465,.T.);
#44900=ORIENTED_EDGE('',*,*,#31461,.F.);
#44901=ORIENTED_EDGE('',*,*,#31466,.F.);
#44902=ORIENTED_EDGE('',*,*,#31414,.T.);
#44903=ORIENTED_EDGE('',*,*,#31467,.T.);
#44904=ORIENTED_EDGE('',*,*,#31464,.F.);
#44905=ORIENTED_EDGE('',*,*,#31467,.F.);
#44906=ORIENTED_EDGE('',*,*,#31413,.F.);
#44907=ORIENTED_EDGE('',*,*,#31417,.F.);
#44908=ORIENTED_EDGE('',*,*,#31420,.F.);
#44909=ORIENTED_EDGE('',*,*,#31423,.F.);
#44910=ORIENTED_EDGE('',*,*,#31426,.F.);
#44911=ORIENTED_EDGE('',*,*,#31429,.F.);
#44912=ORIENTED_EDGE('',*,*,#31432,.F.);
#44913=ORIENTED_EDGE('',*,*,#31435,.F.);
#44914=ORIENTED_EDGE('',*,*,#31438,.F.);
#44915=ORIENTED_EDGE('',*,*,#31441,.F.);
#44916=ORIENTED_EDGE('',*,*,#31444,.F.);
#44917=ORIENTED_EDGE('',*,*,#31447,.F.);
#44918=ORIENTED_EDGE('',*,*,#31450,.F.);
#44919=ORIENTED_EDGE('',*,*,#31453,.F.);
#44920=ORIENTED_EDGE('',*,*,#31456,.F.);
#44921=ORIENTED_EDGE('',*,*,#31459,.F.);
#44922=ORIENTED_EDGE('',*,*,#31462,.F.);
#44923=ORIENTED_EDGE('',*,*,#31465,.F.);
#44924=ORIENTED_EDGE('',*,*,#31468,.F.);
#44925=ORIENTED_EDGE('',*,*,#31469,.F.);
#44926=ORIENTED_EDGE('',*,*,#31470,.F.);
#44927=ORIENTED_EDGE('',*,*,#31471,.T.);
#44928=ORIENTED_EDGE('',*,*,#31472,.F.);
#44929=ORIENTED_EDGE('',*,*,#31471,.F.);
#44930=ORIENTED_EDGE('',*,*,#31473,.F.);
#44931=ORIENTED_EDGE('',*,*,#31474,.T.);
#44932=ORIENTED_EDGE('',*,*,#31475,.F.);
#44933=ORIENTED_EDGE('',*,*,#31474,.F.);
#44934=ORIENTED_EDGE('',*,*,#31476,.F.);
#44935=ORIENTED_EDGE('',*,*,#31477,.T.);
#44936=ORIENTED_EDGE('',*,*,#31478,.F.);
#44937=ORIENTED_EDGE('',*,*,#31477,.F.);
#44938=ORIENTED_EDGE('',*,*,#31479,.F.);
#44939=ORIENTED_EDGE('',*,*,#31469,.T.);
#44940=ORIENTED_EDGE('',*,*,#31473,.T.);
#44941=ORIENTED_EDGE('',*,*,#31470,.T.);
#44942=ORIENTED_EDGE('',*,*,#31479,.T.);
#44943=ORIENTED_EDGE('',*,*,#31476,.T.);
#44944=ORIENTED_EDGE('',*,*,#31411,.T.);
#44945=ORIENTED_EDGE('',*,*,#31466,.T.);
#44946=ORIENTED_EDGE('',*,*,#31463,.T.);
#44947=ORIENTED_EDGE('',*,*,#31460,.T.);
#44948=ORIENTED_EDGE('',*,*,#31457,.T.);
#44949=ORIENTED_EDGE('',*,*,#31454,.T.);
#44950=ORIENTED_EDGE('',*,*,#31451,.T.);
#44951=ORIENTED_EDGE('',*,*,#31448,.T.);
#44952=ORIENTED_EDGE('',*,*,#31445,.T.);
#44953=ORIENTED_EDGE('',*,*,#31442,.T.);
#44954=ORIENTED_EDGE('',*,*,#31439,.T.);
#44955=ORIENTED_EDGE('',*,*,#31436,.T.);
#44956=ORIENTED_EDGE('',*,*,#31433,.T.);
#44957=ORIENTED_EDGE('',*,*,#31430,.T.);
#44958=ORIENTED_EDGE('',*,*,#31427,.T.);
#44959=ORIENTED_EDGE('',*,*,#31424,.T.);
#44960=ORIENTED_EDGE('',*,*,#31421,.T.);
#44961=ORIENTED_EDGE('',*,*,#31418,.T.);
#44962=ORIENTED_EDGE('',*,*,#31415,.T.);
#44963=ORIENTED_EDGE('',*,*,#31375,.T.);
#44964=ORIENTED_EDGE('',*,*,#31409,.T.);
#44965=ORIENTED_EDGE('',*,*,#31406,.T.);
#44966=ORIENTED_EDGE('',*,*,#31403,.T.);
#44967=ORIENTED_EDGE('',*,*,#31400,.T.);
#44968=ORIENTED_EDGE('',*,*,#31397,.T.);
#44969=ORIENTED_EDGE('',*,*,#31394,.T.);
#44970=ORIENTED_EDGE('',*,*,#31391,.T.);
#44971=ORIENTED_EDGE('',*,*,#31388,.T.);
#44972=ORIENTED_EDGE('',*,*,#31385,.T.);
#44973=ORIENTED_EDGE('',*,*,#31382,.T.);
#44974=ORIENTED_EDGE('',*,*,#31379,.T.);
#44975=ORIENTED_EDGE('',*,*,#31357,.T.);
#44976=ORIENTED_EDGE('',*,*,#31373,.T.);
#44977=ORIENTED_EDGE('',*,*,#31370,.T.);
#44978=ORIENTED_EDGE('',*,*,#31367,.T.);
#44979=ORIENTED_EDGE('',*,*,#31364,.T.);
#44980=ORIENTED_EDGE('',*,*,#31361,.T.);
#44981=ORIENTED_EDGE('',*,*,#31321,.T.);
#44982=ORIENTED_EDGE('',*,*,#31355,.T.);
#44983=ORIENTED_EDGE('',*,*,#31352,.T.);
#44984=ORIENTED_EDGE('',*,*,#31349,.T.);
#44985=ORIENTED_EDGE('',*,*,#31346,.T.);
#44986=ORIENTED_EDGE('',*,*,#31343,.T.);
#44987=ORIENTED_EDGE('',*,*,#31340,.T.);
#44988=ORIENTED_EDGE('',*,*,#31337,.T.);
#44989=ORIENTED_EDGE('',*,*,#31334,.T.);
#44990=ORIENTED_EDGE('',*,*,#31331,.T.);
#44991=ORIENTED_EDGE('',*,*,#31328,.T.);
#44992=ORIENTED_EDGE('',*,*,#31325,.T.);
#44993=ORIENTED_EDGE('',*,*,#31288,.T.);
#44994=ORIENTED_EDGE('',*,*,#31319,.T.);
#44995=ORIENTED_EDGE('',*,*,#31316,.T.);
#44996=ORIENTED_EDGE('',*,*,#31313,.T.);
#44997=ORIENTED_EDGE('',*,*,#31310,.T.);
#44998=ORIENTED_EDGE('',*,*,#31307,.T.);
#44999=ORIENTED_EDGE('',*,*,#31304,.T.);
#45000=ORIENTED_EDGE('',*,*,#31301,.T.);
#45001=ORIENTED_EDGE('',*,*,#31298,.T.);
#45002=ORIENTED_EDGE('',*,*,#31295,.T.);
#45003=ORIENTED_EDGE('',*,*,#31292,.T.);
#45004=ORIENTED_EDGE('',*,*,#31276,.T.);
#45005=ORIENTED_EDGE('',*,*,#31286,.T.);
#45006=ORIENTED_EDGE('',*,*,#31283,.T.);
#45007=ORIENTED_EDGE('',*,*,#31280,.T.);
#45008=ORIENTED_EDGE('',*,*,#31240,.T.);
#45009=ORIENTED_EDGE('',*,*,#31274,.T.);
#45010=ORIENTED_EDGE('',*,*,#31271,.T.);
#45011=ORIENTED_EDGE('',*,*,#31268,.T.);
#45012=ORIENTED_EDGE('',*,*,#31265,.T.);
#45013=ORIENTED_EDGE('',*,*,#31262,.T.);
#45014=ORIENTED_EDGE('',*,*,#31259,.T.);
#45015=ORIENTED_EDGE('',*,*,#31256,.T.);
#45016=ORIENTED_EDGE('',*,*,#31253,.T.);
#45017=ORIENTED_EDGE('',*,*,#31250,.T.);
#45018=ORIENTED_EDGE('',*,*,#31247,.T.);
#45019=ORIENTED_EDGE('',*,*,#31244,.T.);
#45020=ORIENTED_EDGE('',*,*,#31195,.T.);
#45021=ORIENTED_EDGE('',*,*,#31238,.T.);
#45022=ORIENTED_EDGE('',*,*,#31235,.T.);
#45023=ORIENTED_EDGE('',*,*,#31232,.T.);
#45024=ORIENTED_EDGE('',*,*,#31229,.T.);
#45025=ORIENTED_EDGE('',*,*,#31226,.T.);
#45026=ORIENTED_EDGE('',*,*,#31223,.T.);
#45027=ORIENTED_EDGE('',*,*,#31220,.T.);
#45028=ORIENTED_EDGE('',*,*,#31217,.T.);
#45029=ORIENTED_EDGE('',*,*,#31214,.T.);
#45030=ORIENTED_EDGE('',*,*,#31211,.T.);
#45031=ORIENTED_EDGE('',*,*,#31208,.T.);
#45032=ORIENTED_EDGE('',*,*,#31205,.T.);
#45033=ORIENTED_EDGE('',*,*,#31202,.T.);
#45034=ORIENTED_EDGE('',*,*,#31199,.T.);
#45035=ORIENTED_EDGE('',*,*,#31162,.T.);
#45036=ORIENTED_EDGE('',*,*,#31193,.T.);
#45037=ORIENTED_EDGE('',*,*,#31190,.T.);
#45038=ORIENTED_EDGE('',*,*,#31187,.T.);
#45039=ORIENTED_EDGE('',*,*,#31184,.T.);
#45040=ORIENTED_EDGE('',*,*,#31181,.T.);
#45041=ORIENTED_EDGE('',*,*,#31178,.T.);
#45042=ORIENTED_EDGE('',*,*,#31175,.T.);
#45043=ORIENTED_EDGE('',*,*,#31172,.T.);
#45044=ORIENTED_EDGE('',*,*,#31169,.T.);
#45045=ORIENTED_EDGE('',*,*,#31166,.T.);
#45046=ORIENTED_EDGE('',*,*,#31096,.T.);
#45047=ORIENTED_EDGE('',*,*,#31160,.T.);
#45048=ORIENTED_EDGE('',*,*,#31157,.T.);
#45049=ORIENTED_EDGE('',*,*,#31154,.T.);
#45050=ORIENTED_EDGE('',*,*,#31151,.T.);
#45051=ORIENTED_EDGE('',*,*,#31148,.T.);
#45052=ORIENTED_EDGE('',*,*,#31145,.T.);
#45053=ORIENTED_EDGE('',*,*,#31142,.T.);
#45054=ORIENTED_EDGE('',*,*,#31139,.T.);
#45055=ORIENTED_EDGE('',*,*,#31136,.T.);
#45056=ORIENTED_EDGE('',*,*,#31133,.T.);
#45057=ORIENTED_EDGE('',*,*,#31130,.T.);
#45058=ORIENTED_EDGE('',*,*,#31127,.T.);
#45059=ORIENTED_EDGE('',*,*,#31124,.T.);
#45060=ORIENTED_EDGE('',*,*,#31121,.T.);
#45061=ORIENTED_EDGE('',*,*,#31118,.T.);
#45062=ORIENTED_EDGE('',*,*,#31115,.T.);
#45063=ORIENTED_EDGE('',*,*,#31112,.T.);
#45064=ORIENTED_EDGE('',*,*,#31109,.T.);
#45065=ORIENTED_EDGE('',*,*,#31106,.T.);
#45066=ORIENTED_EDGE('',*,*,#31103,.T.);
#45067=ORIENTED_EDGE('',*,*,#31100,.T.);
#45068=ORIENTED_EDGE('',*,*,#31084,.T.);
#45069=ORIENTED_EDGE('',*,*,#31094,.T.);
#45070=ORIENTED_EDGE('',*,*,#31091,.T.);
#45071=ORIENTED_EDGE('',*,*,#31088,.T.);
#45072=ORIENTED_EDGE('',*,*,#31057,.T.);
#45073=ORIENTED_EDGE('',*,*,#31082,.T.);
#45074=ORIENTED_EDGE('',*,*,#31079,.T.);
#45075=ORIENTED_EDGE('',*,*,#31076,.T.);
#45076=ORIENTED_EDGE('',*,*,#31073,.T.);
#45077=ORIENTED_EDGE('',*,*,#31070,.T.);
#45078=ORIENTED_EDGE('',*,*,#31067,.T.);
#45079=ORIENTED_EDGE('',*,*,#31064,.T.);
#45080=ORIENTED_EDGE('',*,*,#31061,.T.);
#45081=ORIENTED_EDGE('',*,*,#31021,.T.);
#45082=ORIENTED_EDGE('',*,*,#31055,.T.);
#45083=ORIENTED_EDGE('',*,*,#31052,.T.);
#45084=ORIENTED_EDGE('',*,*,#31049,.T.);
#45085=ORIENTED_EDGE('',*,*,#31046,.T.);
#45086=ORIENTED_EDGE('',*,*,#31043,.T.);
#45087=ORIENTED_EDGE('',*,*,#31040,.T.);
#45088=ORIENTED_EDGE('',*,*,#31037,.T.);
#45089=ORIENTED_EDGE('',*,*,#31034,.T.);
#45090=ORIENTED_EDGE('',*,*,#31031,.T.);
#45091=ORIENTED_EDGE('',*,*,#31028,.T.);
#45092=ORIENTED_EDGE('',*,*,#31025,.T.);
#45093=ORIENTED_EDGE('',*,*,#30994,.T.);
#45094=ORIENTED_EDGE('',*,*,#31019,.T.);
#45095=ORIENTED_EDGE('',*,*,#31016,.T.);
#45096=ORIENTED_EDGE('',*,*,#31013,.T.);
#45097=ORIENTED_EDGE('',*,*,#31010,.T.);
#45098=ORIENTED_EDGE('',*,*,#31007,.T.);
#45099=ORIENTED_EDGE('',*,*,#31004,.T.);
#45100=ORIENTED_EDGE('',*,*,#31001,.T.);
#45101=ORIENTED_EDGE('',*,*,#30998,.T.);
#45102=ORIENTED_EDGE('',*,*,#30970,.T.);
#45103=ORIENTED_EDGE('',*,*,#30992,.T.);
#45104=ORIENTED_EDGE('',*,*,#30989,.T.);
#45105=ORIENTED_EDGE('',*,*,#30986,.T.);
#45106=ORIENTED_EDGE('',*,*,#30983,.T.);
#45107=ORIENTED_EDGE('',*,*,#30980,.T.);
#45108=ORIENTED_EDGE('',*,*,#30977,.T.);
#45109=ORIENTED_EDGE('',*,*,#30974,.T.);
#45110=ORIENTED_EDGE('',*,*,#30913,.T.);
#45111=ORIENTED_EDGE('',*,*,#30968,.T.);
#45112=ORIENTED_EDGE('',*,*,#30965,.T.);
#45113=ORIENTED_EDGE('',*,*,#30962,.T.);
#45114=ORIENTED_EDGE('',*,*,#30959,.T.);
#45115=ORIENTED_EDGE('',*,*,#30956,.T.);
#45116=ORIENTED_EDGE('',*,*,#30953,.T.);
#45117=ORIENTED_EDGE('',*,*,#30950,.T.);
#45118=ORIENTED_EDGE('',*,*,#30947,.T.);
#45119=ORIENTED_EDGE('',*,*,#30944,.T.);
#45120=ORIENTED_EDGE('',*,*,#30941,.T.);
#45121=ORIENTED_EDGE('',*,*,#30938,.T.);
#45122=ORIENTED_EDGE('',*,*,#30935,.T.);
#45123=ORIENTED_EDGE('',*,*,#30932,.T.);
#45124=ORIENTED_EDGE('',*,*,#30929,.T.);
#45125=ORIENTED_EDGE('',*,*,#30926,.T.);
#45126=ORIENTED_EDGE('',*,*,#30923,.T.);
#45127=ORIENTED_EDGE('',*,*,#30920,.T.);
#45128=ORIENTED_EDGE('',*,*,#30917,.T.);
#45129=ORIENTED_EDGE('',*,*,#30862,.T.);
#45130=ORIENTED_EDGE('',*,*,#30911,.T.);
#45131=ORIENTED_EDGE('',*,*,#30908,.T.);
#45132=ORIENTED_EDGE('',*,*,#30905,.T.);
#45133=ORIENTED_EDGE('',*,*,#30902,.T.);
#45134=ORIENTED_EDGE('',*,*,#30899,.T.);
#45135=ORIENTED_EDGE('',*,*,#30896,.T.);
#45136=ORIENTED_EDGE('',*,*,#30893,.T.);
#45137=ORIENTED_EDGE('',*,*,#30890,.T.);
#45138=ORIENTED_EDGE('',*,*,#30887,.T.);
#45139=ORIENTED_EDGE('',*,*,#30884,.T.);
#45140=ORIENTED_EDGE('',*,*,#30881,.T.);
#45141=ORIENTED_EDGE('',*,*,#30878,.T.);
#45142=ORIENTED_EDGE('',*,*,#30875,.T.);
#45143=ORIENTED_EDGE('',*,*,#30872,.T.);
#45144=ORIENTED_EDGE('',*,*,#30869,.T.);
#45145=ORIENTED_EDGE('',*,*,#30866,.T.);
#45146=ORIENTED_EDGE('',*,*,#30838,.T.);
#45147=ORIENTED_EDGE('',*,*,#30860,.T.);
#45148=ORIENTED_EDGE('',*,*,#30857,.T.);
#45149=ORIENTED_EDGE('',*,*,#30854,.T.);
#45150=ORIENTED_EDGE('',*,*,#30851,.T.);
#45151=ORIENTED_EDGE('',*,*,#30848,.T.);
#45152=ORIENTED_EDGE('',*,*,#30845,.T.);
#45153=ORIENTED_EDGE('',*,*,#30842,.T.);
#45154=ORIENTED_EDGE('',*,*,#30820,.T.);
#45155=ORIENTED_EDGE('',*,*,#30836,.T.);
#45156=ORIENTED_EDGE('',*,*,#30833,.T.);
#45157=ORIENTED_EDGE('',*,*,#30830,.T.);
#45158=ORIENTED_EDGE('',*,*,#30827,.T.);
#45159=ORIENTED_EDGE('',*,*,#30824,.T.);
#45160=ORIENTED_EDGE('',*,*,#30754,.T.);
#45161=ORIENTED_EDGE('',*,*,#30818,.T.);
#45162=ORIENTED_EDGE('',*,*,#30815,.T.);
#45163=ORIENTED_EDGE('',*,*,#30812,.T.);
#45164=ORIENTED_EDGE('',*,*,#30809,.T.);
#45165=ORIENTED_EDGE('',*,*,#30806,.T.);
#45166=ORIENTED_EDGE('',*,*,#30803,.T.);
#45167=ORIENTED_EDGE('',*,*,#30800,.T.);
#45168=ORIENTED_EDGE('',*,*,#30797,.T.);
#45169=ORIENTED_EDGE('',*,*,#30794,.T.);
#45170=ORIENTED_EDGE('',*,*,#30791,.T.);
#45171=ORIENTED_EDGE('',*,*,#30788,.T.);
#45172=ORIENTED_EDGE('',*,*,#30785,.T.);
#45173=ORIENTED_EDGE('',*,*,#30782,.T.);
#45174=ORIENTED_EDGE('',*,*,#30779,.T.);
#45175=ORIENTED_EDGE('',*,*,#30776,.T.);
#45176=ORIENTED_EDGE('',*,*,#30773,.T.);
#45177=ORIENTED_EDGE('',*,*,#30770,.T.);
#45178=ORIENTED_EDGE('',*,*,#30767,.T.);
#45179=ORIENTED_EDGE('',*,*,#30764,.T.);
#45180=ORIENTED_EDGE('',*,*,#30761,.T.);
#45181=ORIENTED_EDGE('',*,*,#30758,.T.);
#45182=ORIENTED_EDGE('',*,*,#30649,.T.);
#45183=ORIENTED_EDGE('',*,*,#30752,.T.);
#45184=ORIENTED_EDGE('',*,*,#30749,.T.);
#45185=ORIENTED_EDGE('',*,*,#30746,.T.);
#45186=ORIENTED_EDGE('',*,*,#30743,.T.);
#45187=ORIENTED_EDGE('',*,*,#30740,.T.);
#45188=ORIENTED_EDGE('',*,*,#30737,.T.);
#45189=ORIENTED_EDGE('',*,*,#30734,.T.);
#45190=ORIENTED_EDGE('',*,*,#30731,.T.);
#45191=ORIENTED_EDGE('',*,*,#30728,.T.);
#45192=ORIENTED_EDGE('',*,*,#30725,.T.);
#45193=ORIENTED_EDGE('',*,*,#30722,.T.);
#45194=ORIENTED_EDGE('',*,*,#30719,.T.);
#45195=ORIENTED_EDGE('',*,*,#30716,.T.);
#45196=ORIENTED_EDGE('',*,*,#30713,.T.);
#45197=ORIENTED_EDGE('',*,*,#30710,.T.);
#45198=ORIENTED_EDGE('',*,*,#30707,.T.);
#45199=ORIENTED_EDGE('',*,*,#30704,.T.);
#45200=ORIENTED_EDGE('',*,*,#30701,.T.);
#45201=ORIENTED_EDGE('',*,*,#30698,.T.);
#45202=ORIENTED_EDGE('',*,*,#30695,.T.);
#45203=ORIENTED_EDGE('',*,*,#30692,.T.);
#45204=ORIENTED_EDGE('',*,*,#30689,.T.);
#45205=ORIENTED_EDGE('',*,*,#30686,.T.);
#45206=ORIENTED_EDGE('',*,*,#30683,.T.);
#45207=ORIENTED_EDGE('',*,*,#30680,.T.);
#45208=ORIENTED_EDGE('',*,*,#30677,.T.);
#45209=ORIENTED_EDGE('',*,*,#30674,.T.);
#45210=ORIENTED_EDGE('',*,*,#30671,.T.);
#45211=ORIENTED_EDGE('',*,*,#30668,.T.);
#45212=ORIENTED_EDGE('',*,*,#30665,.T.);
#45213=ORIENTED_EDGE('',*,*,#30662,.T.);
#45214=ORIENTED_EDGE('',*,*,#30659,.T.);
#45215=ORIENTED_EDGE('',*,*,#30656,.T.);
#45216=ORIENTED_EDGE('',*,*,#30653,.T.);
#45217=ORIENTED_EDGE('',*,*,#30637,.T.);
#45218=ORIENTED_EDGE('',*,*,#30647,.T.);
#45219=ORIENTED_EDGE('',*,*,#30644,.T.);
#45220=ORIENTED_EDGE('',*,*,#30641,.T.);
#45221=ORIENTED_EDGE('',*,*,#30601,.T.);
#45222=ORIENTED_EDGE('',*,*,#30635,.T.);
#45223=ORIENTED_EDGE('',*,*,#30632,.T.);
#45224=ORIENTED_EDGE('',*,*,#30629,.T.);
#45225=ORIENTED_EDGE('',*,*,#30626,.T.);
#45226=ORIENTED_EDGE('',*,*,#30623,.T.);
#45227=ORIENTED_EDGE('',*,*,#30620,.T.);
#45228=ORIENTED_EDGE('',*,*,#30617,.T.);
#45229=ORIENTED_EDGE('',*,*,#30614,.T.);
#45230=ORIENTED_EDGE('',*,*,#30611,.T.);
#45231=ORIENTED_EDGE('',*,*,#30608,.T.);
#45232=ORIENTED_EDGE('',*,*,#30605,.T.);
#45233=ORIENTED_EDGE('',*,*,#31480,.T.);
#45234=ORIENTED_EDGE('',*,*,#31481,.T.);
#45235=ORIENTED_EDGE('',*,*,#31482,.T.);
#45236=ORIENTED_EDGE('',*,*,#31481,.F.);
#45237=ORIENTED_EDGE('',*,*,#31483,.F.);
#45238=ORIENTED_EDGE('',*,*,#31484,.T.);
#45239=ORIENTED_EDGE('',*,*,#31482,.F.);
#45240=ORIENTED_EDGE('',*,*,#31484,.F.);
#45241=ORIENTED_EDGE('',*,*,#31485,.F.);
#45242=ORIENTED_EDGE('',*,*,#31486,.F.);
#45243=ORIENTED_EDGE('',*,*,#31487,.F.);
#45244=ORIENTED_EDGE('',*,*,#31488,.F.);
#45245=ORIENTED_EDGE('',*,*,#31489,.F.);
#45246=ORIENTED_EDGE('',*,*,#31490,.F.);
#45247=ORIENTED_EDGE('',*,*,#31491,.F.);
#45248=ORIENTED_EDGE('',*,*,#31492,.F.);
#45249=ORIENTED_EDGE('',*,*,#31480,.F.);
#45250=ORIENTED_EDGE('',*,*,#31493,.F.);
#45251=ORIENTED_EDGE('',*,*,#31494,.T.);
#45252=ORIENTED_EDGE('',*,*,#31495,.T.);
#45253=ORIENTED_EDGE('',*,*,#31496,.T.);
#45254=ORIENTED_EDGE('',*,*,#31497,.T.);
#45255=ORIENTED_EDGE('',*,*,#31498,.T.);
#45256=ORIENTED_EDGE('',*,*,#31499,.T.);
#45257=ORIENTED_EDGE('',*,*,#31500,.T.);
#45258=ORIENTED_EDGE('',*,*,#31501,.F.);
#45259=ORIENTED_EDGE('',*,*,#31502,.F.);
#45260=ORIENTED_EDGE('',*,*,#31475,.T.);
#45261=ORIENTED_EDGE('',*,*,#31478,.T.);
#45262=ORIENTED_EDGE('',*,*,#31468,.T.);
#45263=ORIENTED_EDGE('',*,*,#31472,.T.);
#45264=ORIENTED_EDGE('',*,*,#31503,.T.);
#45265=ORIENTED_EDGE('',*,*,#31504,.T.);
#45266=ORIENTED_EDGE('',*,*,#31483,.T.);
#45267=ORIENTED_EDGE('',*,*,#31504,.F.);
#45268=ORIENTED_EDGE('',*,*,#31505,.F.);
#45269=ORIENTED_EDGE('',*,*,#31506,.F.);
#45270=ORIENTED_EDGE('',*,*,#31507,.F.);
#45271=ORIENTED_EDGE('',*,*,#31508,.F.);
#45272=ORIENTED_EDGE('',*,*,#31509,.F.);
#45273=ORIENTED_EDGE('',*,*,#31510,.F.);
#45274=ORIENTED_EDGE('',*,*,#31511,.F.);
#45275=ORIENTED_EDGE('',*,*,#31512,.F.);
#45276=ORIENTED_EDGE('',*,*,#31513,.F.);
#45277=ORIENTED_EDGE('',*,*,#31514,.F.);
#45278=ORIENTED_EDGE('',*,*,#31515,.F.);
#45279=ORIENTED_EDGE('',*,*,#31503,.F.);
#45280=ORIENTED_EDGE('',*,*,#31502,.T.);
#45281=ORIENTED_EDGE('',*,*,#31516,.T.);
#45282=ORIENTED_EDGE('',*,*,#31517,.T.);
#45283=ORIENTED_EDGE('',*,*,#31516,.F.);
#45284=ORIENTED_EDGE('',*,*,#31518,.F.);
#45285=ORIENTED_EDGE('',*,*,#31519,.T.);
#45286=ORIENTED_EDGE('',*,*,#31517,.F.);
#45287=ORIENTED_EDGE('',*,*,#31519,.F.);
#45288=ORIENTED_EDGE('',*,*,#31513,.T.);
#45289=ORIENTED_EDGE('',*,*,#31520,.T.);
#45290=ORIENTED_EDGE('',*,*,#31518,.T.);
#45291=ORIENTED_EDGE('',*,*,#31520,.F.);
#45292=ORIENTED_EDGE('',*,*,#31493,.T.);
#45293=ORIENTED_EDGE('',*,*,#31521,.T.);
#45294=ORIENTED_EDGE('',*,*,#31522,.T.);
#45295=ORIENTED_EDGE('',*,*,#31521,.F.);
#45296=ORIENTED_EDGE('',*,*,#31523,.F.);
#45297=ORIENTED_EDGE('',*,*,#31524,.T.);
#45298=ORIENTED_EDGE('',*,*,#31522,.F.);
#45299=ORIENTED_EDGE('',*,*,#31524,.F.);
#45300=ORIENTED_EDGE('',*,*,#31515,.T.);
#45301=ORIENTED_EDGE('',*,*,#31525,.T.);
#45302=ORIENTED_EDGE('',*,*,#31523,.T.);
#45303=ORIENTED_EDGE('',*,*,#31525,.F.);
#45304=ORIENTED_EDGE('',*,*,#31501,.T.);
#45305=ORIENTED_EDGE('',*,*,#31526,.T.);
#45306=ORIENTED_EDGE('',*,*,#31527,.T.);
#45307=ORIENTED_EDGE('',*,*,#31526,.F.);
#45308=ORIENTED_EDGE('',*,*,#31528,.F.);
#45309=ORIENTED_EDGE('',*,*,#31529,.T.);
#45310=ORIENTED_EDGE('',*,*,#31527,.F.);
#45311=ORIENTED_EDGE('',*,*,#31529,.F.);
#45312=ORIENTED_EDGE('',*,*,#31514,.T.);
#45313=ORIENTED_EDGE('',*,*,#31530,.T.);
#45314=ORIENTED_EDGE('',*,*,#31528,.T.);
#45315=ORIENTED_EDGE('',*,*,#31530,.F.);
#45316=ORIENTED_EDGE('',*,*,#31531,.F.);
#45317=ORIENTED_EDGE('',*,*,#31532,.T.);
#45318=ORIENTED_EDGE('',*,*,#31532,.F.);
#45319=ORIENTED_EDGE('',*,*,#31500,.F.);
#45320=ORIENTED_EDGE('',*,*,#31533,.T.);
#45321=ORIENTED_EDGE('',*,*,#31531,.T.);
#45322=ORIENTED_EDGE('',*,*,#31533,.F.);
#45323=ORIENTED_EDGE('',*,*,#31534,.F.);
#45324=ORIENTED_EDGE('',*,*,#31535,.T.);
#45325=ORIENTED_EDGE('',*,*,#31535,.F.);
#45326=ORIENTED_EDGE('',*,*,#31499,.F.);
#45327=ORIENTED_EDGE('',*,*,#31536,.T.);
#45328=ORIENTED_EDGE('',*,*,#31534,.T.);
#45329=ORIENTED_EDGE('',*,*,#31536,.F.);
#45330=ORIENTED_EDGE('',*,*,#31537,.F.);
#45331=ORIENTED_EDGE('',*,*,#31538,.T.);
#45332=ORIENTED_EDGE('',*,*,#31538,.F.);
#45333=ORIENTED_EDGE('',*,*,#31494,.F.);
#45334=ORIENTED_EDGE('',*,*,#31539,.T.);
#45335=ORIENTED_EDGE('',*,*,#31540,.T.);
#45336=ORIENTED_EDGE('',*,*,#31539,.F.);
#45337=ORIENTED_EDGE('',*,*,#31540,.F.);
#45338=ORIENTED_EDGE('',*,*,#31541,.T.);
#45339=ORIENTED_EDGE('',*,*,#31537,.T.);
#45340=ORIENTED_EDGE('',*,*,#31541,.F.);
#45341=ORIENTED_EDGE('',*,*,#31542,.F.);
#45342=ORIENTED_EDGE('',*,*,#31543,.T.);
#45343=ORIENTED_EDGE('',*,*,#31543,.F.);
#45344=ORIENTED_EDGE('',*,*,#31495,.F.);
#45345=ORIENTED_EDGE('',*,*,#31544,.T.);
#45346=ORIENTED_EDGE('',*,*,#31545,.T.);
#45347=ORIENTED_EDGE('',*,*,#31544,.F.);
#45348=ORIENTED_EDGE('',*,*,#31545,.F.);
#45349=ORIENTED_EDGE('',*,*,#31546,.T.);
#45350=ORIENTED_EDGE('',*,*,#31542,.T.);
#45351=ORIENTED_EDGE('',*,*,#31546,.F.);
#45352=ORIENTED_EDGE('',*,*,#31547,.F.);
#45353=ORIENTED_EDGE('',*,*,#31548,.T.);
#45354=ORIENTED_EDGE('',*,*,#31548,.F.);
#45355=ORIENTED_EDGE('',*,*,#31496,.F.);
#45356=ORIENTED_EDGE('',*,*,#31549,.T.);
#45357=ORIENTED_EDGE('',*,*,#31550,.T.);
#45358=ORIENTED_EDGE('',*,*,#31549,.F.);
#45359=ORIENTED_EDGE('',*,*,#31550,.F.);
#45360=ORIENTED_EDGE('',*,*,#31551,.T.);
#45361=ORIENTED_EDGE('',*,*,#31547,.T.);
#45362=ORIENTED_EDGE('',*,*,#31551,.F.);
#45363=ORIENTED_EDGE('',*,*,#31552,.F.);
#45364=ORIENTED_EDGE('',*,*,#31553,.T.);
#45365=ORIENTED_EDGE('',*,*,#31553,.F.);
#45366=ORIENTED_EDGE('',*,*,#31497,.F.);
#45367=ORIENTED_EDGE('',*,*,#31554,.T.);
#45368=ORIENTED_EDGE('',*,*,#31555,.T.);
#45369=ORIENTED_EDGE('',*,*,#31554,.F.);
#45370=ORIENTED_EDGE('',*,*,#31555,.F.);
#45371=ORIENTED_EDGE('',*,*,#31556,.T.);
#45372=ORIENTED_EDGE('',*,*,#31552,.T.);
#45373=ORIENTED_EDGE('',*,*,#31556,.F.);
#45374=ORIENTED_EDGE('',*,*,#31557,.F.);
#45375=ORIENTED_EDGE('',*,*,#31558,.T.);
#45376=ORIENTED_EDGE('',*,*,#31498,.F.);
#45377=ORIENTED_EDGE('',*,*,#31558,.F.);
#45378=ORIENTED_EDGE('',*,*,#31557,.T.);
#45379=ORIENTED_EDGE('',*,*,#31559,.T.);
#45380=ORIENTED_EDGE('',*,*,#31560,.T.);
#45381=ORIENTED_EDGE('',*,*,#31561,.T.);
#45382=ORIENTED_EDGE('',*,*,#31505,.T.);
#45383=ORIENTED_EDGE('',*,*,#31562,.T.);
#45384=ORIENTED_EDGE('',*,*,#31563,.T.);
#45385=ORIENTED_EDGE('',*,*,#31559,.F.);
#45386=ORIENTED_EDGE('',*,*,#31512,.T.);
#45387=ORIENTED_EDGE('',*,*,#31564,.T.);
#45388=ORIENTED_EDGE('',*,*,#31565,.T.);
#45389=ORIENTED_EDGE('',*,*,#31562,.F.);
#45390=ORIENTED_EDGE('',*,*,#31511,.T.);
#45391=ORIENTED_EDGE('',*,*,#31566,.T.);
#45392=ORIENTED_EDGE('',*,*,#31567,.T.);
#45393=ORIENTED_EDGE('',*,*,#31564,.F.);
#45394=ORIENTED_EDGE('',*,*,#31510,.T.);
#45395=ORIENTED_EDGE('',*,*,#31568,.T.);
#45396=ORIENTED_EDGE('',*,*,#31569,.T.);
#45397=ORIENTED_EDGE('',*,*,#31566,.F.);
#45398=ORIENTED_EDGE('',*,*,#31509,.T.);
#45399=ORIENTED_EDGE('',*,*,#31570,.T.);
#45400=ORIENTED_EDGE('',*,*,#31571,.T.);
#45401=ORIENTED_EDGE('',*,*,#31568,.F.);
#45402=ORIENTED_EDGE('',*,*,#31508,.T.);
#45403=ORIENTED_EDGE('',*,*,#31572,.T.);
#45404=ORIENTED_EDGE('',*,*,#31573,.T.);
#45405=ORIENTED_EDGE('',*,*,#31570,.F.);
#45406=ORIENTED_EDGE('',*,*,#31507,.T.);
#45407=ORIENTED_EDGE('',*,*,#31561,.F.);
#45408=ORIENTED_EDGE('',*,*,#31574,.T.);
#45409=ORIENTED_EDGE('',*,*,#31572,.F.);
#45410=ORIENTED_EDGE('',*,*,#31506,.T.);
#45411=ORIENTED_EDGE('',*,*,#31571,.F.);
#45412=ORIENTED_EDGE('',*,*,#31575,.T.);
#45413=ORIENTED_EDGE('',*,*,#31576,.F.);
#45414=ORIENTED_EDGE('',*,*,#31577,.F.);
#45415=ORIENTED_EDGE('',*,*,#31573,.F.);
#45416=ORIENTED_EDGE('',*,*,#31578,.T.);
#45417=ORIENTED_EDGE('',*,*,#31579,.F.);
#45418=ORIENTED_EDGE('',*,*,#31575,.F.);
#45419=ORIENTED_EDGE('',*,*,#31574,.F.);
#45420=ORIENTED_EDGE('',*,*,#31580,.T.);
#45421=ORIENTED_EDGE('',*,*,#31581,.F.);
#45422=ORIENTED_EDGE('',*,*,#31578,.F.);
#45423=ORIENTED_EDGE('',*,*,#31560,.F.);
#45424=ORIENTED_EDGE('',*,*,#31582,.T.);
#45425=ORIENTED_EDGE('',*,*,#31583,.F.);
#45426=ORIENTED_EDGE('',*,*,#31580,.F.);
#45427=ORIENTED_EDGE('',*,*,#31584,.T.);
#45428=ORIENTED_EDGE('',*,*,#31485,.T.);
#45429=ORIENTED_EDGE('',*,*,#31585,.T.);
#45430=ORIENTED_EDGE('',*,*,#31576,.T.);
#45431=ORIENTED_EDGE('',*,*,#31586,.T.);
#45432=ORIENTED_EDGE('',*,*,#31486,.T.);
#45433=ORIENTED_EDGE('',*,*,#31584,.F.);
#45434=ORIENTED_EDGE('',*,*,#31579,.T.);
#45435=ORIENTED_EDGE('',*,*,#31587,.T.);
#45436=ORIENTED_EDGE('',*,*,#31487,.T.);
#45437=ORIENTED_EDGE('',*,*,#31586,.F.);
#45438=ORIENTED_EDGE('',*,*,#31581,.T.);
#45439=ORIENTED_EDGE('',*,*,#31588,.T.);
#45440=ORIENTED_EDGE('',*,*,#31488,.T.);
#45441=ORIENTED_EDGE('',*,*,#31587,.F.);
#45442=ORIENTED_EDGE('',*,*,#31583,.T.);
#45443=ORIENTED_EDGE('',*,*,#31589,.T.);
#45444=ORIENTED_EDGE('',*,*,#31489,.T.);
#45445=ORIENTED_EDGE('',*,*,#31588,.F.);
#45446=ORIENTED_EDGE('',*,*,#31590,.T.);
#45447=ORIENTED_EDGE('',*,*,#31591,.T.);
#45448=ORIENTED_EDGE('',*,*,#31490,.T.);
#45449=ORIENTED_EDGE('',*,*,#31589,.F.);
#45450=ORIENTED_EDGE('',*,*,#31592,.T.);
#45451=ORIENTED_EDGE('',*,*,#31593,.T.);
#45452=ORIENTED_EDGE('',*,*,#31491,.T.);
#45453=ORIENTED_EDGE('',*,*,#31591,.F.);
#45454=ORIENTED_EDGE('',*,*,#31594,.T.);
#45455=ORIENTED_EDGE('',*,*,#31585,.F.);
#45456=ORIENTED_EDGE('',*,*,#31492,.T.);
#45457=ORIENTED_EDGE('',*,*,#31593,.F.);
#45458=ORIENTED_EDGE('',*,*,#31595,.T.);
#45459=ORIENTED_EDGE('',*,*,#31569,.F.);
#45460=ORIENTED_EDGE('',*,*,#31577,.T.);
#45461=ORIENTED_EDGE('',*,*,#31595,.F.);
#45462=ORIENTED_EDGE('',*,*,#31596,.F.);
#45463=ORIENTED_EDGE('',*,*,#31567,.F.);
#45464=ORIENTED_EDGE('',*,*,#31596,.T.);
#45465=ORIENTED_EDGE('',*,*,#31594,.F.);
#45466=ORIENTED_EDGE('',*,*,#31597,.F.);
#45467=ORIENTED_EDGE('',*,*,#31565,.F.);
#45468=ORIENTED_EDGE('',*,*,#31597,.T.);
#45469=ORIENTED_EDGE('',*,*,#31592,.F.);
#45470=ORIENTED_EDGE('',*,*,#31598,.F.);
#45471=ORIENTED_EDGE('',*,*,#31563,.F.);
#45472=ORIENTED_EDGE('',*,*,#31598,.T.);
#45473=ORIENTED_EDGE('',*,*,#31590,.F.);
#45474=ORIENTED_EDGE('',*,*,#31582,.F.);
#45475=ORIENTED_EDGE('',*,*,#31599,.T.);
#45476=ORIENTED_EDGE('',*,*,#31600,.T.);
#45477=ORIENTED_EDGE('',*,*,#31601,.F.);
#45478=ORIENTED_EDGE('',*,*,#31600,.F.);
#45479=ORIENTED_EDGE('',*,*,#31601,.T.);
#45480=ORIENTED_EDGE('',*,*,#31602,.T.);
#45481=ORIENTED_EDGE('',*,*,#31603,.F.);
#45482=ORIENTED_EDGE('',*,*,#31602,.F.);
#45483=ORIENTED_EDGE('',*,*,#31604,.F.);
#45484=ORIENTED_EDGE('',*,*,#31603,.T.);
#45485=ORIENTED_EDGE('',*,*,#31605,.F.);
#45486=ORIENTED_EDGE('',*,*,#31606,.T.);
#45487=ORIENTED_EDGE('',*,*,#31604,.T.);
#45488=ORIENTED_EDGE('',*,*,#31606,.F.);
#45489=ORIENTED_EDGE('',*,*,#31607,.F.);
#45490=ORIENTED_EDGE('',*,*,#31608,.T.);
#45491=ORIENTED_EDGE('',*,*,#31605,.T.);
#45492=ORIENTED_EDGE('',*,*,#31608,.F.);
#45493=ORIENTED_EDGE('',*,*,#31609,.F.);
#45494=ORIENTED_EDGE('',*,*,#31610,.T.);
#45495=ORIENTED_EDGE('',*,*,#31607,.T.);
#45496=ORIENTED_EDGE('',*,*,#31610,.F.);
#45497=ORIENTED_EDGE('',*,*,#31609,.T.);
#45498=ORIENTED_EDGE('',*,*,#31611,.F.);
#45499=ORIENTED_EDGE('',*,*,#31611,.T.);
#45500=ORIENTED_EDGE('',*,*,#31612,.T.);
#45501=ORIENTED_EDGE('',*,*,#31599,.F.);
#45502=ORIENTED_EDGE('',*,*,#31612,.F.);
#45503=ORIENTED_EDGE('',*,*,#31613,.F.);
#45504=ORIENTED_EDGE('',*,*,#31614,.T.);
#45505=ORIENTED_EDGE('',*,*,#31615,.T.);
#45506=ORIENTED_EDGE('',*,*,#31616,.T.);
#45507=ORIENTED_EDGE('',*,*,#31617,.F.);
#45508=ORIENTED_EDGE('',*,*,#31618,.T.);
#45509=ORIENTED_EDGE('',*,*,#31613,.T.);
#45510=ORIENTED_EDGE('',*,*,#31619,.T.);
#45511=ORIENTED_EDGE('',*,*,#31620,.F.);
#45512=ORIENTED_EDGE('',*,*,#31621,.T.);
#45513=ORIENTED_EDGE('',*,*,#31617,.T.);
#45514=ORIENTED_EDGE('',*,*,#31622,.T.);
#45515=ORIENTED_EDGE('',*,*,#31623,.F.);
#45516=ORIENTED_EDGE('',*,*,#31624,.T.);
#45517=ORIENTED_EDGE('',*,*,#31620,.T.);
#45518=ORIENTED_EDGE('',*,*,#31625,.T.);
#45519=ORIENTED_EDGE('',*,*,#31626,.F.);
#45520=ORIENTED_EDGE('',*,*,#31627,.T.);
#45521=ORIENTED_EDGE('',*,*,#31623,.T.);
#45522=ORIENTED_EDGE('',*,*,#31628,.T.);
#45523=ORIENTED_EDGE('',*,*,#31629,.F.);
#45524=ORIENTED_EDGE('',*,*,#31630,.T.);
#45525=ORIENTED_EDGE('',*,*,#31626,.T.);
#45526=ORIENTED_EDGE('',*,*,#31631,.T.);
#45527=ORIENTED_EDGE('',*,*,#31632,.F.);
#45528=ORIENTED_EDGE('',*,*,#31633,.T.);
#45529=ORIENTED_EDGE('',*,*,#31629,.T.);
#45530=ORIENTED_EDGE('',*,*,#31634,.T.);
#45531=ORIENTED_EDGE('',*,*,#31635,.F.);
#45532=ORIENTED_EDGE('',*,*,#31636,.T.);
#45533=ORIENTED_EDGE('',*,*,#31632,.T.);
#45534=ORIENTED_EDGE('',*,*,#31637,.T.);
#45535=ORIENTED_EDGE('',*,*,#31638,.F.);
#45536=ORIENTED_EDGE('',*,*,#31639,.T.);
#45537=ORIENTED_EDGE('',*,*,#31635,.T.);
#45538=ORIENTED_EDGE('',*,*,#31640,.T.);
#45539=ORIENTED_EDGE('',*,*,#31641,.F.);
#45540=ORIENTED_EDGE('',*,*,#31642,.T.);
#45541=ORIENTED_EDGE('',*,*,#31638,.T.);
#45542=ORIENTED_EDGE('',*,*,#31643,.T.);
#45543=ORIENTED_EDGE('',*,*,#31644,.F.);
#45544=ORIENTED_EDGE('',*,*,#31645,.T.);
#45545=ORIENTED_EDGE('',*,*,#31641,.T.);
#45546=ORIENTED_EDGE('',*,*,#31646,.T.);
#45547=ORIENTED_EDGE('',*,*,#31647,.F.);
#45548=ORIENTED_EDGE('',*,*,#31648,.T.);
#45549=ORIENTED_EDGE('',*,*,#31644,.T.);
#45550=ORIENTED_EDGE('',*,*,#31649,.T.);
#45551=ORIENTED_EDGE('',*,*,#31650,.F.);
#45552=ORIENTED_EDGE('',*,*,#31651,.T.);
#45553=ORIENTED_EDGE('',*,*,#31647,.T.);
#45554=ORIENTED_EDGE('',*,*,#31652,.T.);
#45555=ORIENTED_EDGE('',*,*,#31653,.F.);
#45556=ORIENTED_EDGE('',*,*,#31654,.T.);
#45557=ORIENTED_EDGE('',*,*,#31650,.T.);
#45558=ORIENTED_EDGE('',*,*,#31655,.T.);
#45559=ORIENTED_EDGE('',*,*,#31656,.F.);
#45560=ORIENTED_EDGE('',*,*,#31657,.T.);
#45561=ORIENTED_EDGE('',*,*,#31653,.T.);
#45562=ORIENTED_EDGE('',*,*,#31658,.T.);
#45563=ORIENTED_EDGE('',*,*,#31659,.F.);
#45564=ORIENTED_EDGE('',*,*,#31660,.T.);
#45565=ORIENTED_EDGE('',*,*,#31656,.T.);
#45566=ORIENTED_EDGE('',*,*,#31661,.T.);
#45567=ORIENTED_EDGE('',*,*,#31662,.F.);
#45568=ORIENTED_EDGE('',*,*,#31663,.T.);
#45569=ORIENTED_EDGE('',*,*,#31664,.F.);
#45570=ORIENTED_EDGE('',*,*,#31665,.F.);
#45571=ORIENTED_EDGE('',*,*,#31666,.T.);
#45572=ORIENTED_EDGE('',*,*,#31662,.T.);
#45573=ORIENTED_EDGE('',*,*,#31667,.F.);
#45574=ORIENTED_EDGE('',*,*,#31668,.F.);
#45575=ORIENTED_EDGE('',*,*,#31669,.F.);
#45576=ORIENTED_EDGE('',*,*,#31670,.T.);
#45577=ORIENTED_EDGE('',*,*,#31665,.T.);
#45578=ORIENTED_EDGE('',*,*,#31671,.F.);
#45579=ORIENTED_EDGE('',*,*,#31672,.F.);
#45580=ORIENTED_EDGE('',*,*,#31673,.T.);
#45581=ORIENTED_EDGE('',*,*,#31669,.T.);
#45582=ORIENTED_EDGE('',*,*,#31674,.F.);
#45583=ORIENTED_EDGE('',*,*,#31675,.F.);
#45584=ORIENTED_EDGE('',*,*,#31676,.T.);
#45585=ORIENTED_EDGE('',*,*,#31672,.T.);
#45586=ORIENTED_EDGE('',*,*,#31677,.F.);
#45587=ORIENTED_EDGE('',*,*,#31678,.F.);
#45588=ORIENTED_EDGE('',*,*,#31679,.T.);
#45589=ORIENTED_EDGE('',*,*,#31675,.T.);
#45590=ORIENTED_EDGE('',*,*,#31680,.F.);
#45591=ORIENTED_EDGE('',*,*,#31681,.F.);
#45592=ORIENTED_EDGE('',*,*,#31682,.T.);
#45593=ORIENTED_EDGE('',*,*,#31678,.T.);
#45594=ORIENTED_EDGE('',*,*,#31683,.F.);
#45595=ORIENTED_EDGE('',*,*,#31684,.F.);
#45596=ORIENTED_EDGE('',*,*,#31685,.T.);
#45597=ORIENTED_EDGE('',*,*,#31681,.T.);
#45598=ORIENTED_EDGE('',*,*,#31686,.F.);
#45599=ORIENTED_EDGE('',*,*,#31687,.F.);
#45600=ORIENTED_EDGE('',*,*,#31688,.T.);
#45601=ORIENTED_EDGE('',*,*,#31684,.T.);
#45602=ORIENTED_EDGE('',*,*,#31689,.F.);
#45603=ORIENTED_EDGE('',*,*,#31690,.F.);
#45604=ORIENTED_EDGE('',*,*,#31691,.T.);
#45605=ORIENTED_EDGE('',*,*,#31687,.T.);
#45606=ORIENTED_EDGE('',*,*,#31692,.F.);
#45607=ORIENTED_EDGE('',*,*,#31693,.F.);
#45608=ORIENTED_EDGE('',*,*,#31694,.T.);
#45609=ORIENTED_EDGE('',*,*,#31690,.T.);
#45610=ORIENTED_EDGE('',*,*,#31695,.F.);
#45611=ORIENTED_EDGE('',*,*,#31696,.F.);
#45612=ORIENTED_EDGE('',*,*,#31697,.T.);
#45613=ORIENTED_EDGE('',*,*,#31693,.T.);
#45614=ORIENTED_EDGE('',*,*,#31698,.F.);
#45615=ORIENTED_EDGE('',*,*,#31699,.F.);
#45616=ORIENTED_EDGE('',*,*,#31700,.T.);
#45617=ORIENTED_EDGE('',*,*,#31696,.T.);
#45618=ORIENTED_EDGE('',*,*,#31701,.F.);
#45619=ORIENTED_EDGE('',*,*,#31702,.F.);
#45620=ORIENTED_EDGE('',*,*,#31703,.T.);
#45621=ORIENTED_EDGE('',*,*,#31699,.T.);
#45622=ORIENTED_EDGE('',*,*,#31704,.F.);
#45623=ORIENTED_EDGE('',*,*,#31705,.F.);
#45624=ORIENTED_EDGE('',*,*,#31706,.T.);
#45625=ORIENTED_EDGE('',*,*,#31702,.T.);
#45626=ORIENTED_EDGE('',*,*,#31707,.F.);
#45627=ORIENTED_EDGE('',*,*,#31708,.F.);
#45628=ORIENTED_EDGE('',*,*,#31709,.T.);
#45629=ORIENTED_EDGE('',*,*,#31705,.T.);
#45630=ORIENTED_EDGE('',*,*,#31710,.F.);
#45631=ORIENTED_EDGE('',*,*,#31667,.T.);
#45632=ORIENTED_EDGE('',*,*,#31664,.T.);
#45633=ORIENTED_EDGE('',*,*,#31711,.T.);
#45634=ORIENTED_EDGE('',*,*,#31712,.F.);
#45635=ORIENTED_EDGE('',*,*,#31713,.F.);
#45636=ORIENTED_EDGE('',*,*,#31714,.T.);
#45637=ORIENTED_EDGE('',*,*,#31714,.F.);
#45638=ORIENTED_EDGE('',*,*,#31715,.F.);
#45639=ORIENTED_EDGE('',*,*,#31661,.F.);
#45640=ORIENTED_EDGE('',*,*,#31658,.F.);
#45641=ORIENTED_EDGE('',*,*,#31655,.F.);
#45642=ORIENTED_EDGE('',*,*,#31652,.F.);
#45643=ORIENTED_EDGE('',*,*,#31649,.F.);
#45644=ORIENTED_EDGE('',*,*,#31646,.F.);
#45645=ORIENTED_EDGE('',*,*,#31643,.F.);
#45646=ORIENTED_EDGE('',*,*,#31640,.F.);
#45647=ORIENTED_EDGE('',*,*,#31637,.F.);
#45648=ORIENTED_EDGE('',*,*,#31634,.F.);
#45649=ORIENTED_EDGE('',*,*,#31631,.F.);
#45650=ORIENTED_EDGE('',*,*,#31628,.F.);
#45651=ORIENTED_EDGE('',*,*,#31625,.F.);
#45652=ORIENTED_EDGE('',*,*,#31622,.F.);
#45653=ORIENTED_EDGE('',*,*,#31619,.F.);
#45654=ORIENTED_EDGE('',*,*,#31616,.F.);
#45655=ORIENTED_EDGE('',*,*,#31716,.F.);
#45656=ORIENTED_EDGE('',*,*,#31717,.T.);
#45657=ORIENTED_EDGE('',*,*,#31710,.T.);
#45658=ORIENTED_EDGE('',*,*,#31707,.T.);
#45659=ORIENTED_EDGE('',*,*,#31704,.T.);
#45660=ORIENTED_EDGE('',*,*,#31701,.T.);
#45661=ORIENTED_EDGE('',*,*,#31698,.T.);
#45662=ORIENTED_EDGE('',*,*,#31695,.T.);
#45663=ORIENTED_EDGE('',*,*,#31692,.T.);
#45664=ORIENTED_EDGE('',*,*,#31689,.T.);
#45665=ORIENTED_EDGE('',*,*,#31686,.T.);
#45666=ORIENTED_EDGE('',*,*,#31683,.T.);
#45667=ORIENTED_EDGE('',*,*,#31680,.T.);
#45668=ORIENTED_EDGE('',*,*,#31677,.T.);
#45669=ORIENTED_EDGE('',*,*,#31674,.T.);
#45670=ORIENTED_EDGE('',*,*,#31671,.T.);
#45671=ORIENTED_EDGE('',*,*,#31668,.T.);
#45672=ORIENTED_EDGE('',*,*,#31718,.T.);
#45673=ORIENTED_EDGE('',*,*,#31719,.T.);
#45674=ORIENTED_EDGE('',*,*,#31720,.T.);
#45675=ORIENTED_EDGE('',*,*,#31721,.T.);
#45676=ORIENTED_EDGE('',*,*,#31716,.T.);
#45677=ORIENTED_EDGE('',*,*,#31708,.T.);
#45678=ORIENTED_EDGE('',*,*,#31717,.F.);
#45679=ORIENTED_EDGE('',*,*,#31721,.F.);
#45680=ORIENTED_EDGE('',*,*,#31722,.T.);
#45681=ORIENTED_EDGE('',*,*,#31711,.F.);
#45682=ORIENTED_EDGE('',*,*,#31663,.F.);
#45683=ORIENTED_EDGE('',*,*,#31666,.F.);
#45684=ORIENTED_EDGE('',*,*,#31670,.F.);
#45685=ORIENTED_EDGE('',*,*,#31673,.F.);
#45686=ORIENTED_EDGE('',*,*,#31676,.F.);
#45687=ORIENTED_EDGE('',*,*,#31679,.F.);
#45688=ORIENTED_EDGE('',*,*,#31682,.F.);
#45689=ORIENTED_EDGE('',*,*,#31685,.F.);
#45690=ORIENTED_EDGE('',*,*,#31688,.F.);
#45691=ORIENTED_EDGE('',*,*,#31691,.F.);
#45692=ORIENTED_EDGE('',*,*,#31694,.F.);
#45693=ORIENTED_EDGE('',*,*,#31697,.F.);
#45694=ORIENTED_EDGE('',*,*,#31700,.F.);
#45695=ORIENTED_EDGE('',*,*,#31703,.F.);
#45696=ORIENTED_EDGE('',*,*,#31706,.F.);
#45697=ORIENTED_EDGE('',*,*,#31709,.F.);
#45698=ORIENTED_EDGE('',*,*,#31722,.F.);
#45699=ORIENTED_EDGE('',*,*,#31720,.F.);
#45700=ORIENTED_EDGE('',*,*,#31614,.F.);
#45701=ORIENTED_EDGE('',*,*,#31618,.F.);
#45702=ORIENTED_EDGE('',*,*,#31621,.F.);
#45703=ORIENTED_EDGE('',*,*,#31624,.F.);
#45704=ORIENTED_EDGE('',*,*,#31627,.F.);
#45705=ORIENTED_EDGE('',*,*,#31630,.F.);
#45706=ORIENTED_EDGE('',*,*,#31633,.F.);
#45707=ORIENTED_EDGE('',*,*,#31636,.F.);
#45708=ORIENTED_EDGE('',*,*,#31639,.F.);
#45709=ORIENTED_EDGE('',*,*,#31642,.F.);
#45710=ORIENTED_EDGE('',*,*,#31645,.F.);
#45711=ORIENTED_EDGE('',*,*,#31648,.F.);
#45712=ORIENTED_EDGE('',*,*,#31651,.F.);
#45713=ORIENTED_EDGE('',*,*,#31654,.F.);
#45714=ORIENTED_EDGE('',*,*,#31657,.F.);
#45715=ORIENTED_EDGE('',*,*,#31660,.F.);
#45716=ORIENTED_EDGE('',*,*,#31723,.F.);
#45717=ORIENTED_EDGE('',*,*,#31713,.T.);
#45718=ORIENTED_EDGE('',*,*,#31724,.T.);
#45719=ORIENTED_EDGE('',*,*,#31725,.T.);
#45720=ORIENTED_EDGE('',*,*,#31724,.F.);
#45721=ORIENTED_EDGE('',*,*,#31712,.T.);
#45722=ORIENTED_EDGE('',*,*,#31726,.T.);
#45723=ORIENTED_EDGE('',*,*,#31659,.T.);
#45724=ORIENTED_EDGE('',*,*,#31715,.T.);
#45725=ORIENTED_EDGE('',*,*,#31726,.F.);
#45726=ORIENTED_EDGE('',*,*,#31723,.T.);
#45727=ORIENTED_EDGE('',*,*,#31727,.F.);
#45728=ORIENTED_EDGE('',*,*,#31725,.F.);
#45729=ORIENTED_EDGE('',*,*,#31728,.F.);
#45730=ORIENTED_EDGE('',*,*,#31729,.T.);
#45731=ORIENTED_EDGE('',*,*,#31730,.T.);
#45732=ORIENTED_EDGE('',*,*,#31731,.T.);
#45733=ORIENTED_EDGE('',*,*,#31732,.F.);
#45734=ORIENTED_EDGE('',*,*,#31731,.F.);
#45735=ORIENTED_EDGE('',*,*,#31733,.F.);
#45736=ORIENTED_EDGE('',*,*,#31734,.F.);
#45737=ORIENTED_EDGE('',*,*,#31733,.T.);
#45738=ORIENTED_EDGE('',*,*,#31730,.F.);
#45739=ORIENTED_EDGE('',*,*,#31735,.T.);
#45740=ORIENTED_EDGE('',*,*,#31736,.F.);
#45741=ORIENTED_EDGE('',*,*,#31735,.F.);
#45742=ORIENTED_EDGE('',*,*,#31729,.F.);
#45743=ORIENTED_EDGE('',*,*,#31737,.F.);
#45744=ORIENTED_EDGE('',*,*,#31738,.T.);
#45745=ORIENTED_EDGE('',*,*,#31739,.T.);
#45746=ORIENTED_EDGE('',*,*,#31740,.T.);
#45747=ORIENTED_EDGE('',*,*,#31741,.F.);
#45748=ORIENTED_EDGE('',*,*,#31740,.F.);
#45749=ORIENTED_EDGE('',*,*,#31742,.F.);
#45750=ORIENTED_EDGE('',*,*,#31743,.F.);
#45751=ORIENTED_EDGE('',*,*,#31742,.T.);
#45752=ORIENTED_EDGE('',*,*,#31739,.F.);
#45753=ORIENTED_EDGE('',*,*,#31744,.T.);
#45754=ORIENTED_EDGE('',*,*,#31745,.F.);
#45755=ORIENTED_EDGE('',*,*,#31744,.F.);
#45756=ORIENTED_EDGE('',*,*,#31738,.F.);
#45757=ORIENTED_EDGE('',*,*,#31746,.F.);
#45758=ORIENTED_EDGE('',*,*,#31747,.T.);
#45759=ORIENTED_EDGE('',*,*,#31748,.T.);
#45760=ORIENTED_EDGE('',*,*,#31749,.T.);
#45761=ORIENTED_EDGE('',*,*,#31750,.F.);
#45762=ORIENTED_EDGE('',*,*,#31749,.F.);
#45763=ORIENTED_EDGE('',*,*,#31751,.F.);
#45764=ORIENTED_EDGE('',*,*,#31752,.F.);
#45765=ORIENTED_EDGE('',*,*,#31751,.T.);
#45766=ORIENTED_EDGE('',*,*,#31748,.F.);
#45767=ORIENTED_EDGE('',*,*,#31753,.T.);
#45768=ORIENTED_EDGE('',*,*,#31754,.F.);
#45769=ORIENTED_EDGE('',*,*,#31753,.F.);
#45770=ORIENTED_EDGE('',*,*,#31747,.F.);
#45771=ORIENTED_EDGE('',*,*,#31755,.F.);
#45772=ORIENTED_EDGE('',*,*,#31756,.T.);
#45773=ORIENTED_EDGE('',*,*,#31757,.T.);
#45774=ORIENTED_EDGE('',*,*,#31758,.T.);
#45775=ORIENTED_EDGE('',*,*,#31759,.F.);
#45776=ORIENTED_EDGE('',*,*,#31758,.F.);
#45777=ORIENTED_EDGE('',*,*,#31760,.F.);
#45778=ORIENTED_EDGE('',*,*,#31761,.F.);
#45779=ORIENTED_EDGE('',*,*,#31760,.T.);
#45780=ORIENTED_EDGE('',*,*,#31757,.F.);
#45781=ORIENTED_EDGE('',*,*,#31762,.T.);
#45782=ORIENTED_EDGE('',*,*,#31763,.F.);
#45783=ORIENTED_EDGE('',*,*,#31762,.F.);
#45784=ORIENTED_EDGE('',*,*,#31756,.F.);
#45785=ORIENTED_EDGE('',*,*,#31764,.F.);
#45786=ORIENTED_EDGE('',*,*,#31765,.T.);
#45787=ORIENTED_EDGE('',*,*,#31766,.T.);
#45788=ORIENTED_EDGE('',*,*,#31767,.T.);
#45789=ORIENTED_EDGE('',*,*,#31768,.F.);
#45790=ORIENTED_EDGE('',*,*,#31767,.F.);
#45791=ORIENTED_EDGE('',*,*,#31769,.F.);
#45792=ORIENTED_EDGE('',*,*,#31770,.F.);
#45793=ORIENTED_EDGE('',*,*,#31769,.T.);
#45794=ORIENTED_EDGE('',*,*,#31766,.F.);
#45795=ORIENTED_EDGE('',*,*,#31771,.T.);
#45796=ORIENTED_EDGE('',*,*,#31772,.F.);
#45797=ORIENTED_EDGE('',*,*,#31771,.F.);
#45798=ORIENTED_EDGE('',*,*,#31765,.F.);
#45799=ORIENTED_EDGE('',*,*,#31773,.F.);
#45800=ORIENTED_EDGE('',*,*,#31774,.T.);
#45801=ORIENTED_EDGE('',*,*,#31775,.T.);
#45802=ORIENTED_EDGE('',*,*,#31776,.T.);
#45803=ORIENTED_EDGE('',*,*,#31777,.F.);
#45804=ORIENTED_EDGE('',*,*,#31776,.F.);
#45805=ORIENTED_EDGE('',*,*,#31778,.F.);
#45806=ORIENTED_EDGE('',*,*,#31779,.F.);
#45807=ORIENTED_EDGE('',*,*,#31778,.T.);
#45808=ORIENTED_EDGE('',*,*,#31775,.F.);
#45809=ORIENTED_EDGE('',*,*,#31780,.T.);
#45810=ORIENTED_EDGE('',*,*,#31781,.F.);
#45811=ORIENTED_EDGE('',*,*,#31780,.F.);
#45812=ORIENTED_EDGE('',*,*,#31774,.F.);
#45813=ORIENTED_EDGE('',*,*,#31782,.F.);
#45814=ORIENTED_EDGE('',*,*,#31783,.T.);
#45815=ORIENTED_EDGE('',*,*,#31784,.T.);
#45816=ORIENTED_EDGE('',*,*,#31785,.T.);
#45817=ORIENTED_EDGE('',*,*,#31786,.F.);
#45818=ORIENTED_EDGE('',*,*,#31785,.F.);
#45819=ORIENTED_EDGE('',*,*,#31787,.F.);
#45820=ORIENTED_EDGE('',*,*,#31788,.F.);
#45821=ORIENTED_EDGE('',*,*,#31787,.T.);
#45822=ORIENTED_EDGE('',*,*,#31784,.F.);
#45823=ORIENTED_EDGE('',*,*,#31789,.T.);
#45824=ORIENTED_EDGE('',*,*,#31790,.F.);
#45825=ORIENTED_EDGE('',*,*,#31789,.F.);
#45826=ORIENTED_EDGE('',*,*,#31783,.F.);
#45827=ORIENTED_EDGE('',*,*,#31791,.F.);
#45828=ORIENTED_EDGE('',*,*,#31792,.T.);
#45829=ORIENTED_EDGE('',*,*,#31793,.T.);
#45830=ORIENTED_EDGE('',*,*,#31794,.T.);
#45831=ORIENTED_EDGE('',*,*,#31795,.F.);
#45832=ORIENTED_EDGE('',*,*,#31794,.F.);
#45833=ORIENTED_EDGE('',*,*,#31796,.F.);
#45834=ORIENTED_EDGE('',*,*,#31797,.F.);
#45835=ORIENTED_EDGE('',*,*,#31796,.T.);
#45836=ORIENTED_EDGE('',*,*,#31793,.F.);
#45837=ORIENTED_EDGE('',*,*,#31798,.T.);
#45838=ORIENTED_EDGE('',*,*,#31799,.F.);
#45839=ORIENTED_EDGE('',*,*,#31798,.F.);
#45840=ORIENTED_EDGE('',*,*,#31792,.F.);
#45841=ORIENTED_EDGE('',*,*,#31800,.F.);
#45842=ORIENTED_EDGE('',*,*,#31801,.T.);
#45843=ORIENTED_EDGE('',*,*,#31802,.T.);
#45844=ORIENTED_EDGE('',*,*,#31803,.T.);
#45845=ORIENTED_EDGE('',*,*,#31804,.F.);
#45846=ORIENTED_EDGE('',*,*,#31803,.F.);
#45847=ORIENTED_EDGE('',*,*,#31805,.F.);
#45848=ORIENTED_EDGE('',*,*,#31806,.F.);
#45849=ORIENTED_EDGE('',*,*,#31805,.T.);
#45850=ORIENTED_EDGE('',*,*,#31802,.F.);
#45851=ORIENTED_EDGE('',*,*,#31807,.T.);
#45852=ORIENTED_EDGE('',*,*,#31808,.F.);
#45853=ORIENTED_EDGE('',*,*,#31807,.F.);
#45854=ORIENTED_EDGE('',*,*,#31801,.F.);
#45855=ORIENTED_EDGE('',*,*,#31809,.F.);
#45856=ORIENTED_EDGE('',*,*,#31810,.T.);
#45857=ORIENTED_EDGE('',*,*,#31811,.T.);
#45858=ORIENTED_EDGE('',*,*,#31812,.T.);
#45859=ORIENTED_EDGE('',*,*,#31813,.F.);
#45860=ORIENTED_EDGE('',*,*,#31812,.F.);
#45861=ORIENTED_EDGE('',*,*,#31814,.F.);
#45862=ORIENTED_EDGE('',*,*,#31815,.F.);
#45863=ORIENTED_EDGE('',*,*,#31814,.T.);
#45864=ORIENTED_EDGE('',*,*,#31811,.F.);
#45865=ORIENTED_EDGE('',*,*,#31816,.T.);
#45866=ORIENTED_EDGE('',*,*,#31817,.F.);
#45867=ORIENTED_EDGE('',*,*,#31816,.F.);
#45868=ORIENTED_EDGE('',*,*,#31810,.F.);
#45869=ORIENTED_EDGE('',*,*,#31818,.F.);
#45870=ORIENTED_EDGE('',*,*,#31819,.T.);
#45871=ORIENTED_EDGE('',*,*,#31820,.T.);
#45872=ORIENTED_EDGE('',*,*,#31821,.T.);
#45873=ORIENTED_EDGE('',*,*,#31822,.F.);
#45874=ORIENTED_EDGE('',*,*,#31821,.F.);
#45875=ORIENTED_EDGE('',*,*,#31823,.F.);
#45876=ORIENTED_EDGE('',*,*,#31824,.F.);
#45877=ORIENTED_EDGE('',*,*,#31823,.T.);
#45878=ORIENTED_EDGE('',*,*,#31820,.F.);
#45879=ORIENTED_EDGE('',*,*,#31825,.T.);
#45880=ORIENTED_EDGE('',*,*,#31826,.F.);
#45881=ORIENTED_EDGE('',*,*,#31825,.F.);
#45882=ORIENTED_EDGE('',*,*,#31819,.F.);
#45883=ORIENTED_EDGE('',*,*,#31827,.F.);
#45884=ORIENTED_EDGE('',*,*,#31828,.T.);
#45885=ORIENTED_EDGE('',*,*,#31829,.T.);
#45886=ORIENTED_EDGE('',*,*,#31830,.T.);
#45887=ORIENTED_EDGE('',*,*,#31831,.F.);
#45888=ORIENTED_EDGE('',*,*,#31830,.F.);
#45889=ORIENTED_EDGE('',*,*,#31832,.F.);
#45890=ORIENTED_EDGE('',*,*,#31833,.F.);
#45891=ORIENTED_EDGE('',*,*,#31832,.T.);
#45892=ORIENTED_EDGE('',*,*,#31829,.F.);
#45893=ORIENTED_EDGE('',*,*,#31834,.T.);
#45894=ORIENTED_EDGE('',*,*,#31835,.F.);
#45895=ORIENTED_EDGE('',*,*,#31834,.F.);
#45896=ORIENTED_EDGE('',*,*,#31828,.F.);
#45897=ORIENTED_EDGE('',*,*,#31836,.F.);
#45898=ORIENTED_EDGE('',*,*,#31837,.T.);
#45899=ORIENTED_EDGE('',*,*,#31838,.T.);
#45900=ORIENTED_EDGE('',*,*,#31839,.T.);
#45901=ORIENTED_EDGE('',*,*,#31840,.F.);
#45902=ORIENTED_EDGE('',*,*,#31839,.F.);
#45903=ORIENTED_EDGE('',*,*,#31841,.F.);
#45904=ORIENTED_EDGE('',*,*,#31842,.F.);
#45905=ORIENTED_EDGE('',*,*,#31841,.T.);
#45906=ORIENTED_EDGE('',*,*,#31838,.F.);
#45907=ORIENTED_EDGE('',*,*,#31843,.T.);
#45908=ORIENTED_EDGE('',*,*,#31844,.F.);
#45909=ORIENTED_EDGE('',*,*,#31843,.F.);
#45910=ORIENTED_EDGE('',*,*,#31837,.F.);
#45911=ORIENTED_EDGE('',*,*,#31845,.F.);
#45912=ORIENTED_EDGE('',*,*,#31846,.T.);
#45913=ORIENTED_EDGE('',*,*,#31847,.T.);
#45914=ORIENTED_EDGE('',*,*,#31848,.T.);
#45915=ORIENTED_EDGE('',*,*,#31849,.F.);
#45916=ORIENTED_EDGE('',*,*,#31848,.F.);
#45917=ORIENTED_EDGE('',*,*,#31850,.F.);
#45918=ORIENTED_EDGE('',*,*,#31851,.F.);
#45919=ORIENTED_EDGE('',*,*,#31850,.T.);
#45920=ORIENTED_EDGE('',*,*,#31847,.F.);
#45921=ORIENTED_EDGE('',*,*,#31852,.T.);
#45922=ORIENTED_EDGE('',*,*,#31853,.F.);
#45923=ORIENTED_EDGE('',*,*,#31852,.F.);
#45924=ORIENTED_EDGE('',*,*,#31846,.F.);
#45925=ORIENTED_EDGE('',*,*,#31854,.F.);
#45926=ORIENTED_EDGE('',*,*,#31855,.T.);
#45927=ORIENTED_EDGE('',*,*,#31856,.T.);
#45928=ORIENTED_EDGE('',*,*,#31857,.T.);
#45929=ORIENTED_EDGE('',*,*,#31858,.F.);
#45930=ORIENTED_EDGE('',*,*,#31857,.F.);
#45931=ORIENTED_EDGE('',*,*,#31859,.F.);
#45932=ORIENTED_EDGE('',*,*,#31860,.F.);
#45933=ORIENTED_EDGE('',*,*,#31859,.T.);
#45934=ORIENTED_EDGE('',*,*,#31856,.F.);
#45935=ORIENTED_EDGE('',*,*,#31861,.T.);
#45936=ORIENTED_EDGE('',*,*,#31862,.F.);
#45937=ORIENTED_EDGE('',*,*,#31861,.F.);
#45938=ORIENTED_EDGE('',*,*,#31855,.F.);
#45939=ORIENTED_EDGE('',*,*,#31863,.F.);
#45940=ORIENTED_EDGE('',*,*,#31864,.T.);
#45941=ORIENTED_EDGE('',*,*,#31865,.T.);
#45942=ORIENTED_EDGE('',*,*,#31866,.T.);
#45943=ORIENTED_EDGE('',*,*,#31867,.F.);
#45944=ORIENTED_EDGE('',*,*,#31866,.F.);
#45945=ORIENTED_EDGE('',*,*,#31868,.F.);
#45946=ORIENTED_EDGE('',*,*,#31869,.F.);
#45947=ORIENTED_EDGE('',*,*,#31868,.T.);
#45948=ORIENTED_EDGE('',*,*,#31865,.F.);
#45949=ORIENTED_EDGE('',*,*,#31870,.T.);
#45950=ORIENTED_EDGE('',*,*,#31871,.F.);
#45951=ORIENTED_EDGE('',*,*,#31870,.F.);
#45952=ORIENTED_EDGE('',*,*,#31864,.F.);
#45953=ORIENTED_EDGE('',*,*,#31872,.F.);
#45954=ORIENTED_EDGE('',*,*,#31873,.T.);
#45955=ORIENTED_EDGE('',*,*,#31874,.T.);
#45956=ORIENTED_EDGE('',*,*,#31875,.T.);
#45957=ORIENTED_EDGE('',*,*,#31876,.F.);
#45958=ORIENTED_EDGE('',*,*,#31875,.F.);
#45959=ORIENTED_EDGE('',*,*,#31877,.F.);
#45960=ORIENTED_EDGE('',*,*,#31878,.F.);
#45961=ORIENTED_EDGE('',*,*,#31877,.T.);
#45962=ORIENTED_EDGE('',*,*,#31874,.F.);
#45963=ORIENTED_EDGE('',*,*,#31879,.T.);
#45964=ORIENTED_EDGE('',*,*,#31880,.F.);
#45965=ORIENTED_EDGE('',*,*,#31879,.F.);
#45966=ORIENTED_EDGE('',*,*,#31873,.F.);
#45967=ORIENTED_EDGE('',*,*,#31881,.F.);
#45968=ORIENTED_EDGE('',*,*,#31882,.T.);
#45969=ORIENTED_EDGE('',*,*,#31883,.T.);
#45970=ORIENTED_EDGE('',*,*,#31884,.T.);
#45971=ORIENTED_EDGE('',*,*,#31885,.F.);
#45972=ORIENTED_EDGE('',*,*,#31884,.F.);
#45973=ORIENTED_EDGE('',*,*,#31886,.F.);
#45974=ORIENTED_EDGE('',*,*,#31887,.F.);
#45975=ORIENTED_EDGE('',*,*,#31888,.F.);
#45976=ORIENTED_EDGE('',*,*,#31886,.T.);
#45977=ORIENTED_EDGE('',*,*,#31883,.F.);
#45978=ORIENTED_EDGE('',*,*,#31889,.T.);
#45979=ORIENTED_EDGE('',*,*,#31890,.F.);
#45980=ORIENTED_EDGE('',*,*,#31889,.F.);
#45981=ORIENTED_EDGE('',*,*,#31882,.F.);
#45982=ORIENTED_EDGE('',*,*,#31891,.F.);
#45983=ORIENTED_EDGE('',*,*,#31892,.F.);
#45984=ORIENTED_EDGE('',*,*,#31893,.T.);
#45985=ORIENTED_EDGE('',*,*,#31894,.T.);
#45986=ORIENTED_EDGE('',*,*,#31895,.T.);
#45987=ORIENTED_EDGE('',*,*,#31896,.F.);
#45988=ORIENTED_EDGE('',*,*,#31895,.F.);
#45989=ORIENTED_EDGE('',*,*,#31897,.F.);
#45990=ORIENTED_EDGE('',*,*,#31898,.F.);
#45991=ORIENTED_EDGE('',*,*,#31897,.T.);
#45992=ORIENTED_EDGE('',*,*,#31894,.F.);
#45993=ORIENTED_EDGE('',*,*,#31899,.T.);
#45994=ORIENTED_EDGE('',*,*,#31900,.F.);
#45995=ORIENTED_EDGE('',*,*,#31899,.F.);
#45996=ORIENTED_EDGE('',*,*,#31893,.F.);
#45997=ORIENTED_EDGE('',*,*,#31901,.F.);
#45998=ORIENTED_EDGE('',*,*,#31902,.T.);
#45999=ORIENTED_EDGE('',*,*,#31903,.T.);
#46000=ORIENTED_EDGE('',*,*,#31904,.T.);
#46001=ORIENTED_EDGE('',*,*,#31905,.F.);
#46002=ORIENTED_EDGE('',*,*,#31904,.F.);
#46003=ORIENTED_EDGE('',*,*,#31906,.F.);
#46004=ORIENTED_EDGE('',*,*,#31907,.F.);
#46005=ORIENTED_EDGE('',*,*,#31906,.T.);
#46006=ORIENTED_EDGE('',*,*,#31903,.F.);
#46007=ORIENTED_EDGE('',*,*,#31908,.T.);
#46008=ORIENTED_EDGE('',*,*,#31909,.F.);
#46009=ORIENTED_EDGE('',*,*,#31908,.F.);
#46010=ORIENTED_EDGE('',*,*,#31902,.F.);
#46011=ORIENTED_EDGE('',*,*,#31910,.F.);
#46012=ORIENTED_EDGE('',*,*,#31911,.T.);
#46013=ORIENTED_EDGE('',*,*,#31912,.T.);
#46014=ORIENTED_EDGE('',*,*,#31913,.T.);
#46015=ORIENTED_EDGE('',*,*,#31914,.F.);
#46016=ORIENTED_EDGE('',*,*,#31913,.F.);
#46017=ORIENTED_EDGE('',*,*,#31915,.F.);
#46018=ORIENTED_EDGE('',*,*,#31916,.F.);
#46019=ORIENTED_EDGE('',*,*,#31915,.T.);
#46020=ORIENTED_EDGE('',*,*,#31912,.F.);
#46021=ORIENTED_EDGE('',*,*,#31917,.T.);
#46022=ORIENTED_EDGE('',*,*,#31918,.F.);
#46023=ORIENTED_EDGE('',*,*,#31917,.F.);
#46024=ORIENTED_EDGE('',*,*,#31911,.F.);
#46025=ORIENTED_EDGE('',*,*,#31919,.F.);
#46026=ORIENTED_EDGE('',*,*,#31920,.T.);
#46027=ORIENTED_EDGE('',*,*,#31921,.T.);
#46028=ORIENTED_EDGE('',*,*,#31922,.T.);
#46029=ORIENTED_EDGE('',*,*,#31923,.F.);
#46030=ORIENTED_EDGE('',*,*,#31922,.F.);
#46031=ORIENTED_EDGE('',*,*,#31924,.F.);
#46032=ORIENTED_EDGE('',*,*,#31925,.F.);
#46033=ORIENTED_EDGE('',*,*,#31924,.T.);
#46034=ORIENTED_EDGE('',*,*,#31921,.F.);
#46035=ORIENTED_EDGE('',*,*,#31926,.T.);
#46036=ORIENTED_EDGE('',*,*,#31927,.F.);
#46037=ORIENTED_EDGE('',*,*,#31926,.F.);
#46038=ORIENTED_EDGE('',*,*,#31920,.F.);
#46039=ORIENTED_EDGE('',*,*,#31928,.F.);
#46040=ORIENTED_EDGE('',*,*,#31929,.T.);
#46041=ORIENTED_EDGE('',*,*,#31930,.T.);
#46042=ORIENTED_EDGE('',*,*,#31931,.T.);
#46043=ORIENTED_EDGE('',*,*,#31932,.F.);
#46044=ORIENTED_EDGE('',*,*,#31931,.F.);
#46045=ORIENTED_EDGE('',*,*,#31933,.F.);
#46046=ORIENTED_EDGE('',*,*,#31934,.F.);
#46047=ORIENTED_EDGE('',*,*,#31933,.T.);
#46048=ORIENTED_EDGE('',*,*,#31930,.F.);
#46049=ORIENTED_EDGE('',*,*,#31935,.T.);
#46050=ORIENTED_EDGE('',*,*,#31936,.F.);
#46051=ORIENTED_EDGE('',*,*,#31935,.F.);
#46052=ORIENTED_EDGE('',*,*,#31929,.F.);
#46053=ORIENTED_EDGE('',*,*,#31937,.F.);
#46054=ORIENTED_EDGE('',*,*,#31938,.T.);
#46055=ORIENTED_EDGE('',*,*,#31939,.T.);
#46056=ORIENTED_EDGE('',*,*,#31940,.T.);
#46057=ORIENTED_EDGE('',*,*,#31941,.F.);
#46058=ORIENTED_EDGE('',*,*,#31940,.F.);
#46059=ORIENTED_EDGE('',*,*,#31942,.F.);
#46060=ORIENTED_EDGE('',*,*,#31943,.F.);
#46061=ORIENTED_EDGE('',*,*,#31942,.T.);
#46062=ORIENTED_EDGE('',*,*,#31939,.F.);
#46063=ORIENTED_EDGE('',*,*,#31944,.T.);
#46064=ORIENTED_EDGE('',*,*,#31945,.F.);
#46065=ORIENTED_EDGE('',*,*,#31944,.F.);
#46066=ORIENTED_EDGE('',*,*,#31938,.F.);
#46067=ORIENTED_EDGE('',*,*,#31946,.F.);
#46068=ORIENTED_EDGE('',*,*,#31947,.T.);
#46069=ORIENTED_EDGE('',*,*,#31948,.T.);
#46070=ORIENTED_EDGE('',*,*,#31949,.T.);
#46071=ORIENTED_EDGE('',*,*,#31950,.F.);
#46072=ORIENTED_EDGE('',*,*,#31949,.F.);
#46073=ORIENTED_EDGE('',*,*,#31951,.F.);
#46074=ORIENTED_EDGE('',*,*,#31952,.F.);
#46075=ORIENTED_EDGE('',*,*,#31951,.T.);
#46076=ORIENTED_EDGE('',*,*,#31948,.F.);
#46077=ORIENTED_EDGE('',*,*,#31953,.T.);
#46078=ORIENTED_EDGE('',*,*,#31954,.F.);
#46079=ORIENTED_EDGE('',*,*,#31953,.F.);
#46080=ORIENTED_EDGE('',*,*,#31947,.F.);
#46081=ORIENTED_EDGE('',*,*,#31955,.F.);
#46082=ORIENTED_EDGE('',*,*,#31956,.T.);
#46083=ORIENTED_EDGE('',*,*,#31957,.T.);
#46084=ORIENTED_EDGE('',*,*,#31958,.T.);
#46085=ORIENTED_EDGE('',*,*,#31959,.F.);
#46086=ORIENTED_EDGE('',*,*,#31958,.F.);
#46087=ORIENTED_EDGE('',*,*,#31960,.F.);
#46088=ORIENTED_EDGE('',*,*,#31961,.F.);
#46089=ORIENTED_EDGE('',*,*,#31960,.T.);
#46090=ORIENTED_EDGE('',*,*,#31957,.F.);
#46091=ORIENTED_EDGE('',*,*,#31962,.T.);
#46092=ORIENTED_EDGE('',*,*,#31963,.F.);
#46093=ORIENTED_EDGE('',*,*,#31962,.F.);
#46094=ORIENTED_EDGE('',*,*,#31956,.F.);
#46095=ORIENTED_EDGE('',*,*,#31964,.F.);
#46096=ORIENTED_EDGE('',*,*,#31965,.T.);
#46097=ORIENTED_EDGE('',*,*,#31966,.T.);
#46098=ORIENTED_EDGE('',*,*,#31967,.T.);
#46099=ORIENTED_EDGE('',*,*,#31968,.F.);
#46100=ORIENTED_EDGE('',*,*,#31967,.F.);
#46101=ORIENTED_EDGE('',*,*,#31969,.F.);
#46102=ORIENTED_EDGE('',*,*,#31970,.F.);
#46103=ORIENTED_EDGE('',*,*,#31969,.T.);
#46104=ORIENTED_EDGE('',*,*,#31966,.F.);
#46105=ORIENTED_EDGE('',*,*,#31971,.T.);
#46106=ORIENTED_EDGE('',*,*,#31972,.F.);
#46107=ORIENTED_EDGE('',*,*,#31971,.F.);
#46108=ORIENTED_EDGE('',*,*,#31965,.F.);
#46109=ORIENTED_EDGE('',*,*,#31973,.F.);
#46110=ORIENTED_EDGE('',*,*,#31974,.T.);
#46111=ORIENTED_EDGE('',*,*,#31975,.T.);
#46112=ORIENTED_EDGE('',*,*,#31976,.T.);
#46113=ORIENTED_EDGE('',*,*,#31977,.F.);
#46114=ORIENTED_EDGE('',*,*,#31976,.F.);
#46115=ORIENTED_EDGE('',*,*,#31978,.F.);
#46116=ORIENTED_EDGE('',*,*,#31979,.F.);
#46117=ORIENTED_EDGE('',*,*,#31978,.T.);
#46118=ORIENTED_EDGE('',*,*,#31975,.F.);
#46119=ORIENTED_EDGE('',*,*,#31980,.T.);
#46120=ORIENTED_EDGE('',*,*,#31981,.F.);
#46121=ORIENTED_EDGE('',*,*,#31980,.F.);
#46122=ORIENTED_EDGE('',*,*,#31974,.F.);
#46123=ORIENTED_EDGE('',*,*,#31982,.F.);
#46124=ORIENTED_EDGE('',*,*,#31983,.T.);
#46125=ORIENTED_EDGE('',*,*,#31984,.T.);
#46126=ORIENTED_EDGE('',*,*,#31985,.T.);
#46127=ORIENTED_EDGE('',*,*,#31986,.F.);
#46128=ORIENTED_EDGE('',*,*,#31985,.F.);
#46129=ORIENTED_EDGE('',*,*,#31987,.F.);
#46130=ORIENTED_EDGE('',*,*,#31988,.F.);
#46131=ORIENTED_EDGE('',*,*,#31987,.T.);
#46132=ORIENTED_EDGE('',*,*,#31984,.F.);
#46133=ORIENTED_EDGE('',*,*,#31989,.T.);
#46134=ORIENTED_EDGE('',*,*,#31990,.F.);
#46135=ORIENTED_EDGE('',*,*,#31989,.F.);
#46136=ORIENTED_EDGE('',*,*,#31983,.F.);
#46137=ORIENTED_EDGE('',*,*,#31991,.F.);
#46138=ORIENTED_EDGE('',*,*,#31992,.T.);
#46139=ORIENTED_EDGE('',*,*,#31993,.T.);
#46140=ORIENTED_EDGE('',*,*,#31994,.T.);
#46141=ORIENTED_EDGE('',*,*,#31995,.F.);
#46142=ORIENTED_EDGE('',*,*,#31994,.F.);
#46143=ORIENTED_EDGE('',*,*,#31996,.F.);
#46144=ORIENTED_EDGE('',*,*,#31997,.F.);
#46145=ORIENTED_EDGE('',*,*,#31996,.T.);
#46146=ORIENTED_EDGE('',*,*,#31993,.F.);
#46147=ORIENTED_EDGE('',*,*,#31998,.T.);
#46148=ORIENTED_EDGE('',*,*,#31999,.F.);
#46149=ORIENTED_EDGE('',*,*,#31998,.F.);
#46150=ORIENTED_EDGE('',*,*,#31992,.F.);
#46151=ORIENTED_EDGE('',*,*,#32000,.F.);
#46152=ORIENTED_EDGE('',*,*,#32001,.T.);
#46153=ORIENTED_EDGE('',*,*,#32002,.T.);
#46154=ORIENTED_EDGE('',*,*,#32003,.T.);
#46155=ORIENTED_EDGE('',*,*,#32004,.F.);
#46156=ORIENTED_EDGE('',*,*,#32003,.F.);
#46157=ORIENTED_EDGE('',*,*,#32005,.F.);
#46158=ORIENTED_EDGE('',*,*,#32006,.F.);
#46159=ORIENTED_EDGE('',*,*,#32005,.T.);
#46160=ORIENTED_EDGE('',*,*,#32002,.F.);
#46161=ORIENTED_EDGE('',*,*,#32007,.T.);
#46162=ORIENTED_EDGE('',*,*,#32008,.F.);
#46163=ORIENTED_EDGE('',*,*,#32007,.F.);
#46164=ORIENTED_EDGE('',*,*,#32001,.F.);
#46165=ORIENTED_EDGE('',*,*,#32009,.F.);
#46166=ORIENTED_EDGE('',*,*,#32010,.T.);
#46167=ORIENTED_EDGE('',*,*,#32011,.T.);
#46168=ORIENTED_EDGE('',*,*,#32012,.T.);
#46169=ORIENTED_EDGE('',*,*,#32013,.F.);
#46170=ORIENTED_EDGE('',*,*,#32012,.F.);
#46171=ORIENTED_EDGE('',*,*,#32014,.F.);
#46172=ORIENTED_EDGE('',*,*,#32015,.F.);
#46173=ORIENTED_EDGE('',*,*,#32014,.T.);
#46174=ORIENTED_EDGE('',*,*,#32011,.F.);
#46175=ORIENTED_EDGE('',*,*,#32016,.T.);
#46176=ORIENTED_EDGE('',*,*,#32017,.F.);
#46177=ORIENTED_EDGE('',*,*,#32016,.F.);
#46178=ORIENTED_EDGE('',*,*,#32010,.F.);
#46179=ORIENTED_EDGE('',*,*,#32018,.F.);
#46180=ORIENTED_EDGE('',*,*,#32019,.T.);
#46181=ORIENTED_EDGE('',*,*,#32020,.T.);
#46182=ORIENTED_EDGE('',*,*,#32021,.T.);
#46183=ORIENTED_EDGE('',*,*,#32022,.F.);
#46184=ORIENTED_EDGE('',*,*,#32021,.F.);
#46185=ORIENTED_EDGE('',*,*,#32023,.F.);
#46186=ORIENTED_EDGE('',*,*,#32024,.F.);
#46187=ORIENTED_EDGE('',*,*,#32023,.T.);
#46188=ORIENTED_EDGE('',*,*,#32020,.F.);
#46189=ORIENTED_EDGE('',*,*,#32025,.T.);
#46190=ORIENTED_EDGE('',*,*,#32026,.F.);
#46191=ORIENTED_EDGE('',*,*,#32025,.F.);
#46192=ORIENTED_EDGE('',*,*,#32019,.F.);
#46193=ORIENTED_EDGE('',*,*,#32027,.F.);
#46194=ORIENTED_EDGE('',*,*,#32028,.T.);
#46195=ORIENTED_EDGE('',*,*,#32029,.T.);
#46196=ORIENTED_EDGE('',*,*,#32030,.T.);
#46197=ORIENTED_EDGE('',*,*,#32031,.F.);
#46198=ORIENTED_EDGE('',*,*,#32030,.F.);
#46199=ORIENTED_EDGE('',*,*,#32032,.F.);
#46200=ORIENTED_EDGE('',*,*,#32033,.F.);
#46201=ORIENTED_EDGE('',*,*,#32032,.T.);
#46202=ORIENTED_EDGE('',*,*,#32029,.F.);
#46203=ORIENTED_EDGE('',*,*,#32034,.T.);
#46204=ORIENTED_EDGE('',*,*,#32035,.F.);
#46205=ORIENTED_EDGE('',*,*,#32034,.F.);
#46206=ORIENTED_EDGE('',*,*,#32028,.F.);
#46207=ORIENTED_EDGE('',*,*,#32036,.F.);
#46208=ORIENTED_EDGE('',*,*,#32037,.T.);
#46209=ORIENTED_EDGE('',*,*,#32038,.T.);
#46210=ORIENTED_EDGE('',*,*,#32039,.T.);
#46211=ORIENTED_EDGE('',*,*,#32040,.F.);
#46212=ORIENTED_EDGE('',*,*,#32039,.F.);
#46213=ORIENTED_EDGE('',*,*,#32041,.F.);
#46214=ORIENTED_EDGE('',*,*,#32042,.F.);
#46215=ORIENTED_EDGE('',*,*,#32041,.T.);
#46216=ORIENTED_EDGE('',*,*,#32038,.F.);
#46217=ORIENTED_EDGE('',*,*,#32043,.T.);
#46218=ORIENTED_EDGE('',*,*,#32044,.F.);
#46219=ORIENTED_EDGE('',*,*,#32043,.F.);
#46220=ORIENTED_EDGE('',*,*,#32037,.F.);
#46221=ORIENTED_EDGE('',*,*,#32045,.F.);
#46222=ORIENTED_EDGE('',*,*,#32046,.F.);
#46223=ORIENTED_EDGE('',*,*,#32047,.F.);
#46224=ORIENTED_EDGE('',*,*,#32048,.F.);
#46225=ORIENTED_EDGE('',*,*,#32049,.T.);
#46226=ORIENTED_EDGE('',*,*,#32050,.T.);
#46227=ORIENTED_EDGE('',*,*,#32046,.T.);
#46228=ORIENTED_EDGE('',*,*,#32051,.F.);
#46229=ORIENTED_EDGE('',*,*,#32047,.T.);
#46230=ORIENTED_EDGE('',*,*,#32050,.F.);
#46231=ORIENTED_EDGE('',*,*,#32052,.T.);
#46232=ORIENTED_EDGE('',*,*,#32053,.F.);
#46233=ORIENTED_EDGE('',*,*,#32052,.F.);
#46234=ORIENTED_EDGE('',*,*,#32049,.F.);
#46235=ORIENTED_EDGE('',*,*,#32054,.T.);
#46236=ORIENTED_EDGE('',*,*,#32055,.F.);
#46237=ORIENTED_EDGE('',*,*,#32054,.F.);
#46238=ORIENTED_EDGE('',*,*,#32056,.F.);
#46239=ORIENTED_EDGE('',*,*,#32057,.F.);
#46240=ORIENTED_EDGE('',*,*,#32058,.F.);
#46241=ORIENTED_EDGE('',*,*,#32059,.T.);
#46242=ORIENTED_EDGE('',*,*,#32060,.F.);
#46243=ORIENTED_EDGE('',*,*,#32059,.F.);
#46244=ORIENTED_EDGE('',*,*,#32061,.F.);
#46245=ORIENTED_EDGE('',*,*,#32062,.T.);
#46246=ORIENTED_EDGE('',*,*,#32063,.F.);
#46247=ORIENTED_EDGE('',*,*,#32062,.F.);
#46248=ORIENTED_EDGE('',*,*,#32064,.F.);
#46249=ORIENTED_EDGE('',*,*,#32065,.T.);
#46250=ORIENTED_EDGE('',*,*,#32066,.F.);
#46251=ORIENTED_EDGE('',*,*,#32065,.F.);
#46252=ORIENTED_EDGE('',*,*,#32067,.F.);
#46253=ORIENTED_EDGE('',*,*,#32068,.T.);
#46254=ORIENTED_EDGE('',*,*,#32069,.F.);
#46255=ORIENTED_EDGE('',*,*,#32068,.F.);
#46256=ORIENTED_EDGE('',*,*,#32070,.F.);
#46257=ORIENTED_EDGE('',*,*,#32071,.T.);
#46258=ORIENTED_EDGE('',*,*,#32072,.F.);
#46259=ORIENTED_EDGE('',*,*,#32071,.F.);
#46260=ORIENTED_EDGE('',*,*,#32073,.F.);
#46261=ORIENTED_EDGE('',*,*,#32057,.T.);
#46262=ORIENTED_EDGE('',*,*,#32064,.T.);
#46263=ORIENTED_EDGE('',*,*,#32061,.T.);
#46264=ORIENTED_EDGE('',*,*,#32058,.T.);
#46265=ORIENTED_EDGE('',*,*,#32073,.T.);
#46266=ORIENTED_EDGE('',*,*,#32070,.T.);
#46267=ORIENTED_EDGE('',*,*,#32067,.T.);
#46268=ORIENTED_EDGE('',*,*,#32055,.T.);
#46269=ORIENTED_EDGE('',*,*,#32074,.F.);
#46270=ORIENTED_EDGE('',*,*,#31718,.F.);
#46271=ORIENTED_EDGE('',*,*,#31615,.F.);
#46272=ORIENTED_EDGE('',*,*,#31719,.F.);
#46273=ORIENTED_EDGE('',*,*,#32075,.T.);
#46274=ORIENTED_EDGE('',*,*,#32074,.T.);
#46275=ORIENTED_EDGE('',*,*,#32075,.F.);
#46276=ORIENTED_EDGE('',*,*,#31728,.T.);
#46277=ORIENTED_EDGE('',*,*,#32076,.F.);
#46278=ORIENTED_EDGE('',*,*,#31743,.T.);
#46279=ORIENTED_EDGE('',*,*,#31745,.T.);
#46280=ORIENTED_EDGE('',*,*,#31737,.T.);
#46281=ORIENTED_EDGE('',*,*,#32077,.F.);
#46282=ORIENTED_EDGE('',*,*,#31752,.T.);
#46283=ORIENTED_EDGE('',*,*,#31754,.T.);
#46284=ORIENTED_EDGE('',*,*,#31746,.T.);
#46285=ORIENTED_EDGE('',*,*,#32078,.F.);
#46286=ORIENTED_EDGE('',*,*,#31761,.T.);
#46287=ORIENTED_EDGE('',*,*,#31763,.T.);
#46288=ORIENTED_EDGE('',*,*,#31755,.T.);
#46289=ORIENTED_EDGE('',*,*,#32079,.F.);
#46290=ORIENTED_EDGE('',*,*,#31770,.T.);
#46291=ORIENTED_EDGE('',*,*,#31772,.T.);
#46292=ORIENTED_EDGE('',*,*,#31764,.T.);
#46293=ORIENTED_EDGE('',*,*,#32080,.F.);
#46294=ORIENTED_EDGE('',*,*,#31779,.T.);
#46295=ORIENTED_EDGE('',*,*,#31781,.T.);
#46296=ORIENTED_EDGE('',*,*,#31773,.T.);
#46297=ORIENTED_EDGE('',*,*,#32081,.F.);
#46298=ORIENTED_EDGE('',*,*,#31788,.T.);
#46299=ORIENTED_EDGE('',*,*,#31790,.T.);
#46300=ORIENTED_EDGE('',*,*,#31782,.T.);
#46301=ORIENTED_EDGE('',*,*,#32082,.F.);
#46302=ORIENTED_EDGE('',*,*,#31797,.T.);
#46303=ORIENTED_EDGE('',*,*,#31799,.T.);
#46304=ORIENTED_EDGE('',*,*,#31791,.T.);
#46305=ORIENTED_EDGE('',*,*,#32083,.F.);
#46306=ORIENTED_EDGE('',*,*,#31806,.T.);
#46307=ORIENTED_EDGE('',*,*,#31808,.T.);
#46308=ORIENTED_EDGE('',*,*,#31800,.T.);
#46309=ORIENTED_EDGE('',*,*,#32084,.F.);
#46310=ORIENTED_EDGE('',*,*,#31815,.T.);
#46311=ORIENTED_EDGE('',*,*,#31817,.T.);
#46312=ORIENTED_EDGE('',*,*,#31809,.T.);
#46313=ORIENTED_EDGE('',*,*,#32085,.F.);
#46314=ORIENTED_EDGE('',*,*,#31824,.T.);
#46315=ORIENTED_EDGE('',*,*,#31826,.T.);
#46316=ORIENTED_EDGE('',*,*,#31818,.T.);
#46317=ORIENTED_EDGE('',*,*,#32086,.F.);
#46318=ORIENTED_EDGE('',*,*,#31833,.T.);
#46319=ORIENTED_EDGE('',*,*,#31835,.T.);
#46320=ORIENTED_EDGE('',*,*,#31827,.T.);
#46321=ORIENTED_EDGE('',*,*,#32087,.F.);
#46322=ORIENTED_EDGE('',*,*,#31842,.T.);
#46323=ORIENTED_EDGE('',*,*,#31844,.T.);
#46324=ORIENTED_EDGE('',*,*,#31836,.T.);
#46325=ORIENTED_EDGE('',*,*,#32088,.F.);
#46326=ORIENTED_EDGE('',*,*,#31851,.T.);
#46327=ORIENTED_EDGE('',*,*,#31853,.T.);
#46328=ORIENTED_EDGE('',*,*,#31845,.T.);
#46329=ORIENTED_EDGE('',*,*,#32089,.F.);
#46330=ORIENTED_EDGE('',*,*,#31860,.T.);
#46331=ORIENTED_EDGE('',*,*,#31862,.T.);
#46332=ORIENTED_EDGE('',*,*,#31854,.T.);
#46333=ORIENTED_EDGE('',*,*,#32090,.F.);
#46334=ORIENTED_EDGE('',*,*,#31869,.T.);
#46335=ORIENTED_EDGE('',*,*,#31871,.T.);
#46336=ORIENTED_EDGE('',*,*,#31863,.T.);
#46337=ORIENTED_EDGE('',*,*,#32091,.F.);
#46338=ORIENTED_EDGE('',*,*,#31878,.T.);
#46339=ORIENTED_EDGE('',*,*,#31880,.T.);
#46340=ORIENTED_EDGE('',*,*,#31872,.T.);
#46341=ORIENTED_EDGE('',*,*,#32092,.F.);
#46342=ORIENTED_EDGE('',*,*,#31888,.T.);
#46343=ORIENTED_EDGE('',*,*,#31890,.T.);
#46344=ORIENTED_EDGE('',*,*,#32093,.T.);
#46345=ORIENTED_EDGE('',*,*,#31727,.T.);
#46346=ORIENTED_EDGE('',*,*,#32093,.F.);
#46347=ORIENTED_EDGE('',*,*,#31891,.T.);
#46348=ORIENTED_EDGE('',*,*,#31881,.T.);
#46349=ORIENTED_EDGE('',*,*,#32094,.F.);
#46350=ORIENTED_EDGE('',*,*,#31898,.T.);
#46351=ORIENTED_EDGE('',*,*,#31900,.T.);
#46352=ORIENTED_EDGE('',*,*,#31892,.T.);
#46353=ORIENTED_EDGE('',*,*,#32095,.F.);
#46354=ORIENTED_EDGE('',*,*,#31907,.T.);
#46355=ORIENTED_EDGE('',*,*,#31909,.T.);
#46356=ORIENTED_EDGE('',*,*,#31901,.T.);
#46357=ORIENTED_EDGE('',*,*,#32096,.F.);
#46358=ORIENTED_EDGE('',*,*,#31916,.T.);
#46359=ORIENTED_EDGE('',*,*,#31918,.T.);
#46360=ORIENTED_EDGE('',*,*,#31910,.T.);
#46361=ORIENTED_EDGE('',*,*,#32097,.F.);
#46362=ORIENTED_EDGE('',*,*,#31925,.T.);
#46363=ORIENTED_EDGE('',*,*,#31927,.T.);
#46364=ORIENTED_EDGE('',*,*,#31919,.T.);
#46365=ORIENTED_EDGE('',*,*,#32098,.F.);
#46366=ORIENTED_EDGE('',*,*,#31934,.T.);
#46367=ORIENTED_EDGE('',*,*,#31936,.T.);
#46368=ORIENTED_EDGE('',*,*,#31928,.T.);
#46369=ORIENTED_EDGE('',*,*,#32099,.F.);
#46370=ORIENTED_EDGE('',*,*,#31943,.T.);
#46371=ORIENTED_EDGE('',*,*,#31945,.T.);
#46372=ORIENTED_EDGE('',*,*,#31937,.T.);
#46373=ORIENTED_EDGE('',*,*,#32100,.F.);
#46374=ORIENTED_EDGE('',*,*,#31952,.T.);
#46375=ORIENTED_EDGE('',*,*,#31954,.T.);
#46376=ORIENTED_EDGE('',*,*,#31946,.T.);
#46377=ORIENTED_EDGE('',*,*,#32101,.F.);
#46378=ORIENTED_EDGE('',*,*,#31961,.T.);
#46379=ORIENTED_EDGE('',*,*,#31963,.T.);
#46380=ORIENTED_EDGE('',*,*,#31955,.T.);
#46381=ORIENTED_EDGE('',*,*,#32102,.F.);
#46382=ORIENTED_EDGE('',*,*,#31970,.T.);
#46383=ORIENTED_EDGE('',*,*,#31972,.T.);
#46384=ORIENTED_EDGE('',*,*,#31964,.T.);
#46385=ORIENTED_EDGE('',*,*,#32103,.F.);
#46386=ORIENTED_EDGE('',*,*,#31979,.T.);
#46387=ORIENTED_EDGE('',*,*,#31981,.T.);
#46388=ORIENTED_EDGE('',*,*,#31973,.T.);
#46389=ORIENTED_EDGE('',*,*,#32104,.F.);
#46390=ORIENTED_EDGE('',*,*,#31988,.T.);
#46391=ORIENTED_EDGE('',*,*,#31990,.T.);
#46392=ORIENTED_EDGE('',*,*,#31982,.T.);
#46393=ORIENTED_EDGE('',*,*,#32105,.F.);
#46394=ORIENTED_EDGE('',*,*,#31997,.T.);
#46395=ORIENTED_EDGE('',*,*,#31999,.T.);
#46396=ORIENTED_EDGE('',*,*,#31991,.T.);
#46397=ORIENTED_EDGE('',*,*,#32106,.F.);
#46398=ORIENTED_EDGE('',*,*,#32006,.T.);
#46399=ORIENTED_EDGE('',*,*,#32008,.T.);
#46400=ORIENTED_EDGE('',*,*,#32000,.T.);
#46401=ORIENTED_EDGE('',*,*,#32107,.F.);
#46402=ORIENTED_EDGE('',*,*,#32015,.T.);
#46403=ORIENTED_EDGE('',*,*,#32017,.T.);
#46404=ORIENTED_EDGE('',*,*,#32009,.T.);
#46405=ORIENTED_EDGE('',*,*,#32108,.F.);
#46406=ORIENTED_EDGE('',*,*,#32024,.T.);
#46407=ORIENTED_EDGE('',*,*,#32026,.T.);
#46408=ORIENTED_EDGE('',*,*,#32018,.T.);
#46409=ORIENTED_EDGE('',*,*,#32109,.F.);
#46410=ORIENTED_EDGE('',*,*,#32033,.T.);
#46411=ORIENTED_EDGE('',*,*,#32035,.T.);
#46412=ORIENTED_EDGE('',*,*,#32027,.T.);
#46413=ORIENTED_EDGE('',*,*,#32110,.F.);
#46414=ORIENTED_EDGE('',*,*,#32042,.T.);
#46415=ORIENTED_EDGE('',*,*,#32044,.T.);
#46416=ORIENTED_EDGE('',*,*,#32036,.T.);
#46417=ORIENTED_EDGE('',*,*,#32111,.F.);
#46418=ORIENTED_EDGE('',*,*,#32051,.T.);
#46419=ORIENTED_EDGE('',*,*,#32053,.T.);
#46420=ORIENTED_EDGE('',*,*,#32048,.T.);
#46421=ORIENTED_EDGE('',*,*,#32112,.F.);
#46422=ORIENTED_EDGE('',*,*,#31734,.T.);
#46423=ORIENTED_EDGE('',*,*,#31736,.T.);
#46424=ORIENTED_EDGE('',*,*,#32113,.F.);
#46425=ORIENTED_EDGE('',*,*,#32114,.T.);
#46426=ORIENTED_EDGE('',*,*,#31887,.T.);
#46427=ORIENTED_EDGE('',*,*,#32092,.T.);
#46428=ORIENTED_EDGE('',*,*,#31876,.T.);
#46429=ORIENTED_EDGE('',*,*,#32091,.T.);
#46430=ORIENTED_EDGE('',*,*,#31867,.T.);
#46431=ORIENTED_EDGE('',*,*,#32090,.T.);
#46432=ORIENTED_EDGE('',*,*,#31858,.T.);
#46433=ORIENTED_EDGE('',*,*,#32089,.T.);
#46434=ORIENTED_EDGE('',*,*,#31849,.T.);
#46435=ORIENTED_EDGE('',*,*,#32088,.T.);
#46436=ORIENTED_EDGE('',*,*,#31840,.T.);
#46437=ORIENTED_EDGE('',*,*,#32087,.T.);
#46438=ORIENTED_EDGE('',*,*,#31831,.T.);
#46439=ORIENTED_EDGE('',*,*,#32086,.T.);
#46440=ORIENTED_EDGE('',*,*,#31822,.T.);
#46441=ORIENTED_EDGE('',*,*,#32085,.T.);
#46442=ORIENTED_EDGE('',*,*,#31813,.T.);
#46443=ORIENTED_EDGE('',*,*,#32084,.T.);
#46444=ORIENTED_EDGE('',*,*,#31804,.T.);
#46445=ORIENTED_EDGE('',*,*,#32083,.T.);
#46446=ORIENTED_EDGE('',*,*,#31795,.T.);
#46447=ORIENTED_EDGE('',*,*,#32082,.T.);
#46448=ORIENTED_EDGE('',*,*,#31786,.T.);
#46449=ORIENTED_EDGE('',*,*,#32081,.T.);
#46450=ORIENTED_EDGE('',*,*,#31777,.T.);
#46451=ORIENTED_EDGE('',*,*,#32080,.T.);
#46452=ORIENTED_EDGE('',*,*,#31768,.T.);
#46453=ORIENTED_EDGE('',*,*,#32079,.T.);
#46454=ORIENTED_EDGE('',*,*,#31759,.T.);
#46455=ORIENTED_EDGE('',*,*,#32078,.T.);
#46456=ORIENTED_EDGE('',*,*,#31750,.T.);
#46457=ORIENTED_EDGE('',*,*,#32077,.T.);
#46458=ORIENTED_EDGE('',*,*,#31741,.T.);
#46459=ORIENTED_EDGE('',*,*,#32076,.T.);
#46460=ORIENTED_EDGE('',*,*,#31732,.T.);
#46461=ORIENTED_EDGE('',*,*,#32112,.T.);
#46462=ORIENTED_EDGE('',*,*,#32045,.T.);
#46463=ORIENTED_EDGE('',*,*,#32111,.T.);
#46464=ORIENTED_EDGE('',*,*,#32040,.T.);
#46465=ORIENTED_EDGE('',*,*,#32110,.T.);
#46466=ORIENTED_EDGE('',*,*,#32031,.T.);
#46467=ORIENTED_EDGE('',*,*,#32109,.T.);
#46468=ORIENTED_EDGE('',*,*,#32022,.T.);
#46469=ORIENTED_EDGE('',*,*,#32108,.T.);
#46470=ORIENTED_EDGE('',*,*,#32013,.T.);
#46471=ORIENTED_EDGE('',*,*,#32107,.T.);
#46472=ORIENTED_EDGE('',*,*,#32004,.T.);
#46473=ORIENTED_EDGE('',*,*,#32106,.T.);
#46474=ORIENTED_EDGE('',*,*,#31995,.T.);
#46475=ORIENTED_EDGE('',*,*,#32105,.T.);
#46476=ORIENTED_EDGE('',*,*,#31986,.T.);
#46477=ORIENTED_EDGE('',*,*,#32104,.T.);
#46478=ORIENTED_EDGE('',*,*,#31977,.T.);
#46479=ORIENTED_EDGE('',*,*,#32103,.T.);
#46480=ORIENTED_EDGE('',*,*,#31968,.T.);
#46481=ORIENTED_EDGE('',*,*,#32102,.T.);
#46482=ORIENTED_EDGE('',*,*,#31959,.T.);
#46483=ORIENTED_EDGE('',*,*,#32101,.T.);
#46484=ORIENTED_EDGE('',*,*,#31950,.T.);
#46485=ORIENTED_EDGE('',*,*,#32100,.T.);
#46486=ORIENTED_EDGE('',*,*,#31941,.T.);
#46487=ORIENTED_EDGE('',*,*,#32099,.T.);
#46488=ORIENTED_EDGE('',*,*,#31932,.T.);
#46489=ORIENTED_EDGE('',*,*,#32098,.T.);
#46490=ORIENTED_EDGE('',*,*,#31923,.T.);
#46491=ORIENTED_EDGE('',*,*,#32097,.T.);
#46492=ORIENTED_EDGE('',*,*,#31914,.T.);
#46493=ORIENTED_EDGE('',*,*,#32096,.T.);
#46494=ORIENTED_EDGE('',*,*,#31905,.T.);
#46495=ORIENTED_EDGE('',*,*,#32095,.T.);
#46496=ORIENTED_EDGE('',*,*,#31896,.T.);
#46497=ORIENTED_EDGE('',*,*,#32094,.T.);
#46498=ORIENTED_EDGE('',*,*,#31885,.T.);
#46499=ORIENTED_EDGE('',*,*,#32114,.F.);
#46500=ORIENTED_EDGE('',*,*,#32113,.T.);
#46501=ORIENTED_EDGE('',*,*,#32066,.T.);
#46502=ORIENTED_EDGE('',*,*,#32069,.T.);
#46503=ORIENTED_EDGE('',*,*,#32072,.T.);
#46504=ORIENTED_EDGE('',*,*,#32056,.T.);
#46505=ORIENTED_EDGE('',*,*,#32060,.T.);
#46506=ORIENTED_EDGE('',*,*,#32063,.T.);
#46507=ORIENTED_EDGE('',*,*,#32115,.F.);
#46508=ORIENTED_EDGE('',*,*,#32116,.T.);
#46509=ORIENTED_EDGE('',*,*,#32117,.T.);
#46510=ORIENTED_EDGE('',*,*,#32116,.F.);
#46511=ORIENTED_EDGE('',*,*,#32118,.F.);
#46512=ORIENTED_EDGE('',*,*,#32119,.T.);
#46513=ORIENTED_EDGE('',*,*,#32115,.T.);
#46514=ORIENTED_EDGE('',*,*,#32119,.F.);
#46515=ORIENTED_EDGE('',*,*,#32120,.F.);
#46516=ORIENTED_EDGE('',*,*,#32121,.T.);
#46517=ORIENTED_EDGE('',*,*,#32118,.T.);
#46518=ORIENTED_EDGE('',*,*,#32121,.F.);
#46519=ORIENTED_EDGE('',*,*,#32120,.T.);
#46520=ORIENTED_EDGE('',*,*,#32122,.F.);
#46521=ORIENTED_EDGE('',*,*,#32122,.T.);
#46522=ORIENTED_EDGE('',*,*,#32123,.T.);
#46523=ORIENTED_EDGE('',*,*,#32124,.F.);
#46524=ORIENTED_EDGE('',*,*,#32123,.F.);
#46525=ORIENTED_EDGE('',*,*,#32124,.T.);
#46526=ORIENTED_EDGE('',*,*,#32125,.T.);
#46527=ORIENTED_EDGE('',*,*,#32126,.F.);
#46528=ORIENTED_EDGE('',*,*,#32125,.F.);
#46529=ORIENTED_EDGE('',*,*,#32126,.T.);
#46530=ORIENTED_EDGE('',*,*,#32127,.T.);
#46531=ORIENTED_EDGE('',*,*,#32128,.F.);
#46532=ORIENTED_EDGE('',*,*,#32127,.F.);
#46533=ORIENTED_EDGE('',*,*,#32117,.F.);
#46534=ORIENTED_EDGE('',*,*,#32128,.T.);
#46535=ORIENTED_EDGE('',*,*,#32129,.F.);
#46536=ORIENTED_EDGE('',*,*,#32130,.F.);
#46537=ORIENTED_EDGE('',*,*,#32131,.T.);
#46538=ORIENTED_EDGE('',*,*,#32132,.F.);
#46539=ORIENTED_EDGE('',*,*,#32133,.F.);
#46540=ORIENTED_EDGE('',*,*,#32134,.F.);
#46541=ORIENTED_EDGE('',*,*,#32135,.T.);
#46542=ORIENTED_EDGE('',*,*,#32136,.F.);
#46543=ORIENTED_EDGE('',*,*,#32137,.F.);
#46544=ORIENTED_EDGE('',*,*,#32138,.F.);
#46545=ORIENTED_EDGE('',*,*,#32139,.F.);
#46546=ORIENTED_EDGE('',*,*,#32140,.F.);
#46547=ORIENTED_EDGE('',*,*,#32141,.F.);
#46548=ORIENTED_EDGE('',*,*,#32142,.F.);
#46549=ORIENTED_EDGE('',*,*,#32143,.F.);
#46550=ORIENTED_EDGE('',*,*,#32131,.F.);
#46551=ORIENTED_EDGE('',*,*,#32144,.F.);
#46552=ORIENTED_EDGE('',*,*,#32145,.F.);
#46553=ORIENTED_EDGE('',*,*,#32146,.F.);
#46554=ORIENTED_EDGE('',*,*,#32147,.F.);
#46555=ORIENTED_EDGE('',*,*,#32148,.F.);
#46556=ORIENTED_EDGE('',*,*,#32135,.F.);
#46557=ORIENTED_EDGE('',*,*,#32149,.F.);
#46558=ORIENTED_EDGE('',*,*,#32150,.F.);
#46559=ORIENTED_EDGE('',*,*,#32141,.T.);
#46560=ORIENTED_EDGE('',*,*,#32151,.T.);
#46561=ORIENTED_EDGE('',*,*,#32136,.T.);
#46562=ORIENTED_EDGE('',*,*,#32148,.T.);
#46563=ORIENTED_EDGE('',*,*,#32152,.T.);
#46564=ORIENTED_EDGE('',*,*,#32133,.T.);
#46565=ORIENTED_EDGE('',*,*,#32151,.F.);
#46566=ORIENTED_EDGE('',*,*,#32140,.T.);
#46567=ORIENTED_EDGE('',*,*,#32153,.F.);
#46568=ORIENTED_EDGE('',*,*,#32139,.T.);
#46569=ORIENTED_EDGE('',*,*,#32154,.T.);
#46570=ORIENTED_EDGE('',*,*,#32149,.T.);
#46571=ORIENTED_EDGE('',*,*,#32134,.T.);
#46572=ORIENTED_EDGE('',*,*,#32153,.T.);
#46573=ORIENTED_EDGE('',*,*,#32138,.T.);
#46574=ORIENTED_EDGE('',*,*,#32155,.F.);
#46575=ORIENTED_EDGE('',*,*,#32150,.T.);
#46576=ORIENTED_EDGE('',*,*,#32154,.F.);
#46577=ORIENTED_EDGE('',*,*,#32137,.T.);
#46578=ORIENTED_EDGE('',*,*,#32130,.T.);
#46579=ORIENTED_EDGE('',*,*,#32156,.T.);
#46580=ORIENTED_EDGE('',*,*,#32144,.T.);
#46581=ORIENTED_EDGE('',*,*,#32155,.T.);
#46582=ORIENTED_EDGE('',*,*,#32129,.T.);
#46583=ORIENTED_EDGE('',*,*,#32157,.F.);
#46584=ORIENTED_EDGE('',*,*,#32145,.T.);
#46585=ORIENTED_EDGE('',*,*,#32156,.F.);
#46586=ORIENTED_EDGE('',*,*,#32143,.T.);
#46587=ORIENTED_EDGE('',*,*,#32158,.T.);
#46588=ORIENTED_EDGE('',*,*,#32146,.T.);
#46589=ORIENTED_EDGE('',*,*,#32157,.T.);
#46590=ORIENTED_EDGE('',*,*,#32132,.T.);
#46591=ORIENTED_EDGE('',*,*,#32142,.T.);
#46592=ORIENTED_EDGE('',*,*,#32152,.F.);
#46593=ORIENTED_EDGE('',*,*,#32147,.T.);
#46594=ORIENTED_EDGE('',*,*,#32158,.F.);
#46595=ORIENTED_EDGE('',*,*,#32159,.F.);
#46596=ORIENTED_EDGE('',*,*,#32160,.T.);
#46597=ORIENTED_EDGE('',*,*,#32161,.T.);
#46598=ORIENTED_EDGE('',*,*,#32162,.T.);
#46599=ORIENTED_EDGE('',*,*,#32163,.F.);
#46600=ORIENTED_EDGE('',*,*,#32164,.T.);
#46601=ORIENTED_EDGE('',*,*,#32159,.T.);
#46602=ORIENTED_EDGE('',*,*,#32165,.T.);
#46603=ORIENTED_EDGE('',*,*,#32166,.F.);
#46604=ORIENTED_EDGE('',*,*,#32167,.T.);
#46605=ORIENTED_EDGE('',*,*,#32163,.T.);
#46606=ORIENTED_EDGE('',*,*,#32168,.T.);
#46607=ORIENTED_EDGE('',*,*,#32169,.F.);
#46608=ORIENTED_EDGE('',*,*,#32170,.T.);
#46609=ORIENTED_EDGE('',*,*,#32166,.T.);
#46610=ORIENTED_EDGE('',*,*,#32171,.T.);
#46611=ORIENTED_EDGE('',*,*,#32172,.F.);
#46612=ORIENTED_EDGE('',*,*,#32173,.T.);
#46613=ORIENTED_EDGE('',*,*,#32169,.T.);
#46614=ORIENTED_EDGE('',*,*,#32174,.T.);
#46615=ORIENTED_EDGE('',*,*,#32175,.F.);
#46616=ORIENTED_EDGE('',*,*,#32176,.T.);
#46617=ORIENTED_EDGE('',*,*,#32172,.T.);
#46618=ORIENTED_EDGE('',*,*,#32177,.T.);
#46619=ORIENTED_EDGE('',*,*,#32178,.F.);
#46620=ORIENTED_EDGE('',*,*,#32179,.T.);
#46621=ORIENTED_EDGE('',*,*,#32175,.T.);
#46622=ORIENTED_EDGE('',*,*,#32180,.T.);
#46623=ORIENTED_EDGE('',*,*,#32181,.F.);
#46624=ORIENTED_EDGE('',*,*,#32182,.T.);
#46625=ORIENTED_EDGE('',*,*,#32178,.T.);
#46626=ORIENTED_EDGE('',*,*,#32183,.T.);
#46627=ORIENTED_EDGE('',*,*,#32184,.F.);
#46628=ORIENTED_EDGE('',*,*,#32185,.T.);
#46629=ORIENTED_EDGE('',*,*,#32181,.T.);
#46630=ORIENTED_EDGE('',*,*,#32186,.T.);
#46631=ORIENTED_EDGE('',*,*,#32187,.F.);
#46632=ORIENTED_EDGE('',*,*,#32188,.T.);
#46633=ORIENTED_EDGE('',*,*,#32184,.T.);
#46634=ORIENTED_EDGE('',*,*,#32189,.T.);
#46635=ORIENTED_EDGE('',*,*,#32190,.F.);
#46636=ORIENTED_EDGE('',*,*,#32191,.T.);
#46637=ORIENTED_EDGE('',*,*,#32187,.T.);
#46638=ORIENTED_EDGE('',*,*,#32192,.T.);
#46639=ORIENTED_EDGE('',*,*,#32193,.F.);
#46640=ORIENTED_EDGE('',*,*,#32194,.T.);
#46641=ORIENTED_EDGE('',*,*,#32190,.T.);
#46642=ORIENTED_EDGE('',*,*,#32195,.T.);
#46643=ORIENTED_EDGE('',*,*,#32196,.F.);
#46644=ORIENTED_EDGE('',*,*,#32197,.T.);
#46645=ORIENTED_EDGE('',*,*,#32193,.T.);
#46646=ORIENTED_EDGE('',*,*,#32198,.T.);
#46647=ORIENTED_EDGE('',*,*,#32199,.F.);
#46648=ORIENTED_EDGE('',*,*,#32200,.T.);
#46649=ORIENTED_EDGE('',*,*,#32196,.T.);
#46650=ORIENTED_EDGE('',*,*,#32201,.T.);
#46651=ORIENTED_EDGE('',*,*,#32202,.F.);
#46652=ORIENTED_EDGE('',*,*,#32203,.T.);
#46653=ORIENTED_EDGE('',*,*,#32199,.T.);
#46654=ORIENTED_EDGE('',*,*,#32204,.T.);
#46655=ORIENTED_EDGE('',*,*,#32205,.F.);
#46656=ORIENTED_EDGE('',*,*,#32206,.F.);
#46657=ORIENTED_EDGE('',*,*,#32207,.T.);
#46658=ORIENTED_EDGE('',*,*,#32202,.T.);
#46659=ORIENTED_EDGE('',*,*,#32208,.T.);
#46660=ORIENTED_EDGE('',*,*,#32209,.F.);
#46661=ORIENTED_EDGE('',*,*,#32210,.T.);
#46662=ORIENTED_EDGE('',*,*,#32211,.F.);
#46663=ORIENTED_EDGE('',*,*,#32212,.F.);
#46664=ORIENTED_EDGE('',*,*,#32213,.F.);
#46665=ORIENTED_EDGE('',*,*,#32214,.T.);
#46666=ORIENTED_EDGE('',*,*,#32209,.T.);
#46667=ORIENTED_EDGE('',*,*,#32215,.F.);
#46668=ORIENTED_EDGE('',*,*,#32216,.F.);
#46669=ORIENTED_EDGE('',*,*,#32217,.T.);
#46670=ORIENTED_EDGE('',*,*,#32213,.T.);
#46671=ORIENTED_EDGE('',*,*,#32218,.F.);
#46672=ORIENTED_EDGE('',*,*,#32219,.F.);
#46673=ORIENTED_EDGE('',*,*,#32220,.T.);
#46674=ORIENTED_EDGE('',*,*,#32216,.T.);
#46675=ORIENTED_EDGE('',*,*,#32221,.F.);
#46676=ORIENTED_EDGE('',*,*,#32222,.F.);
#46677=ORIENTED_EDGE('',*,*,#32223,.T.);
#46678=ORIENTED_EDGE('',*,*,#32219,.T.);
#46679=ORIENTED_EDGE('',*,*,#32224,.F.);
#46680=ORIENTED_EDGE('',*,*,#32225,.F.);
#46681=ORIENTED_EDGE('',*,*,#32226,.T.);
#46682=ORIENTED_EDGE('',*,*,#32222,.T.);
#46683=ORIENTED_EDGE('',*,*,#32227,.F.);
#46684=ORIENTED_EDGE('',*,*,#32228,.F.);
#46685=ORIENTED_EDGE('',*,*,#32229,.T.);
#46686=ORIENTED_EDGE('',*,*,#32225,.T.);
#46687=ORIENTED_EDGE('',*,*,#32230,.F.);
#46688=ORIENTED_EDGE('',*,*,#32231,.F.);
#46689=ORIENTED_EDGE('',*,*,#32232,.T.);
#46690=ORIENTED_EDGE('',*,*,#32228,.T.);
#46691=ORIENTED_EDGE('',*,*,#32233,.F.);
#46692=ORIENTED_EDGE('',*,*,#32234,.F.);
#46693=ORIENTED_EDGE('',*,*,#32235,.T.);
#46694=ORIENTED_EDGE('',*,*,#32231,.T.);
#46695=ORIENTED_EDGE('',*,*,#32236,.F.);
#46696=ORIENTED_EDGE('',*,*,#32237,.F.);
#46697=ORIENTED_EDGE('',*,*,#32238,.T.);
#46698=ORIENTED_EDGE('',*,*,#32234,.T.);
#46699=ORIENTED_EDGE('',*,*,#32239,.F.);
#46700=ORIENTED_EDGE('',*,*,#32240,.F.);
#46701=ORIENTED_EDGE('',*,*,#32241,.T.);
#46702=ORIENTED_EDGE('',*,*,#32237,.T.);
#46703=ORIENTED_EDGE('',*,*,#32242,.F.);
#46704=ORIENTED_EDGE('',*,*,#32243,.F.);
#46705=ORIENTED_EDGE('',*,*,#32244,.T.);
#46706=ORIENTED_EDGE('',*,*,#32240,.T.);
#46707=ORIENTED_EDGE('',*,*,#32245,.F.);
#46708=ORIENTED_EDGE('',*,*,#32246,.F.);
#46709=ORIENTED_EDGE('',*,*,#32247,.T.);
#46710=ORIENTED_EDGE('',*,*,#32243,.T.);
#46711=ORIENTED_EDGE('',*,*,#32248,.F.);
#46712=ORIENTED_EDGE('',*,*,#32249,.F.);
#46713=ORIENTED_EDGE('',*,*,#32250,.T.);
#46714=ORIENTED_EDGE('',*,*,#32246,.T.);
#46715=ORIENTED_EDGE('',*,*,#32251,.F.);
#46716=ORIENTED_EDGE('',*,*,#32252,.F.);
#46717=ORIENTED_EDGE('',*,*,#32253,.T.);
#46718=ORIENTED_EDGE('',*,*,#32249,.T.);
#46719=ORIENTED_EDGE('',*,*,#32254,.F.);
#46720=ORIENTED_EDGE('',*,*,#32211,.T.);
#46721=ORIENTED_EDGE('',*,*,#32255,.T.);
#46722=ORIENTED_EDGE('',*,*,#32256,.F.);
#46723=ORIENTED_EDGE('',*,*,#32257,.F.);
#46724=ORIENTED_EDGE('',*,*,#32258,.T.);
#46725=ORIENTED_EDGE('',*,*,#32258,.F.);
#46726=ORIENTED_EDGE('',*,*,#32259,.F.);
#46727=ORIENTED_EDGE('',*,*,#32208,.F.);
#46728=ORIENTED_EDGE('',*,*,#32204,.F.);
#46729=ORIENTED_EDGE('',*,*,#32201,.F.);
#46730=ORIENTED_EDGE('',*,*,#32198,.F.);
#46731=ORIENTED_EDGE('',*,*,#32195,.F.);
#46732=ORIENTED_EDGE('',*,*,#32192,.F.);
#46733=ORIENTED_EDGE('',*,*,#32189,.F.);
#46734=ORIENTED_EDGE('',*,*,#32186,.F.);
#46735=ORIENTED_EDGE('',*,*,#32183,.F.);
#46736=ORIENTED_EDGE('',*,*,#32180,.F.);
#46737=ORIENTED_EDGE('',*,*,#32177,.F.);
#46738=ORIENTED_EDGE('',*,*,#32174,.F.);
#46739=ORIENTED_EDGE('',*,*,#32171,.F.);
#46740=ORIENTED_EDGE('',*,*,#32168,.F.);
#46741=ORIENTED_EDGE('',*,*,#32165,.F.);
#46742=ORIENTED_EDGE('',*,*,#32162,.F.);
#46743=ORIENTED_EDGE('',*,*,#32260,.F.);
#46744=ORIENTED_EDGE('',*,*,#32261,.T.);
#46745=ORIENTED_EDGE('',*,*,#32254,.T.);
#46746=ORIENTED_EDGE('',*,*,#32251,.T.);
#46747=ORIENTED_EDGE('',*,*,#32248,.T.);
#46748=ORIENTED_EDGE('',*,*,#32245,.T.);
#46749=ORIENTED_EDGE('',*,*,#32242,.T.);
#46750=ORIENTED_EDGE('',*,*,#32239,.T.);
#46751=ORIENTED_EDGE('',*,*,#32236,.T.);
#46752=ORIENTED_EDGE('',*,*,#32233,.T.);
#46753=ORIENTED_EDGE('',*,*,#32230,.T.);
#46754=ORIENTED_EDGE('',*,*,#32227,.T.);
#46755=ORIENTED_EDGE('',*,*,#32224,.T.);
#46756=ORIENTED_EDGE('',*,*,#32221,.T.);
#46757=ORIENTED_EDGE('',*,*,#32218,.T.);
#46758=ORIENTED_EDGE('',*,*,#32215,.T.);
#46759=ORIENTED_EDGE('',*,*,#32212,.T.);
#46760=ORIENTED_EDGE('',*,*,#32262,.T.);
#46761=ORIENTED_EDGE('',*,*,#32263,.T.);
#46762=ORIENTED_EDGE('',*,*,#32264,.T.);
#46763=ORIENTED_EDGE('',*,*,#32265,.T.);
#46764=ORIENTED_EDGE('',*,*,#32260,.T.);
#46765=ORIENTED_EDGE('',*,*,#32252,.T.);
#46766=ORIENTED_EDGE('',*,*,#32261,.F.);
#46767=ORIENTED_EDGE('',*,*,#32265,.F.);
#46768=ORIENTED_EDGE('',*,*,#32266,.T.);
#46769=ORIENTED_EDGE('',*,*,#32255,.F.);
#46770=ORIENTED_EDGE('',*,*,#32210,.F.);
#46771=ORIENTED_EDGE('',*,*,#32214,.F.);
#46772=ORIENTED_EDGE('',*,*,#32217,.F.);
#46773=ORIENTED_EDGE('',*,*,#32220,.F.);
#46774=ORIENTED_EDGE('',*,*,#32223,.F.);
#46775=ORIENTED_EDGE('',*,*,#32226,.F.);
#46776=ORIENTED_EDGE('',*,*,#32229,.F.);
#46777=ORIENTED_EDGE('',*,*,#32232,.F.);
#46778=ORIENTED_EDGE('',*,*,#32235,.F.);
#46779=ORIENTED_EDGE('',*,*,#32238,.F.);
#46780=ORIENTED_EDGE('',*,*,#32241,.F.);
#46781=ORIENTED_EDGE('',*,*,#32244,.F.);
#46782=ORIENTED_EDGE('',*,*,#32247,.F.);
#46783=ORIENTED_EDGE('',*,*,#32250,.F.);
#46784=ORIENTED_EDGE('',*,*,#32253,.F.);
#46785=ORIENTED_EDGE('',*,*,#32266,.F.);
#46786=ORIENTED_EDGE('',*,*,#32264,.F.);
#46787=ORIENTED_EDGE('',*,*,#32160,.F.);
#46788=ORIENTED_EDGE('',*,*,#32164,.F.);
#46789=ORIENTED_EDGE('',*,*,#32167,.F.);
#46790=ORIENTED_EDGE('',*,*,#32170,.F.);
#46791=ORIENTED_EDGE('',*,*,#32173,.F.);
#46792=ORIENTED_EDGE('',*,*,#32176,.F.);
#46793=ORIENTED_EDGE('',*,*,#32179,.F.);
#46794=ORIENTED_EDGE('',*,*,#32182,.F.);
#46795=ORIENTED_EDGE('',*,*,#32185,.F.);
#46796=ORIENTED_EDGE('',*,*,#32188,.F.);
#46797=ORIENTED_EDGE('',*,*,#32191,.F.);
#46798=ORIENTED_EDGE('',*,*,#32194,.F.);
#46799=ORIENTED_EDGE('',*,*,#32197,.F.);
#46800=ORIENTED_EDGE('',*,*,#32200,.F.);
#46801=ORIENTED_EDGE('',*,*,#32203,.F.);
#46802=ORIENTED_EDGE('',*,*,#32207,.F.);
#46803=ORIENTED_EDGE('',*,*,#32206,.T.);
#46804=ORIENTED_EDGE('',*,*,#32267,.T.);
#46805=ORIENTED_EDGE('',*,*,#32257,.T.);
#46806=ORIENTED_EDGE('',*,*,#32268,.T.);
#46807=ORIENTED_EDGE('',*,*,#32269,.T.);
#46808=ORIENTED_EDGE('',*,*,#32268,.F.);
#46809=ORIENTED_EDGE('',*,*,#32256,.T.);
#46810=ORIENTED_EDGE('',*,*,#32205,.T.);
#46811=ORIENTED_EDGE('',*,*,#32259,.T.);
#46812=ORIENTED_EDGE('',*,*,#32267,.F.);
#46813=ORIENTED_EDGE('',*,*,#32270,.F.);
#46814=ORIENTED_EDGE('',*,*,#32269,.F.);
#46815=ORIENTED_EDGE('',*,*,#32271,.F.);
#46816=ORIENTED_EDGE('',*,*,#32272,.T.);
#46817=ORIENTED_EDGE('',*,*,#32273,.T.);
#46818=ORIENTED_EDGE('',*,*,#32274,.T.);
#46819=ORIENTED_EDGE('',*,*,#32275,.F.);
#46820=ORIENTED_EDGE('',*,*,#32274,.F.);
#46821=ORIENTED_EDGE('',*,*,#32276,.F.);
#46822=ORIENTED_EDGE('',*,*,#32277,.F.);
#46823=ORIENTED_EDGE('',*,*,#32276,.T.);
#46824=ORIENTED_EDGE('',*,*,#32273,.F.);
#46825=ORIENTED_EDGE('',*,*,#32278,.T.);
#46826=ORIENTED_EDGE('',*,*,#32279,.F.);
#46827=ORIENTED_EDGE('',*,*,#32278,.F.);
#46828=ORIENTED_EDGE('',*,*,#32272,.F.);
#46829=ORIENTED_EDGE('',*,*,#32280,.F.);
#46830=ORIENTED_EDGE('',*,*,#32281,.T.);
#46831=ORIENTED_EDGE('',*,*,#32282,.T.);
#46832=ORIENTED_EDGE('',*,*,#32283,.T.);
#46833=ORIENTED_EDGE('',*,*,#32284,.F.);
#46834=ORIENTED_EDGE('',*,*,#32283,.F.);
#46835=ORIENTED_EDGE('',*,*,#32285,.F.);
#46836=ORIENTED_EDGE('',*,*,#32286,.F.);
#46837=ORIENTED_EDGE('',*,*,#32285,.T.);
#46838=ORIENTED_EDGE('',*,*,#32282,.F.);
#46839=ORIENTED_EDGE('',*,*,#32287,.T.);
#46840=ORIENTED_EDGE('',*,*,#32288,.F.);
#46841=ORIENTED_EDGE('',*,*,#32287,.F.);
#46842=ORIENTED_EDGE('',*,*,#32281,.F.);
#46843=ORIENTED_EDGE('',*,*,#32289,.F.);
#46844=ORIENTED_EDGE('',*,*,#32290,.T.);
#46845=ORIENTED_EDGE('',*,*,#32291,.T.);
#46846=ORIENTED_EDGE('',*,*,#32292,.T.);
#46847=ORIENTED_EDGE('',*,*,#32293,.F.);
#46848=ORIENTED_EDGE('',*,*,#32292,.F.);
#46849=ORIENTED_EDGE('',*,*,#32294,.F.);
#46850=ORIENTED_EDGE('',*,*,#32295,.F.);
#46851=ORIENTED_EDGE('',*,*,#32294,.T.);
#46852=ORIENTED_EDGE('',*,*,#32291,.F.);
#46853=ORIENTED_EDGE('',*,*,#32296,.T.);
#46854=ORIENTED_EDGE('',*,*,#32297,.F.);
#46855=ORIENTED_EDGE('',*,*,#32296,.F.);
#46856=ORIENTED_EDGE('',*,*,#32290,.F.);
#46857=ORIENTED_EDGE('',*,*,#32298,.F.);
#46858=ORIENTED_EDGE('',*,*,#32299,.T.);
#46859=ORIENTED_EDGE('',*,*,#32300,.T.);
#46860=ORIENTED_EDGE('',*,*,#32301,.T.);
#46861=ORIENTED_EDGE('',*,*,#32302,.F.);
#46862=ORIENTED_EDGE('',*,*,#32301,.F.);
#46863=ORIENTED_EDGE('',*,*,#32303,.F.);
#46864=ORIENTED_EDGE('',*,*,#32304,.F.);
#46865=ORIENTED_EDGE('',*,*,#32303,.T.);
#46866=ORIENTED_EDGE('',*,*,#32300,.F.);
#46867=ORIENTED_EDGE('',*,*,#32305,.T.);
#46868=ORIENTED_EDGE('',*,*,#32306,.F.);
#46869=ORIENTED_EDGE('',*,*,#32305,.F.);
#46870=ORIENTED_EDGE('',*,*,#32299,.F.);
#46871=ORIENTED_EDGE('',*,*,#32307,.F.);
#46872=ORIENTED_EDGE('',*,*,#32308,.T.);
#46873=ORIENTED_EDGE('',*,*,#32309,.T.);
#46874=ORIENTED_EDGE('',*,*,#32310,.T.);
#46875=ORIENTED_EDGE('',*,*,#32311,.F.);
#46876=ORIENTED_EDGE('',*,*,#32310,.F.);
#46877=ORIENTED_EDGE('',*,*,#32312,.F.);
#46878=ORIENTED_EDGE('',*,*,#32313,.F.);
#46879=ORIENTED_EDGE('',*,*,#32312,.T.);
#46880=ORIENTED_EDGE('',*,*,#32309,.F.);
#46881=ORIENTED_EDGE('',*,*,#32314,.T.);
#46882=ORIENTED_EDGE('',*,*,#32315,.F.);
#46883=ORIENTED_EDGE('',*,*,#32314,.F.);
#46884=ORIENTED_EDGE('',*,*,#32308,.F.);
#46885=ORIENTED_EDGE('',*,*,#32316,.F.);
#46886=ORIENTED_EDGE('',*,*,#32317,.T.);
#46887=ORIENTED_EDGE('',*,*,#32318,.T.);
#46888=ORIENTED_EDGE('',*,*,#32319,.T.);
#46889=ORIENTED_EDGE('',*,*,#32320,.F.);
#46890=ORIENTED_EDGE('',*,*,#32319,.F.);
#46891=ORIENTED_EDGE('',*,*,#32321,.F.);
#46892=ORIENTED_EDGE('',*,*,#32322,.F.);
#46893=ORIENTED_EDGE('',*,*,#32321,.T.);
#46894=ORIENTED_EDGE('',*,*,#32318,.F.);
#46895=ORIENTED_EDGE('',*,*,#32323,.T.);
#46896=ORIENTED_EDGE('',*,*,#32324,.F.);
#46897=ORIENTED_EDGE('',*,*,#32323,.F.);
#46898=ORIENTED_EDGE('',*,*,#32317,.F.);
#46899=ORIENTED_EDGE('',*,*,#32325,.F.);
#46900=ORIENTED_EDGE('',*,*,#32326,.T.);
#46901=ORIENTED_EDGE('',*,*,#32327,.T.);
#46902=ORIENTED_EDGE('',*,*,#32328,.T.);
#46903=ORIENTED_EDGE('',*,*,#32329,.F.);
#46904=ORIENTED_EDGE('',*,*,#32328,.F.);
#46905=ORIENTED_EDGE('',*,*,#32330,.F.);
#46906=ORIENTED_EDGE('',*,*,#32331,.F.);
#46907=ORIENTED_EDGE('',*,*,#32330,.T.);
#46908=ORIENTED_EDGE('',*,*,#32327,.F.);
#46909=ORIENTED_EDGE('',*,*,#32332,.T.);
#46910=ORIENTED_EDGE('',*,*,#32333,.F.);
#46911=ORIENTED_EDGE('',*,*,#32332,.F.);
#46912=ORIENTED_EDGE('',*,*,#32326,.F.);
#46913=ORIENTED_EDGE('',*,*,#32334,.F.);
#46914=ORIENTED_EDGE('',*,*,#32335,.T.);
#46915=ORIENTED_EDGE('',*,*,#32336,.T.);
#46916=ORIENTED_EDGE('',*,*,#32337,.T.);
#46917=ORIENTED_EDGE('',*,*,#32338,.F.);
#46918=ORIENTED_EDGE('',*,*,#32337,.F.);
#46919=ORIENTED_EDGE('',*,*,#32339,.F.);
#46920=ORIENTED_EDGE('',*,*,#32340,.F.);
#46921=ORIENTED_EDGE('',*,*,#32339,.T.);
#46922=ORIENTED_EDGE('',*,*,#32336,.F.);
#46923=ORIENTED_EDGE('',*,*,#32341,.T.);
#46924=ORIENTED_EDGE('',*,*,#32342,.F.);
#46925=ORIENTED_EDGE('',*,*,#32341,.F.);
#46926=ORIENTED_EDGE('',*,*,#32335,.F.);
#46927=ORIENTED_EDGE('',*,*,#32343,.F.);
#46928=ORIENTED_EDGE('',*,*,#32344,.T.);
#46929=ORIENTED_EDGE('',*,*,#32345,.T.);
#46930=ORIENTED_EDGE('',*,*,#32346,.T.);
#46931=ORIENTED_EDGE('',*,*,#32347,.F.);
#46932=ORIENTED_EDGE('',*,*,#32346,.F.);
#46933=ORIENTED_EDGE('',*,*,#32348,.F.);
#46934=ORIENTED_EDGE('',*,*,#32349,.F.);
#46935=ORIENTED_EDGE('',*,*,#32348,.T.);
#46936=ORIENTED_EDGE('',*,*,#32345,.F.);
#46937=ORIENTED_EDGE('',*,*,#32350,.T.);
#46938=ORIENTED_EDGE('',*,*,#32351,.F.);
#46939=ORIENTED_EDGE('',*,*,#32350,.F.);
#46940=ORIENTED_EDGE('',*,*,#32344,.F.);
#46941=ORIENTED_EDGE('',*,*,#32352,.F.);
#46942=ORIENTED_EDGE('',*,*,#32353,.T.);
#46943=ORIENTED_EDGE('',*,*,#32354,.T.);
#46944=ORIENTED_EDGE('',*,*,#32355,.T.);
#46945=ORIENTED_EDGE('',*,*,#32356,.F.);
#46946=ORIENTED_EDGE('',*,*,#32355,.F.);
#46947=ORIENTED_EDGE('',*,*,#32357,.F.);
#46948=ORIENTED_EDGE('',*,*,#32358,.F.);
#46949=ORIENTED_EDGE('',*,*,#32357,.T.);
#46950=ORIENTED_EDGE('',*,*,#32354,.F.);
#46951=ORIENTED_EDGE('',*,*,#32359,.T.);
#46952=ORIENTED_EDGE('',*,*,#32360,.F.);
#46953=ORIENTED_EDGE('',*,*,#32359,.F.);
#46954=ORIENTED_EDGE('',*,*,#32353,.F.);
#46955=ORIENTED_EDGE('',*,*,#32361,.F.);
#46956=ORIENTED_EDGE('',*,*,#32362,.T.);
#46957=ORIENTED_EDGE('',*,*,#32363,.T.);
#46958=ORIENTED_EDGE('',*,*,#32364,.T.);
#46959=ORIENTED_EDGE('',*,*,#32365,.F.);
#46960=ORIENTED_EDGE('',*,*,#32364,.F.);
#46961=ORIENTED_EDGE('',*,*,#32366,.F.);
#46962=ORIENTED_EDGE('',*,*,#32367,.F.);
#46963=ORIENTED_EDGE('',*,*,#32366,.T.);
#46964=ORIENTED_EDGE('',*,*,#32363,.F.);
#46965=ORIENTED_EDGE('',*,*,#32368,.T.);
#46966=ORIENTED_EDGE('',*,*,#32369,.F.);
#46967=ORIENTED_EDGE('',*,*,#32368,.F.);
#46968=ORIENTED_EDGE('',*,*,#32362,.F.);
#46969=ORIENTED_EDGE('',*,*,#32370,.F.);
#46970=ORIENTED_EDGE('',*,*,#32371,.T.);
#46971=ORIENTED_EDGE('',*,*,#32372,.T.);
#46972=ORIENTED_EDGE('',*,*,#32373,.T.);
#46973=ORIENTED_EDGE('',*,*,#32374,.F.);
#46974=ORIENTED_EDGE('',*,*,#32373,.F.);
#46975=ORIENTED_EDGE('',*,*,#32375,.F.);
#46976=ORIENTED_EDGE('',*,*,#32376,.F.);
#46977=ORIENTED_EDGE('',*,*,#32375,.T.);
#46978=ORIENTED_EDGE('',*,*,#32372,.F.);
#46979=ORIENTED_EDGE('',*,*,#32377,.T.);
#46980=ORIENTED_EDGE('',*,*,#32378,.F.);
#46981=ORIENTED_EDGE('',*,*,#32377,.F.);
#46982=ORIENTED_EDGE('',*,*,#32371,.F.);
#46983=ORIENTED_EDGE('',*,*,#32379,.F.);
#46984=ORIENTED_EDGE('',*,*,#32380,.T.);
#46985=ORIENTED_EDGE('',*,*,#32381,.T.);
#46986=ORIENTED_EDGE('',*,*,#32382,.T.);
#46987=ORIENTED_EDGE('',*,*,#32383,.F.);
#46988=ORIENTED_EDGE('',*,*,#32382,.F.);
#46989=ORIENTED_EDGE('',*,*,#32384,.F.);
#46990=ORIENTED_EDGE('',*,*,#32385,.F.);
#46991=ORIENTED_EDGE('',*,*,#32384,.T.);
#46992=ORIENTED_EDGE('',*,*,#32381,.F.);
#46993=ORIENTED_EDGE('',*,*,#32386,.T.);
#46994=ORIENTED_EDGE('',*,*,#32387,.F.);
#46995=ORIENTED_EDGE('',*,*,#32386,.F.);
#46996=ORIENTED_EDGE('',*,*,#32380,.F.);
#46997=ORIENTED_EDGE('',*,*,#32388,.F.);
#46998=ORIENTED_EDGE('',*,*,#32389,.T.);
#46999=ORIENTED_EDGE('',*,*,#32390,.T.);
#47000=ORIENTED_EDGE('',*,*,#32391,.T.);
#47001=ORIENTED_EDGE('',*,*,#32392,.F.);
#47002=ORIENTED_EDGE('',*,*,#32391,.F.);
#47003=ORIENTED_EDGE('',*,*,#32393,.F.);
#47004=ORIENTED_EDGE('',*,*,#32394,.F.);
#47005=ORIENTED_EDGE('',*,*,#32393,.T.);
#47006=ORIENTED_EDGE('',*,*,#32390,.F.);
#47007=ORIENTED_EDGE('',*,*,#32395,.T.);
#47008=ORIENTED_EDGE('',*,*,#32396,.F.);
#47009=ORIENTED_EDGE('',*,*,#32395,.F.);
#47010=ORIENTED_EDGE('',*,*,#32389,.F.);
#47011=ORIENTED_EDGE('',*,*,#32397,.F.);
#47012=ORIENTED_EDGE('',*,*,#32398,.T.);
#47013=ORIENTED_EDGE('',*,*,#32399,.T.);
#47014=ORIENTED_EDGE('',*,*,#32400,.T.);
#47015=ORIENTED_EDGE('',*,*,#32401,.F.);
#47016=ORIENTED_EDGE('',*,*,#32400,.F.);
#47017=ORIENTED_EDGE('',*,*,#32402,.F.);
#47018=ORIENTED_EDGE('',*,*,#32403,.F.);
#47019=ORIENTED_EDGE('',*,*,#32402,.T.);
#47020=ORIENTED_EDGE('',*,*,#32399,.F.);
#47021=ORIENTED_EDGE('',*,*,#32404,.T.);
#47022=ORIENTED_EDGE('',*,*,#32405,.F.);
#47023=ORIENTED_EDGE('',*,*,#32404,.F.);
#47024=ORIENTED_EDGE('',*,*,#32398,.F.);
#47025=ORIENTED_EDGE('',*,*,#32406,.F.);
#47026=ORIENTED_EDGE('',*,*,#32407,.T.);
#47027=ORIENTED_EDGE('',*,*,#32408,.T.);
#47028=ORIENTED_EDGE('',*,*,#32409,.T.);
#47029=ORIENTED_EDGE('',*,*,#32410,.F.);
#47030=ORIENTED_EDGE('',*,*,#32409,.F.);
#47031=ORIENTED_EDGE('',*,*,#32411,.F.);
#47032=ORIENTED_EDGE('',*,*,#32412,.F.);
#47033=ORIENTED_EDGE('',*,*,#32411,.T.);
#47034=ORIENTED_EDGE('',*,*,#32408,.F.);
#47035=ORIENTED_EDGE('',*,*,#32413,.T.);
#47036=ORIENTED_EDGE('',*,*,#32414,.F.);
#47037=ORIENTED_EDGE('',*,*,#32413,.F.);
#47038=ORIENTED_EDGE('',*,*,#32407,.F.);
#47039=ORIENTED_EDGE('',*,*,#32415,.F.);
#47040=ORIENTED_EDGE('',*,*,#32416,.T.);
#47041=ORIENTED_EDGE('',*,*,#32417,.T.);
#47042=ORIENTED_EDGE('',*,*,#32418,.T.);
#47043=ORIENTED_EDGE('',*,*,#32419,.F.);
#47044=ORIENTED_EDGE('',*,*,#32418,.F.);
#47045=ORIENTED_EDGE('',*,*,#32420,.F.);
#47046=ORIENTED_EDGE('',*,*,#32421,.F.);
#47047=ORIENTED_EDGE('',*,*,#32420,.T.);
#47048=ORIENTED_EDGE('',*,*,#32417,.F.);
#47049=ORIENTED_EDGE('',*,*,#32422,.T.);
#47050=ORIENTED_EDGE('',*,*,#32423,.F.);
#47051=ORIENTED_EDGE('',*,*,#32422,.F.);
#47052=ORIENTED_EDGE('',*,*,#32416,.F.);
#47053=ORIENTED_EDGE('',*,*,#32424,.F.);
#47054=ORIENTED_EDGE('',*,*,#32425,.T.);
#47055=ORIENTED_EDGE('',*,*,#32426,.T.);
#47056=ORIENTED_EDGE('',*,*,#32427,.T.);
#47057=ORIENTED_EDGE('',*,*,#32428,.F.);
#47058=ORIENTED_EDGE('',*,*,#32427,.F.);
#47059=ORIENTED_EDGE('',*,*,#32429,.F.);
#47060=ORIENTED_EDGE('',*,*,#32430,.F.);
#47061=ORIENTED_EDGE('',*,*,#32431,.F.);
#47062=ORIENTED_EDGE('',*,*,#32429,.T.);
#47063=ORIENTED_EDGE('',*,*,#32426,.F.);
#47064=ORIENTED_EDGE('',*,*,#32432,.T.);
#47065=ORIENTED_EDGE('',*,*,#32433,.F.);
#47066=ORIENTED_EDGE('',*,*,#32432,.F.);
#47067=ORIENTED_EDGE('',*,*,#32425,.F.);
#47068=ORIENTED_EDGE('',*,*,#32434,.F.);
#47069=ORIENTED_EDGE('',*,*,#32435,.F.);
#47070=ORIENTED_EDGE('',*,*,#32436,.T.);
#47071=ORIENTED_EDGE('',*,*,#32437,.T.);
#47072=ORIENTED_EDGE('',*,*,#32438,.T.);
#47073=ORIENTED_EDGE('',*,*,#32439,.F.);
#47074=ORIENTED_EDGE('',*,*,#32438,.F.);
#47075=ORIENTED_EDGE('',*,*,#32440,.F.);
#47076=ORIENTED_EDGE('',*,*,#32441,.F.);
#47077=ORIENTED_EDGE('',*,*,#32440,.T.);
#47078=ORIENTED_EDGE('',*,*,#32437,.F.);
#47079=ORIENTED_EDGE('',*,*,#32442,.T.);
#47080=ORIENTED_EDGE('',*,*,#32443,.F.);
#47081=ORIENTED_EDGE('',*,*,#32442,.F.);
#47082=ORIENTED_EDGE('',*,*,#32436,.F.);
#47083=ORIENTED_EDGE('',*,*,#32444,.F.);
#47084=ORIENTED_EDGE('',*,*,#32445,.T.);
#47085=ORIENTED_EDGE('',*,*,#32446,.T.);
#47086=ORIENTED_EDGE('',*,*,#32447,.T.);
#47087=ORIENTED_EDGE('',*,*,#32448,.F.);
#47088=ORIENTED_EDGE('',*,*,#32447,.F.);
#47089=ORIENTED_EDGE('',*,*,#32449,.F.);
#47090=ORIENTED_EDGE('',*,*,#32450,.F.);
#47091=ORIENTED_EDGE('',*,*,#32449,.T.);
#47092=ORIENTED_EDGE('',*,*,#32446,.F.);
#47093=ORIENTED_EDGE('',*,*,#32451,.T.);
#47094=ORIENTED_EDGE('',*,*,#32452,.F.);
#47095=ORIENTED_EDGE('',*,*,#32451,.F.);
#47096=ORIENTED_EDGE('',*,*,#32445,.F.);
#47097=ORIENTED_EDGE('',*,*,#32453,.F.);
#47098=ORIENTED_EDGE('',*,*,#32454,.T.);
#47099=ORIENTED_EDGE('',*,*,#32455,.T.);
#47100=ORIENTED_EDGE('',*,*,#32456,.T.);
#47101=ORIENTED_EDGE('',*,*,#32457,.F.);
#47102=ORIENTED_EDGE('',*,*,#32456,.F.);
#47103=ORIENTED_EDGE('',*,*,#32458,.F.);
#47104=ORIENTED_EDGE('',*,*,#32459,.F.);
#47105=ORIENTED_EDGE('',*,*,#32458,.T.);
#47106=ORIENTED_EDGE('',*,*,#32455,.F.);
#47107=ORIENTED_EDGE('',*,*,#32460,.T.);
#47108=ORIENTED_EDGE('',*,*,#32461,.F.);
#47109=ORIENTED_EDGE('',*,*,#32460,.F.);
#47110=ORIENTED_EDGE('',*,*,#32454,.F.);
#47111=ORIENTED_EDGE('',*,*,#32462,.F.);
#47112=ORIENTED_EDGE('',*,*,#32463,.T.);
#47113=ORIENTED_EDGE('',*,*,#32464,.T.);
#47114=ORIENTED_EDGE('',*,*,#32465,.T.);
#47115=ORIENTED_EDGE('',*,*,#32466,.F.);
#47116=ORIENTED_EDGE('',*,*,#32465,.F.);
#47117=ORIENTED_EDGE('',*,*,#32467,.F.);
#47118=ORIENTED_EDGE('',*,*,#32468,.F.);
#47119=ORIENTED_EDGE('',*,*,#32467,.T.);
#47120=ORIENTED_EDGE('',*,*,#32464,.F.);
#47121=ORIENTED_EDGE('',*,*,#32469,.T.);
#47122=ORIENTED_EDGE('',*,*,#32470,.F.);
#47123=ORIENTED_EDGE('',*,*,#32469,.F.);
#47124=ORIENTED_EDGE('',*,*,#32463,.F.);
#47125=ORIENTED_EDGE('',*,*,#32471,.F.);
#47126=ORIENTED_EDGE('',*,*,#32472,.T.);
#47127=ORIENTED_EDGE('',*,*,#32473,.T.);
#47128=ORIENTED_EDGE('',*,*,#32474,.T.);
#47129=ORIENTED_EDGE('',*,*,#32475,.F.);
#47130=ORIENTED_EDGE('',*,*,#32474,.F.);
#47131=ORIENTED_EDGE('',*,*,#32476,.F.);
#47132=ORIENTED_EDGE('',*,*,#32477,.F.);
#47133=ORIENTED_EDGE('',*,*,#32476,.T.);
#47134=ORIENTED_EDGE('',*,*,#32473,.F.);
#47135=ORIENTED_EDGE('',*,*,#32478,.T.);
#47136=ORIENTED_EDGE('',*,*,#32479,.F.);
#47137=ORIENTED_EDGE('',*,*,#32478,.F.);
#47138=ORIENTED_EDGE('',*,*,#32472,.F.);
#47139=ORIENTED_EDGE('',*,*,#32480,.F.);
#47140=ORIENTED_EDGE('',*,*,#32481,.T.);
#47141=ORIENTED_EDGE('',*,*,#32482,.T.);
#47142=ORIENTED_EDGE('',*,*,#32483,.T.);
#47143=ORIENTED_EDGE('',*,*,#32484,.F.);
#47144=ORIENTED_EDGE('',*,*,#32483,.F.);
#47145=ORIENTED_EDGE('',*,*,#32485,.F.);
#47146=ORIENTED_EDGE('',*,*,#32486,.F.);
#47147=ORIENTED_EDGE('',*,*,#32485,.T.);
#47148=ORIENTED_EDGE('',*,*,#32482,.F.);
#47149=ORIENTED_EDGE('',*,*,#32487,.T.);
#47150=ORIENTED_EDGE('',*,*,#32488,.F.);
#47151=ORIENTED_EDGE('',*,*,#32487,.F.);
#47152=ORIENTED_EDGE('',*,*,#32481,.F.);
#47153=ORIENTED_EDGE('',*,*,#32489,.F.);
#47154=ORIENTED_EDGE('',*,*,#32490,.T.);
#47155=ORIENTED_EDGE('',*,*,#32491,.T.);
#47156=ORIENTED_EDGE('',*,*,#32492,.T.);
#47157=ORIENTED_EDGE('',*,*,#32493,.F.);
#47158=ORIENTED_EDGE('',*,*,#32492,.F.);
#47159=ORIENTED_EDGE('',*,*,#32494,.F.);
#47160=ORIENTED_EDGE('',*,*,#32495,.F.);
#47161=ORIENTED_EDGE('',*,*,#32494,.T.);
#47162=ORIENTED_EDGE('',*,*,#32491,.F.);
#47163=ORIENTED_EDGE('',*,*,#32496,.T.);
#47164=ORIENTED_EDGE('',*,*,#32497,.F.);
#47165=ORIENTED_EDGE('',*,*,#32496,.F.);
#47166=ORIENTED_EDGE('',*,*,#32490,.F.);
#47167=ORIENTED_EDGE('',*,*,#32498,.F.);
#47168=ORIENTED_EDGE('',*,*,#32499,.T.);
#47169=ORIENTED_EDGE('',*,*,#32500,.T.);
#47170=ORIENTED_EDGE('',*,*,#32501,.T.);
#47171=ORIENTED_EDGE('',*,*,#32502,.F.);
#47172=ORIENTED_EDGE('',*,*,#32501,.F.);
#47173=ORIENTED_EDGE('',*,*,#32503,.F.);
#47174=ORIENTED_EDGE('',*,*,#32504,.F.);
#47175=ORIENTED_EDGE('',*,*,#32503,.T.);
#47176=ORIENTED_EDGE('',*,*,#32500,.F.);
#47177=ORIENTED_EDGE('',*,*,#32505,.T.);
#47178=ORIENTED_EDGE('',*,*,#32506,.F.);
#47179=ORIENTED_EDGE('',*,*,#32505,.F.);
#47180=ORIENTED_EDGE('',*,*,#32499,.F.);
#47181=ORIENTED_EDGE('',*,*,#32507,.F.);
#47182=ORIENTED_EDGE('',*,*,#32508,.T.);
#47183=ORIENTED_EDGE('',*,*,#32509,.T.);
#47184=ORIENTED_EDGE('',*,*,#32510,.T.);
#47185=ORIENTED_EDGE('',*,*,#32511,.F.);
#47186=ORIENTED_EDGE('',*,*,#32510,.F.);
#47187=ORIENTED_EDGE('',*,*,#32512,.F.);
#47188=ORIENTED_EDGE('',*,*,#32513,.F.);
#47189=ORIENTED_EDGE('',*,*,#32512,.T.);
#47190=ORIENTED_EDGE('',*,*,#32509,.F.);
#47191=ORIENTED_EDGE('',*,*,#32514,.T.);
#47192=ORIENTED_EDGE('',*,*,#32515,.F.);
#47193=ORIENTED_EDGE('',*,*,#32514,.F.);
#47194=ORIENTED_EDGE('',*,*,#32508,.F.);
#47195=ORIENTED_EDGE('',*,*,#32516,.F.);
#47196=ORIENTED_EDGE('',*,*,#32517,.T.);
#47197=ORIENTED_EDGE('',*,*,#32518,.T.);
#47198=ORIENTED_EDGE('',*,*,#32519,.T.);
#47199=ORIENTED_EDGE('',*,*,#32520,.F.);
#47200=ORIENTED_EDGE('',*,*,#32519,.F.);
#47201=ORIENTED_EDGE('',*,*,#32521,.F.);
#47202=ORIENTED_EDGE('',*,*,#32522,.F.);
#47203=ORIENTED_EDGE('',*,*,#32521,.T.);
#47204=ORIENTED_EDGE('',*,*,#32518,.F.);
#47205=ORIENTED_EDGE('',*,*,#32523,.T.);
#47206=ORIENTED_EDGE('',*,*,#32524,.F.);
#47207=ORIENTED_EDGE('',*,*,#32523,.F.);
#47208=ORIENTED_EDGE('',*,*,#32517,.F.);
#47209=ORIENTED_EDGE('',*,*,#32525,.F.);
#47210=ORIENTED_EDGE('',*,*,#32526,.T.);
#47211=ORIENTED_EDGE('',*,*,#32527,.T.);
#47212=ORIENTED_EDGE('',*,*,#32528,.T.);
#47213=ORIENTED_EDGE('',*,*,#32529,.F.);
#47214=ORIENTED_EDGE('',*,*,#32528,.F.);
#47215=ORIENTED_EDGE('',*,*,#32530,.F.);
#47216=ORIENTED_EDGE('',*,*,#32531,.F.);
#47217=ORIENTED_EDGE('',*,*,#32530,.T.);
#47218=ORIENTED_EDGE('',*,*,#32527,.F.);
#47219=ORIENTED_EDGE('',*,*,#32532,.T.);
#47220=ORIENTED_EDGE('',*,*,#32533,.F.);
#47221=ORIENTED_EDGE('',*,*,#32532,.F.);
#47222=ORIENTED_EDGE('',*,*,#32526,.F.);
#47223=ORIENTED_EDGE('',*,*,#32534,.F.);
#47224=ORIENTED_EDGE('',*,*,#32535,.T.);
#47225=ORIENTED_EDGE('',*,*,#32536,.T.);
#47226=ORIENTED_EDGE('',*,*,#32537,.T.);
#47227=ORIENTED_EDGE('',*,*,#32538,.F.);
#47228=ORIENTED_EDGE('',*,*,#32537,.F.);
#47229=ORIENTED_EDGE('',*,*,#32539,.F.);
#47230=ORIENTED_EDGE('',*,*,#32540,.F.);
#47231=ORIENTED_EDGE('',*,*,#32539,.T.);
#47232=ORIENTED_EDGE('',*,*,#32536,.F.);
#47233=ORIENTED_EDGE('',*,*,#32541,.T.);
#47234=ORIENTED_EDGE('',*,*,#32542,.F.);
#47235=ORIENTED_EDGE('',*,*,#32541,.F.);
#47236=ORIENTED_EDGE('',*,*,#32535,.F.);
#47237=ORIENTED_EDGE('',*,*,#32543,.F.);
#47238=ORIENTED_EDGE('',*,*,#32544,.T.);
#47239=ORIENTED_EDGE('',*,*,#32545,.T.);
#47240=ORIENTED_EDGE('',*,*,#32546,.T.);
#47241=ORIENTED_EDGE('',*,*,#32547,.F.);
#47242=ORIENTED_EDGE('',*,*,#32546,.F.);
#47243=ORIENTED_EDGE('',*,*,#32548,.F.);
#47244=ORIENTED_EDGE('',*,*,#32549,.F.);
#47245=ORIENTED_EDGE('',*,*,#32548,.T.);
#47246=ORIENTED_EDGE('',*,*,#32545,.F.);
#47247=ORIENTED_EDGE('',*,*,#32550,.T.);
#47248=ORIENTED_EDGE('',*,*,#32551,.F.);
#47249=ORIENTED_EDGE('',*,*,#32550,.F.);
#47250=ORIENTED_EDGE('',*,*,#32544,.F.);
#47251=ORIENTED_EDGE('',*,*,#32552,.F.);
#47252=ORIENTED_EDGE('',*,*,#32553,.T.);
#47253=ORIENTED_EDGE('',*,*,#32554,.T.);
#47254=ORIENTED_EDGE('',*,*,#32555,.T.);
#47255=ORIENTED_EDGE('',*,*,#32556,.F.);
#47256=ORIENTED_EDGE('',*,*,#32555,.F.);
#47257=ORIENTED_EDGE('',*,*,#32557,.F.);
#47258=ORIENTED_EDGE('',*,*,#32558,.F.);
#47259=ORIENTED_EDGE('',*,*,#32557,.T.);
#47260=ORIENTED_EDGE('',*,*,#32554,.F.);
#47261=ORIENTED_EDGE('',*,*,#32559,.T.);
#47262=ORIENTED_EDGE('',*,*,#32560,.F.);
#47263=ORIENTED_EDGE('',*,*,#32559,.F.);
#47264=ORIENTED_EDGE('',*,*,#32553,.F.);
#47265=ORIENTED_EDGE('',*,*,#32561,.F.);
#47266=ORIENTED_EDGE('',*,*,#32562,.T.);
#47267=ORIENTED_EDGE('',*,*,#32563,.T.);
#47268=ORIENTED_EDGE('',*,*,#32564,.T.);
#47269=ORIENTED_EDGE('',*,*,#32565,.F.);
#47270=ORIENTED_EDGE('',*,*,#32564,.F.);
#47271=ORIENTED_EDGE('',*,*,#32566,.F.);
#47272=ORIENTED_EDGE('',*,*,#32567,.F.);
#47273=ORIENTED_EDGE('',*,*,#32566,.T.);
#47274=ORIENTED_EDGE('',*,*,#32563,.F.);
#47275=ORIENTED_EDGE('',*,*,#32568,.T.);
#47276=ORIENTED_EDGE('',*,*,#32569,.F.);
#47277=ORIENTED_EDGE('',*,*,#32568,.F.);
#47278=ORIENTED_EDGE('',*,*,#32562,.F.);
#47279=ORIENTED_EDGE('',*,*,#32570,.F.);
#47280=ORIENTED_EDGE('',*,*,#32571,.T.);
#47281=ORIENTED_EDGE('',*,*,#32572,.T.);
#47282=ORIENTED_EDGE('',*,*,#32573,.T.);
#47283=ORIENTED_EDGE('',*,*,#32574,.F.);
#47284=ORIENTED_EDGE('',*,*,#32573,.F.);
#47285=ORIENTED_EDGE('',*,*,#32575,.F.);
#47286=ORIENTED_EDGE('',*,*,#32576,.F.);
#47287=ORIENTED_EDGE('',*,*,#32575,.T.);
#47288=ORIENTED_EDGE('',*,*,#32572,.F.);
#47289=ORIENTED_EDGE('',*,*,#32577,.T.);
#47290=ORIENTED_EDGE('',*,*,#32578,.F.);
#47291=ORIENTED_EDGE('',*,*,#32577,.F.);
#47292=ORIENTED_EDGE('',*,*,#32571,.F.);
#47293=ORIENTED_EDGE('',*,*,#32579,.F.);
#47294=ORIENTED_EDGE('',*,*,#32580,.T.);
#47295=ORIENTED_EDGE('',*,*,#32581,.T.);
#47296=ORIENTED_EDGE('',*,*,#32582,.T.);
#47297=ORIENTED_EDGE('',*,*,#32583,.F.);
#47298=ORIENTED_EDGE('',*,*,#32582,.F.);
#47299=ORIENTED_EDGE('',*,*,#32584,.F.);
#47300=ORIENTED_EDGE('',*,*,#32585,.F.);
#47301=ORIENTED_EDGE('',*,*,#32584,.T.);
#47302=ORIENTED_EDGE('',*,*,#32581,.F.);
#47303=ORIENTED_EDGE('',*,*,#32586,.T.);
#47304=ORIENTED_EDGE('',*,*,#32587,.F.);
#47305=ORIENTED_EDGE('',*,*,#32586,.F.);
#47306=ORIENTED_EDGE('',*,*,#32580,.F.);
#47307=ORIENTED_EDGE('',*,*,#32588,.F.);
#47308=ORIENTED_EDGE('',*,*,#32589,.F.);
#47309=ORIENTED_EDGE('',*,*,#32590,.F.);
#47310=ORIENTED_EDGE('',*,*,#32591,.F.);
#47311=ORIENTED_EDGE('',*,*,#32592,.T.);
#47312=ORIENTED_EDGE('',*,*,#32593,.T.);
#47313=ORIENTED_EDGE('',*,*,#32589,.T.);
#47314=ORIENTED_EDGE('',*,*,#32594,.F.);
#47315=ORIENTED_EDGE('',*,*,#32590,.T.);
#47316=ORIENTED_EDGE('',*,*,#32593,.F.);
#47317=ORIENTED_EDGE('',*,*,#32595,.T.);
#47318=ORIENTED_EDGE('',*,*,#32596,.F.);
#47319=ORIENTED_EDGE('',*,*,#32595,.F.);
#47320=ORIENTED_EDGE('',*,*,#32592,.F.);
#47321=ORIENTED_EDGE('',*,*,#32597,.T.);
#47322=ORIENTED_EDGE('',*,*,#32598,.F.);
#47323=ORIENTED_EDGE('',*,*,#32597,.F.);
#47324=ORIENTED_EDGE('',*,*,#32599,.F.);
#47325=ORIENTED_EDGE('',*,*,#32600,.F.);
#47326=ORIENTED_EDGE('',*,*,#32601,.F.);
#47327=ORIENTED_EDGE('',*,*,#32602,.T.);
#47328=ORIENTED_EDGE('',*,*,#32603,.F.);
#47329=ORIENTED_EDGE('',*,*,#32602,.F.);
#47330=ORIENTED_EDGE('',*,*,#32604,.F.);
#47331=ORIENTED_EDGE('',*,*,#32605,.T.);
#47332=ORIENTED_EDGE('',*,*,#32606,.F.);
#47333=ORIENTED_EDGE('',*,*,#32605,.F.);
#47334=ORIENTED_EDGE('',*,*,#32607,.F.);
#47335=ORIENTED_EDGE('',*,*,#32608,.T.);
#47336=ORIENTED_EDGE('',*,*,#32609,.F.);
#47337=ORIENTED_EDGE('',*,*,#32608,.F.);
#47338=ORIENTED_EDGE('',*,*,#32610,.F.);
#47339=ORIENTED_EDGE('',*,*,#32611,.T.);
#47340=ORIENTED_EDGE('',*,*,#32612,.F.);
#47341=ORIENTED_EDGE('',*,*,#32611,.F.);
#47342=ORIENTED_EDGE('',*,*,#32613,.F.);
#47343=ORIENTED_EDGE('',*,*,#32614,.T.);
#47344=ORIENTED_EDGE('',*,*,#32615,.F.);
#47345=ORIENTED_EDGE('',*,*,#32614,.F.);
#47346=ORIENTED_EDGE('',*,*,#32616,.F.);
#47347=ORIENTED_EDGE('',*,*,#32600,.T.);
#47348=ORIENTED_EDGE('',*,*,#32607,.T.);
#47349=ORIENTED_EDGE('',*,*,#32604,.T.);
#47350=ORIENTED_EDGE('',*,*,#32601,.T.);
#47351=ORIENTED_EDGE('',*,*,#32616,.T.);
#47352=ORIENTED_EDGE('',*,*,#32613,.T.);
#47353=ORIENTED_EDGE('',*,*,#32610,.T.);
#47354=ORIENTED_EDGE('',*,*,#32598,.T.);
#47355=ORIENTED_EDGE('',*,*,#32617,.F.);
#47356=ORIENTED_EDGE('',*,*,#32262,.F.);
#47357=ORIENTED_EDGE('',*,*,#32161,.F.);
#47358=ORIENTED_EDGE('',*,*,#32263,.F.);
#47359=ORIENTED_EDGE('',*,*,#32618,.T.);
#47360=ORIENTED_EDGE('',*,*,#32617,.T.);
#47361=ORIENTED_EDGE('',*,*,#32618,.F.);
#47362=ORIENTED_EDGE('',*,*,#32271,.T.);
#47363=ORIENTED_EDGE('',*,*,#32619,.F.);
#47364=ORIENTED_EDGE('',*,*,#32286,.T.);
#47365=ORIENTED_EDGE('',*,*,#32288,.T.);
#47366=ORIENTED_EDGE('',*,*,#32280,.T.);
#47367=ORIENTED_EDGE('',*,*,#32620,.F.);
#47368=ORIENTED_EDGE('',*,*,#32295,.T.);
#47369=ORIENTED_EDGE('',*,*,#32297,.T.);
#47370=ORIENTED_EDGE('',*,*,#32289,.T.);
#47371=ORIENTED_EDGE('',*,*,#32621,.F.);
#47372=ORIENTED_EDGE('',*,*,#32304,.T.);
#47373=ORIENTED_EDGE('',*,*,#32306,.T.);
#47374=ORIENTED_EDGE('',*,*,#32298,.T.);
#47375=ORIENTED_EDGE('',*,*,#32622,.F.);
#47376=ORIENTED_EDGE('',*,*,#32313,.T.);
#47377=ORIENTED_EDGE('',*,*,#32315,.T.);
#47378=ORIENTED_EDGE('',*,*,#32307,.T.);
#47379=ORIENTED_EDGE('',*,*,#32623,.F.);
#47380=ORIENTED_EDGE('',*,*,#32322,.T.);
#47381=ORIENTED_EDGE('',*,*,#32324,.T.);
#47382=ORIENTED_EDGE('',*,*,#32316,.T.);
#47383=ORIENTED_EDGE('',*,*,#32624,.F.);
#47384=ORIENTED_EDGE('',*,*,#32331,.T.);
#47385=ORIENTED_EDGE('',*,*,#32333,.T.);
#47386=ORIENTED_EDGE('',*,*,#32325,.T.);
#47387=ORIENTED_EDGE('',*,*,#32625,.F.);
#47388=ORIENTED_EDGE('',*,*,#32340,.T.);
#47389=ORIENTED_EDGE('',*,*,#32342,.T.);
#47390=ORIENTED_EDGE('',*,*,#32334,.T.);
#47391=ORIENTED_EDGE('',*,*,#32626,.F.);
#47392=ORIENTED_EDGE('',*,*,#32349,.T.);
#47393=ORIENTED_EDGE('',*,*,#32351,.T.);
#47394=ORIENTED_EDGE('',*,*,#32343,.T.);
#47395=ORIENTED_EDGE('',*,*,#32627,.F.);
#47396=ORIENTED_EDGE('',*,*,#32358,.T.);
#47397=ORIENTED_EDGE('',*,*,#32360,.T.);
#47398=ORIENTED_EDGE('',*,*,#32352,.T.);
#47399=ORIENTED_EDGE('',*,*,#32628,.F.);
#47400=ORIENTED_EDGE('',*,*,#32367,.T.);
#47401=ORIENTED_EDGE('',*,*,#32369,.T.);
#47402=ORIENTED_EDGE('',*,*,#32361,.T.);
#47403=ORIENTED_EDGE('',*,*,#32629,.F.);
#47404=ORIENTED_EDGE('',*,*,#32376,.T.);
#47405=ORIENTED_EDGE('',*,*,#32378,.T.);
#47406=ORIENTED_EDGE('',*,*,#32370,.T.);
#47407=ORIENTED_EDGE('',*,*,#32630,.F.);
#47408=ORIENTED_EDGE('',*,*,#32385,.T.);
#47409=ORIENTED_EDGE('',*,*,#32387,.T.);
#47410=ORIENTED_EDGE('',*,*,#32379,.T.);
#47411=ORIENTED_EDGE('',*,*,#32631,.F.);
#47412=ORIENTED_EDGE('',*,*,#32394,.T.);
#47413=ORIENTED_EDGE('',*,*,#32396,.T.);
#47414=ORIENTED_EDGE('',*,*,#32388,.T.);
#47415=ORIENTED_EDGE('',*,*,#32632,.F.);
#47416=ORIENTED_EDGE('',*,*,#32403,.T.);
#47417=ORIENTED_EDGE('',*,*,#32405,.T.);
#47418=ORIENTED_EDGE('',*,*,#32397,.T.);
#47419=ORIENTED_EDGE('',*,*,#32633,.F.);
#47420=ORIENTED_EDGE('',*,*,#32412,.T.);
#47421=ORIENTED_EDGE('',*,*,#32414,.T.);
#47422=ORIENTED_EDGE('',*,*,#32406,.T.);
#47423=ORIENTED_EDGE('',*,*,#32634,.F.);
#47424=ORIENTED_EDGE('',*,*,#32421,.T.);
#47425=ORIENTED_EDGE('',*,*,#32423,.T.);
#47426=ORIENTED_EDGE('',*,*,#32415,.T.);
#47427=ORIENTED_EDGE('',*,*,#32635,.F.);
#47428=ORIENTED_EDGE('',*,*,#32431,.T.);
#47429=ORIENTED_EDGE('',*,*,#32433,.T.);
#47430=ORIENTED_EDGE('',*,*,#32636,.T.);
#47431=ORIENTED_EDGE('',*,*,#32270,.T.);
#47432=ORIENTED_EDGE('',*,*,#32636,.F.);
#47433=ORIENTED_EDGE('',*,*,#32434,.T.);
#47434=ORIENTED_EDGE('',*,*,#32424,.T.);
#47435=ORIENTED_EDGE('',*,*,#32637,.F.);
#47436=ORIENTED_EDGE('',*,*,#32441,.T.);
#47437=ORIENTED_EDGE('',*,*,#32443,.T.);
#47438=ORIENTED_EDGE('',*,*,#32435,.T.);
#47439=ORIENTED_EDGE('',*,*,#32638,.F.);
#47440=ORIENTED_EDGE('',*,*,#32450,.T.);
#47441=ORIENTED_EDGE('',*,*,#32452,.T.);
#47442=ORIENTED_EDGE('',*,*,#32444,.T.);
#47443=ORIENTED_EDGE('',*,*,#32639,.F.);
#47444=ORIENTED_EDGE('',*,*,#32459,.T.);
#47445=ORIENTED_EDGE('',*,*,#32461,.T.);
#47446=ORIENTED_EDGE('',*,*,#32453,.T.);
#47447=ORIENTED_EDGE('',*,*,#32640,.F.);
#47448=ORIENTED_EDGE('',*,*,#32468,.T.);
#47449=ORIENTED_EDGE('',*,*,#32470,.T.);
#47450=ORIENTED_EDGE('',*,*,#32462,.T.);
#47451=ORIENTED_EDGE('',*,*,#32641,.F.);
#47452=ORIENTED_EDGE('',*,*,#32477,.T.);
#47453=ORIENTED_EDGE('',*,*,#32479,.T.);
#47454=ORIENTED_EDGE('',*,*,#32471,.T.);
#47455=ORIENTED_EDGE('',*,*,#32642,.F.);
#47456=ORIENTED_EDGE('',*,*,#32486,.T.);
#47457=ORIENTED_EDGE('',*,*,#32488,.T.);
#47458=ORIENTED_EDGE('',*,*,#32480,.T.);
#47459=ORIENTED_EDGE('',*,*,#32643,.F.);
#47460=ORIENTED_EDGE('',*,*,#32495,.T.);
#47461=ORIENTED_EDGE('',*,*,#32497,.T.);
#47462=ORIENTED_EDGE('',*,*,#32489,.T.);
#47463=ORIENTED_EDGE('',*,*,#32644,.F.);
#47464=ORIENTED_EDGE('',*,*,#32504,.T.);
#47465=ORIENTED_EDGE('',*,*,#32506,.T.);
#47466=ORIENTED_EDGE('',*,*,#32498,.T.);
#47467=ORIENTED_EDGE('',*,*,#32645,.F.);
#47468=ORIENTED_EDGE('',*,*,#32513,.T.);
#47469=ORIENTED_EDGE('',*,*,#32515,.T.);
#47470=ORIENTED_EDGE('',*,*,#32507,.T.);
#47471=ORIENTED_EDGE('',*,*,#32646,.F.);
#47472=ORIENTED_EDGE('',*,*,#32522,.T.);
#47473=ORIENTED_EDGE('',*,*,#32524,.T.);
#47474=ORIENTED_EDGE('',*,*,#32516,.T.);
#47475=ORIENTED_EDGE('',*,*,#32647,.F.);
#47476=ORIENTED_EDGE('',*,*,#32531,.T.);
#47477=ORIENTED_EDGE('',*,*,#32533,.T.);
#47478=ORIENTED_EDGE('',*,*,#32525,.T.);
#47479=ORIENTED_EDGE('',*,*,#32648,.F.);
#47480=ORIENTED_EDGE('',*,*,#32540,.T.);
#47481=ORIENTED_EDGE('',*,*,#32542,.T.);
#47482=ORIENTED_EDGE('',*,*,#32534,.T.);
#47483=ORIENTED_EDGE('',*,*,#32649,.F.);
#47484=ORIENTED_EDGE('',*,*,#32549,.T.);
#47485=ORIENTED_EDGE('',*,*,#32551,.T.);
#47486=ORIENTED_EDGE('',*,*,#32543,.T.);
#47487=ORIENTED_EDGE('',*,*,#32650,.F.);
#47488=ORIENTED_EDGE('',*,*,#32558,.T.);
#47489=ORIENTED_EDGE('',*,*,#32560,.T.);
#47490=ORIENTED_EDGE('',*,*,#32552,.T.);
#47491=ORIENTED_EDGE('',*,*,#32651,.F.);
#47492=ORIENTED_EDGE('',*,*,#32567,.T.);
#47493=ORIENTED_EDGE('',*,*,#32569,.T.);
#47494=ORIENTED_EDGE('',*,*,#32561,.T.);
#47495=ORIENTED_EDGE('',*,*,#32652,.F.);
#47496=ORIENTED_EDGE('',*,*,#32576,.T.);
#47497=ORIENTED_EDGE('',*,*,#32578,.T.);
#47498=ORIENTED_EDGE('',*,*,#32570,.T.);
#47499=ORIENTED_EDGE('',*,*,#32653,.F.);
#47500=ORIENTED_EDGE('',*,*,#32585,.T.);
#47501=ORIENTED_EDGE('',*,*,#32587,.T.);
#47502=ORIENTED_EDGE('',*,*,#32579,.T.);
#47503=ORIENTED_EDGE('',*,*,#32654,.F.);
#47504=ORIENTED_EDGE('',*,*,#32594,.T.);
#47505=ORIENTED_EDGE('',*,*,#32596,.T.);
#47506=ORIENTED_EDGE('',*,*,#32591,.T.);
#47507=ORIENTED_EDGE('',*,*,#32655,.F.);
#47508=ORIENTED_EDGE('',*,*,#32277,.T.);
#47509=ORIENTED_EDGE('',*,*,#32279,.T.);
#47510=ORIENTED_EDGE('',*,*,#32656,.F.);
#47511=ORIENTED_EDGE('',*,*,#32657,.T.);
#47512=ORIENTED_EDGE('',*,*,#32430,.T.);
#47513=ORIENTED_EDGE('',*,*,#32635,.T.);
#47514=ORIENTED_EDGE('',*,*,#32419,.T.);
#47515=ORIENTED_EDGE('',*,*,#32634,.T.);
#47516=ORIENTED_EDGE('',*,*,#32410,.T.);
#47517=ORIENTED_EDGE('',*,*,#32633,.T.);
#47518=ORIENTED_EDGE('',*,*,#32401,.T.);
#47519=ORIENTED_EDGE('',*,*,#32632,.T.);
#47520=ORIENTED_EDGE('',*,*,#32392,.T.);
#47521=ORIENTED_EDGE('',*,*,#32631,.T.);
#47522=ORIENTED_EDGE('',*,*,#32383,.T.);
#47523=ORIENTED_EDGE('',*,*,#32630,.T.);
#47524=ORIENTED_EDGE('',*,*,#32374,.T.);
#47525=ORIENTED_EDGE('',*,*,#32629,.T.);
#47526=ORIENTED_EDGE('',*,*,#32365,.T.);
#47527=ORIENTED_EDGE('',*,*,#32628,.T.);
#47528=ORIENTED_EDGE('',*,*,#32356,.T.);
#47529=ORIENTED_EDGE('',*,*,#32627,.T.);
#47530=ORIENTED_EDGE('',*,*,#32347,.T.);
#47531=ORIENTED_EDGE('',*,*,#32626,.T.);
#47532=ORIENTED_EDGE('',*,*,#32338,.T.);
#47533=ORIENTED_EDGE('',*,*,#32625,.T.);
#47534=ORIENTED_EDGE('',*,*,#32329,.T.);
#47535=ORIENTED_EDGE('',*,*,#32624,.T.);
#47536=ORIENTED_EDGE('',*,*,#32320,.T.);
#47537=ORIENTED_EDGE('',*,*,#32623,.T.);
#47538=ORIENTED_EDGE('',*,*,#32311,.T.);
#47539=ORIENTED_EDGE('',*,*,#32622,.T.);
#47540=ORIENTED_EDGE('',*,*,#32302,.T.);
#47541=ORIENTED_EDGE('',*,*,#32621,.T.);
#47542=ORIENTED_EDGE('',*,*,#32293,.T.);
#47543=ORIENTED_EDGE('',*,*,#32620,.T.);
#47544=ORIENTED_EDGE('',*,*,#32284,.T.);
#47545=ORIENTED_EDGE('',*,*,#32619,.T.);
#47546=ORIENTED_EDGE('',*,*,#32275,.T.);
#47547=ORIENTED_EDGE('',*,*,#32655,.T.);
#47548=ORIENTED_EDGE('',*,*,#32588,.T.);
#47549=ORIENTED_EDGE('',*,*,#32654,.T.);
#47550=ORIENTED_EDGE('',*,*,#32583,.T.);
#47551=ORIENTED_EDGE('',*,*,#32653,.T.);
#47552=ORIENTED_EDGE('',*,*,#32574,.T.);
#47553=ORIENTED_EDGE('',*,*,#32652,.T.);
#47554=ORIENTED_EDGE('',*,*,#32565,.T.);
#47555=ORIENTED_EDGE('',*,*,#32651,.T.);
#47556=ORIENTED_EDGE('',*,*,#32556,.T.);
#47557=ORIENTED_EDGE('',*,*,#32650,.T.);
#47558=ORIENTED_EDGE('',*,*,#32547,.T.);
#47559=ORIENTED_EDGE('',*,*,#32649,.T.);
#47560=ORIENTED_EDGE('',*,*,#32538,.T.);
#47561=ORIENTED_EDGE('',*,*,#32648,.T.);
#47562=ORIENTED_EDGE('',*,*,#32529,.T.);
#47563=ORIENTED_EDGE('',*,*,#32647,.T.);
#47564=ORIENTED_EDGE('',*,*,#32520,.T.);
#47565=ORIENTED_EDGE('',*,*,#32646,.T.);
#47566=ORIENTED_EDGE('',*,*,#32511,.T.);
#47567=ORIENTED_EDGE('',*,*,#32645,.T.);
#47568=ORIENTED_EDGE('',*,*,#32502,.T.);
#47569=ORIENTED_EDGE('',*,*,#32644,.T.);
#47570=ORIENTED_EDGE('',*,*,#32493,.T.);
#47571=ORIENTED_EDGE('',*,*,#32643,.T.);
#47572=ORIENTED_EDGE('',*,*,#32484,.T.);
#47573=ORIENTED_EDGE('',*,*,#32642,.T.);
#47574=ORIENTED_EDGE('',*,*,#32475,.T.);
#47575=ORIENTED_EDGE('',*,*,#32641,.T.);
#47576=ORIENTED_EDGE('',*,*,#32466,.T.);
#47577=ORIENTED_EDGE('',*,*,#32640,.T.);
#47578=ORIENTED_EDGE('',*,*,#32457,.T.);
#47579=ORIENTED_EDGE('',*,*,#32639,.T.);
#47580=ORIENTED_EDGE('',*,*,#32448,.T.);
#47581=ORIENTED_EDGE('',*,*,#32638,.T.);
#47582=ORIENTED_EDGE('',*,*,#32439,.T.);
#47583=ORIENTED_EDGE('',*,*,#32637,.T.);
#47584=ORIENTED_EDGE('',*,*,#32428,.T.);
#47585=ORIENTED_EDGE('',*,*,#32657,.F.);
#47586=ORIENTED_EDGE('',*,*,#32656,.T.);
#47587=ORIENTED_EDGE('',*,*,#32609,.T.);
#47588=ORIENTED_EDGE('',*,*,#32612,.T.);
#47589=ORIENTED_EDGE('',*,*,#32615,.T.);
#47590=ORIENTED_EDGE('',*,*,#32599,.T.);
#47591=ORIENTED_EDGE('',*,*,#32603,.T.);
#47592=ORIENTED_EDGE('',*,*,#32606,.T.);
#47593=ORIENTED_EDGE('',*,*,#32658,.T.);
#47594=ORIENTED_EDGE('',*,*,#32659,.T.);
#47595=ORIENTED_EDGE('',*,*,#32660,.T.);
#47596=ORIENTED_EDGE('',*,*,#32661,.T.);
#47597=ORIENTED_EDGE('',*,*,#32659,.F.);
#47598=ORIENTED_EDGE('',*,*,#32661,.F.);
#47599=ORIENTED_EDGE('',*,*,#32662,.T.);
#47600=ORIENTED_EDGE('',*,*,#32663,.T.);
#47601=ORIENTED_EDGE('',*,*,#32662,.F.);
#47602=ORIENTED_EDGE('',*,*,#32660,.F.);
#47603=ORIENTED_EDGE('',*,*,#32658,.F.);
#47604=ORIENTED_EDGE('',*,*,#32664,.F.);
#47605=ORIENTED_EDGE('',*,*,#32665,.F.);
#47606=ORIENTED_EDGE('',*,*,#32666,.T.);
#47607=ORIENTED_EDGE('',*,*,#32664,.T.);
#47608=ORIENTED_EDGE('',*,*,#32666,.F.);
#47609=ORIENTED_EDGE('',*,*,#32663,.F.);
#47610=ORIENTED_EDGE('',*,*,#32667,.T.);
#47611=ORIENTED_EDGE('',*,*,#32665,.T.);
#47612=ORIENTED_EDGE('',*,*,#32667,.F.);
#47613=ORIENTED_EDGE('',*,*,#32668,.F.);
#47614=ORIENTED_EDGE('',*,*,#32669,.T.);
#47615=ORIENTED_EDGE('',*,*,#32670,.T.);
#47616=ORIENTED_EDGE('',*,*,#32671,.T.);
#47617=ORIENTED_EDGE('',*,*,#32672,.F.);
#47618=ORIENTED_EDGE('',*,*,#32673,.T.);
#47619=ORIENTED_EDGE('',*,*,#32668,.T.);
#47620=ORIENTED_EDGE('',*,*,#32674,.T.);
#47621=ORIENTED_EDGE('',*,*,#32675,.F.);
#47622=ORIENTED_EDGE('',*,*,#32676,.T.);
#47623=ORIENTED_EDGE('',*,*,#32672,.T.);
#47624=ORIENTED_EDGE('',*,*,#32677,.T.);
#47625=ORIENTED_EDGE('',*,*,#32678,.F.);
#47626=ORIENTED_EDGE('',*,*,#32679,.T.);
#47627=ORIENTED_EDGE('',*,*,#32675,.T.);
#47628=ORIENTED_EDGE('',*,*,#32680,.T.);
#47629=ORIENTED_EDGE('',*,*,#32681,.F.);
#47630=ORIENTED_EDGE('',*,*,#32682,.T.);
#47631=ORIENTED_EDGE('',*,*,#32678,.T.);
#47632=ORIENTED_EDGE('',*,*,#32683,.T.);
#47633=ORIENTED_EDGE('',*,*,#32684,.F.);
#47634=ORIENTED_EDGE('',*,*,#32685,.T.);
#47635=ORIENTED_EDGE('',*,*,#32681,.T.);
#47636=ORIENTED_EDGE('',*,*,#32686,.T.);
#47637=ORIENTED_EDGE('',*,*,#32687,.F.);
#47638=ORIENTED_EDGE('',*,*,#32688,.T.);
#47639=ORIENTED_EDGE('',*,*,#32684,.T.);
#47640=ORIENTED_EDGE('',*,*,#32689,.T.);
#47641=ORIENTED_EDGE('',*,*,#32690,.F.);
#47642=ORIENTED_EDGE('',*,*,#32691,.T.);
#47643=ORIENTED_EDGE('',*,*,#32687,.T.);
#47644=ORIENTED_EDGE('',*,*,#32692,.T.);
#47645=ORIENTED_EDGE('',*,*,#32693,.F.);
#47646=ORIENTED_EDGE('',*,*,#32694,.T.);
#47647=ORIENTED_EDGE('',*,*,#32690,.T.);
#47648=ORIENTED_EDGE('',*,*,#32695,.T.);
#47649=ORIENTED_EDGE('',*,*,#32696,.F.);
#47650=ORIENTED_EDGE('',*,*,#32697,.T.);
#47651=ORIENTED_EDGE('',*,*,#32693,.T.);
#47652=ORIENTED_EDGE('',*,*,#32698,.T.);
#47653=ORIENTED_EDGE('',*,*,#32699,.F.);
#47654=ORIENTED_EDGE('',*,*,#32700,.T.);
#47655=ORIENTED_EDGE('',*,*,#32696,.T.);
#47656=ORIENTED_EDGE('',*,*,#32701,.T.);
#47657=ORIENTED_EDGE('',*,*,#32702,.F.);
#47658=ORIENTED_EDGE('',*,*,#32703,.T.);
#47659=ORIENTED_EDGE('',*,*,#32699,.T.);
#47660=ORIENTED_EDGE('',*,*,#32704,.T.);
#47661=ORIENTED_EDGE('',*,*,#32705,.F.);
#47662=ORIENTED_EDGE('',*,*,#32706,.T.);
#47663=ORIENTED_EDGE('',*,*,#32702,.T.);
#47664=ORIENTED_EDGE('',*,*,#32707,.T.);
#47665=ORIENTED_EDGE('',*,*,#32708,.F.);
#47666=ORIENTED_EDGE('',*,*,#32709,.T.);
#47667=ORIENTED_EDGE('',*,*,#32705,.T.);
#47668=ORIENTED_EDGE('',*,*,#32710,.T.);
#47669=ORIENTED_EDGE('',*,*,#32711,.F.);
#47670=ORIENTED_EDGE('',*,*,#32712,.T.);
#47671=ORIENTED_EDGE('',*,*,#32708,.T.);
#47672=ORIENTED_EDGE('',*,*,#32713,.T.);
#47673=ORIENTED_EDGE('',*,*,#32714,.F.);
#47674=ORIENTED_EDGE('',*,*,#32715,.T.);
#47675=ORIENTED_EDGE('',*,*,#32711,.T.);
#47676=ORIENTED_EDGE('',*,*,#32716,.T.);
#47677=ORIENTED_EDGE('',*,*,#32717,.F.);
#47678=ORIENTED_EDGE('',*,*,#32718,.T.);
#47679=ORIENTED_EDGE('',*,*,#32714,.T.);
#47680=ORIENTED_EDGE('',*,*,#32719,.T.);
#47681=ORIENTED_EDGE('',*,*,#32720,.F.);
#47682=ORIENTED_EDGE('',*,*,#32721,.T.);
#47683=ORIENTED_EDGE('',*,*,#32717,.T.);
#47684=ORIENTED_EDGE('',*,*,#32722,.T.);
#47685=ORIENTED_EDGE('',*,*,#32723,.F.);
#47686=ORIENTED_EDGE('',*,*,#32724,.T.);
#47687=ORIENTED_EDGE('',*,*,#32720,.T.);
#47688=ORIENTED_EDGE('',*,*,#32725,.T.);
#47689=ORIENTED_EDGE('',*,*,#32726,.F.);
#47690=ORIENTED_EDGE('',*,*,#32727,.T.);
#47691=ORIENTED_EDGE('',*,*,#32723,.T.);
#47692=ORIENTED_EDGE('',*,*,#32728,.T.);
#47693=ORIENTED_EDGE('',*,*,#32729,.F.);
#47694=ORIENTED_EDGE('',*,*,#32730,.T.);
#47695=ORIENTED_EDGE('',*,*,#32726,.T.);
#47696=ORIENTED_EDGE('',*,*,#32731,.T.);
#47697=ORIENTED_EDGE('',*,*,#32732,.F.);
#47698=ORIENTED_EDGE('',*,*,#32733,.T.);
#47699=ORIENTED_EDGE('',*,*,#32729,.T.);
#47700=ORIENTED_EDGE('',*,*,#32734,.T.);
#47701=ORIENTED_EDGE('',*,*,#32735,.F.);
#47702=ORIENTED_EDGE('',*,*,#32736,.T.);
#47703=ORIENTED_EDGE('',*,*,#32732,.T.);
#47704=ORIENTED_EDGE('',*,*,#32737,.T.);
#47705=ORIENTED_EDGE('',*,*,#32738,.F.);
#47706=ORIENTED_EDGE('',*,*,#32739,.T.);
#47707=ORIENTED_EDGE('',*,*,#32740,.F.);
#47708=ORIENTED_EDGE('',*,*,#32741,.F.);
#47709=ORIENTED_EDGE('',*,*,#32742,.F.);
#47710=ORIENTED_EDGE('',*,*,#32743,.T.);
#47711=ORIENTED_EDGE('',*,*,#32738,.T.);
#47712=ORIENTED_EDGE('',*,*,#32744,.F.);
#47713=ORIENTED_EDGE('',*,*,#32745,.F.);
#47714=ORIENTED_EDGE('',*,*,#32746,.T.);
#47715=ORIENTED_EDGE('',*,*,#32742,.T.);
#47716=ORIENTED_EDGE('',*,*,#32747,.F.);
#47717=ORIENTED_EDGE('',*,*,#32748,.F.);
#47718=ORIENTED_EDGE('',*,*,#32749,.T.);
#47719=ORIENTED_EDGE('',*,*,#32745,.T.);
#47720=ORIENTED_EDGE('',*,*,#32750,.F.);
#47721=ORIENTED_EDGE('',*,*,#32751,.F.);
#47722=ORIENTED_EDGE('',*,*,#32752,.T.);
#47723=ORIENTED_EDGE('',*,*,#32748,.T.);
#47724=ORIENTED_EDGE('',*,*,#32753,.F.);
#47725=ORIENTED_EDGE('',*,*,#32754,.F.);
#47726=ORIENTED_EDGE('',*,*,#32755,.T.);
#47727=ORIENTED_EDGE('',*,*,#32751,.T.);
#47728=ORIENTED_EDGE('',*,*,#32756,.F.);
#47729=ORIENTED_EDGE('',*,*,#32757,.F.);
#47730=ORIENTED_EDGE('',*,*,#32758,.T.);
#47731=ORIENTED_EDGE('',*,*,#32754,.T.);
#47732=ORIENTED_EDGE('',*,*,#32759,.F.);
#47733=ORIENTED_EDGE('',*,*,#32760,.F.);
#47734=ORIENTED_EDGE('',*,*,#32761,.T.);
#47735=ORIENTED_EDGE('',*,*,#32757,.T.);
#47736=ORIENTED_EDGE('',*,*,#32762,.F.);
#47737=ORIENTED_EDGE('',*,*,#32763,.F.);
#47738=ORIENTED_EDGE('',*,*,#32764,.T.);
#47739=ORIENTED_EDGE('',*,*,#32760,.T.);
#47740=ORIENTED_EDGE('',*,*,#32765,.F.);
#47741=ORIENTED_EDGE('',*,*,#32766,.F.);
#47742=ORIENTED_EDGE('',*,*,#32767,.T.);
#47743=ORIENTED_EDGE('',*,*,#32763,.T.);
#47744=ORIENTED_EDGE('',*,*,#32768,.F.);
#47745=ORIENTED_EDGE('',*,*,#32769,.F.);
#47746=ORIENTED_EDGE('',*,*,#32770,.T.);
#47747=ORIENTED_EDGE('',*,*,#32766,.T.);
#47748=ORIENTED_EDGE('',*,*,#32771,.F.);
#47749=ORIENTED_EDGE('',*,*,#32772,.F.);
#47750=ORIENTED_EDGE('',*,*,#32773,.T.);
#47751=ORIENTED_EDGE('',*,*,#32769,.T.);
#47752=ORIENTED_EDGE('',*,*,#32774,.F.);
#47753=ORIENTED_EDGE('',*,*,#32775,.F.);
#47754=ORIENTED_EDGE('',*,*,#32776,.T.);
#47755=ORIENTED_EDGE('',*,*,#32772,.T.);
#47756=ORIENTED_EDGE('',*,*,#32777,.F.);
#47757=ORIENTED_EDGE('',*,*,#32778,.F.);
#47758=ORIENTED_EDGE('',*,*,#32779,.T.);
#47759=ORIENTED_EDGE('',*,*,#32775,.T.);
#47760=ORIENTED_EDGE('',*,*,#32780,.F.);
#47761=ORIENTED_EDGE('',*,*,#32781,.F.);
#47762=ORIENTED_EDGE('',*,*,#32782,.T.);
#47763=ORIENTED_EDGE('',*,*,#32778,.T.);
#47764=ORIENTED_EDGE('',*,*,#32783,.F.);
#47765=ORIENTED_EDGE('',*,*,#32784,.F.);
#47766=ORIENTED_EDGE('',*,*,#32785,.T.);
#47767=ORIENTED_EDGE('',*,*,#32781,.T.);
#47768=ORIENTED_EDGE('',*,*,#32786,.F.);
#47769=ORIENTED_EDGE('',*,*,#32787,.F.);
#47770=ORIENTED_EDGE('',*,*,#32788,.T.);
#47771=ORIENTED_EDGE('',*,*,#32784,.T.);
#47772=ORIENTED_EDGE('',*,*,#32789,.F.);
#47773=ORIENTED_EDGE('',*,*,#32790,.F.);
#47774=ORIENTED_EDGE('',*,*,#32791,.T.);
#47775=ORIENTED_EDGE('',*,*,#32787,.T.);
#47776=ORIENTED_EDGE('',*,*,#32792,.F.);
#47777=ORIENTED_EDGE('',*,*,#32793,.F.);
#47778=ORIENTED_EDGE('',*,*,#32794,.T.);
#47779=ORIENTED_EDGE('',*,*,#32790,.T.);
#47780=ORIENTED_EDGE('',*,*,#32795,.F.);
#47781=ORIENTED_EDGE('',*,*,#32796,.F.);
#47782=ORIENTED_EDGE('',*,*,#32797,.T.);
#47783=ORIENTED_EDGE('',*,*,#32793,.T.);
#47784=ORIENTED_EDGE('',*,*,#32798,.F.);
#47785=ORIENTED_EDGE('',*,*,#32799,.F.);
#47786=ORIENTED_EDGE('',*,*,#32800,.T.);
#47787=ORIENTED_EDGE('',*,*,#32796,.T.);
#47788=ORIENTED_EDGE('',*,*,#32801,.F.);
#47789=ORIENTED_EDGE('',*,*,#32802,.F.);
#47790=ORIENTED_EDGE('',*,*,#32803,.T.);
#47791=ORIENTED_EDGE('',*,*,#32799,.T.);
#47792=ORIENTED_EDGE('',*,*,#32804,.F.);
#47793=ORIENTED_EDGE('',*,*,#32805,.F.);
#47794=ORIENTED_EDGE('',*,*,#32806,.T.);
#47795=ORIENTED_EDGE('',*,*,#32802,.T.);
#47796=ORIENTED_EDGE('',*,*,#32807,.F.);
#47797=ORIENTED_EDGE('',*,*,#32740,.T.);
#47798=ORIENTED_EDGE('',*,*,#32808,.T.);
#47799=ORIENTED_EDGE('',*,*,#32809,.F.);
#47800=ORIENTED_EDGE('',*,*,#32810,.F.);
#47801=ORIENTED_EDGE('',*,*,#32811,.T.);
#47802=ORIENTED_EDGE('',*,*,#32811,.F.);
#47803=ORIENTED_EDGE('',*,*,#32812,.F.);
#47804=ORIENTED_EDGE('',*,*,#32737,.F.);
#47805=ORIENTED_EDGE('',*,*,#32734,.F.);
#47806=ORIENTED_EDGE('',*,*,#32731,.F.);
#47807=ORIENTED_EDGE('',*,*,#32728,.F.);
#47808=ORIENTED_EDGE('',*,*,#32725,.F.);
#47809=ORIENTED_EDGE('',*,*,#32722,.F.);
#47810=ORIENTED_EDGE('',*,*,#32719,.F.);
#47811=ORIENTED_EDGE('',*,*,#32716,.F.);
#47812=ORIENTED_EDGE('',*,*,#32713,.F.);
#47813=ORIENTED_EDGE('',*,*,#32710,.F.);
#47814=ORIENTED_EDGE('',*,*,#32707,.F.);
#47815=ORIENTED_EDGE('',*,*,#32704,.F.);
#47816=ORIENTED_EDGE('',*,*,#32701,.F.);
#47817=ORIENTED_EDGE('',*,*,#32698,.F.);
#47818=ORIENTED_EDGE('',*,*,#32695,.F.);
#47819=ORIENTED_EDGE('',*,*,#32692,.F.);
#47820=ORIENTED_EDGE('',*,*,#32689,.F.);
#47821=ORIENTED_EDGE('',*,*,#32686,.F.);
#47822=ORIENTED_EDGE('',*,*,#32683,.F.);
#47823=ORIENTED_EDGE('',*,*,#32680,.F.);
#47824=ORIENTED_EDGE('',*,*,#32677,.F.);
#47825=ORIENTED_EDGE('',*,*,#32674,.F.);
#47826=ORIENTED_EDGE('',*,*,#32671,.F.);
#47827=ORIENTED_EDGE('',*,*,#32813,.F.);
#47828=ORIENTED_EDGE('',*,*,#32814,.T.);
#47829=ORIENTED_EDGE('',*,*,#32807,.T.);
#47830=ORIENTED_EDGE('',*,*,#32804,.T.);
#47831=ORIENTED_EDGE('',*,*,#32801,.T.);
#47832=ORIENTED_EDGE('',*,*,#32798,.T.);
#47833=ORIENTED_EDGE('',*,*,#32795,.T.);
#47834=ORIENTED_EDGE('',*,*,#32792,.T.);
#47835=ORIENTED_EDGE('',*,*,#32789,.T.);
#47836=ORIENTED_EDGE('',*,*,#32786,.T.);
#47837=ORIENTED_EDGE('',*,*,#32783,.T.);
#47838=ORIENTED_EDGE('',*,*,#32780,.T.);
#47839=ORIENTED_EDGE('',*,*,#32777,.T.);
#47840=ORIENTED_EDGE('',*,*,#32774,.T.);
#47841=ORIENTED_EDGE('',*,*,#32771,.T.);
#47842=ORIENTED_EDGE('',*,*,#32768,.T.);
#47843=ORIENTED_EDGE('',*,*,#32765,.T.);
#47844=ORIENTED_EDGE('',*,*,#32762,.T.);
#47845=ORIENTED_EDGE('',*,*,#32759,.T.);
#47846=ORIENTED_EDGE('',*,*,#32756,.T.);
#47847=ORIENTED_EDGE('',*,*,#32753,.T.);
#47848=ORIENTED_EDGE('',*,*,#32750,.T.);
#47849=ORIENTED_EDGE('',*,*,#32747,.T.);
#47850=ORIENTED_EDGE('',*,*,#32744,.T.);
#47851=ORIENTED_EDGE('',*,*,#32741,.T.);
#47852=ORIENTED_EDGE('',*,*,#32815,.T.);
#47853=ORIENTED_EDGE('',*,*,#32816,.T.);
#47854=ORIENTED_EDGE('',*,*,#32817,.T.);
#47855=ORIENTED_EDGE('',*,*,#32818,.T.);
#47856=ORIENTED_EDGE('',*,*,#32813,.T.);
#47857=ORIENTED_EDGE('',*,*,#32805,.T.);
#47858=ORIENTED_EDGE('',*,*,#32814,.F.);
#47859=ORIENTED_EDGE('',*,*,#32818,.F.);
#47860=ORIENTED_EDGE('',*,*,#32819,.T.);
#47861=ORIENTED_EDGE('',*,*,#32808,.F.);
#47862=ORIENTED_EDGE('',*,*,#32739,.F.);
#47863=ORIENTED_EDGE('',*,*,#32743,.F.);
#47864=ORIENTED_EDGE('',*,*,#32746,.F.);
#47865=ORIENTED_EDGE('',*,*,#32749,.F.);
#47866=ORIENTED_EDGE('',*,*,#32752,.F.);
#47867=ORIENTED_EDGE('',*,*,#32755,.F.);
#47868=ORIENTED_EDGE('',*,*,#32758,.F.);
#47869=ORIENTED_EDGE('',*,*,#32761,.F.);
#47870=ORIENTED_EDGE('',*,*,#32764,.F.);
#47871=ORIENTED_EDGE('',*,*,#32767,.F.);
#47872=ORIENTED_EDGE('',*,*,#32770,.F.);
#47873=ORIENTED_EDGE('',*,*,#32773,.F.);
#47874=ORIENTED_EDGE('',*,*,#32776,.F.);
#47875=ORIENTED_EDGE('',*,*,#32779,.F.);
#47876=ORIENTED_EDGE('',*,*,#32782,.F.);
#47877=ORIENTED_EDGE('',*,*,#32785,.F.);
#47878=ORIENTED_EDGE('',*,*,#32788,.F.);
#47879=ORIENTED_EDGE('',*,*,#32791,.F.);
#47880=ORIENTED_EDGE('',*,*,#32794,.F.);
#47881=ORIENTED_EDGE('',*,*,#32797,.F.);
#47882=ORIENTED_EDGE('',*,*,#32800,.F.);
#47883=ORIENTED_EDGE('',*,*,#32803,.F.);
#47884=ORIENTED_EDGE('',*,*,#32806,.F.);
#47885=ORIENTED_EDGE('',*,*,#32819,.F.);
#47886=ORIENTED_EDGE('',*,*,#32817,.F.);
#47887=ORIENTED_EDGE('',*,*,#32669,.F.);
#47888=ORIENTED_EDGE('',*,*,#32673,.F.);
#47889=ORIENTED_EDGE('',*,*,#32676,.F.);
#47890=ORIENTED_EDGE('',*,*,#32679,.F.);
#47891=ORIENTED_EDGE('',*,*,#32682,.F.);
#47892=ORIENTED_EDGE('',*,*,#32685,.F.);
#47893=ORIENTED_EDGE('',*,*,#32688,.F.);
#47894=ORIENTED_EDGE('',*,*,#32691,.F.);
#47895=ORIENTED_EDGE('',*,*,#32694,.F.);
#47896=ORIENTED_EDGE('',*,*,#32697,.F.);
#47897=ORIENTED_EDGE('',*,*,#32700,.F.);
#47898=ORIENTED_EDGE('',*,*,#32703,.F.);
#47899=ORIENTED_EDGE('',*,*,#32706,.F.);
#47900=ORIENTED_EDGE('',*,*,#32709,.F.);
#47901=ORIENTED_EDGE('',*,*,#32712,.F.);
#47902=ORIENTED_EDGE('',*,*,#32715,.F.);
#47903=ORIENTED_EDGE('',*,*,#32718,.F.);
#47904=ORIENTED_EDGE('',*,*,#32721,.F.);
#47905=ORIENTED_EDGE('',*,*,#32724,.F.);
#47906=ORIENTED_EDGE('',*,*,#32727,.F.);
#47907=ORIENTED_EDGE('',*,*,#32730,.F.);
#47908=ORIENTED_EDGE('',*,*,#32733,.F.);
#47909=ORIENTED_EDGE('',*,*,#32736,.F.);
#47910=ORIENTED_EDGE('',*,*,#32820,.F.);
#47911=ORIENTED_EDGE('',*,*,#32810,.T.);
#47912=ORIENTED_EDGE('',*,*,#32821,.T.);
#47913=ORIENTED_EDGE('',*,*,#32822,.T.);
#47914=ORIENTED_EDGE('',*,*,#32821,.F.);
#47915=ORIENTED_EDGE('',*,*,#32809,.T.);
#47916=ORIENTED_EDGE('',*,*,#32823,.T.);
#47917=ORIENTED_EDGE('',*,*,#32735,.T.);
#47918=ORIENTED_EDGE('',*,*,#32812,.T.);
#47919=ORIENTED_EDGE('',*,*,#32823,.F.);
#47920=ORIENTED_EDGE('',*,*,#32820,.T.);
#47921=ORIENTED_EDGE('',*,*,#32824,.F.);
#47922=ORIENTED_EDGE('',*,*,#32822,.F.);
#47923=ORIENTED_EDGE('',*,*,#32825,.F.);
#47924=ORIENTED_EDGE('',*,*,#32826,.F.);
#47925=ORIENTED_EDGE('',*,*,#32827,.F.);
#47926=ORIENTED_EDGE('',*,*,#32828,.F.);
#47927=ORIENTED_EDGE('',*,*,#32829,.F.);
#47928=ORIENTED_EDGE('',*,*,#32830,.T.);
#47929=ORIENTED_EDGE('',*,*,#32831,.F.);
#47930=ORIENTED_EDGE('',*,*,#32830,.F.);
#47931=ORIENTED_EDGE('',*,*,#32832,.F.);
#47932=ORIENTED_EDGE('',*,*,#32828,.T.);
#47933=ORIENTED_EDGE('',*,*,#32833,.F.);
#47934=ORIENTED_EDGE('',*,*,#32834,.T.);
#47935=ORIENTED_EDGE('',*,*,#32835,.T.);
#47936=ORIENTED_EDGE('',*,*,#32827,.T.);
#47937=ORIENTED_EDGE('',*,*,#32836,.F.);
#47938=ORIENTED_EDGE('',*,*,#32837,.T.);
#47939=ORIENTED_EDGE('',*,*,#32833,.T.);
#47940=ORIENTED_EDGE('',*,*,#32826,.T.);
#47941=ORIENTED_EDGE('',*,*,#32838,.F.);
#47942=ORIENTED_EDGE('',*,*,#32839,.T.);
#47943=ORIENTED_EDGE('',*,*,#32836,.T.);
#47944=ORIENTED_EDGE('',*,*,#32840,.F.);
#47945=ORIENTED_EDGE('',*,*,#32841,.T.);
#47946=ORIENTED_EDGE('',*,*,#32824,.T.);
#47947=ORIENTED_EDGE('',*,*,#32841,.F.);
#47948=ORIENTED_EDGE('',*,*,#32842,.F.);
#47949=ORIENTED_EDGE('',*,*,#32815,.F.);
#47950=ORIENTED_EDGE('',*,*,#32670,.F.);
#47951=ORIENTED_EDGE('',*,*,#32816,.F.);
#47952=ORIENTED_EDGE('',*,*,#32843,.T.);
#47953=ORIENTED_EDGE('',*,*,#32842,.T.);
#47954=ORIENTED_EDGE('',*,*,#32843,.F.);
#47955=ORIENTED_EDGE('',*,*,#32825,.T.);
#47956=ORIENTED_EDGE('',*,*,#32844,.F.);
#47957=ORIENTED_EDGE('',*,*,#32845,.T.);
#47958=ORIENTED_EDGE('',*,*,#32838,.T.);
#47959=ORIENTED_EDGE('',*,*,#32832,.T.);
#47960=ORIENTED_EDGE('',*,*,#32846,.F.);
#47961=ORIENTED_EDGE('',*,*,#32847,.T.);
#47962=ORIENTED_EDGE('',*,*,#32844,.T.);
#47963=ORIENTED_EDGE('',*,*,#32829,.T.);
#47964=ORIENTED_EDGE('',*,*,#32835,.F.);
#47965=ORIENTED_EDGE('',*,*,#32848,.T.);
#47966=ORIENTED_EDGE('',*,*,#32846,.T.);
#47967=ORIENTED_EDGE('',*,*,#32831,.T.);
#47968=ORIENTED_EDGE('',*,*,#32839,.F.);
#47969=ORIENTED_EDGE('',*,*,#32845,.F.);
#47970=ORIENTED_EDGE('',*,*,#32847,.F.);
#47971=ORIENTED_EDGE('',*,*,#32848,.F.);
#47972=ORIENTED_EDGE('',*,*,#32834,.F.);
#47973=ORIENTED_EDGE('',*,*,#32837,.F.);
#47974=ORIENTED_EDGE('',*,*,#32840,.T.);
#47975=ORIENTED_EDGE('',*,*,#32849,.F.);
#47976=ORIENTED_EDGE('',*,*,#32850,.T.);
#47977=ORIENTED_EDGE('',*,*,#32851,.T.);
#47978=ORIENTED_EDGE('',*,*,#32850,.F.);
#47979=ORIENTED_EDGE('',*,*,#32852,.F.);
#47980=ORIENTED_EDGE('',*,*,#32853,.T.);
#47981=ORIENTED_EDGE('',*,*,#32849,.T.);
#47982=ORIENTED_EDGE('',*,*,#32853,.F.);
#47983=ORIENTED_EDGE('',*,*,#32854,.F.);
#47984=ORIENTED_EDGE('',*,*,#32855,.T.);
#47985=ORIENTED_EDGE('',*,*,#32852,.T.);
#47986=ORIENTED_EDGE('',*,*,#32855,.F.);
#47987=ORIENTED_EDGE('',*,*,#32854,.T.);
#47988=ORIENTED_EDGE('',*,*,#32856,.F.);
#47989=ORIENTED_EDGE('',*,*,#32856,.T.);
#47990=ORIENTED_EDGE('',*,*,#32857,.T.);
#47991=ORIENTED_EDGE('',*,*,#32858,.F.);
#47992=ORIENTED_EDGE('',*,*,#32857,.F.);
#47993=ORIENTED_EDGE('',*,*,#32858,.T.);
#47994=ORIENTED_EDGE('',*,*,#32859,.T.);
#47995=ORIENTED_EDGE('',*,*,#32860,.F.);
#47996=ORIENTED_EDGE('',*,*,#32859,.F.);
#47997=ORIENTED_EDGE('',*,*,#32860,.T.);
#47998=ORIENTED_EDGE('',*,*,#32861,.T.);
#47999=ORIENTED_EDGE('',*,*,#32862,.F.);
#48000=ORIENTED_EDGE('',*,*,#32861,.F.);
#48001=ORIENTED_EDGE('',*,*,#32851,.F.);
#48002=ORIENTED_EDGE('',*,*,#32862,.T.);
#48003=ORIENTED_EDGE('',*,*,#32863,.F.);
#48004=ORIENTED_EDGE('',*,*,#32864,.F.);
#48005=ORIENTED_EDGE('',*,*,#32865,.T.);
#48006=ORIENTED_EDGE('',*,*,#32866,.F.);
#48007=ORIENTED_EDGE('',*,*,#32867,.F.);
#48008=ORIENTED_EDGE('',*,*,#32868,.F.);
#48009=ORIENTED_EDGE('',*,*,#32869,.F.);
#48010=ORIENTED_EDGE('',*,*,#32870,.F.);
#48011=ORIENTED_EDGE('',*,*,#32871,.F.);
#48012=ORIENTED_EDGE('',*,*,#32872,.F.);
#48013=ORIENTED_EDGE('',*,*,#32873,.F.);
#48014=ORIENTED_EDGE('',*,*,#32874,.F.);
#48015=ORIENTED_EDGE('',*,*,#32875,.F.);
#48016=ORIENTED_EDGE('',*,*,#32876,.F.);
#48017=ORIENTED_EDGE('',*,*,#32877,.F.);
#48018=ORIENTED_EDGE('',*,*,#32878,.F.);
#48019=ORIENTED_EDGE('',*,*,#32879,.F.);
#48020=ORIENTED_EDGE('',*,*,#32865,.F.);
#48021=ORIENTED_EDGE('',*,*,#32880,.F.);
#48022=ORIENTED_EDGE('',*,*,#32881,.F.);
#48023=ORIENTED_EDGE('',*,*,#32871,.T.);
#48024=ORIENTED_EDGE('',*,*,#32882,.T.);
#48025=ORIENTED_EDGE('',*,*,#32866,.T.);
#48026=ORIENTED_EDGE('',*,*,#32879,.T.);
#48027=ORIENTED_EDGE('',*,*,#32883,.T.);
#48028=ORIENTED_EDGE('',*,*,#32863,.T.);
#48029=ORIENTED_EDGE('',*,*,#32882,.F.);
#48030=ORIENTED_EDGE('',*,*,#32870,.T.);
#48031=ORIENTED_EDGE('',*,*,#32884,.F.);
#48032=ORIENTED_EDGE('',*,*,#32869,.T.);
#48033=ORIENTED_EDGE('',*,*,#32885,.T.);
#48034=ORIENTED_EDGE('',*,*,#32880,.T.);
#48035=ORIENTED_EDGE('',*,*,#32864,.T.);
#48036=ORIENTED_EDGE('',*,*,#32884,.T.);
#48037=ORIENTED_EDGE('',*,*,#32868,.T.);
#48038=ORIENTED_EDGE('',*,*,#32886,.F.);
#48039=ORIENTED_EDGE('',*,*,#32881,.T.);
#48040=ORIENTED_EDGE('',*,*,#32885,.F.);
#48041=ORIENTED_EDGE('',*,*,#32867,.T.);
#48042=ORIENTED_EDGE('',*,*,#32887,.T.);
#48043=ORIENTED_EDGE('',*,*,#32875,.T.);
#48044=ORIENTED_EDGE('',*,*,#32886,.T.);
#48045=ORIENTED_EDGE('',*,*,#32874,.T.);
#48046=ORIENTED_EDGE('',*,*,#32888,.F.);
#48047=ORIENTED_EDGE('',*,*,#32876,.T.);
#48048=ORIENTED_EDGE('',*,*,#32887,.F.);
#48049=ORIENTED_EDGE('',*,*,#32873,.T.);
#48050=ORIENTED_EDGE('',*,*,#32889,.T.);
#48051=ORIENTED_EDGE('',*,*,#32877,.T.);
#48052=ORIENTED_EDGE('',*,*,#32888,.T.);
#48053=ORIENTED_EDGE('',*,*,#32872,.T.);
#48054=ORIENTED_EDGE('',*,*,#32883,.F.);
#48055=ORIENTED_EDGE('',*,*,#32878,.T.);
#48056=ORIENTED_EDGE('',*,*,#32889,.F.);
#48057=ORIENTED_EDGE('',*,*,#32890,.F.);
#48058=ORIENTED_EDGE('',*,*,#32891,.T.);
#48059=ORIENTED_EDGE('',*,*,#32892,.T.);
#48060=ORIENTED_EDGE('',*,*,#32891,.F.);
#48061=ORIENTED_EDGE('',*,*,#32892,.F.);
#48062=ORIENTED_EDGE('',*,*,#32893,.T.);
#48063=ORIENTED_EDGE('',*,*,#32894,.T.);
#48064=ORIENTED_EDGE('',*,*,#32893,.F.);
#48065=ORIENTED_EDGE('',*,*,#32894,.F.);
#48066=ORIENTED_EDGE('',*,*,#32895,.T.);
#48067=ORIENTED_EDGE('',*,*,#32896,.F.);
#48068=ORIENTED_EDGE('',*,*,#32895,.F.);
#48069=ORIENTED_EDGE('',*,*,#32897,.F.);
#48070=ORIENTED_EDGE('',*,*,#32898,.T.);
#48071=ORIENTED_EDGE('',*,*,#32899,.F.);
#48072=ORIENTED_EDGE('',*,*,#32900,.F.);
#48073=ORIENTED_EDGE('',*,*,#32901,.F.);
#48074=ORIENTED_EDGE('',*,*,#32902,.F.);
#48075=ORIENTED_EDGE('',*,*,#32903,.F.);
#48076=ORIENTED_EDGE('',*,*,#32904,.F.);
#48077=ORIENTED_EDGE('',*,*,#32898,.F.);
#48078=ORIENTED_EDGE('',*,*,#32903,.T.);
#48079=ORIENTED_EDGE('',*,*,#32905,.T.);
#48080=ORIENTED_EDGE('',*,*,#32906,.T.);
#48081=ORIENTED_EDGE('',*,*,#32907,.F.);
#48082=ORIENTED_EDGE('',*,*,#32902,.T.);
#48083=ORIENTED_EDGE('',*,*,#32908,.T.);
#48084=ORIENTED_EDGE('',*,*,#32909,.T.);
#48085=ORIENTED_EDGE('',*,*,#32905,.F.);
#48086=ORIENTED_EDGE('',*,*,#32901,.T.);
#48087=ORIENTED_EDGE('',*,*,#32910,.T.);
#48088=ORIENTED_EDGE('',*,*,#32911,.T.);
#48089=ORIENTED_EDGE('',*,*,#32908,.F.);
#48090=ORIENTED_EDGE('',*,*,#32906,.F.);
#48091=ORIENTED_EDGE('',*,*,#32909,.F.);
#48092=ORIENTED_EDGE('',*,*,#32911,.F.);
#48093=ORIENTED_EDGE('',*,*,#32912,.F.);
#48094=ORIENTED_EDGE('',*,*,#32913,.F.);
#48095=ORIENTED_EDGE('',*,*,#32914,.T.);
#48096=ORIENTED_EDGE('',*,*,#32915,.F.);
#48097=ORIENTED_EDGE('',*,*,#32914,.F.);
#48098=ORIENTED_EDGE('',*,*,#32916,.F.);
#48099=ORIENTED_EDGE('',*,*,#32900,.T.);
#48100=ORIENTED_EDGE('',*,*,#32917,.T.);
#48101=ORIENTED_EDGE('',*,*,#32912,.T.);
#48102=ORIENTED_EDGE('',*,*,#32910,.F.);
#48103=ORIENTED_EDGE('',*,*,#32904,.T.);
#48104=ORIENTED_EDGE('',*,*,#32907,.T.);
#48105=ORIENTED_EDGE('',*,*,#32916,.T.);
#48106=ORIENTED_EDGE('',*,*,#32918,.F.);
#48107=ORIENTED_EDGE('',*,*,#32899,.T.);
#48108=ORIENTED_EDGE('',*,*,#32918,.T.);
#48109=ORIENTED_EDGE('',*,*,#32913,.T.);
#48110=ORIENTED_EDGE('',*,*,#32917,.F.);
#48111=ORIENTED_EDGE('',*,*,#32915,.T.);
#48112=ORIENTED_EDGE('',*,*,#32896,.T.);
#48113=ORIENTED_EDGE('',*,*,#32897,.T.);
#48114=ORIENTED_EDGE('',*,*,#32890,.T.);
#48115=CONICAL_SURFACE('',#51189,38.8,0.785398163397448);
#48116=CONICAL_SURFACE('',#51191,38.8,0.785398163397448);
#48117=CONICAL_SURFACE('',#51193,38.8,0.785398163397448);
#48118=CONICAL_SURFACE('',#51195,38.8,0.785398163397448);
#48119=CONICAL_SURFACE('',#51197,38.8,0.785398163397448);
#48120=CONICAL_SURFACE('',#51199,38.8,0.785398163397448);
#48121=CONICAL_SURFACE('',#51201,38.8,0.785398163397448);
#48122=CONICAL_SURFACE('',#51203,38.8,0.785398163397448);
#48123=CONICAL_SURFACE('',#51205,38.8,0.785398163397448);
#48124=CONICAL_SURFACE('',#51207,38.8,0.785398163397448);
#48125=CONICAL_SURFACE('',#51209,38.8,0.785398163397448);
#48126=CONICAL_SURFACE('',#51211,38.8,0.785398163397448);
#48127=CONICAL_SURFACE('',#51213,38.8,0.785398163397448);
#48128=CONICAL_SURFACE('',#51215,38.8,0.785398163397448);
#48129=CONICAL_SURFACE('',#51217,38.8,0.785398163397448);
#48130=CONICAL_SURFACE('',#51219,38.8,0.785398163397448);
#48131=CONICAL_SURFACE('',#51221,38.8,0.785398163397448);
#48132=CONICAL_SURFACE('',#51223,38.8,0.785398163397448);
#48133=CONICAL_SURFACE('',#51225,38.8,0.785398163397448);
#48134=CONICAL_SURFACE('',#51227,38.8,0.785398163397448);
#48135=CONICAL_SURFACE('',#51229,38.8,0.785398163397448);
#48136=CONICAL_SURFACE('',#51231,38.8,0.785398163397448);
#48137=CONICAL_SURFACE('',#51233,38.8,0.785398163397448);
#48138=CONICAL_SURFACE('',#51235,38.8,0.785398163397448);
#48139=CONICAL_SURFACE('',#51237,38.8,0.785398163397448);
#48140=CONICAL_SURFACE('',#51239,38.8,0.785398163397448);
#48141=CONICAL_SURFACE('',#51241,38.8,0.785398163397448);
#48142=CONICAL_SURFACE('',#51243,38.8,0.785398163397448);
#48143=CONICAL_SURFACE('',#51245,38.8,0.785398163397448);
#48144=CONICAL_SURFACE('',#51247,38.8,0.785398163397448);
#48145=CONICAL_SURFACE('',#51249,38.8,0.785398163397448);
#48146=CONICAL_SURFACE('',#51251,38.8,0.785398163397448);
#48147=CONICAL_SURFACE('',#51253,38.8,0.785398163397448);
#48148=CONICAL_SURFACE('',#51255,38.8,0.785398163397448);
#48149=CONICAL_SURFACE('',#51257,38.8,0.785398163397448);
#48150=CONICAL_SURFACE('',#51259,38.8,0.785398163397448);
#48151=CONICAL_SURFACE('',#51369,38.8,0.785398163397448);
#48152=CONICAL_SURFACE('',#51371,38.8,0.785398163397448);
#48153=CONICAL_SURFACE('',#51373,38.8,0.785398163397448);
#48154=CONICAL_SURFACE('',#51375,38.8,0.785398163397448);
#48155=CONICAL_SURFACE('',#51377,38.8,0.785398163397448);
#48156=CONICAL_SURFACE('',#51379,38.8,0.785398163397448);
#48157=CONICAL_SURFACE('',#51381,38.8,0.785398163397448);
#48158=CONICAL_SURFACE('',#51383,38.8,0.785398163397448);
#48159=CONICAL_SURFACE('',#51385,38.8,0.785398163397448);
#48160=CONICAL_SURFACE('',#51387,38.8,0.785398163397448);
#48161=CONICAL_SURFACE('',#51389,38.8,0.785398163397448);
#48162=CONICAL_SURFACE('',#51391,38.8,0.785398163397448);
#48163=CONICAL_SURFACE('',#51393,38.8,0.785398163397448);
#48164=CONICAL_SURFACE('',#51395,38.8,0.785398163397448);
#48165=CONICAL_SURFACE('',#51397,38.8,0.785398163397448);
#48166=CONICAL_SURFACE('',#51399,38.8,0.785398163397448);
#48167=CONICAL_SURFACE('',#51401,38.8,0.785398163397448);
#48168=CONICAL_SURFACE('',#51403,38.8,0.785398163397448);
#48169=CONICAL_SURFACE('',#51405,38.8,0.785398163397448);
#48170=CONICAL_SURFACE('',#51407,38.8,0.785398163397448);
#48171=CONICAL_SURFACE('',#51409,38.8,0.785398163397448);
#48172=CONICAL_SURFACE('',#51411,38.8,0.785398163397448);
#48173=CONICAL_SURFACE('',#51413,38.8,0.785398163397448);
#48174=CONICAL_SURFACE('',#51415,38.8,0.785398163397448);
#48175=CONICAL_SURFACE('',#51417,38.8,0.785398163397448);
#48176=CONICAL_SURFACE('',#51419,38.8,0.785398163397448);
#48177=CONICAL_SURFACE('',#51421,38.8,0.785398163397448);
#48178=CONICAL_SURFACE('',#51423,38.8,0.785398163397448);
#48179=CONICAL_SURFACE('',#51425,38.8,0.785398163397448);
#48180=CONICAL_SURFACE('',#51427,38.8,0.785398163397448);
#48181=CONICAL_SURFACE('',#51429,38.8,0.785398163397448);
#48182=CONICAL_SURFACE('',#51431,38.8,0.785398163397448);
#48183=CONICAL_SURFACE('',#51433,38.8,0.785398163397448);
#48184=CONICAL_SURFACE('',#51435,38.8,0.785398163397448);
#48185=CONICAL_SURFACE('',#51437,38.8,0.785398163397448);
#48186=CONICAL_SURFACE('',#51439,38.8,0.785398163397448);
#48187=CONICAL_SURFACE('',#51741,42.6,0.785398163397452);
#48188=CONICAL_SURFACE('',#53565,42.6,0.785398163397452);
#48189=CONICAL_SURFACE('',#53568,47.3660700849456,0.953735573090811);
#48190=CONICAL_SURFACE('',#53572,49.25,0.336674819386727);
#48191=CONICAL_SURFACE('',#53600,50.1,0.785398163397443);
#48192=CONICAL_SURFACE('',#53604,50.25,0.785398163397446);
#48193=CONICAL_SURFACE('',#53607,50.7,1.10714871779409);
#48194=CONICAL_SURFACE('',#53615,37.55,0.785398163397448);
#48195=CONICAL_SURFACE('',#53634,37.55,0.785398163397451);
#48196=CONICAL_SURFACE('',#53647,37.55,0.785398163397451);
#48197=CONICAL_SURFACE('',#53662,37.55,0.785398163397448);
#48198=CONICAL_SURFACE('',#53676,37.55,0.785398163397448);
#48199=CONICAL_SURFACE('',#53690,37.55,0.785398163397451);
#48200=CONICAL_SURFACE('',#53707,41.85,0.750929062397939);
#48201=CONICAL_SURFACE('',#53709,41.85,0.750929062397939);
#48202=CONICAL_SURFACE('',#53711,41.85,0.750929062397939);
#48203=CONICAL_SURFACE('',#53713,41.85,0.750929062397939);
#48204=CONICAL_SURFACE('',#53715,41.85,0.750929062397939);
#48205=CONICAL_SURFACE('',#53717,41.85,0.750929062397939);
#48206=CONICAL_SURFACE('',#53719,41.85,0.750929062397939);
#48207=CONICAL_SURFACE('',#53721,41.85,0.750929062397939);
#48208=CONICAL_SURFACE('',#53723,41.85,0.750929062397939);
#48209=CONICAL_SURFACE('',#53725,41.85,0.750929062397939);
#48210=CONICAL_SURFACE('',#53727,41.85,0.750929062397939);
#48211=CONICAL_SURFACE('',#53729,41.85,0.750929062397939);
#48212=CONICAL_SURFACE('',#53731,41.85,0.750929062397939);
#48213=CONICAL_SURFACE('',#53733,41.85,0.750929062397939);
#48214=CONICAL_SURFACE('',#53735,41.85,0.750929062397939);
#48215=CONICAL_SURFACE('',#53737,41.85,0.750929062397939);
#48216=CONICAL_SURFACE('',#53739,41.85,0.750929062397939);
#48217=CONICAL_SURFACE('',#53741,41.85,0.750929062397939);
#48218=CONICAL_SURFACE('',#53743,41.85,0.750929062397939);
#48219=CONICAL_SURFACE('',#53745,41.85,0.750929062397939);
#48220=CONICAL_SURFACE('',#53747,41.85,0.750929062397939);
#48221=CONICAL_SURFACE('',#53749,41.85,0.750929062397939);
#48222=CONICAL_SURFACE('',#53751,41.85,0.750929062397939);
#48223=CONICAL_SURFACE('',#53753,41.85,0.750929062397939);
#48224=CONICAL_SURFACE('',#53755,41.85,0.750929062397939);
#48225=CONICAL_SURFACE('',#53757,41.85,0.750929062397939);
#48226=CONICAL_SURFACE('',#53759,41.85,0.750929062397939);
#48227=CONICAL_SURFACE('',#53761,41.85,0.750929062397939);
#48228=CONICAL_SURFACE('',#53763,41.85,0.750929062397939);
#48229=CONICAL_SURFACE('',#53765,41.85,0.750929062397939);
#48230=CONICAL_SURFACE('',#53767,41.85,0.750929062397939);
#48231=CONICAL_SURFACE('',#53769,41.85,0.750929062397939);
#48232=CONICAL_SURFACE('',#53771,41.85,0.750929062397939);
#48233=CONICAL_SURFACE('',#53839,41.85,0.750929062397939);
#48234=CONICAL_SURFACE('',#53841,41.85,0.750929062397939);
#48235=CONICAL_SURFACE('',#53843,41.85,0.750929062397939);
#48236=CONICAL_SURFACE('',#53845,41.85,0.750929062397939);
#48237=CONICAL_SURFACE('',#53847,41.85,0.750929062397939);
#48238=CONICAL_SURFACE('',#53849,41.85,0.750929062397939);
#48239=CONICAL_SURFACE('',#53851,41.85,0.750929062397939);
#48240=CONICAL_SURFACE('',#53853,41.85,0.750929062397939);
#48241=CONICAL_SURFACE('',#53855,41.85,0.750929062397939);
#48242=CONICAL_SURFACE('',#53857,41.85,0.750929062397939);
#48243=CONICAL_SURFACE('',#53859,41.85,0.750929062397939);
#48244=CONICAL_SURFACE('',#53861,41.85,0.750929062397939);
#48245=CONICAL_SURFACE('',#53863,41.85,0.750929062397939);
#48246=CONICAL_SURFACE('',#53865,41.85,0.750929062397939);
#48247=CONICAL_SURFACE('',#53867,41.85,0.750929062397939);
#48248=CONICAL_SURFACE('',#53869,41.85,0.750929062397939);
#48249=CONICAL_SURFACE('',#53871,41.85,0.750929062397939);
#48250=CONICAL_SURFACE('',#53873,41.85,0.750929062397939);
#48251=CONICAL_SURFACE('',#53875,41.85,0.750929062397939);
#48252=CONICAL_SURFACE('',#53877,41.85,0.750929062397939);
#48253=CONICAL_SURFACE('',#53879,41.85,0.750929062397939);
#48254=CONICAL_SURFACE('',#53881,41.85,0.750929062397939);
#48255=CONICAL_SURFACE('',#53883,41.85,0.750929062397939);
#48256=CONICAL_SURFACE('',#53885,41.85,0.750929062397939);
#48257=CONICAL_SURFACE('',#53887,41.85,0.750929062397939);
#48258=CONICAL_SURFACE('',#53889,41.85,0.750929062397939);
#48259=CONICAL_SURFACE('',#53891,41.85,0.750929062397939);
#48260=CONICAL_SURFACE('',#53893,41.85,0.750929062397939);
#48261=CONICAL_SURFACE('',#53895,41.85,0.750929062397939);
#48262=CONICAL_SURFACE('',#53897,41.85,0.750929062397939);
#48263=CONICAL_SURFACE('',#53899,41.85,0.750929062397939);
#48264=CONICAL_SURFACE('',#53901,41.85,0.750929062397939);
#48265=CONICAL_SURFACE('',#53903,41.85,0.750929062397939);
#48266=CONICAL_SURFACE('',#54135,15.41,0.785398163397449);
#48267=CONICAL_SURFACE('',#54141,15.41,0.785398163397448);
#48268=CONICAL_SURFACE('',#54143,3.15,0.785398163397444);
#48269=CONICAL_SURFACE('',#54156,3.15,0.785398163397444);
#48270=CONICAL_SURFACE('',#54184,2.525,1.02974425867665);
#48271=CONICAL_SURFACE('',#54188,5.35,0.785398163397451);
#48272=CONICAL_SURFACE('',#54198,19.75,0.785398163397448);
#48273=CONICAL_SURFACE('',#54204,47.5,0.785398163397447);
#48274=CONICAL_SURFACE('',#54208,47.5,0.785398163397447);
#48275=CONICAL_SURFACE('',#54213,14.495,0.785398163397447);
#48276=CONICAL_SURFACE('',#54368,4.75,0.785398163397446);
#48277=CONICAL_SURFACE('',#54388,4.75,0.785398163397446);
#48278=CONICAL_SURFACE('',#54398,4.75,0.785398163397446);
#48279=CONICAL_SURFACE('',#54402,4.75,0.785398163397446);
#48280=CONICAL_SURFACE('',#54403,4.75,0.785398163397446);
#48281=CONICAL_SURFACE('',#54407,4.75,0.785398163397446);
#48282=CONICAL_SURFACE('',#54408,4.75,0.785398163397446);
#48283=CONICAL_SURFACE('',#54412,4.75,0.785398163397446);
#48284=CONICAL_SURFACE('',#54413,1.5,1.02974425867665);
#48285=CONICAL_SURFACE('',#54416,1.5,1.02974425867665);
#48286=CONICAL_SURFACE('',#54419,1.525,1.02974425867665);
#48287=CONICAL_SURFACE('',#54421,3.175,0.785398163397448);
#48288=CONICAL_SURFACE('',#54424,1.525,1.02974425867665);
#48289=CONICAL_SURFACE('',#54426,3.175,0.785398163397448);
#48290=CONICAL_SURFACE('',#54429,1.525,1.02974425867665);
#48291=CONICAL_SURFACE('',#54431,3.175,0.785398163397448);
#48292=CONICAL_SURFACE('',#54434,1.525,1.02974425867665);
#48293=CONICAL_SURFACE('',#54436,3.175,0.785398163397448);
#48294=CONICAL_SURFACE('',#54442,9.75,0.785398163397447);
#48295=CONICAL_SURFACE('',#54445,9.75,0.785398163397447);
#48296=CONICAL_SURFACE('',#54448,9.75,0.785398163397447);
#48297=CONICAL_SURFACE('',#54451,9.75,0.785398163397447);
#48298=CONICAL_SURFACE('',#54461,9.5,0.785398163397447);
#48299=CONICAL_SURFACE('',#54463,9.5,0.785398163397447);
#48300=CONICAL_SURFACE('',#54465,9.5,0.785398163397447);
#48301=CONICAL_SURFACE('',#54468,9.5,0.785398163397447);
#48302=CONICAL_SURFACE('',#54478,5.75,0.785398163397448);
#48303=CONICAL_SURFACE('',#54482,27.75,0.785398163397447);
#48304=CONICAL_SURFACE('',#54486,27.5,0.785398163397447);
#48305=CONICAL_SURFACE('',#54490,5.75,0.785398163397448);
#48306=CONICAL_SURFACE('',#54760,2.,1.02790944633836);
#48307=CONICAL_SURFACE('',#54771,4.5,0.785398163397448);
#48308=CONICAL_SURFACE('',#54809,7.5,0.785398163397449);
#48309=CONICAL_SURFACE('',#54813,9.9,0.785398163397446);
#48310=CONICAL_SURFACE('',#54818,9.9,0.785398163397446);
#48311=CONICAL_SURFACE('',#54822,5.35,0.785398163397448);
#48312=CONICAL_SURFACE('',#54826,5.35,0.785398163397449);
#48313=CONICAL_SURFACE('',#54842,8.975,0.785398163397449);
#48314=CONICAL_SURFACE('',#54847,8.975,0.785398163397448);
#48315=CONICAL_SURFACE('',#54851,5.35,0.785398163397449);
#48316=CONICAL_SURFACE('',#54855,5.35,0.785398163397449);
#48317=CONICAL_SURFACE('',#55126,1.25,1.02681050468488);
#48318=CONICAL_SURFACE('',#55137,2.7,0.785398163397448);
#48319=CONICAL_SURFACE('',#55175,4.7,0.785398163397448);
#48320=CONICAL_SURFACE('',#55184,2.7,0.785398163397448);
#48321=CONICAL_SURFACE('',#55189,2.7,0.785398163397448);
#48322=CONICAL_SURFACE('',#55256,7.09027674973257,1.0071944566367);
#48323=CONICAL_SURFACE('',#55265,3.6,0.785398163397448);
#48324=CONICAL_SURFACE('',#55272,7.9,0.785398163397449);
#48325=CONICAL_SURFACE('',#55277,7.9,0.785398163397449);
#48326=CONICAL_SURFACE('',#55281,4.3,0.785398163397449);
#48327=CONICAL_SURFACE('',#55285,4.3,0.785398163397449);
#48328=CONICAL_SURFACE('',#55298,7.325,0.785398163397449);
#48329=CONICAL_SURFACE('',#55303,7.325,0.785398163397448);
#48330=CONICAL_SURFACE('',#55307,4.3,0.785398163397448);
#48331=CONICAL_SURFACE('',#55311,4.3,0.785398163397448);
#48332=CONICAL_SURFACE('',#55315,4.425,0.819867264396957);
#48333=CONICAL_SURFACE('',#55320,4.425,0.819867264396957);
#48334=CONICAL_SURFACE('',#55322,7.09027674973257,1.0071944566367);
#48335=CONICAL_SURFACE('',#55327,7.09027674973257,1.0071944566367);
#48336=ADVANCED_FACE('',(#13249),#48115,.F.);
#48337=ADVANCED_FACE('',(#13250),#48116,.F.);
#48338=ADVANCED_FACE('',(#13251),#48117,.F.);
#48339=ADVANCED_FACE('',(#13252),#48118,.F.);
#48340=ADVANCED_FACE('',(#13253),#48119,.F.);
#48341=ADVANCED_FACE('',(#13254),#48120,.F.);
#48342=ADVANCED_FACE('',(#13255),#48121,.F.);
#48343=ADVANCED_FACE('',(#13256),#48122,.F.);
#48344=ADVANCED_FACE('',(#13257),#48123,.F.);
#48345=ADVANCED_FACE('',(#13258),#48124,.F.);
#48346=ADVANCED_FACE('',(#13259),#48125,.F.);
#48347=ADVANCED_FACE('',(#13260),#48126,.F.);
#48348=ADVANCED_FACE('',(#13261),#48127,.F.);
#48349=ADVANCED_FACE('',(#13262),#48128,.F.);
#48350=ADVANCED_FACE('',(#13263),#48129,.F.);
#48351=ADVANCED_FACE('',(#13264),#48130,.F.);
#48352=ADVANCED_FACE('',(#13265),#48131,.F.);
#48353=ADVANCED_FACE('',(#13266),#48132,.F.);
#48354=ADVANCED_FACE('',(#13267),#48133,.F.);
#48355=ADVANCED_FACE('',(#13268),#48134,.F.);
#48356=ADVANCED_FACE('',(#13269),#48135,.F.);
#48357=ADVANCED_FACE('',(#13270),#48136,.F.);
#48358=ADVANCED_FACE('',(#13271),#48137,.F.);
#48359=ADVANCED_FACE('',(#13272),#48138,.F.);
#48360=ADVANCED_FACE('',(#13273),#48139,.F.);
#48361=ADVANCED_FACE('',(#13274),#48140,.F.);
#48362=ADVANCED_FACE('',(#13275),#48141,.F.);
#48363=ADVANCED_FACE('',(#13276),#48142,.F.);
#48364=ADVANCED_FACE('',(#13277),#48143,.F.);
#48365=ADVANCED_FACE('',(#13278),#48144,.F.);
#48366=ADVANCED_FACE('',(#13279),#48145,.F.);
#48367=ADVANCED_FACE('',(#13280),#48146,.F.);
#48368=ADVANCED_FACE('',(#13281),#48147,.F.);
#48369=ADVANCED_FACE('',(#13282),#48148,.F.);
#48370=ADVANCED_FACE('',(#13283),#48149,.F.);
#48371=ADVANCED_FACE('',(#13284),#48150,.F.);
#48372=ADVANCED_FACE('',(#13285),#11216,.F.);
#48373=ADVANCED_FACE('',(#13286),#11217,.T.);
#48374=ADVANCED_FACE('',(#13287),#11218,.F.);
#48375=ADVANCED_FACE('',(#13288),#11219,.T.);
#48376=ADVANCED_FACE('',(#13289),#11220,.F.);
#48377=ADVANCED_FACE('',(#13290),#11221,.T.);
#48378=ADVANCED_FACE('',(#13291),#11222,.F.);
#48379=ADVANCED_FACE('',(#13292),#11223,.T.);
#48380=ADVANCED_FACE('',(#13293),#11224,.F.);
#48381=ADVANCED_FACE('',(#13294),#11225,.T.);
#48382=ADVANCED_FACE('',(#13295),#11226,.F.);
#48383=ADVANCED_FACE('',(#13296),#11227,.T.);
#48384=ADVANCED_FACE('',(#13297),#11228,.F.);
#48385=ADVANCED_FACE('',(#13298),#11229,.T.);
#48386=ADVANCED_FACE('',(#13299),#11230,.F.);
#48387=ADVANCED_FACE('',(#13300),#11231,.T.);
#48388=ADVANCED_FACE('',(#13301),#11232,.F.);
#48389=ADVANCED_FACE('',(#13302),#11233,.T.);
#48390=ADVANCED_FACE('',(#13303),#11234,.F.);
#48391=ADVANCED_FACE('',(#13304),#11235,.T.);
#48392=ADVANCED_FACE('',(#13305),#11236,.F.);
#48393=ADVANCED_FACE('',(#13306),#11237,.T.);
#48394=ADVANCED_FACE('',(#13307),#11238,.F.);
#48395=ADVANCED_FACE('',(#13308),#11239,.T.);
#48396=ADVANCED_FACE('',(#13309),#11240,.F.);
#48397=ADVANCED_FACE('',(#13310),#11241,.T.);
#48398=ADVANCED_FACE('',(#13311),#11242,.F.);
#48399=ADVANCED_FACE('',(#13312),#11243,.T.);
#48400=ADVANCED_FACE('',(#13313),#11244,.F.);
#48401=ADVANCED_FACE('',(#13314),#11245,.T.);
#48402=ADVANCED_FACE('',(#13315),#11246,.F.);
#48403=ADVANCED_FACE('',(#13316),#11247,.T.);
#48404=ADVANCED_FACE('',(#13317),#11248,.F.);
#48405=ADVANCED_FACE('',(#13318),#11249,.T.);
#48406=ADVANCED_FACE('',(#13319),#11250,.F.);
#48407=ADVANCED_FACE('',(#13320),#11251,.T.);
#48408=ADVANCED_FACE('',(#13321),#11252,.F.);
#48409=ADVANCED_FACE('',(#13322),#11253,.T.);
#48410=ADVANCED_FACE('',(#13323),#11254,.F.);
#48411=ADVANCED_FACE('',(#13324),#11255,.T.);
#48412=ADVANCED_FACE('',(#13325),#11256,.F.);
#48413=ADVANCED_FACE('',(#13326),#11257,.T.);
#48414=ADVANCED_FACE('',(#13327),#11258,.F.);
#48415=ADVANCED_FACE('',(#13328),#11259,.T.);
#48416=ADVANCED_FACE('',(#13329),#11260,.F.);
#48417=ADVANCED_FACE('',(#13330),#11261,.T.);
#48418=ADVANCED_FACE('',(#13331),#11262,.F.);
#48419=ADVANCED_FACE('',(#13332),#11263,.T.);
#48420=ADVANCED_FACE('',(#13333),#11264,.F.);
#48421=ADVANCED_FACE('',(#13334),#11265,.T.);
#48422=ADVANCED_FACE('',(#13335),#11266,.F.);
#48423=ADVANCED_FACE('',(#13336),#11267,.T.);
#48424=ADVANCED_FACE('',(#13337),#11268,.F.);
#48425=ADVANCED_FACE('',(#13338),#11269,.T.);
#48426=ADVANCED_FACE('',(#13339),#11270,.F.);
#48427=ADVANCED_FACE('',(#13340),#11271,.T.);
#48428=ADVANCED_FACE('',(#13341),#11272,.F.);
#48429=ADVANCED_FACE('',(#13342),#11273,.T.);
#48430=ADVANCED_FACE('',(#13343),#11274,.F.);
#48431=ADVANCED_FACE('',(#13344),#11275,.T.);
#48432=ADVANCED_FACE('',(#13345),#11276,.F.);
#48433=ADVANCED_FACE('',(#13346),#11277,.T.);
#48434=ADVANCED_FACE('',(#13347),#11278,.F.);
#48435=ADVANCED_FACE('',(#13348),#11279,.T.);
#48436=ADVANCED_FACE('',(#13349),#11280,.F.);
#48437=ADVANCED_FACE('',(#13350),#11281,.T.);
#48438=ADVANCED_FACE('',(#13351),#11282,.F.);
#48439=ADVANCED_FACE('',(#13352),#11283,.T.);
#48440=ADVANCED_FACE('',(#13353),#11284,.F.);
#48441=ADVANCED_FACE('',(#13354),#11285,.T.);
#48442=ADVANCED_FACE('',(#13355),#11286,.F.);
#48443=ADVANCED_FACE('',(#13356),#11287,.T.);
#48444=ADVANCED_FACE('',(#13357),#48151,.F.);
#48445=ADVANCED_FACE('',(#13358),#48152,.F.);
#48446=ADVANCED_FACE('',(#13359),#48153,.F.);
#48447=ADVANCED_FACE('',(#13360),#48154,.F.);
#48448=ADVANCED_FACE('',(#13361),#48155,.F.);
#48449=ADVANCED_FACE('',(#13362),#48156,.F.);
#48450=ADVANCED_FACE('',(#13363),#48157,.F.);
#48451=ADVANCED_FACE('',(#13364),#48158,.F.);
#48452=ADVANCED_FACE('',(#13365),#48159,.F.);
#48453=ADVANCED_FACE('',(#13366),#48160,.F.);
#48454=ADVANCED_FACE('',(#13367),#48161,.F.);
#48455=ADVANCED_FACE('',(#13368),#48162,.F.);
#48456=ADVANCED_FACE('',(#13369),#48163,.F.);
#48457=ADVANCED_FACE('',(#13370),#48164,.F.);
#48458=ADVANCED_FACE('',(#13371),#48165,.F.);
#48459=ADVANCED_FACE('',(#13372),#48166,.F.);
#48460=ADVANCED_FACE('',(#13373),#48167,.F.);
#48461=ADVANCED_FACE('',(#13374),#48168,.F.);
#48462=ADVANCED_FACE('',(#13375),#48169,.F.);
#48463=ADVANCED_FACE('',(#13376),#48170,.F.);
#48464=ADVANCED_FACE('',(#13377),#48171,.F.);
#48465=ADVANCED_FACE('',(#13378),#48172,.F.);
#48466=ADVANCED_FACE('',(#13379),#48173,.F.);
#48467=ADVANCED_FACE('',(#13380),#48174,.F.);
#48468=ADVANCED_FACE('',(#13381),#48175,.F.);
#48469=ADVANCED_FACE('',(#13382),#48176,.F.);
#48470=ADVANCED_FACE('',(#13383),#48177,.F.);
#48471=ADVANCED_FACE('',(#13384),#48178,.F.);
#48472=ADVANCED_FACE('',(#13385),#48179,.F.);
#48473=ADVANCED_FACE('',(#13386),#48180,.F.);
#48474=ADVANCED_FACE('',(#13387),#48181,.F.);
#48475=ADVANCED_FACE('',(#13388),#48182,.F.);
#48476=ADVANCED_FACE('',(#13389),#48183,.F.);
#48477=ADVANCED_FACE('',(#13390),#48184,.F.);
#48478=ADVANCED_FACE('',(#13391),#48185,.F.);
#48479=ADVANCED_FACE('',(#13392),#48186,.F.);
#48480=ADVANCED_FACE('',(#13393),#11288,.T.);
#48481=ADVANCED_FACE('',(#13394),#11289,.T.);
#48482=ADVANCED_FACE('',(#13395),#11290,.T.);
#48483=ADVANCED_FACE('',(#13396),#11291,.T.);
#48484=ADVANCED_FACE('',(#13397),#11292,.T.);
#48485=ADVANCED_FACE('',(#13398),#11293,.T.);
#48486=ADVANCED_FACE('',(#13399),#11294,.T.);
#48487=ADVANCED_FACE('',(#13400),#11295,.T.);
#48488=ADVANCED_FACE('',(#13401),#11296,.T.);
#48489=ADVANCED_FACE('',(#13402),#11297,.T.);
#48490=ADVANCED_FACE('',(#13403),#11298,.T.);
#48491=ADVANCED_FACE('',(#13404),#11299,.T.);
#48492=ADVANCED_FACE('',(#13405),#11300,.T.);
#48493=ADVANCED_FACE('',(#13406),#11301,.T.);
#48494=ADVANCED_FACE('',(#13407),#11302,.T.);
#48495=ADVANCED_FACE('',(#13408),#11303,.T.);
#48496=ADVANCED_FACE('',(#13409),#11304,.T.);
#48497=ADVANCED_FACE('',(#13410),#11305,.T.);
#48498=ADVANCED_FACE('',(#13411),#11306,.T.);
#48499=ADVANCED_FACE('',(#13412),#11307,.T.);
#48500=ADVANCED_FACE('',(#13413),#11308,.T.);
#48501=ADVANCED_FACE('',(#13414),#11309,.T.);
#48502=ADVANCED_FACE('',(#13415),#11310,.T.);
#48503=ADVANCED_FACE('',(#13416),#11311,.T.);
#48504=ADVANCED_FACE('',(#13417),#11312,.T.);
#48505=ADVANCED_FACE('',(#13418),#11313,.T.);
#48506=ADVANCED_FACE('',(#13419),#11314,.T.);
#48507=ADVANCED_FACE('',(#13420),#11315,.T.);
#48508=ADVANCED_FACE('',(#13421),#11316,.T.);
#48509=ADVANCED_FACE('',(#13422),#11317,.T.);
#48510=ADVANCED_FACE('',(#13423),#11318,.T.);
#48511=ADVANCED_FACE('',(#13424),#11319,.T.);
#48512=ADVANCED_FACE('',(#13425),#11320,.T.);
#48513=ADVANCED_FACE('',(#13426),#11321,.T.);
#48514=ADVANCED_FACE('',(#13427),#11322,.T.);
#48515=ADVANCED_FACE('',(#13428),#11323,.T.);
#48516=ADVANCED_FACE('',(#13429),#11324,.F.);
#48517=ADVANCED_FACE('',(#13430),#11325,.F.);
#48518=ADVANCED_FACE('',(#13431),#11326,.F.);
#48519=ADVANCED_FACE('',(#13432),#11327,.F.);
#48520=ADVANCED_FACE('',(#13433),#11328,.F.);
#48521=ADVANCED_FACE('',(#13434),#11329,.F.);
#48522=ADVANCED_FACE('',(#13435),#11330,.F.);
#48523=ADVANCED_FACE('',(#13436),#11331,.F.);
#48524=ADVANCED_FACE('',(#13437),#11332,.F.);
#48525=ADVANCED_FACE('',(#13438),#11333,.F.);
#48526=ADVANCED_FACE('',(#13439),#11334,.F.);
#48527=ADVANCED_FACE('',(#13440),#11335,.F.);
#48528=ADVANCED_FACE('',(#13441),#11336,.F.);
#48529=ADVANCED_FACE('',(#13442),#11337,.F.);
#48530=ADVANCED_FACE('',(#13443),#11338,.F.);
#48531=ADVANCED_FACE('',(#13444),#11339,.F.);
#48532=ADVANCED_FACE('',(#13445),#11340,.F.);
#48533=ADVANCED_FACE('',(#13446),#11341,.F.);
#48534=ADVANCED_FACE('',(#13447),#11342,.F.);
#48535=ADVANCED_FACE('',(#13448),#11343,.F.);
#48536=ADVANCED_FACE('',(#13449),#11344,.F.);
#48537=ADVANCED_FACE('',(#13450),#11345,.F.);
#48538=ADVANCED_FACE('',(#13451),#11346,.F.);
#48539=ADVANCED_FACE('',(#13452),#11347,.F.);
#48540=ADVANCED_FACE('',(#13453),#11348,.F.);
#48541=ADVANCED_FACE('',(#13454),#11349,.F.);
#48542=ADVANCED_FACE('',(#13455),#11350,.F.);
#48543=ADVANCED_FACE('',(#13456),#11351,.F.);
#48544=ADVANCED_FACE('',(#13457),#11352,.F.);
#48545=ADVANCED_FACE('',(#13458),#11353,.F.);
#48546=ADVANCED_FACE('',(#13459),#11354,.F.);
#48547=ADVANCED_FACE('',(#13460),#11355,.F.);
#48548=ADVANCED_FACE('',(#13461),#11356,.F.);
#48549=ADVANCED_FACE('',(#13462),#11357,.F.);
#48550=ADVANCED_FACE('',(#13463),#11358,.F.);
#48551=ADVANCED_FACE('',(#13464),#11359,.F.);
#48552=ADVANCED_FACE('',(#13465),#11360,.T.);
#48553=ADVANCED_FACE('',(#13466),#11361,.T.);
#48554=ADVANCED_FACE('',(#13467),#11362,.T.);
#48555=ADVANCED_FACE('',(#13468),#11363,.T.);
#48556=ADVANCED_FACE('',(#13469),#11364,.T.);
#48557=ADVANCED_FACE('',(#13470),#11365,.T.);
#48558=ADVANCED_FACE('',(#13471),#11366,.T.);
#48559=ADVANCED_FACE('',(#13472),#11367,.T.);
#48560=ADVANCED_FACE('',(#13473),#11368,.T.);
#48561=ADVANCED_FACE('',(#13474),#11369,.T.);
#48562=ADVANCED_FACE('',(#13475),#11370,.T.);
#48563=ADVANCED_FACE('',(#13476),#11371,.T.);
#48564=ADVANCED_FACE('',(#13477),#11372,.T.);
#48565=ADVANCED_FACE('',(#13478),#11373,.T.);
#48566=ADVANCED_FACE('',(#13479),#11374,.T.);
#48567=ADVANCED_FACE('',(#13480),#11375,.T.);
#48568=ADVANCED_FACE('',(#13481),#11376,.T.);
#48569=ADVANCED_FACE('',(#13482),#11377,.T.);
#48570=ADVANCED_FACE('',(#13483),#11378,.T.);
#48571=ADVANCED_FACE('',(#13484),#11379,.T.);
#48572=ADVANCED_FACE('',(#13485),#11380,.T.);
#48573=ADVANCED_FACE('',(#13486),#11381,.T.);
#48574=ADVANCED_FACE('',(#13487),#11382,.T.);
#48575=ADVANCED_FACE('',(#13488),#11383,.T.);
#48576=ADVANCED_FACE('',(#13489),#11384,.T.);
#48577=ADVANCED_FACE('',(#13490),#11385,.T.);
#48578=ADVANCED_FACE('',(#13491),#11386,.T.);
#48579=ADVANCED_FACE('',(#13492),#11387,.T.);
#48580=ADVANCED_FACE('',(#13493),#11388,.T.);
#48581=ADVANCED_FACE('',(#13494),#11389,.T.);
#48582=ADVANCED_FACE('',(#13495),#11390,.T.);
#48583=ADVANCED_FACE('',(#13496),#11391,.T.);
#48584=ADVANCED_FACE('',(#13497),#11392,.T.);
#48585=ADVANCED_FACE('',(#13498),#11393,.T.);
#48586=ADVANCED_FACE('',(#13499),#11394,.T.);
#48587=ADVANCED_FACE('',(#13500),#11395,.T.);
#48588=ADVANCED_FACE('',(#13501),#11396,.F.);
#48589=ADVANCED_FACE('',(#13502),#11397,.F.);
#48590=ADVANCED_FACE('',(#13503),#11398,.F.);
#48591=ADVANCED_FACE('',(#13504),#11399,.F.);
#48592=ADVANCED_FACE('',(#13505),#11400,.F.);
#48593=ADVANCED_FACE('',(#13506),#11401,.F.);
#48594=ADVANCED_FACE('',(#13507),#11402,.F.);
#48595=ADVANCED_FACE('',(#13508),#11403,.F.);
#48596=ADVANCED_FACE('',(#13509),#11404,.F.);
#48597=ADVANCED_FACE('',(#13510),#11405,.F.);
#48598=ADVANCED_FACE('',(#13511),#11406,.F.);
#48599=ADVANCED_FACE('',(#13512),#11407,.F.);
#48600=ADVANCED_FACE('',(#13513),#11408,.F.);
#48601=ADVANCED_FACE('',(#13514),#11409,.F.);
#48602=ADVANCED_FACE('',(#13515),#11410,.F.);
#48603=ADVANCED_FACE('',(#13516),#11411,.F.);
#48604=ADVANCED_FACE('',(#13517),#11412,.F.);
#48605=ADVANCED_FACE('',(#13518),#11413,.F.);
#48606=ADVANCED_FACE('',(#13519),#11414,.F.);
#48607=ADVANCED_FACE('',(#13520),#11415,.F.);
#48608=ADVANCED_FACE('',(#13521),#11416,.F.);
#48609=ADVANCED_FACE('',(#13522),#11417,.F.);
#48610=ADVANCED_FACE('',(#13523),#11418,.F.);
#48611=ADVANCED_FACE('',(#13524),#11419,.F.);
#48612=ADVANCED_FACE('',(#13525),#11420,.F.);
#48613=ADVANCED_FACE('',(#13526),#11421,.F.);
#48614=ADVANCED_FACE('',(#13527),#11422,.F.);
#48615=ADVANCED_FACE('',(#13528),#11423,.F.);
#48616=ADVANCED_FACE('',(#13529),#11424,.F.);
#48617=ADVANCED_FACE('',(#13530),#11425,.F.);
#48618=ADVANCED_FACE('',(#13531),#11426,.F.);
#48619=ADVANCED_FACE('',(#13532),#11427,.F.);
#48620=ADVANCED_FACE('',(#13533),#11428,.F.);
#48621=ADVANCED_FACE('',(#13534),#11429,.F.);
#48622=ADVANCED_FACE('',(#13535),#11430,.F.);
#48623=ADVANCED_FACE('',(#13536),#11431,.F.);
#48624=ADVANCED_FACE('',(#13537),#11432,.T.);
#48625=ADVANCED_FACE('',(#13538),#11433,.T.);
#48626=ADVANCED_FACE('',(#13539),#11434,.T.);
#48627=ADVANCED_FACE('',(#13540),#11435,.T.);
#48628=ADVANCED_FACE('',(#13541),#11436,.T.);
#48629=ADVANCED_FACE('',(#13542),#11437,.T.);
#48630=ADVANCED_FACE('',(#13543),#11438,.T.);
#48631=ADVANCED_FACE('',(#13544),#11439,.T.);
#48632=ADVANCED_FACE('',(#13545),#11440,.T.);
#48633=ADVANCED_FACE('',(#13546),#11441,.T.);
#48634=ADVANCED_FACE('',(#13547),#11442,.T.);
#48635=ADVANCED_FACE('',(#13548),#11443,.T.);
#48636=ADVANCED_FACE('',(#13549),#11444,.T.);
#48637=ADVANCED_FACE('',(#13550),#11445,.T.);
#48638=ADVANCED_FACE('',(#13551),#11446,.T.);
#48639=ADVANCED_FACE('',(#13552),#11447,.T.);
#48640=ADVANCED_FACE('',(#13553),#11448,.T.);
#48641=ADVANCED_FACE('',(#13554),#11449,.T.);
#48642=ADVANCED_FACE('',(#13555),#11450,.T.);
#48643=ADVANCED_FACE('',(#13556),#11451,.T.);
#48644=ADVANCED_FACE('',(#13557),#11452,.T.);
#48645=ADVANCED_FACE('',(#13558),#11453,.T.);
#48646=ADVANCED_FACE('',(#13559),#11454,.T.);
#48647=ADVANCED_FACE('',(#13560),#11455,.T.);
#48648=ADVANCED_FACE('',(#13561),#11456,.T.);
#48649=ADVANCED_FACE('',(#13562),#11457,.T.);
#48650=ADVANCED_FACE('',(#13563),#11458,.T.);
#48651=ADVANCED_FACE('',(#13564),#11459,.T.);
#48652=ADVANCED_FACE('',(#13565),#11460,.T.);
#48653=ADVANCED_FACE('',(#13566),#11461,.T.);
#48654=ADVANCED_FACE('',(#13567),#11462,.T.);
#48655=ADVANCED_FACE('',(#13568),#11463,.T.);
#48656=ADVANCED_FACE('',(#13569),#11464,.T.);
#48657=ADVANCED_FACE('',(#13570),#11465,.T.);
#48658=ADVANCED_FACE('',(#13571),#11466,.T.);
#48659=ADVANCED_FACE('',(#13572),#11467,.T.);
#48660=ADVANCED_FACE('',(#13573),#11468,.T.);
#48661=ADVANCED_FACE('',(#13574),#11469,.T.);
#48662=ADVANCED_FACE('',(#13575),#11470,.T.);
#48663=ADVANCED_FACE('',(#13576),#11471,.T.);
#48664=ADVANCED_FACE('',(#13577),#11472,.T.);
#48665=ADVANCED_FACE('',(#13578),#11473,.T.);
#48666=ADVANCED_FACE('',(#13579),#11474,.T.);
#48667=ADVANCED_FACE('',(#13580),#11475,.T.);
#48668=ADVANCED_FACE('',(#13581),#11476,.T.);
#48669=ADVANCED_FACE('',(#13582),#11477,.T.);
#48670=ADVANCED_FACE('',(#13583),#11478,.T.);
#48671=ADVANCED_FACE('',(#13584),#11479,.T.);
#48672=ADVANCED_FACE('',(#13585),#11480,.T.);
#48673=ADVANCED_FACE('',(#13586),#11481,.T.);
#48674=ADVANCED_FACE('',(#13587),#11482,.T.);
#48675=ADVANCED_FACE('',(#13588),#11483,.T.);
#48676=ADVANCED_FACE('',(#13589),#11484,.T.);
#48677=ADVANCED_FACE('',(#13590),#11485,.T.);
#48678=ADVANCED_FACE('',(#13591),#11486,.T.);
#48679=ADVANCED_FACE('',(#13592),#11487,.T.);
#48680=ADVANCED_FACE('',(#13593),#11488,.T.);
#48681=ADVANCED_FACE('',(#13594),#11489,.T.);
#48682=ADVANCED_FACE('',(#13595),#11490,.T.);
#48683=ADVANCED_FACE('',(#13596),#11491,.T.);
#48684=ADVANCED_FACE('',(#13597),#11492,.T.);
#48685=ADVANCED_FACE('',(#13598),#11493,.T.);
#48686=ADVANCED_FACE('',(#13599),#11494,.T.);
#48687=ADVANCED_FACE('',(#13600),#11495,.T.);
#48688=ADVANCED_FACE('',(#13601),#48187,.F.);
#48689=ADVANCED_FACE('',(#13602),#1044,.F.);
#48690=ADVANCED_FACE('',(#13603),#11496,.T.);
#48691=ADVANCED_FACE('',(#13604),#11497,.T.);
#48692=ADVANCED_FACE('',(#13605),#11498,.T.);
#48693=ADVANCED_FACE('',(#13606),#11499,.T.);
#48694=ADVANCED_FACE('',(#13607),#11500,.T.);
#48695=ADVANCED_FACE('',(#13608),#11501,.T.);
#48696=ADVANCED_FACE('',(#13609),#11502,.T.);
#48697=ADVANCED_FACE('',(#13610),#11503,.T.);
#48698=ADVANCED_FACE('',(#13611),#11504,.T.);
#48699=ADVANCED_FACE('',(#13612),#11505,.T.);
#48700=ADVANCED_FACE('',(#13613),#11506,.T.);
#48701=ADVANCED_FACE('',(#13614),#11507,.T.);
#48702=ADVANCED_FACE('',(#13615),#11508,.T.);
#48703=ADVANCED_FACE('',(#13616),#11509,.T.);
#48704=ADVANCED_FACE('',(#13617),#11510,.T.);
#48705=ADVANCED_FACE('',(#13618),#11511,.T.);
#48706=ADVANCED_FACE('',(#13619),#11512,.T.);
#48707=ADVANCED_FACE('',(#13620),#11513,.T.);
#48708=ADVANCED_FACE('',(#13621),#11514,.T.);
#48709=ADVANCED_FACE('',(#13622),#11515,.T.);
#48710=ADVANCED_FACE('',(#13623),#11516,.T.);
#48711=ADVANCED_FACE('',(#13624),#11517,.T.);
#48712=ADVANCED_FACE('',(#13625),#11518,.T.);
#48713=ADVANCED_FACE('',(#13626),#11519,.T.);
#48714=ADVANCED_FACE('',(#13627),#11520,.T.);
#48715=ADVANCED_FACE('',(#13628),#11521,.T.);
#48716=ADVANCED_FACE('',(#13629),#11522,.T.);
#48717=ADVANCED_FACE('',(#13630),#11523,.T.);
#48718=ADVANCED_FACE('',(#13631),#1045,.F.);
#48719=ADVANCED_FACE('',(#13632),#11524,.T.);
#48720=ADVANCED_FACE('',(#13633),#11525,.T.);
#48721=ADVANCED_FACE('',(#13634),#11526,.T.);
#48722=ADVANCED_FACE('',(#13635),#11527,.T.);
#48723=ADVANCED_FACE('',(#13636),#11528,.T.);
#48724=ADVANCED_FACE('',(#13637),#11529,.T.);
#48725=ADVANCED_FACE('',(#13638),#11530,.T.);
#48726=ADVANCED_FACE('',(#13639),#11531,.T.);
#48727=ADVANCED_FACE('',(#13640),#11532,.T.);
#48728=ADVANCED_FACE('',(#13641),#11533,.T.);
#48729=ADVANCED_FACE('',(#13642),#11534,.T.);
#48730=ADVANCED_FACE('',(#13643),#11535,.T.);
#48731=ADVANCED_FACE('',(#13644),#11536,.T.);
#48732=ADVANCED_FACE('',(#13645),#11537,.T.);
#48733=ADVANCED_FACE('',(#13646),#11538,.T.);
#48734=ADVANCED_FACE('',(#13647),#11539,.T.);
#48735=ADVANCED_FACE('',(#13648),#11540,.T.);
#48736=ADVANCED_FACE('',(#13649),#11541,.T.);
#48737=ADVANCED_FACE('',(#13650),#11542,.T.);
#48738=ADVANCED_FACE('',(#13651),#11543,.T.);
#48739=ADVANCED_FACE('',(#13652),#11544,.T.);
#48740=ADVANCED_FACE('',(#13653),#11545,.T.);
#48741=ADVANCED_FACE('',(#13654),#11546,.T.);
#48742=ADVANCED_FACE('',(#13655),#11547,.T.);
#48743=ADVANCED_FACE('',(#13656),#11548,.T.);
#48744=ADVANCED_FACE('',(#13657),#11549,.T.);
#48745=ADVANCED_FACE('',(#13658),#11550,.T.);
#48746=ADVANCED_FACE('',(#13659),#11551,.T.);
#48747=ADVANCED_FACE('',(#13660),#1046,.F.);
#48748=ADVANCED_FACE('',(#13661),#11552,.T.);
#48749=ADVANCED_FACE('',(#13662),#11553,.T.);
#48750=ADVANCED_FACE('',(#13663),#11554,.T.);
#48751=ADVANCED_FACE('',(#13664),#11555,.T.);
#48752=ADVANCED_FACE('',(#13665),#11556,.T.);
#48753=ADVANCED_FACE('',(#13666),#11557,.T.);
#48754=ADVANCED_FACE('',(#13667),#11558,.T.);
#48755=ADVANCED_FACE('',(#13668),#11559,.T.);
#48756=ADVANCED_FACE('',(#13669),#11560,.T.);
#48757=ADVANCED_FACE('',(#13670),#11561,.T.);
#48758=ADVANCED_FACE('',(#13671),#11562,.T.);
#48759=ADVANCED_FACE('',(#13672),#11563,.T.);
#48760=ADVANCED_FACE('',(#13673),#11564,.T.);
#48761=ADVANCED_FACE('',(#13674),#11565,.T.);
#48762=ADVANCED_FACE('',(#13675),#11566,.T.);
#48763=ADVANCED_FACE('',(#13676),#11567,.T.);
#48764=ADVANCED_FACE('',(#13677),#11568,.T.);
#48765=ADVANCED_FACE('',(#13678),#11569,.T.);
#48766=ADVANCED_FACE('',(#13679),#11570,.T.);
#48767=ADVANCED_FACE('',(#13680),#11571,.T.);
#48768=ADVANCED_FACE('',(#13681),#11572,.T.);
#48769=ADVANCED_FACE('',(#13682),#11573,.T.);
#48770=ADVANCED_FACE('',(#13683),#11574,.T.);
#48771=ADVANCED_FACE('',(#13684),#11575,.T.);
#48772=ADVANCED_FACE('',(#13685),#11576,.T.);
#48773=ADVANCED_FACE('',(#13686),#11577,.T.);
#48774=ADVANCED_FACE('',(#13687),#11578,.T.);
#48775=ADVANCED_FACE('',(#13688),#11579,.T.);
#48776=ADVANCED_FACE('',(#13689),#1047,.F.);
#48777=ADVANCED_FACE('',(#13690),#11580,.T.);
#48778=ADVANCED_FACE('',(#13691),#11581,.T.);
#48779=ADVANCED_FACE('',(#13692),#11582,.T.);
#48780=ADVANCED_FACE('',(#13693),#11583,.T.);
#48781=ADVANCED_FACE('',(#13694),#11584,.T.);
#48782=ADVANCED_FACE('',(#13695),#11585,.T.);
#48783=ADVANCED_FACE('',(#13696),#11586,.T.);
#48784=ADVANCED_FACE('',(#13697),#11587,.T.);
#48785=ADVANCED_FACE('',(#13698),#11588,.T.);
#48786=ADVANCED_FACE('',(#13699),#11589,.T.);
#48787=ADVANCED_FACE('',(#13700),#11590,.T.);
#48788=ADVANCED_FACE('',(#13701),#11591,.T.);
#48789=ADVANCED_FACE('',(#13702),#11592,.T.);
#48790=ADVANCED_FACE('',(#13703),#11593,.T.);
#48791=ADVANCED_FACE('',(#13704),#11594,.T.);
#48792=ADVANCED_FACE('',(#13705),#11595,.T.);
#48793=ADVANCED_FACE('',(#13706),#11596,.T.);
#48794=ADVANCED_FACE('',(#13707),#11597,.T.);
#48795=ADVANCED_FACE('',(#13708),#11598,.T.);
#48796=ADVANCED_FACE('',(#13709),#11599,.T.);
#48797=ADVANCED_FACE('',(#13710),#11600,.T.);
#48798=ADVANCED_FACE('',(#13711),#11601,.T.);
#48799=ADVANCED_FACE('',(#13712),#11602,.T.);
#48800=ADVANCED_FACE('',(#13713),#11603,.T.);
#48801=ADVANCED_FACE('',(#13714),#11604,.T.);
#48802=ADVANCED_FACE('',(#13715),#11605,.T.);
#48803=ADVANCED_FACE('',(#13716),#11606,.T.);
#48804=ADVANCED_FACE('',(#13717),#11607,.T.);
#48805=ADVANCED_FACE('',(#13718),#1048,.F.);
#48806=ADVANCED_FACE('',(#13719),#11608,.T.);
#48807=ADVANCED_FACE('',(#13720),#11609,.T.);
#48808=ADVANCED_FACE('',(#13721),#11610,.T.);
#48809=ADVANCED_FACE('',(#13722),#11611,.T.);
#48810=ADVANCED_FACE('',(#13723),#11612,.T.);
#48811=ADVANCED_FACE('',(#13724),#11613,.T.);
#48812=ADVANCED_FACE('',(#13725),#11614,.T.);
#48813=ADVANCED_FACE('',(#13726),#11615,.T.);
#48814=ADVANCED_FACE('',(#13727),#11616,.T.);
#48815=ADVANCED_FACE('',(#13728),#11617,.T.);
#48816=ADVANCED_FACE('',(#13729),#11618,.T.);
#48817=ADVANCED_FACE('',(#13730),#11619,.T.);
#48818=ADVANCED_FACE('',(#13731),#11620,.T.);
#48819=ADVANCED_FACE('',(#13732),#11621,.T.);
#48820=ADVANCED_FACE('',(#13733),#11622,.T.);
#48821=ADVANCED_FACE('',(#13734),#11623,.T.);
#48822=ADVANCED_FACE('',(#13735),#11624,.T.);
#48823=ADVANCED_FACE('',(#13736),#11625,.T.);
#48824=ADVANCED_FACE('',(#13737),#11626,.T.);
#48825=ADVANCED_FACE('',(#13738),#11627,.T.);
#48826=ADVANCED_FACE('',(#13739),#11628,.T.);
#48827=ADVANCED_FACE('',(#13740),#11629,.T.);
#48828=ADVANCED_FACE('',(#13741),#11630,.T.);
#48829=ADVANCED_FACE('',(#13742),#11631,.T.);
#48830=ADVANCED_FACE('',(#13743),#11632,.T.);
#48831=ADVANCED_FACE('',(#13744),#11633,.T.);
#48832=ADVANCED_FACE('',(#13745),#11634,.T.);
#48833=ADVANCED_FACE('',(#13746),#11635,.T.);
#48834=ADVANCED_FACE('',(#13747),#1049,.F.);
#48835=ADVANCED_FACE('',(#13748),#11636,.T.);
#48836=ADVANCED_FACE('',(#13749),#11637,.T.);
#48837=ADVANCED_FACE('',(#13750),#11638,.T.);
#48838=ADVANCED_FACE('',(#13751),#11639,.T.);
#48839=ADVANCED_FACE('',(#13752),#11640,.T.);
#48840=ADVANCED_FACE('',(#13753),#11641,.T.);
#48841=ADVANCED_FACE('',(#13754),#11642,.T.);
#48842=ADVANCED_FACE('',(#13755),#11643,.T.);
#48843=ADVANCED_FACE('',(#13756),#11644,.T.);
#48844=ADVANCED_FACE('',(#13757),#11645,.T.);
#48845=ADVANCED_FACE('',(#13758),#11646,.T.);
#48846=ADVANCED_FACE('',(#13759),#11647,.T.);
#48847=ADVANCED_FACE('',(#13760),#11648,.T.);
#48848=ADVANCED_FACE('',(#13761),#11649,.T.);
#48849=ADVANCED_FACE('',(#13762),#11650,.T.);
#48850=ADVANCED_FACE('',(#13763),#11651,.T.);
#48851=ADVANCED_FACE('',(#13764),#11652,.T.);
#48852=ADVANCED_FACE('',(#13765),#11653,.T.);
#48853=ADVANCED_FACE('',(#13766),#11654,.T.);
#48854=ADVANCED_FACE('',(#13767),#11655,.T.);
#48855=ADVANCED_FACE('',(#13768),#11656,.T.);
#48856=ADVANCED_FACE('',(#13769),#11657,.T.);
#48857=ADVANCED_FACE('',(#13770),#11658,.T.);
#48858=ADVANCED_FACE('',(#13771),#11659,.T.);
#48859=ADVANCED_FACE('',(#13772),#11660,.T.);
#48860=ADVANCED_FACE('',(#13773),#11661,.T.);
#48861=ADVANCED_FACE('',(#13774),#11662,.T.);
#48862=ADVANCED_FACE('',(#13775),#11663,.T.);
#48863=ADVANCED_FACE('',(#13776),#1050,.F.);
#48864=ADVANCED_FACE('',(#13777),#11664,.T.);
#48865=ADVANCED_FACE('',(#13778),#11665,.T.);
#48866=ADVANCED_FACE('',(#13779),#11666,.T.);
#48867=ADVANCED_FACE('',(#13780),#11667,.T.);
#48868=ADVANCED_FACE('',(#13781),#11668,.T.);
#48869=ADVANCED_FACE('',(#13782),#11669,.T.);
#48870=ADVANCED_FACE('',(#13783),#11670,.T.);
#48871=ADVANCED_FACE('',(#13784),#11671,.T.);
#48872=ADVANCED_FACE('',(#13785),#11672,.T.);
#48873=ADVANCED_FACE('',(#13786),#11673,.T.);
#48874=ADVANCED_FACE('',(#13787),#11674,.T.);
#48875=ADVANCED_FACE('',(#13788),#11675,.T.);
#48876=ADVANCED_FACE('',(#13789),#11676,.T.);
#48877=ADVANCED_FACE('',(#13790),#11677,.T.);
#48878=ADVANCED_FACE('',(#13791),#11678,.T.);
#48879=ADVANCED_FACE('',(#13792),#11679,.T.);
#48880=ADVANCED_FACE('',(#13793),#11680,.T.);
#48881=ADVANCED_FACE('',(#13794),#11681,.T.);
#48882=ADVANCED_FACE('',(#13795),#11682,.T.);
#48883=ADVANCED_FACE('',(#13796),#11683,.T.);
#48884=ADVANCED_FACE('',(#13797),#11684,.T.);
#48885=ADVANCED_FACE('',(#13798),#11685,.T.);
#48886=ADVANCED_FACE('',(#13799),#11686,.T.);
#48887=ADVANCED_FACE('',(#13800),#11687,.T.);
#48888=ADVANCED_FACE('',(#13801),#11688,.T.);
#48889=ADVANCED_FACE('',(#13802),#11689,.T.);
#48890=ADVANCED_FACE('',(#13803),#11690,.T.);
#48891=ADVANCED_FACE('',(#13804),#11691,.T.);
#48892=ADVANCED_FACE('',(#13805),#1051,.F.);
#48893=ADVANCED_FACE('',(#13806),#11692,.T.);
#48894=ADVANCED_FACE('',(#13807),#11693,.T.);
#48895=ADVANCED_FACE('',(#13808),#11694,.T.);
#48896=ADVANCED_FACE('',(#13809),#11695,.T.);
#48897=ADVANCED_FACE('',(#13810),#11696,.T.);
#48898=ADVANCED_FACE('',(#13811),#11697,.T.);
#48899=ADVANCED_FACE('',(#13812),#11698,.T.);
#48900=ADVANCED_FACE('',(#13813),#11699,.T.);
#48901=ADVANCED_FACE('',(#13814),#11700,.T.);
#48902=ADVANCED_FACE('',(#13815),#11701,.T.);
#48903=ADVANCED_FACE('',(#13816),#11702,.T.);
#48904=ADVANCED_FACE('',(#13817),#11703,.T.);
#48905=ADVANCED_FACE('',(#13818),#11704,.T.);
#48906=ADVANCED_FACE('',(#13819),#11705,.T.);
#48907=ADVANCED_FACE('',(#13820),#11706,.T.);
#48908=ADVANCED_FACE('',(#13821),#11707,.T.);
#48909=ADVANCED_FACE('',(#13822),#11708,.T.);
#48910=ADVANCED_FACE('',(#13823),#11709,.T.);
#48911=ADVANCED_FACE('',(#13824),#11710,.T.);
#48912=ADVANCED_FACE('',(#13825),#11711,.T.);
#48913=ADVANCED_FACE('',(#13826),#11712,.T.);
#48914=ADVANCED_FACE('',(#13827),#11713,.T.);
#48915=ADVANCED_FACE('',(#13828),#11714,.T.);
#48916=ADVANCED_FACE('',(#13829),#11715,.T.);
#48917=ADVANCED_FACE('',(#13830),#11716,.T.);
#48918=ADVANCED_FACE('',(#13831),#11717,.T.);
#48919=ADVANCED_FACE('',(#13832),#11718,.T.);
#48920=ADVANCED_FACE('',(#13833),#11719,.T.);
#48921=ADVANCED_FACE('',(#13834),#1052,.F.);
#48922=ADVANCED_FACE('',(#13835),#11720,.T.);
#48923=ADVANCED_FACE('',(#13836),#11721,.T.);
#48924=ADVANCED_FACE('',(#13837),#11722,.T.);
#48925=ADVANCED_FACE('',(#13838),#11723,.T.);
#48926=ADVANCED_FACE('',(#13839),#11724,.T.);
#48927=ADVANCED_FACE('',(#13840),#11725,.T.);
#48928=ADVANCED_FACE('',(#13841),#11726,.T.);
#48929=ADVANCED_FACE('',(#13842),#11727,.T.);
#48930=ADVANCED_FACE('',(#13843),#11728,.T.);
#48931=ADVANCED_FACE('',(#13844),#11729,.T.);
#48932=ADVANCED_FACE('',(#13845),#11730,.T.);
#48933=ADVANCED_FACE('',(#13846),#11731,.T.);
#48934=ADVANCED_FACE('',(#13847),#11732,.T.);
#48935=ADVANCED_FACE('',(#13848),#11733,.T.);
#48936=ADVANCED_FACE('',(#13849),#11734,.T.);
#48937=ADVANCED_FACE('',(#13850),#11735,.T.);
#48938=ADVANCED_FACE('',(#13851),#11736,.T.);
#48939=ADVANCED_FACE('',(#13852),#11737,.T.);
#48940=ADVANCED_FACE('',(#13853),#11738,.T.);
#48941=ADVANCED_FACE('',(#13854),#11739,.T.);
#48942=ADVANCED_FACE('',(#13855),#11740,.T.);
#48943=ADVANCED_FACE('',(#13856),#11741,.T.);
#48944=ADVANCED_FACE('',(#13857),#11742,.T.);
#48945=ADVANCED_FACE('',(#13858),#11743,.T.);
#48946=ADVANCED_FACE('',(#13859),#11744,.T.);
#48947=ADVANCED_FACE('',(#13860),#11745,.T.);
#48948=ADVANCED_FACE('',(#13861),#11746,.T.);
#48949=ADVANCED_FACE('',(#13862),#11747,.T.);
#48950=ADVANCED_FACE('',(#13863),#1053,.F.);
#48951=ADVANCED_FACE('',(#13864),#11748,.T.);
#48952=ADVANCED_FACE('',(#13865),#11749,.T.);
#48953=ADVANCED_FACE('',(#13866),#11750,.T.);
#48954=ADVANCED_FACE('',(#13867),#11751,.T.);
#48955=ADVANCED_FACE('',(#13868),#11752,.T.);
#48956=ADVANCED_FACE('',(#13869),#11753,.T.);
#48957=ADVANCED_FACE('',(#13870),#11754,.T.);
#48958=ADVANCED_FACE('',(#13871),#11755,.T.);
#48959=ADVANCED_FACE('',(#13872),#11756,.T.);
#48960=ADVANCED_FACE('',(#13873),#11757,.T.);
#48961=ADVANCED_FACE('',(#13874),#11758,.T.);
#48962=ADVANCED_FACE('',(#13875),#11759,.T.);
#48963=ADVANCED_FACE('',(#13876),#11760,.T.);
#48964=ADVANCED_FACE('',(#13877),#11761,.T.);
#48965=ADVANCED_FACE('',(#13878),#11762,.T.);
#48966=ADVANCED_FACE('',(#13879),#11763,.T.);
#48967=ADVANCED_FACE('',(#13880),#11764,.T.);
#48968=ADVANCED_FACE('',(#13881),#11765,.T.);
#48969=ADVANCED_FACE('',(#13882),#11766,.T.);
#48970=ADVANCED_FACE('',(#13883),#11767,.T.);
#48971=ADVANCED_FACE('',(#13884),#11768,.T.);
#48972=ADVANCED_FACE('',(#13885),#11769,.T.);
#48973=ADVANCED_FACE('',(#13886),#11770,.T.);
#48974=ADVANCED_FACE('',(#13887),#11771,.T.);
#48975=ADVANCED_FACE('',(#13888),#11772,.T.);
#48976=ADVANCED_FACE('',(#13889),#11773,.T.);
#48977=ADVANCED_FACE('',(#13890),#11774,.T.);
#48978=ADVANCED_FACE('',(#13891),#11775,.T.);
#48979=ADVANCED_FACE('',(#13892),#1054,.F.);
#48980=ADVANCED_FACE('',(#13893),#11776,.T.);
#48981=ADVANCED_FACE('',(#13894),#11777,.T.);
#48982=ADVANCED_FACE('',(#13895),#11778,.T.);
#48983=ADVANCED_FACE('',(#13896),#11779,.T.);
#48984=ADVANCED_FACE('',(#13897),#11780,.T.);
#48985=ADVANCED_FACE('',(#13898),#11781,.T.);
#48986=ADVANCED_FACE('',(#13899),#11782,.T.);
#48987=ADVANCED_FACE('',(#13900),#11783,.T.);
#48988=ADVANCED_FACE('',(#13901),#11784,.T.);
#48989=ADVANCED_FACE('',(#13902),#11785,.T.);
#48990=ADVANCED_FACE('',(#13903),#11786,.T.);
#48991=ADVANCED_FACE('',(#13904),#11787,.T.);
#48992=ADVANCED_FACE('',(#13905),#11788,.T.);
#48993=ADVANCED_FACE('',(#13906),#11789,.T.);
#48994=ADVANCED_FACE('',(#13907),#11790,.T.);
#48995=ADVANCED_FACE('',(#13908),#11791,.T.);
#48996=ADVANCED_FACE('',(#13909),#11792,.T.);
#48997=ADVANCED_FACE('',(#13910),#11793,.T.);
#48998=ADVANCED_FACE('',(#13911),#11794,.T.);
#48999=ADVANCED_FACE('',(#13912),#11795,.T.);
#49000=ADVANCED_FACE('',(#13913),#11796,.T.);
#49001=ADVANCED_FACE('',(#13914),#11797,.T.);
#49002=ADVANCED_FACE('',(#13915),#11798,.T.);
#49003=ADVANCED_FACE('',(#13916),#11799,.T.);
#49004=ADVANCED_FACE('',(#13917),#11800,.T.);
#49005=ADVANCED_FACE('',(#13918),#11801,.T.);
#49006=ADVANCED_FACE('',(#13919),#11802,.T.);
#49007=ADVANCED_FACE('',(#13920),#11803,.T.);
#49008=ADVANCED_FACE('',(#13921),#1055,.F.);
#49009=ADVANCED_FACE('',(#13922),#11804,.T.);
#49010=ADVANCED_FACE('',(#13923),#11805,.T.);
#49011=ADVANCED_FACE('',(#13924),#11806,.T.);
#49012=ADVANCED_FACE('',(#13925),#11807,.T.);
#49013=ADVANCED_FACE('',(#13926),#11808,.T.);
#49014=ADVANCED_FACE('',(#13927),#11809,.T.);
#49015=ADVANCED_FACE('',(#13928),#11810,.T.);
#49016=ADVANCED_FACE('',(#13929),#11811,.T.);
#49017=ADVANCED_FACE('',(#13930),#11812,.T.);
#49018=ADVANCED_FACE('',(#13931),#11813,.T.);
#49019=ADVANCED_FACE('',(#13932),#11814,.T.);
#49020=ADVANCED_FACE('',(#13933),#11815,.T.);
#49021=ADVANCED_FACE('',(#13934),#11816,.T.);
#49022=ADVANCED_FACE('',(#13935),#11817,.T.);
#49023=ADVANCED_FACE('',(#13936),#11818,.T.);
#49024=ADVANCED_FACE('',(#13937),#11819,.T.);
#49025=ADVANCED_FACE('',(#13938),#11820,.T.);
#49026=ADVANCED_FACE('',(#13939),#11821,.T.);
#49027=ADVANCED_FACE('',(#13940),#11822,.T.);
#49028=ADVANCED_FACE('',(#13941),#11823,.T.);
#49029=ADVANCED_FACE('',(#13942),#11824,.T.);
#49030=ADVANCED_FACE('',(#13943),#11825,.T.);
#49031=ADVANCED_FACE('',(#13944),#11826,.T.);
#49032=ADVANCED_FACE('',(#13945),#11827,.T.);
#49033=ADVANCED_FACE('',(#13946),#11828,.T.);
#49034=ADVANCED_FACE('',(#13947),#11829,.T.);
#49035=ADVANCED_FACE('',(#13948),#11830,.T.);
#49036=ADVANCED_FACE('',(#13949),#11831,.T.);
#49037=ADVANCED_FACE('',(#13950),#1056,.F.);
#49038=ADVANCED_FACE('',(#13951),#11832,.T.);
#49039=ADVANCED_FACE('',(#13952),#11833,.T.);
#49040=ADVANCED_FACE('',(#13953),#11834,.T.);
#49041=ADVANCED_FACE('',(#13954),#11835,.T.);
#49042=ADVANCED_FACE('',(#13955),#11836,.T.);
#49043=ADVANCED_FACE('',(#13956),#11837,.T.);
#49044=ADVANCED_FACE('',(#13957),#11838,.T.);
#49045=ADVANCED_FACE('',(#13958),#11839,.T.);
#49046=ADVANCED_FACE('',(#13959),#11840,.T.);
#49047=ADVANCED_FACE('',(#13960),#11841,.T.);
#49048=ADVANCED_FACE('',(#13961),#11842,.T.);
#49049=ADVANCED_FACE('',(#13962),#11843,.T.);
#49050=ADVANCED_FACE('',(#13963),#11844,.T.);
#49051=ADVANCED_FACE('',(#13964),#11845,.T.);
#49052=ADVANCED_FACE('',(#13965),#11846,.T.);
#49053=ADVANCED_FACE('',(#13966),#11847,.T.);
#49054=ADVANCED_FACE('',(#13967),#11848,.T.);
#49055=ADVANCED_FACE('',(#13968),#11849,.T.);
#49056=ADVANCED_FACE('',(#13969),#11850,.T.);
#49057=ADVANCED_FACE('',(#13970),#11851,.T.);
#49058=ADVANCED_FACE('',(#13971),#11852,.T.);
#49059=ADVANCED_FACE('',(#13972),#11853,.T.);
#49060=ADVANCED_FACE('',(#13973),#11854,.T.);
#49061=ADVANCED_FACE('',(#13974),#11855,.T.);
#49062=ADVANCED_FACE('',(#13975),#11856,.T.);
#49063=ADVANCED_FACE('',(#13976),#11857,.T.);
#49064=ADVANCED_FACE('',(#13977),#11858,.T.);
#49065=ADVANCED_FACE('',(#13978),#11859,.T.);
#49066=ADVANCED_FACE('',(#13979),#1057,.F.);
#49067=ADVANCED_FACE('',(#13980),#11860,.T.);
#49068=ADVANCED_FACE('',(#13981),#11861,.T.);
#49069=ADVANCED_FACE('',(#13982),#11862,.T.);
#49070=ADVANCED_FACE('',(#13983),#11863,.T.);
#49071=ADVANCED_FACE('',(#13984),#11864,.T.);
#49072=ADVANCED_FACE('',(#13985),#11865,.T.);
#49073=ADVANCED_FACE('',(#13986),#11866,.T.);
#49074=ADVANCED_FACE('',(#13987),#11867,.T.);
#49075=ADVANCED_FACE('',(#13988),#11868,.T.);
#49076=ADVANCED_FACE('',(#13989),#11869,.T.);
#49077=ADVANCED_FACE('',(#13990),#11870,.T.);
#49078=ADVANCED_FACE('',(#13991),#11871,.T.);
#49079=ADVANCED_FACE('',(#13992),#11872,.T.);
#49080=ADVANCED_FACE('',(#13993),#11873,.T.);
#49081=ADVANCED_FACE('',(#13994),#11874,.T.);
#49082=ADVANCED_FACE('',(#13995),#11875,.T.);
#49083=ADVANCED_FACE('',(#13996),#11876,.T.);
#49084=ADVANCED_FACE('',(#13997),#11877,.T.);
#49085=ADVANCED_FACE('',(#13998),#11878,.T.);
#49086=ADVANCED_FACE('',(#13999),#11879,.T.);
#49087=ADVANCED_FACE('',(#14000),#11880,.T.);
#49088=ADVANCED_FACE('',(#14001),#11881,.T.);
#49089=ADVANCED_FACE('',(#14002),#11882,.T.);
#49090=ADVANCED_FACE('',(#14003),#11883,.T.);
#49091=ADVANCED_FACE('',(#14004),#11884,.T.);
#49092=ADVANCED_FACE('',(#14005),#11885,.T.);
#49093=ADVANCED_FACE('',(#14006),#11886,.T.);
#49094=ADVANCED_FACE('',(#14007),#11887,.T.);
#49095=ADVANCED_FACE('',(#14008),#1058,.F.);
#49096=ADVANCED_FACE('',(#14009),#11888,.T.);
#49097=ADVANCED_FACE('',(#14010),#11889,.T.);
#49098=ADVANCED_FACE('',(#14011),#11890,.T.);
#49099=ADVANCED_FACE('',(#14012),#11891,.T.);
#49100=ADVANCED_FACE('',(#14013),#11892,.T.);
#49101=ADVANCED_FACE('',(#14014),#11893,.T.);
#49102=ADVANCED_FACE('',(#14015),#11894,.T.);
#49103=ADVANCED_FACE('',(#14016),#11895,.T.);
#49104=ADVANCED_FACE('',(#14017),#11896,.T.);
#49105=ADVANCED_FACE('',(#14018),#11897,.T.);
#49106=ADVANCED_FACE('',(#14019),#11898,.T.);
#49107=ADVANCED_FACE('',(#14020),#11899,.T.);
#49108=ADVANCED_FACE('',(#14021),#11900,.T.);
#49109=ADVANCED_FACE('',(#14022),#11901,.T.);
#49110=ADVANCED_FACE('',(#14023),#11902,.T.);
#49111=ADVANCED_FACE('',(#14024),#11903,.T.);
#49112=ADVANCED_FACE('',(#14025),#11904,.T.);
#49113=ADVANCED_FACE('',(#14026),#11905,.T.);
#49114=ADVANCED_FACE('',(#14027),#11906,.T.);
#49115=ADVANCED_FACE('',(#14028),#11907,.T.);
#49116=ADVANCED_FACE('',(#14029),#11908,.T.);
#49117=ADVANCED_FACE('',(#14030),#11909,.T.);
#49118=ADVANCED_FACE('',(#14031),#11910,.T.);
#49119=ADVANCED_FACE('',(#14032),#11911,.T.);
#49120=ADVANCED_FACE('',(#14033),#11912,.T.);
#49121=ADVANCED_FACE('',(#14034),#11913,.T.);
#49122=ADVANCED_FACE('',(#14035),#11914,.T.);
#49123=ADVANCED_FACE('',(#14036),#11915,.T.);
#49124=ADVANCED_FACE('',(#14037),#1059,.F.);
#49125=ADVANCED_FACE('',(#14038),#11916,.T.);
#49126=ADVANCED_FACE('',(#14039),#11917,.T.);
#49127=ADVANCED_FACE('',(#14040),#11918,.T.);
#49128=ADVANCED_FACE('',(#14041),#11919,.T.);
#49129=ADVANCED_FACE('',(#14042),#11920,.T.);
#49130=ADVANCED_FACE('',(#14043),#11921,.T.);
#49131=ADVANCED_FACE('',(#14044),#11922,.T.);
#49132=ADVANCED_FACE('',(#14045),#11923,.T.);
#49133=ADVANCED_FACE('',(#14046),#11924,.T.);
#49134=ADVANCED_FACE('',(#14047),#11925,.T.);
#49135=ADVANCED_FACE('',(#14048),#11926,.T.);
#49136=ADVANCED_FACE('',(#14049),#11927,.T.);
#49137=ADVANCED_FACE('',(#14050),#11928,.T.);
#49138=ADVANCED_FACE('',(#14051),#11929,.T.);
#49139=ADVANCED_FACE('',(#14052),#11930,.T.);
#49140=ADVANCED_FACE('',(#14053),#11931,.T.);
#49141=ADVANCED_FACE('',(#14054),#11932,.T.);
#49142=ADVANCED_FACE('',(#14055),#11933,.T.);
#49143=ADVANCED_FACE('',(#14056),#11934,.T.);
#49144=ADVANCED_FACE('',(#14057),#11935,.T.);
#49145=ADVANCED_FACE('',(#14058),#11936,.T.);
#49146=ADVANCED_FACE('',(#14059),#11937,.T.);
#49147=ADVANCED_FACE('',(#14060),#11938,.T.);
#49148=ADVANCED_FACE('',(#14061),#11939,.T.);
#49149=ADVANCED_FACE('',(#14062),#11940,.T.);
#49150=ADVANCED_FACE('',(#14063),#11941,.T.);
#49151=ADVANCED_FACE('',(#14064),#11942,.T.);
#49152=ADVANCED_FACE('',(#14065),#11943,.T.);
#49153=ADVANCED_FACE('',(#14066),#1060,.F.);
#49154=ADVANCED_FACE('',(#14067),#11944,.T.);
#49155=ADVANCED_FACE('',(#14068),#11945,.T.);
#49156=ADVANCED_FACE('',(#14069),#11946,.T.);
#49157=ADVANCED_FACE('',(#14070),#11947,.T.);
#49158=ADVANCED_FACE('',(#14071),#11948,.T.);
#49159=ADVANCED_FACE('',(#14072),#11949,.T.);
#49160=ADVANCED_FACE('',(#14073),#11950,.T.);
#49161=ADVANCED_FACE('',(#14074),#11951,.T.);
#49162=ADVANCED_FACE('',(#14075),#11952,.T.);
#49163=ADVANCED_FACE('',(#14076),#11953,.T.);
#49164=ADVANCED_FACE('',(#14077),#11954,.T.);
#49165=ADVANCED_FACE('',(#14078),#11955,.T.);
#49166=ADVANCED_FACE('',(#14079),#11956,.T.);
#49167=ADVANCED_FACE('',(#14080),#11957,.T.);
#49168=ADVANCED_FACE('',(#14081),#11958,.T.);
#49169=ADVANCED_FACE('',(#14082),#11959,.T.);
#49170=ADVANCED_FACE('',(#14083),#11960,.T.);
#49171=ADVANCED_FACE('',(#14084),#11961,.T.);
#49172=ADVANCED_FACE('',(#14085),#11962,.T.);
#49173=ADVANCED_FACE('',(#14086),#11963,.T.);
#49174=ADVANCED_FACE('',(#14087),#11964,.T.);
#49175=ADVANCED_FACE('',(#14088),#11965,.T.);
#49176=ADVANCED_FACE('',(#14089),#11966,.T.);
#49177=ADVANCED_FACE('',(#14090),#11967,.T.);
#49178=ADVANCED_FACE('',(#14091),#11968,.T.);
#49179=ADVANCED_FACE('',(#14092),#11969,.T.);
#49180=ADVANCED_FACE('',(#14093),#11970,.T.);
#49181=ADVANCED_FACE('',(#14094),#11971,.T.);
#49182=ADVANCED_FACE('',(#14095),#1061,.F.);
#49183=ADVANCED_FACE('',(#14096),#11972,.T.);
#49184=ADVANCED_FACE('',(#14097),#11973,.T.);
#49185=ADVANCED_FACE('',(#14098),#11974,.T.);
#49186=ADVANCED_FACE('',(#14099),#11975,.T.);
#49187=ADVANCED_FACE('',(#14100),#11976,.T.);
#49188=ADVANCED_FACE('',(#14101),#11977,.T.);
#49189=ADVANCED_FACE('',(#14102),#11978,.T.);
#49190=ADVANCED_FACE('',(#14103),#11979,.T.);
#49191=ADVANCED_FACE('',(#14104),#11980,.T.);
#49192=ADVANCED_FACE('',(#14105),#11981,.T.);
#49193=ADVANCED_FACE('',(#14106),#11982,.T.);
#49194=ADVANCED_FACE('',(#14107),#11983,.T.);
#49195=ADVANCED_FACE('',(#14108),#11984,.T.);
#49196=ADVANCED_FACE('',(#14109),#11985,.T.);
#49197=ADVANCED_FACE('',(#14110),#11986,.T.);
#49198=ADVANCED_FACE('',(#14111),#11987,.T.);
#49199=ADVANCED_FACE('',(#14112),#11988,.T.);
#49200=ADVANCED_FACE('',(#14113),#11989,.T.);
#49201=ADVANCED_FACE('',(#14114),#11990,.T.);
#49202=ADVANCED_FACE('',(#14115),#11991,.T.);
#49203=ADVANCED_FACE('',(#14116),#11992,.T.);
#49204=ADVANCED_FACE('',(#14117),#11993,.T.);
#49205=ADVANCED_FACE('',(#14118),#11994,.T.);
#49206=ADVANCED_FACE('',(#14119),#11995,.T.);
#49207=ADVANCED_FACE('',(#14120),#11996,.T.);
#49208=ADVANCED_FACE('',(#14121),#11997,.T.);
#49209=ADVANCED_FACE('',(#14122),#11998,.T.);
#49210=ADVANCED_FACE('',(#14123),#11999,.T.);
#49211=ADVANCED_FACE('',(#14124),#1062,.F.);
#49212=ADVANCED_FACE('',(#14125),#12000,.T.);
#49213=ADVANCED_FACE('',(#14126),#12001,.T.);
#49214=ADVANCED_FACE('',(#14127),#12002,.T.);
#49215=ADVANCED_FACE('',(#14128),#12003,.T.);
#49216=ADVANCED_FACE('',(#14129),#12004,.T.);
#49217=ADVANCED_FACE('',(#14130),#12005,.T.);
#49218=ADVANCED_FACE('',(#14131),#12006,.T.);
#49219=ADVANCED_FACE('',(#14132),#12007,.T.);
#49220=ADVANCED_FACE('',(#14133),#12008,.T.);
#49221=ADVANCED_FACE('',(#14134),#12009,.T.);
#49222=ADVANCED_FACE('',(#14135),#12010,.T.);
#49223=ADVANCED_FACE('',(#14136),#12011,.T.);
#49224=ADVANCED_FACE('',(#14137),#12012,.T.);
#49225=ADVANCED_FACE('',(#14138),#12013,.T.);
#49226=ADVANCED_FACE('',(#14139),#12014,.T.);
#49227=ADVANCED_FACE('',(#14140),#12015,.T.);
#49228=ADVANCED_FACE('',(#14141),#12016,.T.);
#49229=ADVANCED_FACE('',(#14142),#12017,.T.);
#49230=ADVANCED_FACE('',(#14143),#12018,.T.);
#49231=ADVANCED_FACE('',(#14144),#12019,.T.);
#49232=ADVANCED_FACE('',(#14145),#12020,.T.);
#49233=ADVANCED_FACE('',(#14146),#12021,.T.);
#49234=ADVANCED_FACE('',(#14147),#12022,.T.);
#49235=ADVANCED_FACE('',(#14148),#12023,.T.);
#49236=ADVANCED_FACE('',(#14149),#12024,.T.);
#49237=ADVANCED_FACE('',(#14150),#12025,.T.);
#49238=ADVANCED_FACE('',(#14151),#12026,.T.);
#49239=ADVANCED_FACE('',(#14152),#12027,.T.);
#49240=ADVANCED_FACE('',(#14153),#1063,.F.);
#49241=ADVANCED_FACE('',(#14154),#12028,.T.);
#49242=ADVANCED_FACE('',(#14155),#12029,.T.);
#49243=ADVANCED_FACE('',(#14156),#12030,.T.);
#49244=ADVANCED_FACE('',(#14157),#12031,.T.);
#49245=ADVANCED_FACE('',(#14158),#12032,.T.);
#49246=ADVANCED_FACE('',(#14159),#12033,.T.);
#49247=ADVANCED_FACE('',(#14160),#12034,.T.);
#49248=ADVANCED_FACE('',(#14161),#12035,.T.);
#49249=ADVANCED_FACE('',(#14162),#12036,.T.);
#49250=ADVANCED_FACE('',(#14163),#12037,.T.);
#49251=ADVANCED_FACE('',(#14164),#12038,.T.);
#49252=ADVANCED_FACE('',(#14165),#12039,.T.);
#49253=ADVANCED_FACE('',(#14166),#12040,.T.);
#49254=ADVANCED_FACE('',(#14167),#12041,.T.);
#49255=ADVANCED_FACE('',(#14168),#12042,.T.);
#49256=ADVANCED_FACE('',(#14169),#12043,.T.);
#49257=ADVANCED_FACE('',(#14170),#12044,.T.);
#49258=ADVANCED_FACE('',(#14171),#12045,.T.);
#49259=ADVANCED_FACE('',(#14172),#12046,.T.);
#49260=ADVANCED_FACE('',(#14173),#12047,.T.);
#49261=ADVANCED_FACE('',(#14174),#12048,.T.);
#49262=ADVANCED_FACE('',(#14175),#12049,.T.);
#49263=ADVANCED_FACE('',(#14176),#12050,.T.);
#49264=ADVANCED_FACE('',(#14177),#12051,.T.);
#49265=ADVANCED_FACE('',(#14178),#12052,.T.);
#49266=ADVANCED_FACE('',(#14179),#12053,.T.);
#49267=ADVANCED_FACE('',(#14180),#12054,.T.);
#49268=ADVANCED_FACE('',(#14181),#12055,.T.);
#49269=ADVANCED_FACE('',(#14182),#1064,.F.);
#49270=ADVANCED_FACE('',(#14183),#12056,.T.);
#49271=ADVANCED_FACE('',(#14184),#12057,.T.);
#49272=ADVANCED_FACE('',(#14185),#12058,.T.);
#49273=ADVANCED_FACE('',(#14186),#12059,.T.);
#49274=ADVANCED_FACE('',(#14187),#12060,.T.);
#49275=ADVANCED_FACE('',(#14188),#12061,.T.);
#49276=ADVANCED_FACE('',(#14189),#12062,.T.);
#49277=ADVANCED_FACE('',(#14190),#12063,.T.);
#49278=ADVANCED_FACE('',(#14191),#12064,.T.);
#49279=ADVANCED_FACE('',(#14192),#12065,.T.);
#49280=ADVANCED_FACE('',(#14193),#12066,.T.);
#49281=ADVANCED_FACE('',(#14194),#12067,.T.);
#49282=ADVANCED_FACE('',(#14195),#12068,.T.);
#49283=ADVANCED_FACE('',(#14196),#12069,.T.);
#49284=ADVANCED_FACE('',(#14197),#12070,.T.);
#49285=ADVANCED_FACE('',(#14198),#12071,.T.);
#49286=ADVANCED_FACE('',(#14199),#12072,.T.);
#49287=ADVANCED_FACE('',(#14200),#12073,.T.);
#49288=ADVANCED_FACE('',(#14201),#12074,.T.);
#49289=ADVANCED_FACE('',(#14202),#12075,.T.);
#49290=ADVANCED_FACE('',(#14203),#12076,.T.);
#49291=ADVANCED_FACE('',(#14204),#12077,.T.);
#49292=ADVANCED_FACE('',(#14205),#12078,.T.);
#49293=ADVANCED_FACE('',(#14206),#12079,.T.);
#49294=ADVANCED_FACE('',(#14207),#12080,.T.);
#49295=ADVANCED_FACE('',(#14208),#12081,.T.);
#49296=ADVANCED_FACE('',(#14209),#12082,.T.);
#49297=ADVANCED_FACE('',(#14210),#12083,.T.);
#49298=ADVANCED_FACE('',(#14211),#1065,.F.);
#49299=ADVANCED_FACE('',(#14212),#12084,.T.);
#49300=ADVANCED_FACE('',(#14213),#12085,.T.);
#49301=ADVANCED_FACE('',(#14214),#12086,.T.);
#49302=ADVANCED_FACE('',(#14215),#12087,.T.);
#49303=ADVANCED_FACE('',(#14216),#12088,.T.);
#49304=ADVANCED_FACE('',(#14217),#12089,.T.);
#49305=ADVANCED_FACE('',(#14218),#12090,.T.);
#49306=ADVANCED_FACE('',(#14219),#12091,.T.);
#49307=ADVANCED_FACE('',(#14220),#12092,.T.);
#49308=ADVANCED_FACE('',(#14221),#12093,.T.);
#49309=ADVANCED_FACE('',(#14222),#12094,.T.);
#49310=ADVANCED_FACE('',(#14223),#12095,.T.);
#49311=ADVANCED_FACE('',(#14224),#12096,.T.);
#49312=ADVANCED_FACE('',(#14225),#12097,.T.);
#49313=ADVANCED_FACE('',(#14226),#12098,.T.);
#49314=ADVANCED_FACE('',(#14227),#12099,.T.);
#49315=ADVANCED_FACE('',(#14228),#12100,.T.);
#49316=ADVANCED_FACE('',(#14229),#12101,.T.);
#49317=ADVANCED_FACE('',(#14230),#12102,.T.);
#49318=ADVANCED_FACE('',(#14231),#12103,.T.);
#49319=ADVANCED_FACE('',(#14232),#12104,.T.);
#49320=ADVANCED_FACE('',(#14233),#12105,.T.);
#49321=ADVANCED_FACE('',(#14234),#12106,.T.);
#49322=ADVANCED_FACE('',(#14235),#12107,.T.);
#49323=ADVANCED_FACE('',(#14236),#12108,.T.);
#49324=ADVANCED_FACE('',(#14237),#12109,.T.);
#49325=ADVANCED_FACE('',(#14238),#12110,.T.);
#49326=ADVANCED_FACE('',(#14239),#12111,.T.);
#49327=ADVANCED_FACE('',(#14240),#1066,.F.);
#49328=ADVANCED_FACE('',(#14241),#12112,.T.);
#49329=ADVANCED_FACE('',(#14242),#12113,.T.);
#49330=ADVANCED_FACE('',(#14243),#12114,.T.);
#49331=ADVANCED_FACE('',(#14244),#12115,.T.);
#49332=ADVANCED_FACE('',(#14245),#12116,.T.);
#49333=ADVANCED_FACE('',(#14246),#12117,.T.);
#49334=ADVANCED_FACE('',(#14247),#12118,.T.);
#49335=ADVANCED_FACE('',(#14248),#12119,.T.);
#49336=ADVANCED_FACE('',(#14249),#12120,.T.);
#49337=ADVANCED_FACE('',(#14250),#12121,.T.);
#49338=ADVANCED_FACE('',(#14251),#12122,.T.);
#49339=ADVANCED_FACE('',(#14252),#12123,.T.);
#49340=ADVANCED_FACE('',(#14253),#12124,.T.);
#49341=ADVANCED_FACE('',(#14254),#12125,.T.);
#49342=ADVANCED_FACE('',(#14255),#12126,.T.);
#49343=ADVANCED_FACE('',(#14256),#12127,.T.);
#49344=ADVANCED_FACE('',(#14257),#12128,.T.);
#49345=ADVANCED_FACE('',(#14258),#12129,.T.);
#49346=ADVANCED_FACE('',(#14259),#12130,.T.);
#49347=ADVANCED_FACE('',(#14260),#12131,.T.);
#49348=ADVANCED_FACE('',(#14261),#12132,.T.);
#49349=ADVANCED_FACE('',(#14262),#12133,.T.);
#49350=ADVANCED_FACE('',(#14263),#12134,.T.);
#49351=ADVANCED_FACE('',(#14264),#12135,.T.);
#49352=ADVANCED_FACE('',(#14265),#12136,.T.);
#49353=ADVANCED_FACE('',(#14266),#12137,.T.);
#49354=ADVANCED_FACE('',(#14267),#12138,.T.);
#49355=ADVANCED_FACE('',(#14268),#12139,.T.);
#49356=ADVANCED_FACE('',(#14269),#1067,.F.);
#49357=ADVANCED_FACE('',(#14270),#12140,.T.);
#49358=ADVANCED_FACE('',(#14271),#12141,.T.);
#49359=ADVANCED_FACE('',(#14272),#12142,.T.);
#49360=ADVANCED_FACE('',(#14273),#12143,.T.);
#49361=ADVANCED_FACE('',(#14274),#12144,.T.);
#49362=ADVANCED_FACE('',(#14275),#12145,.T.);
#49363=ADVANCED_FACE('',(#14276),#12146,.T.);
#49364=ADVANCED_FACE('',(#14277),#12147,.T.);
#49365=ADVANCED_FACE('',(#14278),#12148,.T.);
#49366=ADVANCED_FACE('',(#14279),#12149,.T.);
#49367=ADVANCED_FACE('',(#14280),#12150,.T.);
#49368=ADVANCED_FACE('',(#14281),#12151,.T.);
#49369=ADVANCED_FACE('',(#14282),#12152,.T.);
#49370=ADVANCED_FACE('',(#14283),#12153,.T.);
#49371=ADVANCED_FACE('',(#14284),#12154,.T.);
#49372=ADVANCED_FACE('',(#14285),#12155,.T.);
#49373=ADVANCED_FACE('',(#14286),#12156,.T.);
#49374=ADVANCED_FACE('',(#14287),#12157,.T.);
#49375=ADVANCED_FACE('',(#14288),#12158,.T.);
#49376=ADVANCED_FACE('',(#14289),#12159,.T.);
#49377=ADVANCED_FACE('',(#14290),#12160,.T.);
#49378=ADVANCED_FACE('',(#14291),#12161,.T.);
#49379=ADVANCED_FACE('',(#14292),#12162,.T.);
#49380=ADVANCED_FACE('',(#14293),#12163,.T.);
#49381=ADVANCED_FACE('',(#14294),#12164,.T.);
#49382=ADVANCED_FACE('',(#14295),#12165,.T.);
#49383=ADVANCED_FACE('',(#14296),#12166,.T.);
#49384=ADVANCED_FACE('',(#14297),#12167,.T.);
#49385=ADVANCED_FACE('',(#14298),#1068,.F.);
#49386=ADVANCED_FACE('',(#14299),#12168,.T.);
#49387=ADVANCED_FACE('',(#14300),#12169,.T.);
#49388=ADVANCED_FACE('',(#14301),#12170,.T.);
#49389=ADVANCED_FACE('',(#14302),#12171,.T.);
#49390=ADVANCED_FACE('',(#14303),#12172,.T.);
#49391=ADVANCED_FACE('',(#14304),#12173,.T.);
#49392=ADVANCED_FACE('',(#14305),#12174,.T.);
#49393=ADVANCED_FACE('',(#14306),#12175,.T.);
#49394=ADVANCED_FACE('',(#14307),#12176,.T.);
#49395=ADVANCED_FACE('',(#14308),#12177,.T.);
#49396=ADVANCED_FACE('',(#14309),#12178,.T.);
#49397=ADVANCED_FACE('',(#14310),#12179,.T.);
#49398=ADVANCED_FACE('',(#14311),#12180,.T.);
#49399=ADVANCED_FACE('',(#14312),#12181,.T.);
#49400=ADVANCED_FACE('',(#14313),#12182,.T.);
#49401=ADVANCED_FACE('',(#14314),#12183,.T.);
#49402=ADVANCED_FACE('',(#14315),#12184,.T.);
#49403=ADVANCED_FACE('',(#14316),#12185,.T.);
#49404=ADVANCED_FACE('',(#14317),#12186,.T.);
#49405=ADVANCED_FACE('',(#14318),#12187,.T.);
#49406=ADVANCED_FACE('',(#14319),#12188,.T.);
#49407=ADVANCED_FACE('',(#14320),#12189,.T.);
#49408=ADVANCED_FACE('',(#14321),#12190,.T.);
#49409=ADVANCED_FACE('',(#14322),#12191,.T.);
#49410=ADVANCED_FACE('',(#14323),#12192,.T.);
#49411=ADVANCED_FACE('',(#14324),#12193,.T.);
#49412=ADVANCED_FACE('',(#14325),#12194,.T.);
#49413=ADVANCED_FACE('',(#14326),#12195,.T.);
#49414=ADVANCED_FACE('',(#14327),#1069,.F.);
#49415=ADVANCED_FACE('',(#14328),#12196,.T.);
#49416=ADVANCED_FACE('',(#14329),#12197,.T.);
#49417=ADVANCED_FACE('',(#14330),#12198,.T.);
#49418=ADVANCED_FACE('',(#14331),#12199,.T.);
#49419=ADVANCED_FACE('',(#14332),#12200,.T.);
#49420=ADVANCED_FACE('',(#14333),#12201,.T.);
#49421=ADVANCED_FACE('',(#14334),#12202,.T.);
#49422=ADVANCED_FACE('',(#14335),#12203,.T.);
#49423=ADVANCED_FACE('',(#14336),#12204,.T.);
#49424=ADVANCED_FACE('',(#14337),#12205,.T.);
#49425=ADVANCED_FACE('',(#14338),#12206,.T.);
#49426=ADVANCED_FACE('',(#14339),#12207,.T.);
#49427=ADVANCED_FACE('',(#14340),#12208,.T.);
#49428=ADVANCED_FACE('',(#14341),#12209,.T.);
#49429=ADVANCED_FACE('',(#14342),#12210,.T.);
#49430=ADVANCED_FACE('',(#14343),#12211,.T.);
#49431=ADVANCED_FACE('',(#14344),#12212,.T.);
#49432=ADVANCED_FACE('',(#14345),#12213,.T.);
#49433=ADVANCED_FACE('',(#14346),#12214,.T.);
#49434=ADVANCED_FACE('',(#14347),#12215,.T.);
#49435=ADVANCED_FACE('',(#14348),#12216,.T.);
#49436=ADVANCED_FACE('',(#14349),#12217,.T.);
#49437=ADVANCED_FACE('',(#14350),#12218,.T.);
#49438=ADVANCED_FACE('',(#14351),#12219,.T.);
#49439=ADVANCED_FACE('',(#14352),#12220,.T.);
#49440=ADVANCED_FACE('',(#14353),#12221,.T.);
#49441=ADVANCED_FACE('',(#14354),#12222,.T.);
#49442=ADVANCED_FACE('',(#14355),#12223,.T.);
#49443=ADVANCED_FACE('',(#14356),#1070,.F.);
#49444=ADVANCED_FACE('',(#14357),#12224,.T.);
#49445=ADVANCED_FACE('',(#14358),#12225,.T.);
#49446=ADVANCED_FACE('',(#14359),#12226,.T.);
#49447=ADVANCED_FACE('',(#14360),#12227,.T.);
#49448=ADVANCED_FACE('',(#14361),#12228,.T.);
#49449=ADVANCED_FACE('',(#14362),#12229,.T.);
#49450=ADVANCED_FACE('',(#14363),#12230,.T.);
#49451=ADVANCED_FACE('',(#14364),#12231,.T.);
#49452=ADVANCED_FACE('',(#14365),#12232,.T.);
#49453=ADVANCED_FACE('',(#14366),#12233,.T.);
#49454=ADVANCED_FACE('',(#14367),#12234,.T.);
#49455=ADVANCED_FACE('',(#14368),#12235,.T.);
#49456=ADVANCED_FACE('',(#14369),#12236,.T.);
#49457=ADVANCED_FACE('',(#14370),#12237,.T.);
#49458=ADVANCED_FACE('',(#14371),#12238,.T.);
#49459=ADVANCED_FACE('',(#14372),#12239,.T.);
#49460=ADVANCED_FACE('',(#14373),#12240,.T.);
#49461=ADVANCED_FACE('',(#14374),#12241,.T.);
#49462=ADVANCED_FACE('',(#14375),#12242,.T.);
#49463=ADVANCED_FACE('',(#14376),#12243,.T.);
#49464=ADVANCED_FACE('',(#14377),#12244,.T.);
#49465=ADVANCED_FACE('',(#14378),#12245,.T.);
#49466=ADVANCED_FACE('',(#14379),#12246,.T.);
#49467=ADVANCED_FACE('',(#14380),#12247,.T.);
#49468=ADVANCED_FACE('',(#14381),#12248,.T.);
#49469=ADVANCED_FACE('',(#14382),#12249,.T.);
#49470=ADVANCED_FACE('',(#14383),#12250,.T.);
#49471=ADVANCED_FACE('',(#14384),#12251,.T.);
#49472=ADVANCED_FACE('',(#14385),#1071,.F.);
#49473=ADVANCED_FACE('',(#14386),#12252,.T.);
#49474=ADVANCED_FACE('',(#14387),#12253,.T.);
#49475=ADVANCED_FACE('',(#14388),#12254,.T.);
#49476=ADVANCED_FACE('',(#14389),#12255,.T.);
#49477=ADVANCED_FACE('',(#14390),#12256,.T.);
#49478=ADVANCED_FACE('',(#14391),#12257,.T.);
#49479=ADVANCED_FACE('',(#14392),#12258,.T.);
#49480=ADVANCED_FACE('',(#14393),#12259,.T.);
#49481=ADVANCED_FACE('',(#14394),#12260,.T.);
#49482=ADVANCED_FACE('',(#14395),#12261,.T.);
#49483=ADVANCED_FACE('',(#14396),#12262,.T.);
#49484=ADVANCED_FACE('',(#14397),#12263,.T.);
#49485=ADVANCED_FACE('',(#14398),#12264,.T.);
#49486=ADVANCED_FACE('',(#14399),#12265,.T.);
#49487=ADVANCED_FACE('',(#14400),#12266,.T.);
#49488=ADVANCED_FACE('',(#14401),#12267,.T.);
#49489=ADVANCED_FACE('',(#14402),#12268,.T.);
#49490=ADVANCED_FACE('',(#14403),#12269,.T.);
#49491=ADVANCED_FACE('',(#14404),#12270,.T.);
#49492=ADVANCED_FACE('',(#14405),#12271,.T.);
#49493=ADVANCED_FACE('',(#14406),#12272,.T.);
#49494=ADVANCED_FACE('',(#14407),#12273,.T.);
#49495=ADVANCED_FACE('',(#14408),#12274,.T.);
#49496=ADVANCED_FACE('',(#14409),#12275,.T.);
#49497=ADVANCED_FACE('',(#14410),#12276,.T.);
#49498=ADVANCED_FACE('',(#14411),#12277,.T.);
#49499=ADVANCED_FACE('',(#14412),#12278,.T.);
#49500=ADVANCED_FACE('',(#14413),#12279,.T.);
#49501=ADVANCED_FACE('',(#14414),#1072,.F.);
#49502=ADVANCED_FACE('',(#14415),#12280,.T.);
#49503=ADVANCED_FACE('',(#14416),#12281,.T.);
#49504=ADVANCED_FACE('',(#14417),#12282,.T.);
#49505=ADVANCED_FACE('',(#14418),#12283,.T.);
#49506=ADVANCED_FACE('',(#14419),#12284,.T.);
#49507=ADVANCED_FACE('',(#14420),#12285,.T.);
#49508=ADVANCED_FACE('',(#14421),#12286,.T.);
#49509=ADVANCED_FACE('',(#14422),#12287,.T.);
#49510=ADVANCED_FACE('',(#14423),#12288,.T.);
#49511=ADVANCED_FACE('',(#14424),#12289,.T.);
#49512=ADVANCED_FACE('',(#14425),#12290,.T.);
#49513=ADVANCED_FACE('',(#14426),#12291,.T.);
#49514=ADVANCED_FACE('',(#14427),#12292,.T.);
#49515=ADVANCED_FACE('',(#14428),#12293,.T.);
#49516=ADVANCED_FACE('',(#14429),#12294,.T.);
#49517=ADVANCED_FACE('',(#14430),#12295,.T.);
#49518=ADVANCED_FACE('',(#14431),#12296,.T.);
#49519=ADVANCED_FACE('',(#14432),#12297,.T.);
#49520=ADVANCED_FACE('',(#14433),#12298,.T.);
#49521=ADVANCED_FACE('',(#14434),#12299,.T.);
#49522=ADVANCED_FACE('',(#14435),#12300,.T.);
#49523=ADVANCED_FACE('',(#14436),#12301,.T.);
#49524=ADVANCED_FACE('',(#14437),#12302,.T.);
#49525=ADVANCED_FACE('',(#14438),#12303,.T.);
#49526=ADVANCED_FACE('',(#14439),#12304,.T.);
#49527=ADVANCED_FACE('',(#14440),#12305,.T.);
#49528=ADVANCED_FACE('',(#14441),#12306,.T.);
#49529=ADVANCED_FACE('',(#14442),#12307,.T.);
#49530=ADVANCED_FACE('',(#14443),#1073,.F.);
#49531=ADVANCED_FACE('',(#14444),#12308,.T.);
#49532=ADVANCED_FACE('',(#14445),#12309,.T.);
#49533=ADVANCED_FACE('',(#14446),#12310,.T.);
#49534=ADVANCED_FACE('',(#14447),#12311,.T.);
#49535=ADVANCED_FACE('',(#14448),#12312,.T.);
#49536=ADVANCED_FACE('',(#14449),#12313,.T.);
#49537=ADVANCED_FACE('',(#14450),#12314,.T.);
#49538=ADVANCED_FACE('',(#14451),#12315,.T.);
#49539=ADVANCED_FACE('',(#14452),#12316,.T.);
#49540=ADVANCED_FACE('',(#14453),#12317,.T.);
#49541=ADVANCED_FACE('',(#14454),#12318,.T.);
#49542=ADVANCED_FACE('',(#14455),#12319,.T.);
#49543=ADVANCED_FACE('',(#14456),#12320,.T.);
#49544=ADVANCED_FACE('',(#14457),#12321,.T.);
#49545=ADVANCED_FACE('',(#14458),#12322,.T.);
#49546=ADVANCED_FACE('',(#14459),#12323,.T.);
#49547=ADVANCED_FACE('',(#14460),#12324,.T.);
#49548=ADVANCED_FACE('',(#14461),#12325,.T.);
#49549=ADVANCED_FACE('',(#14462),#12326,.T.);
#49550=ADVANCED_FACE('',(#14463),#12327,.T.);
#49551=ADVANCED_FACE('',(#14464),#12328,.T.);
#49552=ADVANCED_FACE('',(#14465),#12329,.T.);
#49553=ADVANCED_FACE('',(#14466),#12330,.T.);
#49554=ADVANCED_FACE('',(#14467),#12331,.T.);
#49555=ADVANCED_FACE('',(#14468),#12332,.T.);
#49556=ADVANCED_FACE('',(#14469),#12333,.T.);
#49557=ADVANCED_FACE('',(#14470),#12334,.T.);
#49558=ADVANCED_FACE('',(#14471),#12335,.T.);
#49559=ADVANCED_FACE('',(#14472),#1074,.F.);
#49560=ADVANCED_FACE('',(#14473),#12336,.T.);
#49561=ADVANCED_FACE('',(#14474),#12337,.T.);
#49562=ADVANCED_FACE('',(#14475),#12338,.T.);
#49563=ADVANCED_FACE('',(#14476),#12339,.T.);
#49564=ADVANCED_FACE('',(#14477),#12340,.T.);
#49565=ADVANCED_FACE('',(#14478),#12341,.T.);
#49566=ADVANCED_FACE('',(#14479),#12342,.T.);
#49567=ADVANCED_FACE('',(#14480),#12343,.T.);
#49568=ADVANCED_FACE('',(#14481),#12344,.T.);
#49569=ADVANCED_FACE('',(#14482),#12345,.T.);
#49570=ADVANCED_FACE('',(#14483),#12346,.T.);
#49571=ADVANCED_FACE('',(#14484),#12347,.T.);
#49572=ADVANCED_FACE('',(#14485),#12348,.T.);
#49573=ADVANCED_FACE('',(#14486),#12349,.T.);
#49574=ADVANCED_FACE('',(#14487),#12350,.T.);
#49575=ADVANCED_FACE('',(#14488),#12351,.T.);
#49576=ADVANCED_FACE('',(#14489),#12352,.T.);
#49577=ADVANCED_FACE('',(#14490),#12353,.T.);
#49578=ADVANCED_FACE('',(#14491),#12354,.T.);
#49579=ADVANCED_FACE('',(#14492),#12355,.T.);
#49580=ADVANCED_FACE('',(#14493),#12356,.T.);
#49581=ADVANCED_FACE('',(#14494),#12357,.T.);
#49582=ADVANCED_FACE('',(#14495),#12358,.T.);
#49583=ADVANCED_FACE('',(#14496),#12359,.T.);
#49584=ADVANCED_FACE('',(#14497),#12360,.T.);
#49585=ADVANCED_FACE('',(#14498),#12361,.T.);
#49586=ADVANCED_FACE('',(#14499),#12362,.T.);
#49587=ADVANCED_FACE('',(#14500),#12363,.T.);
#49588=ADVANCED_FACE('',(#14501),#1075,.F.);
#49589=ADVANCED_FACE('',(#14502),#12364,.T.);
#49590=ADVANCED_FACE('',(#14503),#12365,.T.);
#49591=ADVANCED_FACE('',(#14504),#12366,.T.);
#49592=ADVANCED_FACE('',(#14505),#12367,.T.);
#49593=ADVANCED_FACE('',(#14506),#12368,.T.);
#49594=ADVANCED_FACE('',(#14507),#12369,.T.);
#49595=ADVANCED_FACE('',(#14508),#12370,.T.);
#49596=ADVANCED_FACE('',(#14509),#12371,.T.);
#49597=ADVANCED_FACE('',(#14510),#12372,.T.);
#49598=ADVANCED_FACE('',(#14511),#12373,.T.);
#49599=ADVANCED_FACE('',(#14512),#12374,.T.);
#49600=ADVANCED_FACE('',(#14513),#12375,.T.);
#49601=ADVANCED_FACE('',(#14514),#12376,.T.);
#49602=ADVANCED_FACE('',(#14515),#12377,.T.);
#49603=ADVANCED_FACE('',(#14516),#12378,.T.);
#49604=ADVANCED_FACE('',(#14517),#12379,.T.);
#49605=ADVANCED_FACE('',(#14518),#12380,.T.);
#49606=ADVANCED_FACE('',(#14519),#12381,.T.);
#49607=ADVANCED_FACE('',(#14520),#12382,.T.);
#49608=ADVANCED_FACE('',(#14521),#12383,.T.);
#49609=ADVANCED_FACE('',(#14522),#12384,.T.);
#49610=ADVANCED_FACE('',(#14523),#12385,.T.);
#49611=ADVANCED_FACE('',(#14524),#12386,.T.);
#49612=ADVANCED_FACE('',(#14525),#12387,.T.);
#49613=ADVANCED_FACE('',(#14526),#12388,.T.);
#49614=ADVANCED_FACE('',(#14527),#12389,.T.);
#49615=ADVANCED_FACE('',(#14528),#12390,.T.);
#49616=ADVANCED_FACE('',(#14529),#12391,.T.);
#49617=ADVANCED_FACE('',(#14530),#1076,.F.);
#49618=ADVANCED_FACE('',(#14531),#12392,.T.);
#49619=ADVANCED_FACE('',(#14532),#12393,.T.);
#49620=ADVANCED_FACE('',(#14533),#12394,.T.);
#49621=ADVANCED_FACE('',(#14534),#12395,.T.);
#49622=ADVANCED_FACE('',(#14535),#12396,.T.);
#49623=ADVANCED_FACE('',(#14536),#12397,.T.);
#49624=ADVANCED_FACE('',(#14537),#12398,.T.);
#49625=ADVANCED_FACE('',(#14538),#12399,.T.);
#49626=ADVANCED_FACE('',(#14539),#12400,.T.);
#49627=ADVANCED_FACE('',(#14540),#12401,.T.);
#49628=ADVANCED_FACE('',(#14541),#12402,.T.);
#49629=ADVANCED_FACE('',(#14542),#12403,.T.);
#49630=ADVANCED_FACE('',(#14543),#12404,.T.);
#49631=ADVANCED_FACE('',(#14544),#12405,.T.);
#49632=ADVANCED_FACE('',(#14545),#12406,.T.);
#49633=ADVANCED_FACE('',(#14546),#12407,.T.);
#49634=ADVANCED_FACE('',(#14547),#12408,.T.);
#49635=ADVANCED_FACE('',(#14548),#12409,.T.);
#49636=ADVANCED_FACE('',(#14549),#12410,.T.);
#49637=ADVANCED_FACE('',(#14550),#12411,.T.);
#49638=ADVANCED_FACE('',(#14551),#12412,.T.);
#49639=ADVANCED_FACE('',(#14552),#12413,.T.);
#49640=ADVANCED_FACE('',(#14553),#12414,.T.);
#49641=ADVANCED_FACE('',(#14554),#12415,.T.);
#49642=ADVANCED_FACE('',(#14555),#12416,.T.);
#49643=ADVANCED_FACE('',(#14556),#12417,.T.);
#49644=ADVANCED_FACE('',(#14557),#12418,.T.);
#49645=ADVANCED_FACE('',(#14558),#12419,.T.);
#49646=ADVANCED_FACE('',(#14559),#1077,.F.);
#49647=ADVANCED_FACE('',(#14560),#12420,.T.);
#49648=ADVANCED_FACE('',(#14561),#12421,.T.);
#49649=ADVANCED_FACE('',(#14562),#12422,.T.);
#49650=ADVANCED_FACE('',(#14563),#12423,.T.);
#49651=ADVANCED_FACE('',(#14564),#12424,.T.);
#49652=ADVANCED_FACE('',(#14565),#12425,.T.);
#49653=ADVANCED_FACE('',(#14566),#12426,.T.);
#49654=ADVANCED_FACE('',(#14567),#12427,.T.);
#49655=ADVANCED_FACE('',(#14568),#12428,.T.);
#49656=ADVANCED_FACE('',(#14569),#12429,.T.);
#49657=ADVANCED_FACE('',(#14570),#12430,.T.);
#49658=ADVANCED_FACE('',(#14571),#12431,.T.);
#49659=ADVANCED_FACE('',(#14572),#12432,.T.);
#49660=ADVANCED_FACE('',(#14573),#12433,.T.);
#49661=ADVANCED_FACE('',(#14574),#12434,.T.);
#49662=ADVANCED_FACE('',(#14575),#12435,.T.);
#49663=ADVANCED_FACE('',(#14576),#12436,.T.);
#49664=ADVANCED_FACE('',(#14577),#12437,.T.);
#49665=ADVANCED_FACE('',(#14578),#12438,.T.);
#49666=ADVANCED_FACE('',(#14579),#12439,.T.);
#49667=ADVANCED_FACE('',(#14580),#12440,.T.);
#49668=ADVANCED_FACE('',(#14581),#12441,.T.);
#49669=ADVANCED_FACE('',(#14582),#12442,.T.);
#49670=ADVANCED_FACE('',(#14583),#12443,.T.);
#49671=ADVANCED_FACE('',(#14584),#12444,.T.);
#49672=ADVANCED_FACE('',(#14585),#12445,.T.);
#49673=ADVANCED_FACE('',(#14586),#12446,.T.);
#49674=ADVANCED_FACE('',(#14587),#12447,.T.);
#49675=ADVANCED_FACE('',(#14588),#1078,.F.);
#49676=ADVANCED_FACE('',(#14589),#12448,.T.);
#49677=ADVANCED_FACE('',(#14590),#12449,.T.);
#49678=ADVANCED_FACE('',(#14591),#12450,.T.);
#49679=ADVANCED_FACE('',(#14592),#12451,.T.);
#49680=ADVANCED_FACE('',(#14593),#12452,.T.);
#49681=ADVANCED_FACE('',(#14594),#12453,.T.);
#49682=ADVANCED_FACE('',(#14595),#12454,.T.);
#49683=ADVANCED_FACE('',(#14596),#12455,.T.);
#49684=ADVANCED_FACE('',(#14597),#12456,.T.);
#49685=ADVANCED_FACE('',(#14598),#12457,.T.);
#49686=ADVANCED_FACE('',(#14599),#12458,.T.);
#49687=ADVANCED_FACE('',(#14600),#12459,.T.);
#49688=ADVANCED_FACE('',(#14601),#12460,.T.);
#49689=ADVANCED_FACE('',(#14602),#12461,.T.);
#49690=ADVANCED_FACE('',(#14603),#12462,.T.);
#49691=ADVANCED_FACE('',(#14604),#12463,.T.);
#49692=ADVANCED_FACE('',(#14605),#12464,.T.);
#49693=ADVANCED_FACE('',(#14606),#12465,.T.);
#49694=ADVANCED_FACE('',(#14607),#12466,.T.);
#49695=ADVANCED_FACE('',(#14608),#12467,.T.);
#49696=ADVANCED_FACE('',(#14609),#12468,.T.);
#49697=ADVANCED_FACE('',(#14610),#12469,.T.);
#49698=ADVANCED_FACE('',(#14611),#12470,.T.);
#49699=ADVANCED_FACE('',(#14612),#12471,.T.);
#49700=ADVANCED_FACE('',(#14613),#12472,.T.);
#49701=ADVANCED_FACE('',(#14614),#12473,.T.);
#49702=ADVANCED_FACE('',(#14615),#12474,.T.);
#49703=ADVANCED_FACE('',(#14616),#12475,.T.);
#49704=ADVANCED_FACE('',(#14617),#48188,.F.);
#49705=ADVANCED_FACE('',(#14618),#48189,.T.);
#49706=ADVANCED_FACE('',(#14619),#48190,.T.);
#49707=ADVANCED_FACE('',(#14620,#959),#12476,.T.);
#49708=ADVANCED_FACE('',(#14621),#947,.T.);
#49709=ADVANCED_FACE('',(#14622),#1079,.T.);
#49710=ADVANCED_FACE('',(#14623),#948,.F.);
#49711=ADVANCED_FACE('',(#14624),#1080,.T.);
#49712=ADVANCED_FACE('',(#14625,#960),#12477,.T.);
#49713=ADVANCED_FACE('',(#14626),#949,.F.);
#49714=ADVANCED_FACE('',(#14627,#961),#12478,.T.);
#49715=ADVANCED_FACE('',(#14628),#1081,.F.);
#49716=ADVANCED_FACE('',(#14629,#962),#12479,.T.);
#49717=ADVANCED_FACE('',(#14630),#48191,.T.);
#49718=ADVANCED_FACE('',(#14631),#1082,.T.);
#49719=ADVANCED_FACE('',(#14632),#48192,.T.);
#49720=ADVANCED_FACE('',(#14633),#1083,.T.);
#49721=ADVANCED_FACE('',(#14634),#48193,.T.);
#49722=ADVANCED_FACE('',(#14635),#12480,.F.);
#49723=ADVANCED_FACE('',(#14636),#12481,.F.);
#49724=ADVANCED_FACE('',(#14637),#12482,.F.);
#49725=ADVANCED_FACE('',(#14638),#1084,.T.);
#49726=ADVANCED_FACE('',(#14639),#48194,.T.);
#49727=ADVANCED_FACE('',(#14640,#963),#12483,.T.);
#49728=ADVANCED_FACE('',(#14641),#48195,.T.);
#49729=ADVANCED_FACE('',(#14642),#48196,.T.);
#49730=ADVANCED_FACE('',(#14643),#12484,.F.);
#49731=ADVANCED_FACE('',(#14644),#12485,.F.);
#49732=ADVANCED_FACE('',(#14645),#12486,.F.);
#49733=ADVANCED_FACE('',(#14646),#48197,.T.);
#49734=ADVANCED_FACE('',(#14647),#48198,.T.);
#49735=ADVANCED_FACE('',(#14648),#1085,.T.);
#49736=ADVANCED_FACE('',(#14649),#48199,.T.);
#49737=ADVANCED_FACE('',(#14650),#12487,.F.);
#49738=ADVANCED_FACE('',(#14651),#12488,.F.);
#49739=ADVANCED_FACE('',(#14652),#12489,.F.);
#49740=ADVANCED_FACE('',(#14653),#1086,.T.);
#49741=ADVANCED_FACE('',(#14654),#48200,.T.);
#49742=ADVANCED_FACE('',(#14655),#48201,.T.);
#49743=ADVANCED_FACE('',(#14656),#48202,.T.);
#49744=ADVANCED_FACE('',(#14657),#48203,.T.);
#49745=ADVANCED_FACE('',(#14658),#48204,.T.);
#49746=ADVANCED_FACE('',(#14659),#48205,.T.);
#49747=ADVANCED_FACE('',(#14660),#48206,.T.);
#49748=ADVANCED_FACE('',(#14661),#48207,.T.);
#49749=ADVANCED_FACE('',(#14662),#48208,.T.);
#49750=ADVANCED_FACE('',(#14663),#48209,.T.);
#49751=ADVANCED_FACE('',(#14664),#48210,.T.);
#49752=ADVANCED_FACE('',(#14665),#48211,.T.);
#49753=ADVANCED_FACE('',(#14666),#48212,.T.);
#49754=ADVANCED_FACE('',(#14667),#48213,.T.);
#49755=ADVANCED_FACE('',(#14668),#48214,.T.);
#49756=ADVANCED_FACE('',(#14669),#48215,.T.);
#49757=ADVANCED_FACE('',(#14670),#48216,.T.);
#49758=ADVANCED_FACE('',(#14671),#48217,.T.);
#49759=ADVANCED_FACE('',(#14672),#48218,.T.);
#49760=ADVANCED_FACE('',(#14673),#48219,.T.);
#49761=ADVANCED_FACE('',(#14674),#48220,.T.);
#49762=ADVANCED_FACE('',(#14675),#48221,.T.);
#49763=ADVANCED_FACE('',(#14676),#48222,.T.);
#49764=ADVANCED_FACE('',(#14677),#48223,.T.);
#49765=ADVANCED_FACE('',(#14678),#48224,.T.);
#49766=ADVANCED_FACE('',(#14679),#48225,.T.);
#49767=ADVANCED_FACE('',(#14680),#48226,.T.);
#49768=ADVANCED_FACE('',(#14681),#48227,.T.);
#49769=ADVANCED_FACE('',(#14682),#48228,.T.);
#49770=ADVANCED_FACE('',(#14683),#48229,.T.);
#49771=ADVANCED_FACE('',(#14684),#48230,.T.);
#49772=ADVANCED_FACE('',(#14685),#48231,.T.);
#49773=ADVANCED_FACE('',(#14686),#48232,.T.);
#49774=ADVANCED_FACE('',(#14687),#12490,.T.);
#49775=ADVANCED_FACE('',(#14688),#12491,.T.);
#49776=ADVANCED_FACE('',(#14689),#12492,.T.);
#49777=ADVANCED_FACE('',(#14690),#12493,.T.);
#49778=ADVANCED_FACE('',(#14691),#12494,.T.);
#49779=ADVANCED_FACE('',(#14692),#12495,.T.);
#49780=ADVANCED_FACE('',(#14693),#12496,.T.);
#49781=ADVANCED_FACE('',(#14694),#12497,.T.);
#49782=ADVANCED_FACE('',(#14695),#12498,.T.);
#49783=ADVANCED_FACE('',(#14696),#12499,.T.);
#49784=ADVANCED_FACE('',(#14697),#12500,.T.);
#49785=ADVANCED_FACE('',(#14698),#12501,.T.);
#49786=ADVANCED_FACE('',(#14699),#12502,.T.);
#49787=ADVANCED_FACE('',(#14700),#12503,.T.);
#49788=ADVANCED_FACE('',(#14701),#12504,.T.);
#49789=ADVANCED_FACE('',(#14702),#12505,.T.);
#49790=ADVANCED_FACE('',(#14703),#12506,.T.);
#49791=ADVANCED_FACE('',(#14704),#12507,.T.);
#49792=ADVANCED_FACE('',(#14705),#12508,.T.);
#49793=ADVANCED_FACE('',(#14706),#12509,.T.);
#49794=ADVANCED_FACE('',(#14707),#12510,.T.);
#49795=ADVANCED_FACE('',(#14708),#12511,.T.);
#49796=ADVANCED_FACE('',(#14709),#12512,.T.);
#49797=ADVANCED_FACE('',(#14710),#12513,.T.);
#49798=ADVANCED_FACE('',(#14711),#12514,.T.);
#49799=ADVANCED_FACE('',(#14712),#12515,.T.);
#49800=ADVANCED_FACE('',(#14713),#12516,.T.);
#49801=ADVANCED_FACE('',(#14714),#12517,.T.);
#49802=ADVANCED_FACE('',(#14715),#12518,.T.);
#49803=ADVANCED_FACE('',(#14716),#12519,.T.);
#49804=ADVANCED_FACE('',(#14717),#12520,.T.);
#49805=ADVANCED_FACE('',(#14718),#12521,.T.);
#49806=ADVANCED_FACE('',(#14719),#12522,.T.);
#49807=ADVANCED_FACE('',(#14720),#12523,.T.);
#49808=ADVANCED_FACE('',(#14721),#12524,.T.);
#49809=ADVANCED_FACE('',(#14722),#12525,.T.);
#49810=ADVANCED_FACE('',(#14723),#12526,.T.);
#49811=ADVANCED_FACE('',(#14724),#12527,.T.);
#49812=ADVANCED_FACE('',(#14725),#12528,.T.);
#49813=ADVANCED_FACE('',(#14726),#12529,.T.);
#49814=ADVANCED_FACE('',(#14727),#12530,.T.);
#49815=ADVANCED_FACE('',(#14728),#12531,.T.);
#49816=ADVANCED_FACE('',(#14729),#12532,.T.);
#49817=ADVANCED_FACE('',(#14730),#12533,.T.);
#49818=ADVANCED_FACE('',(#14731),#12534,.T.);
#49819=ADVANCED_FACE('',(#14732),#12535,.T.);
#49820=ADVANCED_FACE('',(#14733),#12536,.T.);
#49821=ADVANCED_FACE('',(#14734),#12537,.T.);
#49822=ADVANCED_FACE('',(#14735),#12538,.T.);
#49823=ADVANCED_FACE('',(#14736),#12539,.T.);
#49824=ADVANCED_FACE('',(#14737),#12540,.T.);
#49825=ADVANCED_FACE('',(#14738),#12541,.T.);
#49826=ADVANCED_FACE('',(#14739),#12542,.T.);
#49827=ADVANCED_FACE('',(#14740),#12543,.T.);
#49828=ADVANCED_FACE('',(#14741),#12544,.T.);
#49829=ADVANCED_FACE('',(#14742),#12545,.T.);
#49830=ADVANCED_FACE('',(#14743),#12546,.T.);
#49831=ADVANCED_FACE('',(#14744),#12547,.T.);
#49832=ADVANCED_FACE('',(#14745),#12548,.T.);
#49833=ADVANCED_FACE('',(#14746),#12549,.T.);
#49834=ADVANCED_FACE('',(#14747),#12550,.T.);
#49835=ADVANCED_FACE('',(#14748),#12551,.T.);
#49836=ADVANCED_FACE('',(#14749),#12552,.T.);
#49837=ADVANCED_FACE('',(#14750),#12553,.T.);
#49838=ADVANCED_FACE('',(#14751),#12554,.T.);
#49839=ADVANCED_FACE('',(#14752),#12555,.T.);
#49840=ADVANCED_FACE('',(#14753),#48233,.T.);
#49841=ADVANCED_FACE('',(#14754),#48234,.T.);
#49842=ADVANCED_FACE('',(#14755),#48235,.T.);
#49843=ADVANCED_FACE('',(#14756),#48236,.T.);
#49844=ADVANCED_FACE('',(#14757),#48237,.T.);
#49845=ADVANCED_FACE('',(#14758),#48238,.T.);
#49846=ADVANCED_FACE('',(#14759),#48239,.T.);
#49847=ADVANCED_FACE('',(#14760),#48240,.T.);
#49848=ADVANCED_FACE('',(#14761),#48241,.T.);
#49849=ADVANCED_FACE('',(#14762),#48242,.T.);
#49850=ADVANCED_FACE('',(#14763),#48243,.T.);
#49851=ADVANCED_FACE('',(#14764),#48244,.T.);
#49852=ADVANCED_FACE('',(#14765),#48245,.T.);
#49853=ADVANCED_FACE('',(#14766),#48246,.T.);
#49854=ADVANCED_FACE('',(#14767),#48247,.T.);
#49855=ADVANCED_FACE('',(#14768),#48248,.T.);
#49856=ADVANCED_FACE('',(#14769),#48249,.T.);
#49857=ADVANCED_FACE('',(#14770),#48250,.T.);
#49858=ADVANCED_FACE('',(#14771),#48251,.T.);
#49859=ADVANCED_FACE('',(#14772),#48252,.T.);
#49860=ADVANCED_FACE('',(#14773),#48253,.T.);
#49861=ADVANCED_FACE('',(#14774),#48254,.T.);
#49862=ADVANCED_FACE('',(#14775),#48255,.T.);
#49863=ADVANCED_FACE('',(#14776),#48256,.T.);
#49864=ADVANCED_FACE('',(#14777),#48257,.T.);
#49865=ADVANCED_FACE('',(#14778),#48258,.T.);
#49866=ADVANCED_FACE('',(#14779),#48259,.T.);
#49867=ADVANCED_FACE('',(#14780),#48260,.T.);
#49868=ADVANCED_FACE('',(#14781),#48261,.T.);
#49869=ADVANCED_FACE('',(#14782),#48262,.T.);
#49870=ADVANCED_FACE('',(#14783),#48263,.T.);
#49871=ADVANCED_FACE('',(#14784),#48264,.T.);
#49872=ADVANCED_FACE('',(#14785),#48265,.T.);
#49873=ADVANCED_FACE('',(#14786),#12556,.T.);
#49874=ADVANCED_FACE('',(#14787),#12557,.T.);
#49875=ADVANCED_FACE('',(#14788),#12558,.T.);
#49876=ADVANCED_FACE('',(#14789),#12559,.T.);
#49877=ADVANCED_FACE('',(#14790),#12560,.T.);
#49878=ADVANCED_FACE('',(#14791),#12561,.T.);
#49879=ADVANCED_FACE('',(#14792),#12562,.T.);
#49880=ADVANCED_FACE('',(#14793),#12563,.T.);
#49881=ADVANCED_FACE('',(#14794),#12564,.T.);
#49882=ADVANCED_FACE('',(#14795),#12565,.T.);
#49883=ADVANCED_FACE('',(#14796),#12566,.T.);
#49884=ADVANCED_FACE('',(#14797),#12567,.T.);
#49885=ADVANCED_FACE('',(#14798),#12568,.T.);
#49886=ADVANCED_FACE('',(#14799),#12569,.T.);
#49887=ADVANCED_FACE('',(#14800),#12570,.T.);
#49888=ADVANCED_FACE('',(#14801),#12571,.T.);
#49889=ADVANCED_FACE('',(#14802),#12572,.T.);
#49890=ADVANCED_FACE('',(#14803),#12573,.T.);
#49891=ADVANCED_FACE('',(#14804),#12574,.T.);
#49892=ADVANCED_FACE('',(#14805),#12575,.T.);
#49893=ADVANCED_FACE('',(#14806),#12576,.T.);
#49894=ADVANCED_FACE('',(#14807),#12577,.T.);
#49895=ADVANCED_FACE('',(#14808),#12578,.T.);
#49896=ADVANCED_FACE('',(#14809),#12579,.T.);
#49897=ADVANCED_FACE('',(#14810),#12580,.T.);
#49898=ADVANCED_FACE('',(#14811),#12581,.T.);
#49899=ADVANCED_FACE('',(#14812),#12582,.T.);
#49900=ADVANCED_FACE('',(#14813),#12583,.T.);
#49901=ADVANCED_FACE('',(#14814),#12584,.T.);
#49902=ADVANCED_FACE('',(#14815),#12585,.T.);
#49903=ADVANCED_FACE('',(#14816),#12586,.T.);
#49904=ADVANCED_FACE('',(#14817),#12587,.T.);
#49905=ADVANCED_FACE('',(#14818),#12588,.T.);
#49906=ADVANCED_FACE('',(#14819),#12589,.T.);
#49907=ADVANCED_FACE('',(#14820),#12590,.T.);
#49908=ADVANCED_FACE('',(#14821),#12591,.T.);
#49909=ADVANCED_FACE('',(#14822),#12592,.F.);
#49910=ADVANCED_FACE('',(#14823),#1087,.T.);
#49911=ADVANCED_FACE('',(#14824),#1088,.T.);
#49912=ADVANCED_FACE('',(#14825),#12593,.T.);
#49913=ADVANCED_FACE('',(#14826),#12594,.T.);
#49914=ADVANCED_FACE('',(#14827),#12595,.T.);
#49915=ADVANCED_FACE('',(#14828),#12596,.F.);
#49916=ADVANCED_FACE('',(#14829),#1089,.T.);
#49917=ADVANCED_FACE('',(#14830),#12597,.T.);
#49918=ADVANCED_FACE('',(#14831),#12598,.T.);
#49919=ADVANCED_FACE('',(#14832),#12599,.T.);
#49920=ADVANCED_FACE('',(#14833),#12600,.F.);
#49921=ADVANCED_FACE('',(#14834),#1090,.T.);
#49922=ADVANCED_FACE('',(#14835),#12601,.T.);
#49923=ADVANCED_FACE('',(#14836),#12602,.T.);
#49924=ADVANCED_FACE('',(#14837),#12603,.T.);
#49925=ADVANCED_FACE('',(#14838),#12604,.F.);
#49926=ADVANCED_FACE('',(#14839),#1091,.T.);
#49927=ADVANCED_FACE('',(#14840),#12605,.T.);
#49928=ADVANCED_FACE('',(#14841),#12606,.T.);
#49929=ADVANCED_FACE('',(#14842),#12607,.T.);
#49930=ADVANCED_FACE('',(#14843),#12608,.F.);
#49931=ADVANCED_FACE('',(#14844),#1092,.T.);
#49932=ADVANCED_FACE('',(#14845),#12609,.T.);
#49933=ADVANCED_FACE('',(#14846),#12610,.T.);
#49934=ADVANCED_FACE('',(#14847),#12611,.T.);
#49935=ADVANCED_FACE('',(#14848),#12612,.F.);
#49936=ADVANCED_FACE('',(#14849),#1093,.T.);
#49937=ADVANCED_FACE('',(#14850),#12613,.T.);
#49938=ADVANCED_FACE('',(#14851),#12614,.T.);
#49939=ADVANCED_FACE('',(#14852),#12615,.T.);
#49940=ADVANCED_FACE('',(#14853),#12616,.F.);
#49941=ADVANCED_FACE('',(#14854),#1094,.T.);
#49942=ADVANCED_FACE('',(#14855),#12617,.T.);
#49943=ADVANCED_FACE('',(#14856),#12618,.T.);
#49944=ADVANCED_FACE('',(#14857),#12619,.T.);
#49945=ADVANCED_FACE('',(#14858),#12620,.F.);
#49946=ADVANCED_FACE('',(#14859),#1095,.T.);
#49947=ADVANCED_FACE('',(#14860),#12621,.T.);
#49948=ADVANCED_FACE('',(#14861),#12622,.T.);
#49949=ADVANCED_FACE('',(#14862),#12623,.T.);
#49950=ADVANCED_FACE('',(#14863),#12624,.F.);
#49951=ADVANCED_FACE('',(#14864),#1096,.T.);
#49952=ADVANCED_FACE('',(#14865),#12625,.T.);
#49953=ADVANCED_FACE('',(#14866),#12626,.T.);
#49954=ADVANCED_FACE('',(#14867),#12627,.T.);
#49955=ADVANCED_FACE('',(#14868),#12628,.F.);
#49956=ADVANCED_FACE('',(#14869),#1097,.T.);
#49957=ADVANCED_FACE('',(#14870),#12629,.T.);
#49958=ADVANCED_FACE('',(#14871),#12630,.T.);
#49959=ADVANCED_FACE('',(#14872),#12631,.T.);
#49960=ADVANCED_FACE('',(#14873),#12632,.F.);
#49961=ADVANCED_FACE('',(#14874),#1098,.T.);
#49962=ADVANCED_FACE('',(#14875),#12633,.T.);
#49963=ADVANCED_FACE('',(#14876),#12634,.T.);
#49964=ADVANCED_FACE('',(#14877),#12635,.T.);
#49965=ADVANCED_FACE('',(#14878),#12636,.F.);
#49966=ADVANCED_FACE('',(#14879),#1099,.T.);
#49967=ADVANCED_FACE('',(#14880),#12637,.T.);
#49968=ADVANCED_FACE('',(#14881),#12638,.T.);
#49969=ADVANCED_FACE('',(#14882),#12639,.T.);
#49970=ADVANCED_FACE('',(#14883),#12640,.F.);
#49971=ADVANCED_FACE('',(#14884),#1100,.T.);
#49972=ADVANCED_FACE('',(#14885),#12641,.T.);
#49973=ADVANCED_FACE('',(#14886),#12642,.T.);
#49974=ADVANCED_FACE('',(#14887),#12643,.T.);
#49975=ADVANCED_FACE('',(#14888),#12644,.F.);
#49976=ADVANCED_FACE('',(#14889),#1101,.T.);
#49977=ADVANCED_FACE('',(#14890),#12645,.T.);
#49978=ADVANCED_FACE('',(#14891),#12646,.T.);
#49979=ADVANCED_FACE('',(#14892),#12647,.T.);
#49980=ADVANCED_FACE('',(#14893),#12648,.F.);
#49981=ADVANCED_FACE('',(#14894),#1102,.T.);
#49982=ADVANCED_FACE('',(#14895),#12649,.T.);
#49983=ADVANCED_FACE('',(#14896),#12650,.T.);
#49984=ADVANCED_FACE('',(#14897),#12651,.T.);
#49985=ADVANCED_FACE('',(#14898),#12652,.F.);
#49986=ADVANCED_FACE('',(#14899),#1103,.T.);
#49987=ADVANCED_FACE('',(#14900),#12653,.T.);
#49988=ADVANCED_FACE('',(#14901),#12654,.T.);
#49989=ADVANCED_FACE('',(#14902),#12655,.T.);
#49990=ADVANCED_FACE('',(#14903),#12656,.F.);
#49991=ADVANCED_FACE('',(#14904),#1104,.T.);
#49992=ADVANCED_FACE('',(#14905),#12657,.T.);
#49993=ADVANCED_FACE('',(#14906),#12658,.T.);
#49994=ADVANCED_FACE('',(#14907),#12659,.T.);
#49995=ADVANCED_FACE('',(#14908),#12660,.F.);
#49996=ADVANCED_FACE('',(#14909),#1105,.T.);
#49997=ADVANCED_FACE('',(#14910),#12661,.T.);
#49998=ADVANCED_FACE('',(#14911),#12662,.T.);
#49999=ADVANCED_FACE('',(#14912),#12663,.T.);
#50000=ADVANCED_FACE('',(#14913),#12664,.F.);
#50001=ADVANCED_FACE('',(#14914),#1106,.T.);
#50002=ADVANCED_FACE('',(#14915),#12665,.T.);
#50003=ADVANCED_FACE('',(#14916),#12666,.T.);
#50004=ADVANCED_FACE('',(#14917),#12667,.T.);
#50005=ADVANCED_FACE('',(#14918),#12668,.F.);
#50006=ADVANCED_FACE('',(#14919),#1107,.T.);
#50007=ADVANCED_FACE('',(#14920),#12669,.T.);
#50008=ADVANCED_FACE('',(#14921),#12670,.T.);
#50009=ADVANCED_FACE('',(#14922),#12671,.T.);
#50010=ADVANCED_FACE('',(#14923),#12672,.F.);
#50011=ADVANCED_FACE('',(#14924),#1108,.T.);
#50012=ADVANCED_FACE('',(#14925),#12673,.T.);
#50013=ADVANCED_FACE('',(#14926),#12674,.T.);
#50014=ADVANCED_FACE('',(#14927),#12675,.T.);
#50015=ADVANCED_FACE('',(#14928),#12676,.F.);
#50016=ADVANCED_FACE('',(#14929),#1109,.T.);
#50017=ADVANCED_FACE('',(#14930),#12677,.T.);
#50018=ADVANCED_FACE('',(#14931),#12678,.T.);
#50019=ADVANCED_FACE('',(#14932),#12679,.T.);
#50020=ADVANCED_FACE('',(#14933),#12680,.F.);
#50021=ADVANCED_FACE('',(#14934),#1110,.T.);
#50022=ADVANCED_FACE('',(#14935),#12681,.T.);
#50023=ADVANCED_FACE('',(#14936),#12682,.T.);
#50024=ADVANCED_FACE('',(#14937),#12683,.T.);
#50025=ADVANCED_FACE('',(#14938),#12684,.F.);
#50026=ADVANCED_FACE('',(#14939),#1111,.T.);
#50027=ADVANCED_FACE('',(#14940),#12685,.T.);
#50028=ADVANCED_FACE('',(#14941),#12686,.T.);
#50029=ADVANCED_FACE('',(#14942),#12687,.T.);
#50030=ADVANCED_FACE('',(#14943),#12688,.F.);
#50031=ADVANCED_FACE('',(#14944),#1112,.T.);
#50032=ADVANCED_FACE('',(#14945),#12689,.T.);
#50033=ADVANCED_FACE('',(#14946),#12690,.T.);
#50034=ADVANCED_FACE('',(#14947),#12691,.T.);
#50035=ADVANCED_FACE('',(#14948),#12692,.F.);
#50036=ADVANCED_FACE('',(#14949),#1113,.T.);
#50037=ADVANCED_FACE('',(#14950),#12693,.T.);
#50038=ADVANCED_FACE('',(#14951),#12694,.T.);
#50039=ADVANCED_FACE('',(#14952),#12695,.T.);
#50040=ADVANCED_FACE('',(#14953),#12696,.F.);
#50041=ADVANCED_FACE('',(#14954),#1114,.T.);
#50042=ADVANCED_FACE('',(#14955),#12697,.T.);
#50043=ADVANCED_FACE('',(#14956),#12698,.T.);
#50044=ADVANCED_FACE('',(#14957),#12699,.T.);
#50045=ADVANCED_FACE('',(#14958),#12700,.F.);
#50046=ADVANCED_FACE('',(#14959),#1115,.T.);
#50047=ADVANCED_FACE('',(#14960),#12701,.T.);
#50048=ADVANCED_FACE('',(#14961),#12702,.T.);
#50049=ADVANCED_FACE('',(#14962),#12703,.T.);
#50050=ADVANCED_FACE('',(#14963),#12704,.F.);
#50051=ADVANCED_FACE('',(#14964),#1116,.T.);
#50052=ADVANCED_FACE('',(#14965),#12705,.T.);
#50053=ADVANCED_FACE('',(#14966),#12706,.T.);
#50054=ADVANCED_FACE('',(#14967),#12707,.T.);
#50055=ADVANCED_FACE('',(#14968),#12708,.F.);
#50056=ADVANCED_FACE('',(#14969),#1117,.T.);
#50057=ADVANCED_FACE('',(#14970),#12709,.T.);
#50058=ADVANCED_FACE('',(#14971),#12710,.T.);
#50059=ADVANCED_FACE('',(#14972),#12711,.T.);
#50060=ADVANCED_FACE('',(#14973),#12712,.F.);
#50061=ADVANCED_FACE('',(#14974),#1118,.T.);
#50062=ADVANCED_FACE('',(#14975),#12713,.T.);
#50063=ADVANCED_FACE('',(#14976),#12714,.T.);
#50064=ADVANCED_FACE('',(#14977),#12715,.T.);
#50065=ADVANCED_FACE('',(#14978),#12716,.F.);
#50066=ADVANCED_FACE('',(#14979),#1119,.T.);
#50067=ADVANCED_FACE('',(#14980),#12717,.T.);
#50068=ADVANCED_FACE('',(#14981),#12718,.T.);
#50069=ADVANCED_FACE('',(#14982),#12719,.T.);
#50070=ADVANCED_FACE('',(#14983),#12720,.F.);
#50071=ADVANCED_FACE('',(#14984),#950,.F.);
#50072=ADVANCED_FACE('',(#14985,#964),#12721,.T.);
#50073=ADVANCED_FACE('',(#14986),#1120,.F.);
#50074=ADVANCED_FACE('',(#14987),#951,.F.);
#50075=ADVANCED_FACE('',(#14988,#965),#12722,.T.);
#50076=ADVANCED_FACE('',(#14989),#1121,.F.);
#50077=ADVANCED_FACE('',(#14990),#952,.F.);
#50078=ADVANCED_FACE('',(#14991),#1122,.T.);
#50079=ADVANCED_FACE('',(#14992),#953,.F.);
#50080=ADVANCED_FACE('',(#14993),#1123,.T.);
#50081=ADVANCED_FACE('',(#14994),#1124,.F.);
#50082=ADVANCED_FACE('',(#14995),#48266,.F.);
#50083=ADVANCED_FACE('',(#14996,#966),#12723,.T.);
#50084=ADVANCED_FACE('',(#14997,#967),#12724,.T.);
#50085=ADVANCED_FACE('',(#14998,#968),#12725,.T.);
#50086=ADVANCED_FACE('',(#14999),#48267,.F.);
#50087=ADVANCED_FACE('',(#15000),#48268,.F.);
#50088=ADVANCED_FACE('',(#15001,#969,#970,#971,#972,#973,#974,#975),#12726,
 .T.);
#50089=ADVANCED_FACE('',(#15002),#1125,.F.);
#50090=ADVANCED_FACE('',(#15003),#48269,.F.);
#50091=ADVANCED_FACE('',(#15004),#1126,.F.);
#50092=ADVANCED_FACE('',(#15005),#1127,.F.);
#50093=ADVANCED_FACE('',(#15006),#1128,.F.);
#50094=ADVANCED_FACE('',(#15007),#1129,.F.);
#50095=ADVANCED_FACE('',(#15008),#1130,.F.);
#50096=ADVANCED_FACE('',(#15009),#1131,.F.);
#50097=ADVANCED_FACE('',(#15010,#976),#12727,.T.);
#50098=ADVANCED_FACE('',(#15011),#1132,.F.);
#50099=ADVANCED_FACE('',(#15012,#977),#12728,.T.);
#50100=ADVANCED_FACE('',(#15013),#1133,.F.);
#50101=ADVANCED_FACE('',(#15014,#978),#12729,.T.);
#50102=ADVANCED_FACE('',(#15015),#1134,.F.);
#50103=ADVANCED_FACE('',(#15016,#979),#12730,.T.);
#50104=ADVANCED_FACE('',(#15017),#48270,.F.);
#50105=ADVANCED_FACE('',(#15018),#1135,.F.);
#50106=ADVANCED_FACE('',(#15019),#48271,.F.);
#50107=ADVANCED_FACE('',(#15020),#954,.F.);
#50108=ADVANCED_FACE('',(#15021),#1136,.T.);
#50109=ADVANCED_FACE('',(#15022),#12731,.T.);
#50110=ADVANCED_FACE('',(#15023),#48272,.T.);
#50111=ADVANCED_FACE('',(#15024),#1137,.T.);
#50112=ADVANCED_FACE('',(#15025,#980,#981,#982,#983,#984,#985,#986),#12732,
 .T.);
#50113=ADVANCED_FACE('',(#15026),#48273,.T.);
#50114=ADVANCED_FACE('',(#15027),#1138,.T.);
#50115=ADVANCED_FACE('',(#15028),#48274,.T.);
#50116=ADVANCED_FACE('',(#15029,#987),#12733,.T.);
#50117=ADVANCED_FACE('',(#15030),#1139,.T.);
#50118=ADVANCED_FACE('',(#15031),#48275,.T.);
#50119=ADVANCED_FACE('',(#15032,#988),#12734,.T.);
#50120=ADVANCED_FACE('',(#15033),#12735,.F.);
#50121=ADVANCED_FACE('',(#15034),#12736,.F.);
#50122=ADVANCED_FACE('',(#15035),#12737,.F.);
#50123=ADVANCED_FACE('',(#15036),#12738,.F.);
#50124=ADVANCED_FACE('',(#15037),#12739,.F.);
#50125=ADVANCED_FACE('',(#15038),#12740,.F.);
#50126=ADVANCED_FACE('',(#15039),#12741,.F.);
#50127=ADVANCED_FACE('',(#15040),#12742,.F.);
#50128=ADVANCED_FACE('',(#15041),#12743,.F.);
#50129=ADVANCED_FACE('',(#15042),#12744,.F.);
#50130=ADVANCED_FACE('',(#15043),#12745,.F.);
#50131=ADVANCED_FACE('',(#15044),#12746,.F.);
#50132=ADVANCED_FACE('',(#15045),#12747,.F.);
#50133=ADVANCED_FACE('',(#15046),#12748,.F.);
#50134=ADVANCED_FACE('',(#15047),#12749,.F.);
#50135=ADVANCED_FACE('',(#15048),#12750,.F.);
#50136=ADVANCED_FACE('',(#15049),#12751,.F.);
#50137=ADVANCED_FACE('',(#15050),#12752,.F.);
#50138=ADVANCED_FACE('',(#15051),#719,.F.);
#50139=ADVANCED_FACE('',(#15052),#720,.F.);
#50140=ADVANCED_FACE('',(#15053),#721,.F.);
#50141=ADVANCED_FACE('',(#15054),#722,.F.);
#50142=ADVANCED_FACE('',(#15055),#723,.F.);
#50143=ADVANCED_FACE('',(#15056),#724,.F.);
#50144=ADVANCED_FACE('',(#15057),#725,.F.);
#50145=ADVANCED_FACE('',(#15058),#726,.F.);
#50146=ADVANCED_FACE('',(#15059),#727,.F.);
#50147=ADVANCED_FACE('',(#15060),#728,.F.);
#50148=ADVANCED_FACE('',(#15061),#729,.F.);
#50149=ADVANCED_FACE('',(#15062),#730,.F.);
#50150=ADVANCED_FACE('',(#15063),#731,.F.);
#50151=ADVANCED_FACE('',(#15064),#12753,.F.);
#50152=ADVANCED_FACE('',(#15065),#732,.F.);
#50153=ADVANCED_FACE('',(#15066),#733,.F.);
#50154=ADVANCED_FACE('',(#15067),#734,.F.);
#50155=ADVANCED_FACE('',(#15068),#735,.F.);
#50156=ADVANCED_FACE('',(#15069),#736,.F.);
#50157=ADVANCED_FACE('',(#15070),#737,.F.);
#50158=ADVANCED_FACE('',(#15071),#738,.F.);
#50159=ADVANCED_FACE('',(#15072),#739,.F.);
#50160=ADVANCED_FACE('',(#15073),#740,.F.);
#50161=ADVANCED_FACE('',(#15074),#741,.F.);
#50162=ADVANCED_FACE('',(#15075),#742,.F.);
#50163=ADVANCED_FACE('',(#15076),#743,.F.);
#50164=ADVANCED_FACE('',(#15077),#744,.F.);
#50165=ADVANCED_FACE('',(#15078),#745,.F.);
#50166=ADVANCED_FACE('',(#15079),#746,.F.);
#50167=ADVANCED_FACE('',(#15080),#747,.F.);
#50168=ADVANCED_FACE('',(#15081),#748,.F.);
#50169=ADVANCED_FACE('',(#15082),#749,.F.);
#50170=ADVANCED_FACE('',(#15083),#12754,.F.);
#50171=ADVANCED_FACE('',(#15084),#750,.F.);
#50172=ADVANCED_FACE('',(#15085),#751,.F.);
#50173=ADVANCED_FACE('',(#15086),#12755,.T.);
#50174=ADVANCED_FACE('',(#15087),#752,.F.);
#50175=ADVANCED_FACE('',(#15088),#753,.F.);
#50176=ADVANCED_FACE('',(#15089),#754,.F.);
#50177=ADVANCED_FACE('',(#15090),#755,.F.);
#50178=ADVANCED_FACE('',(#15091),#756,.F.);
#50179=ADVANCED_FACE('',(#15092),#757,.F.);
#50180=ADVANCED_FACE('',(#15093),#758,.F.);
#50181=ADVANCED_FACE('',(#15094),#759,.F.);
#50182=ADVANCED_FACE('',(#15095),#12756,.F.);
#50183=ADVANCED_FACE('',(#15096),#760,.F.);
#50184=ADVANCED_FACE('',(#15097),#761,.F.);
#50185=ADVANCED_FACE('',(#15098),#762,.F.);
#50186=ADVANCED_FACE('',(#15099),#763,.F.);
#50187=ADVANCED_FACE('',(#15100),#764,.F.);
#50188=ADVANCED_FACE('',(#15101),#765,.F.);
#50189=ADVANCED_FACE('',(#15102),#766,.F.);
#50190=ADVANCED_FACE('',(#15103),#767,.F.);
#50191=ADVANCED_FACE('',(#15104),#768,.F.);
#50192=ADVANCED_FACE('',(#15105),#769,.F.);
#50193=ADVANCED_FACE('',(#15106),#12757,.F.);
#50194=ADVANCED_FACE('',(#15107),#770,.F.);
#50195=ADVANCED_FACE('',(#15108),#771,.F.);
#50196=ADVANCED_FACE('',(#15109),#12758,.T.);
#50197=ADVANCED_FACE('',(#15110),#12759,.F.);
#50198=ADVANCED_FACE('',(#15111),#12760,.F.);
#50199=ADVANCED_FACE('',(#15112),#12761,.F.);
#50200=ADVANCED_FACE('',(#15113),#12762,.F.);
#50201=ADVANCED_FACE('',(#15114),#12763,.F.);
#50202=ADVANCED_FACE('',(#15115),#12764,.F.);
#50203=ADVANCED_FACE('',(#15116),#12765,.F.);
#50204=ADVANCED_FACE('',(#15117),#12766,.F.);
#50205=ADVANCED_FACE('',(#15118),#12767,.F.);
#50206=ADVANCED_FACE('',(#15119),#12768,.F.);
#50207=ADVANCED_FACE('',(#15120),#12769,.F.);
#50208=ADVANCED_FACE('',(#15121),#12770,.F.);
#50209=ADVANCED_FACE('',(#15122),#12771,.F.);
#50210=ADVANCED_FACE('',(#15123),#12772,.F.);
#50211=ADVANCED_FACE('',(#15124),#12773,.F.);
#50212=ADVANCED_FACE('',(#15125),#12774,.F.);
#50213=ADVANCED_FACE('',(#15126),#772,.F.);
#50214=ADVANCED_FACE('',(#15127),#773,.F.);
#50215=ADVANCED_FACE('',(#15128),#774,.F.);
#50216=ADVANCED_FACE('',(#15129),#775,.F.);
#50217=ADVANCED_FACE('',(#15130),#12775,.F.);
#50218=ADVANCED_FACE('',(#15131),#12776,.F.);
#50219=ADVANCED_FACE('',(#15132),#12777,.F.);
#50220=ADVANCED_FACE('',(#15133),#776,.F.);
#50221=ADVANCED_FACE('',(#15134),#777,.F.);
#50222=ADVANCED_FACE('',(#15135),#778,.F.);
#50223=ADVANCED_FACE('',(#15136),#779,.F.);
#50224=ADVANCED_FACE('',(#15137),#780,.F.);
#50225=ADVANCED_FACE('',(#15138),#781,.F.);
#50226=ADVANCED_FACE('',(#15139),#12778,.F.);
#50227=ADVANCED_FACE('',(#15140),#12779,.F.);
#50228=ADVANCED_FACE('',(#15141),#12780,.F.);
#50229=ADVANCED_FACE('',(#15142),#782,.F.);
#50230=ADVANCED_FACE('',(#15143),#12781,.T.);
#50231=ADVANCED_FACE('',(#15144),#12782,.F.);
#50232=ADVANCED_FACE('',(#15145),#783,.F.);
#50233=ADVANCED_FACE('',(#15146),#784,.F.);
#50234=ADVANCED_FACE('',(#15147),#785,.F.);
#50235=ADVANCED_FACE('',(#15148),#786,.F.);
#50236=ADVANCED_FACE('',(#15149),#12783,.F.);
#50237=ADVANCED_FACE('',(#15150),#12784,.F.);
#50238=ADVANCED_FACE('',(#15151),#12785,.F.);
#50239=ADVANCED_FACE('',(#15152),#787,.F.);
#50240=ADVANCED_FACE('',(#15153),#788,.F.);
#50241=ADVANCED_FACE('',(#15154),#789,.F.);
#50242=ADVANCED_FACE('',(#15155),#790,.F.);
#50243=ADVANCED_FACE('',(#15156),#791,.F.);
#50244=ADVANCED_FACE('',(#15157),#792,.F.);
#50245=ADVANCED_FACE('',(#15158),#793,.F.);
#50246=ADVANCED_FACE('',(#15159),#12786,.F.);
#50247=ADVANCED_FACE('',(#15160),#12787,.F.);
#50248=ADVANCED_FACE('',(#15161),#12788,.F.);
#50249=ADVANCED_FACE('',(#15162),#12789,.F.);
#50250=ADVANCED_FACE('',(#15163),#12790,.T.);
#50251=ADVANCED_FACE('',(#15164),#12791,.F.);
#50252=ADVANCED_FACE('',(#15165),#12792,.F.);
#50253=ADVANCED_FACE('',(#15166),#12793,.F.);
#50254=ADVANCED_FACE('',(#15167),#12794,.F.);
#50255=ADVANCED_FACE('',(#15168),#12795,.F.);
#50256=ADVANCED_FACE('',(#15169),#12796,.F.);
#50257=ADVANCED_FACE('',(#15170),#12797,.F.);
#50258=ADVANCED_FACE('',(#15171),#12798,.F.);
#50259=ADVANCED_FACE('',(#15172),#12799,.F.);
#50260=ADVANCED_FACE('',(#15173),#794,.F.);
#50261=ADVANCED_FACE('',(#15174),#795,.F.);
#50262=ADVANCED_FACE('',(#15175),#12800,.F.);
#50263=ADVANCED_FACE('',(#15176),#796,.F.);
#50264=ADVANCED_FACE('',(#15177),#797,.F.);
#50265=ADVANCED_FACE('',(#15178),#12801,.F.);
#50266=ADVANCED_FACE('',(#15179),#12802,.F.);
#50267=ADVANCED_FACE('',(#15180),#12803,.F.);
#50268=ADVANCED_FACE('',(#15181),#12804,.F.);
#50269=ADVANCED_FACE('',(#15182),#12805,.T.);
#50270=ADVANCED_FACE('',(#15183),#798,.F.);
#50271=ADVANCED_FACE('',(#15184),#799,.F.);
#50272=ADVANCED_FACE('',(#15185),#800,.F.);
#50273=ADVANCED_FACE('',(#15186),#801,.F.);
#50274=ADVANCED_FACE('',(#15187),#802,.F.);
#50275=ADVANCED_FACE('',(#15188),#803,.F.);
#50276=ADVANCED_FACE('',(#15189),#804,.F.);
#50277=ADVANCED_FACE('',(#15190),#805,.F.);
#50278=ADVANCED_FACE('',(#15191),#806,.F.);
#50279=ADVANCED_FACE('',(#15192),#807,.F.);
#50280=ADVANCED_FACE('',(#15193),#808,.F.);
#50281=ADVANCED_FACE('',(#15194),#809,.F.);
#50282=ADVANCED_FACE('',(#15195),#12806,.T.);
#50283=ADVANCED_FACE('',(#15196),#810,.F.);
#50284=ADVANCED_FACE('',(#15197),#811,.F.);
#50285=ADVANCED_FACE('',(#15198),#12807,.F.);
#50286=ADVANCED_FACE('',(#15199),#812,.F.);
#50287=ADVANCED_FACE('',(#15200),#813,.F.);
#50288=ADVANCED_FACE('',(#15201),#12808,.F.);
#50289=ADVANCED_FACE('',(#15202),#12809,.F.);
#50290=ADVANCED_FACE('',(#15203),#12810,.F.);
#50291=ADVANCED_FACE('',(#15204),#12811,.F.);
#50292=ADVANCED_FACE('',(#15205),#12812,.T.);
#50293=ADVANCED_FACE('',(#15206),#12813,.F.);
#50294=ADVANCED_FACE('',(#15207),#12814,.F.);
#50295=ADVANCED_FACE('',(#15208),#12815,.F.);
#50296=ADVANCED_FACE('',(#15209),#12816,.F.);
#50297=ADVANCED_FACE('',(#15210),#12817,.F.);
#50298=ADVANCED_FACE('',(#15211),#814,.F.);
#50299=ADVANCED_FACE('',(#15212),#815,.F.);
#50300=ADVANCED_FACE('',(#15213),#816,.F.);
#50301=ADVANCED_FACE('',(#15214),#817,.F.);
#50302=ADVANCED_FACE('',(#15215),#818,.F.);
#50303=ADVANCED_FACE('',(#15216),#12818,.F.);
#50304=ADVANCED_FACE('',(#15217),#12819,.F.);
#50305=ADVANCED_FACE('',(#15218),#12820,.F.);
#50306=ADVANCED_FACE('',(#15219),#12821,.F.);
#50307=ADVANCED_FACE('',(#15220),#12822,.F.);
#50308=ADVANCED_FACE('',(#15221),#12823,.F.);
#50309=ADVANCED_FACE('',(#15222),#819,.F.);
#50310=ADVANCED_FACE('',(#15223),#820,.F.);
#50311=ADVANCED_FACE('',(#15224),#821,.F.);
#50312=ADVANCED_FACE('',(#15225),#822,.F.);
#50313=ADVANCED_FACE('',(#15226),#823,.F.);
#50314=ADVANCED_FACE('',(#15227),#824,.F.);
#50315=ADVANCED_FACE('',(#15228),#825,.F.);
#50316=ADVANCED_FACE('',(#15229),#826,.F.);
#50317=ADVANCED_FACE('',(#15230),#12824,.F.);
#50318=ADVANCED_FACE('',(#15231),#827,.F.);
#50319=ADVANCED_FACE('',(#15232),#828,.F.);
#50320=ADVANCED_FACE('',(#15233),#12825,.T.);
#50321=ADVANCED_FACE('',(#15234),#829,.F.);
#50322=ADVANCED_FACE('',(#15235),#830,.F.);
#50323=ADVANCED_FACE('',(#15236),#831,.F.);
#50324=ADVANCED_FACE('',(#15237),#832,.F.);
#50325=ADVANCED_FACE('',(#15238),#833,.F.);
#50326=ADVANCED_FACE('',(#15239),#834,.F.);
#50327=ADVANCED_FACE('',(#15240),#835,.F.);
#50328=ADVANCED_FACE('',(#15241),#836,.F.);
#50329=ADVANCED_FACE('',(#15242),#837,.F.);
#50330=ADVANCED_FACE('',(#15243),#838,.F.);
#50331=ADVANCED_FACE('',(#15244),#839,.F.);
#50332=ADVANCED_FACE('',(#15245),#12826,.T.);
#50333=ADVANCED_FACE('',(#15246),#840,.F.);
#50334=ADVANCED_FACE('',(#15247),#841,.F.);
#50335=ADVANCED_FACE('',(#15248),#842,.F.);
#50336=ADVANCED_FACE('',(#15249),#843,.F.);
#50337=ADVANCED_FACE('',(#15250),#844,.F.);
#50338=ADVANCED_FACE('',(#15251),#845,.F.);
#50339=ADVANCED_FACE('',(#15252),#846,.F.);
#50340=ADVANCED_FACE('',(#15253),#847,.F.);
#50341=ADVANCED_FACE('',(#15254),#848,.F.);
#50342=ADVANCED_FACE('',(#15255),#849,.F.);
#50343=ADVANCED_FACE('',(#15256),#850,.F.);
#50344=ADVANCED_FACE('',(#15257),#12827,.F.);
#50345=ADVANCED_FACE('',(#15258),#851,.F.);
#50346=ADVANCED_FACE('',(#15259),#852,.F.);
#50347=ADVANCED_FACE('',(#15260),#853,.F.);
#50348=ADVANCED_FACE('',(#15261),#12828,.T.);
#50349=ADVANCED_FACE('',(#15262),#12829,.F.);
#50350=ADVANCED_FACE('',(#15263),#12830,.F.);
#50351=ADVANCED_FACE('',(#15264),#12831,.F.);
#50352=ADVANCED_FACE('',(#15265),#12832,.F.);
#50353=ADVANCED_FACE('',(#15266),#12833,.F.);
#50354=ADVANCED_FACE('',(#15267),#12834,.F.);
#50355=ADVANCED_FACE('',(#15268),#12835,.F.);
#50356=ADVANCED_FACE('',(#15269),#12836,.F.);
#50357=ADVANCED_FACE('',(#15270),#12837,.F.);
#50358=ADVANCED_FACE('',(#15271),#12838,.F.);
#50359=ADVANCED_FACE('',(#15272),#12839,.F.);
#50360=ADVANCED_FACE('',(#15273),#12840,.F.);
#50361=ADVANCED_FACE('',(#15274),#12841,.F.);
#50362=ADVANCED_FACE('',(#15275),#12842,.F.);
#50363=ADVANCED_FACE('',(#15276),#12843,.F.);
#50364=ADVANCED_FACE('',(#15277),#12844,.F.);
#50365=ADVANCED_FACE('',(#15278),#12845,.F.);
#50366=ADVANCED_FACE('',(#15279),#12846,.F.);
#50367=ADVANCED_FACE('',(#15280),#854,.F.);
#50368=ADVANCED_FACE('',(#15281),#855,.F.);
#50369=ADVANCED_FACE('',(#15282),#856,.F.);
#50370=ADVANCED_FACE('',(#15283),#857,.F.);
#50371=ADVANCED_FACE('',(#15284),#858,.F.);
#50372=ADVANCED_FACE('',(#15285),#859,.F.);
#50373=ADVANCED_FACE('',(#15286),#860,.F.);
#50374=ADVANCED_FACE('',(#15287),#861,.F.);
#50375=ADVANCED_FACE('',(#15288),#862,.F.);
#50376=ADVANCED_FACE('',(#15289),#863,.F.);
#50377=ADVANCED_FACE('',(#15290),#864,.F.);
#50378=ADVANCED_FACE('',(#15291),#12847,.T.);
#50379=ADVANCED_FACE('',(#15292),#12848,.F.);
#50380=ADVANCED_FACE('',(#15293),#12849,.F.);
#50381=ADVANCED_FACE('',(#15294),#12850,.F.);
#50382=ADVANCED_FACE('',(#15295),#12851,.F.);
#50383=ADVANCED_FACE('',(#15296),#12852,.F.);
#50384=ADVANCED_FACE('',(#15297),#12853,.F.);
#50385=ADVANCED_FACE('',(#15298),#12854,.F.);
#50386=ADVANCED_FACE('',(#15299),#12855,.F.);
#50387=ADVANCED_FACE('',(#15300),#12856,.F.);
#50388=ADVANCED_FACE('',(#15301),#12857,.F.);
#50389=ADVANCED_FACE('',(#15302),#12858,.F.);
#50390=ADVANCED_FACE('',(#15303),#12859,.F.);
#50391=ADVANCED_FACE('',(#15304),#12860,.F.);
#50392=ADVANCED_FACE('',(#15305),#12861,.F.);
#50393=ADVANCED_FACE('',(#15306),#12862,.F.);
#50394=ADVANCED_FACE('',(#15307),#12863,.F.);
#50395=ADVANCED_FACE('',(#15308),#12864,.F.);
#50396=ADVANCED_FACE('',(#15309),#12865,.F.);
#50397=ADVANCED_FACE('',(#15310),#12866,.F.);
#50398=ADVANCED_FACE('',(#15311),#12867,.F.);
#50399=ADVANCED_FACE('',(#15312),#865,.F.);
#50400=ADVANCED_FACE('',(#15313),#866,.F.);
#50401=ADVANCED_FACE('',(#15314),#867,.F.);
#50402=ADVANCED_FACE('',(#15315),#868,.F.);
#50403=ADVANCED_FACE('',(#15316),#869,.F.);
#50404=ADVANCED_FACE('',(#15317),#870,.F.);
#50405=ADVANCED_FACE('',(#15318),#871,.F.);
#50406=ADVANCED_FACE('',(#15319),#872,.F.);
#50407=ADVANCED_FACE('',(#15320),#12868,.F.);
#50408=ADVANCED_FACE('',(#15321),#12869,.F.);
#50409=ADVANCED_FACE('',(#15322),#12870,.F.);
#50410=ADVANCED_FACE('',(#15323),#873,.F.);
#50411=ADVANCED_FACE('',(#15324),#12871,.T.);
#50412=ADVANCED_FACE('',(#15325),#12872,.F.);
#50413=ADVANCED_FACE('',(#15326),#874,.F.);
#50414=ADVANCED_FACE('',(#15327),#875,.F.);
#50415=ADVANCED_FACE('',(#15328),#876,.F.);
#50416=ADVANCED_FACE('',(#15329),#877,.F.);
#50417=ADVANCED_FACE('',(#15330),#12873,.F.);
#50418=ADVANCED_FACE('',(#15331),#12874,.F.);
#50419=ADVANCED_FACE('',(#15332),#12875,.F.);
#50420=ADVANCED_FACE('',(#15333),#878,.F.);
#50421=ADVANCED_FACE('',(#15334),#879,.F.);
#50422=ADVANCED_FACE('',(#15335),#880,.F.);
#50423=ADVANCED_FACE('',(#15336),#881,.F.);
#50424=ADVANCED_FACE('',(#15337),#882,.F.);
#50425=ADVANCED_FACE('',(#15338),#883,.F.);
#50426=ADVANCED_FACE('',(#15339),#884,.F.);
#50427=ADVANCED_FACE('',(#15340),#12876,.F.);
#50428=ADVANCED_FACE('',(#15341),#12877,.F.);
#50429=ADVANCED_FACE('',(#15342),#12878,.F.);
#50430=ADVANCED_FACE('',(#15343),#12879,.F.);
#50431=ADVANCED_FACE('',(#15344),#12880,.T.);
#50432=ADVANCED_FACE('',(#15345),#12881,.F.);
#50433=ADVANCED_FACE('',(#15346),#12882,.F.);
#50434=ADVANCED_FACE('',(#15347),#12883,.F.);
#50435=ADVANCED_FACE('',(#15348),#12884,.F.);
#50436=ADVANCED_FACE('',(#15349,#989,#990,#991,#992,#993,#994,#995,#996,
#997,#998,#999,#1000,#1001,#1002,#1003,#1004,#1005,#1006,#1007,#1008,#1009,
#1010,#1011),#12885,.T.);
#50437=ADVANCED_FACE('',(#15350),#48276,.F.);
#50438=ADVANCED_FACE('',(#15351),#1140,.F.);
#50439=ADVANCED_FACE('',(#15352,#1012,#1013,#1014,#1015,#1016,#1017,#1018,
#1019,#1020,#1021,#1022,#1023),#12886,.T.);
#50440=ADVANCED_FACE('',(#15353),#48277,.F.);
#50441=ADVANCED_FACE('',(#15354,#1024,#1025,#1026,#1027),#12887,.F.);
#50442=ADVANCED_FACE('',(#15355),#48278,.F.);
#50443=ADVANCED_FACE('',(#15356),#1141,.F.);
#50444=ADVANCED_FACE('',(#15357),#48279,.F.);
#50445=ADVANCED_FACE('',(#15358),#48280,.F.);
#50446=ADVANCED_FACE('',(#15359),#1142,.F.);
#50447=ADVANCED_FACE('',(#15360),#48281,.F.);
#50448=ADVANCED_FACE('',(#15361),#48282,.F.);
#50449=ADVANCED_FACE('',(#15362),#1143,.F.);
#50450=ADVANCED_FACE('',(#15363),#48283,.F.);
#50451=ADVANCED_FACE('',(#15364),#48284,.F.);
#50452=ADVANCED_FACE('',(#15365),#1144,.F.);
#50453=ADVANCED_FACE('',(#15366),#48285,.F.);
#50454=ADVANCED_FACE('',(#15367),#1145,.F.);
#50455=ADVANCED_FACE('',(#15368),#48286,.F.);
#50456=ADVANCED_FACE('',(#15369),#48287,.F.);
#50457=ADVANCED_FACE('',(#15370),#1146,.F.);
#50458=ADVANCED_FACE('',(#15371),#48288,.F.);
#50459=ADVANCED_FACE('',(#15372),#48289,.F.);
#50460=ADVANCED_FACE('',(#15373),#1147,.F.);
#50461=ADVANCED_FACE('',(#15374),#48290,.F.);
#50462=ADVANCED_FACE('',(#15375),#48291,.F.);
#50463=ADVANCED_FACE('',(#15376),#1148,.F.);
#50464=ADVANCED_FACE('',(#15377),#48292,.F.);
#50465=ADVANCED_FACE('',(#15378),#48293,.F.);
#50466=ADVANCED_FACE('',(#15379),#1149,.F.);
#50467=ADVANCED_FACE('',(#15380),#1150,.F.);
#50468=ADVANCED_FACE('',(#15381),#12888,.T.);
#50469=ADVANCED_FACE('',(#15382),#48294,.T.);
#50470=ADVANCED_FACE('',(#15383),#12889,.T.);
#50471=ADVANCED_FACE('',(#15384),#48295,.T.);
#50472=ADVANCED_FACE('',(#15385),#12890,.T.);
#50473=ADVANCED_FACE('',(#15386),#48296,.T.);
#50474=ADVANCED_FACE('',(#15387),#12891,.T.);
#50475=ADVANCED_FACE('',(#15388),#48297,.T.);
#50476=ADVANCED_FACE('',(#15389),#12892,.T.);
#50477=ADVANCED_FACE('',(#15390),#12893,.T.);
#50478=ADVANCED_FACE('',(#15391),#1151,.T.);
#50479=ADVANCED_FACE('',(#15392),#12894,.T.);
#50480=ADVANCED_FACE('',(#15393),#1152,.T.);
#50481=ADVANCED_FACE('',(#15394),#12895,.T.);
#50482=ADVANCED_FACE('',(#15395),#48298,.T.);
#50483=ADVANCED_FACE('',(#15396),#12896,.T.);
#50484=ADVANCED_FACE('',(#15397),#48299,.T.);
#50485=ADVANCED_FACE('',(#15398),#12897,.T.);
#50486=ADVANCED_FACE('',(#15399),#48300,.T.);
#50487=ADVANCED_FACE('',(#15400),#12898,.T.);
#50488=ADVANCED_FACE('',(#15401),#48301,.T.);
#50489=ADVANCED_FACE('',(#15402),#1153,.T.);
#50490=ADVANCED_FACE('',(#15403),#12899,.T.);
#50491=ADVANCED_FACE('',(#15404),#1154,.T.);
#50492=ADVANCED_FACE('',(#15405),#12900,.T.);
#50493=ADVANCED_FACE('',(#15406),#1155,.F.);
#50494=ADVANCED_FACE('',(#15407),#48302,.F.);
#50495=ADVANCED_FACE('',(#15408,#1028),#12901,.T.);
#50496=ADVANCED_FACE('',(#15409),#48303,.T.);
#50497=ADVANCED_FACE('',(#15410),#1156,.T.);
#50498=ADVANCED_FACE('',(#15411),#48304,.T.);
#50499=ADVANCED_FACE('',(#15412,#1029),#12902,.T.);
#50500=ADVANCED_FACE('',(#15413),#48305,.F.);
#50501=ADVANCED_FACE('',(#15414),#1157,.T.);
#50502=ADVANCED_FACE('',(#15415),#1158,.T.);
#50503=ADVANCED_FACE('',(#15416),#1159,.T.);
#50504=ADVANCED_FACE('',(#15417),#1160,.T.);
#50505=ADVANCED_FACE('',(#15418),#1161,.T.);
#50506=ADVANCED_FACE('',(#15419),#1162,.T.);
#50507=ADVANCED_FACE('',(#15420),#1163,.T.);
#50508=ADVANCED_FACE('',(#15421),#1164,.T.);
#50509=ADVANCED_FACE('',(#15422),#1165,.T.);
#50510=ADVANCED_FACE('',(#15423),#1166,.T.);
#50511=ADVANCED_FACE('',(#15424),#1167,.T.);
#50512=ADVANCED_FACE('',(#15425),#1168,.T.);
#50513=ADVANCED_FACE('',(#15426),#1169,.T.);
#50514=ADVANCED_FACE('',(#15427),#1170,.T.);
#50515=ADVANCED_FACE('',(#15428),#1171,.T.);
#50516=ADVANCED_FACE('',(#15429),#1172,.T.);
#50517=ADVANCED_FACE('',(#15430),#1173,.T.);
#50518=ADVANCED_FACE('',(#15431),#1174,.T.);
#50519=ADVANCED_FACE('',(#15432),#1175,.T.);
#50520=ADVANCED_FACE('',(#15433),#1176,.T.);
#50521=ADVANCED_FACE('',(#15434),#1177,.T.);
#50522=ADVANCED_FACE('',(#15435),#1178,.T.);
#50523=ADVANCED_FACE('',(#15436),#1179,.T.);
#50524=ADVANCED_FACE('',(#15437),#1180,.T.);
#50525=ADVANCED_FACE('',(#15438),#1181,.T.);
#50526=ADVANCED_FACE('',(#15439),#1182,.T.);
#50527=ADVANCED_FACE('',(#15440),#1183,.T.);
#50528=ADVANCED_FACE('',(#15441),#1184,.T.);
#50529=ADVANCED_FACE('',(#15442),#1185,.T.);
#50530=ADVANCED_FACE('',(#15443),#1186,.T.);
#50531=ADVANCED_FACE('',(#15444),#1187,.T.);
#50532=ADVANCED_FACE('',(#15445),#1188,.T.);
#50533=ADVANCED_FACE('',(#15446),#12903,.F.);
#50534=ADVANCED_FACE('',(#15447),#885,.F.);
#50535=ADVANCED_FACE('',(#15448),#12904,.T.);
#50536=ADVANCED_FACE('',(#15449),#1189,.T.);
#50537=ADVANCED_FACE('',(#15450),#886,.F.);
#50538=ADVANCED_FACE('',(#15451),#955,.F.);
#50539=ADVANCED_FACE('',(#15452),#1190,.T.);
#50540=ADVANCED_FACE('',(#15453,#1030),#12905,.T.);
#50541=ADVANCED_FACE('',(#15454),#12906,.F.);
#50542=ADVANCED_FACE('',(#15455),#12907,.F.);
#50543=ADVANCED_FACE('',(#15456),#12908,.F.);
#50544=ADVANCED_FACE('',(#15457),#12909,.T.);
#50545=ADVANCED_FACE('',(#15458),#12910,.F.);
#50546=ADVANCED_FACE('',(#15459),#12911,.F.);
#50547=ADVANCED_FACE('',(#15460),#12912,.F.);
#50548=ADVANCED_FACE('',(#15461),#12913,.T.);
#50549=ADVANCED_FACE('',(#15462),#12914,.F.);
#50550=ADVANCED_FACE('',(#15463),#12915,.F.);
#50551=ADVANCED_FACE('',(#15464),#12916,.F.);
#50552=ADVANCED_FACE('',(#15465),#12917,.T.);
#50553=ADVANCED_FACE('',(#15466),#12918,.F.);
#50554=ADVANCED_FACE('',(#15467),#12919,.F.);
#50555=ADVANCED_FACE('',(#15468),#12920,.F.);
#50556=ADVANCED_FACE('',(#15469),#12921,.T.);
#50557=ADVANCED_FACE('',(#15470),#12922,.F.);
#50558=ADVANCED_FACE('',(#15471),#12923,.F.);
#50559=ADVANCED_FACE('',(#15472),#12924,.F.);
#50560=ADVANCED_FACE('',(#15473),#12925,.T.);
#50561=ADVANCED_FACE('',(#15474),#12926,.F.);
#50562=ADVANCED_FACE('',(#15475),#12927,.F.);
#50563=ADVANCED_FACE('',(#15476),#12928,.F.);
#50564=ADVANCED_FACE('',(#15477),#12929,.T.);
#50565=ADVANCED_FACE('',(#15478),#12930,.F.);
#50566=ADVANCED_FACE('',(#15479),#12931,.F.);
#50567=ADVANCED_FACE('',(#15480),#12932,.F.);
#50568=ADVANCED_FACE('',(#15481),#12933,.T.);
#50569=ADVANCED_FACE('',(#15482),#12934,.F.);
#50570=ADVANCED_FACE('',(#15483),#12935,.F.);
#50571=ADVANCED_FACE('',(#15484),#12936,.F.);
#50572=ADVANCED_FACE('',(#15485),#12937,.T.);
#50573=ADVANCED_FACE('',(#15486),#12938,.F.);
#50574=ADVANCED_FACE('',(#15487),#12939,.F.);
#50575=ADVANCED_FACE('',(#15488),#12940,.F.);
#50576=ADVANCED_FACE('',(#15489),#12941,.T.);
#50577=ADVANCED_FACE('',(#15490),#12942,.F.);
#50578=ADVANCED_FACE('',(#15491),#12943,.F.);
#50579=ADVANCED_FACE('',(#15492),#12944,.F.);
#50580=ADVANCED_FACE('',(#15493),#12945,.T.);
#50581=ADVANCED_FACE('',(#15494),#12946,.F.);
#50582=ADVANCED_FACE('',(#15495),#12947,.F.);
#50583=ADVANCED_FACE('',(#15496),#12948,.F.);
#50584=ADVANCED_FACE('',(#15497),#12949,.T.);
#50585=ADVANCED_FACE('',(#15498),#12950,.F.);
#50586=ADVANCED_FACE('',(#15499),#12951,.F.);
#50587=ADVANCED_FACE('',(#15500),#12952,.F.);
#50588=ADVANCED_FACE('',(#15501),#12953,.T.);
#50589=ADVANCED_FACE('',(#15502),#12954,.F.);
#50590=ADVANCED_FACE('',(#15503),#12955,.F.);
#50591=ADVANCED_FACE('',(#15504),#12956,.F.);
#50592=ADVANCED_FACE('',(#15505),#12957,.T.);
#50593=ADVANCED_FACE('',(#15506),#12958,.F.);
#50594=ADVANCED_FACE('',(#15507),#12959,.F.);
#50595=ADVANCED_FACE('',(#15508),#12960,.F.);
#50596=ADVANCED_FACE('',(#15509),#12961,.T.);
#50597=ADVANCED_FACE('',(#15510),#12962,.F.);
#50598=ADVANCED_FACE('',(#15511),#12963,.F.);
#50599=ADVANCED_FACE('',(#15512),#12964,.F.);
#50600=ADVANCED_FACE('',(#15513),#12965,.T.);
#50601=ADVANCED_FACE('',(#15514),#12966,.F.);
#50602=ADVANCED_FACE('',(#15515),#12967,.F.);
#50603=ADVANCED_FACE('',(#15516),#12968,.F.);
#50604=ADVANCED_FACE('',(#15517),#12969,.T.);
#50605=ADVANCED_FACE('',(#15518),#12970,.F.);
#50606=ADVANCED_FACE('',(#15519),#12971,.F.);
#50607=ADVANCED_FACE('',(#15520),#12972,.F.);
#50608=ADVANCED_FACE('',(#15521),#12973,.T.);
#50609=ADVANCED_FACE('',(#15522),#12974,.F.);
#50610=ADVANCED_FACE('',(#15523),#12975,.F.);
#50611=ADVANCED_FACE('',(#15524),#12976,.F.);
#50612=ADVANCED_FACE('',(#15525),#12977,.T.);
#50613=ADVANCED_FACE('',(#15526),#12978,.F.);
#50614=ADVANCED_FACE('',(#15527),#12979,.F.);
#50615=ADVANCED_FACE('',(#15528),#12980,.F.);
#50616=ADVANCED_FACE('',(#15529),#12981,.T.);
#50617=ADVANCED_FACE('',(#15530),#12982,.F.);
#50618=ADVANCED_FACE('',(#15531),#12983,.F.);
#50619=ADVANCED_FACE('',(#15532),#12984,.F.);
#50620=ADVANCED_FACE('',(#15533),#12985,.T.);
#50621=ADVANCED_FACE('',(#15534),#12986,.F.);
#50622=ADVANCED_FACE('',(#15535),#12987,.F.);
#50623=ADVANCED_FACE('',(#15536),#12988,.F.);
#50624=ADVANCED_FACE('',(#15537),#12989,.T.);
#50625=ADVANCED_FACE('',(#15538),#12990,.F.);
#50626=ADVANCED_FACE('',(#15539),#12991,.F.);
#50627=ADVANCED_FACE('',(#15540),#12992,.F.);
#50628=ADVANCED_FACE('',(#15541),#12993,.T.);
#50629=ADVANCED_FACE('',(#15542),#12994,.F.);
#50630=ADVANCED_FACE('',(#15543),#12995,.F.);
#50631=ADVANCED_FACE('',(#15544),#12996,.F.);
#50632=ADVANCED_FACE('',(#15545),#12997,.T.);
#50633=ADVANCED_FACE('',(#15546),#12998,.F.);
#50634=ADVANCED_FACE('',(#15547),#12999,.F.);
#50635=ADVANCED_FACE('',(#15548),#13000,.F.);
#50636=ADVANCED_FACE('',(#15549),#13001,.T.);
#50637=ADVANCED_FACE('',(#15550),#13002,.F.);
#50638=ADVANCED_FACE('',(#15551),#13003,.F.);
#50639=ADVANCED_FACE('',(#15552),#13004,.F.);
#50640=ADVANCED_FACE('',(#15553),#13005,.T.);
#50641=ADVANCED_FACE('',(#15554),#13006,.F.);
#50642=ADVANCED_FACE('',(#15555),#13007,.F.);
#50643=ADVANCED_FACE('',(#15556),#13008,.F.);
#50644=ADVANCED_FACE('',(#15557),#13009,.T.);
#50645=ADVANCED_FACE('',(#15558),#13010,.F.);
#50646=ADVANCED_FACE('',(#15559),#13011,.F.);
#50647=ADVANCED_FACE('',(#15560),#13012,.F.);
#50648=ADVANCED_FACE('',(#15561),#13013,.T.);
#50649=ADVANCED_FACE('',(#15562),#13014,.F.);
#50650=ADVANCED_FACE('',(#15563),#13015,.F.);
#50651=ADVANCED_FACE('',(#15564),#13016,.F.);
#50652=ADVANCED_FACE('',(#15565),#13017,.T.);
#50653=ADVANCED_FACE('',(#15566),#13018,.F.);
#50654=ADVANCED_FACE('',(#15567),#13019,.F.);
#50655=ADVANCED_FACE('',(#15568),#13020,.F.);
#50656=ADVANCED_FACE('',(#15569),#13021,.T.);
#50657=ADVANCED_FACE('',(#15570),#13022,.F.);
#50658=ADVANCED_FACE('',(#15571),#13023,.F.);
#50659=ADVANCED_FACE('',(#15572),#13024,.F.);
#50660=ADVANCED_FACE('',(#15573),#13025,.T.);
#50661=ADVANCED_FACE('',(#15574),#13026,.F.);
#50662=ADVANCED_FACE('',(#15575),#13027,.F.);
#50663=ADVANCED_FACE('',(#15576),#13028,.F.);
#50664=ADVANCED_FACE('',(#15577),#13029,.T.);
#50665=ADVANCED_FACE('',(#15578),#13030,.F.);
#50666=ADVANCED_FACE('',(#15579),#13031,.F.);
#50667=ADVANCED_FACE('',(#15580),#13032,.F.);
#50668=ADVANCED_FACE('',(#15581),#13033,.T.);
#50669=ADVANCED_FACE('',(#15582),#13034,.F.);
#50670=ADVANCED_FACE('',(#15583),#13035,.F.);
#50671=ADVANCED_FACE('',(#15584),#13036,.F.);
#50672=ADVANCED_FACE('',(#15585),#13037,.T.);
#50673=ADVANCED_FACE('',(#15586),#13038,.F.);
#50674=ADVANCED_FACE('',(#15587),#13039,.F.);
#50675=ADVANCED_FACE('',(#15588),#13040,.F.);
#50676=ADVANCED_FACE('',(#15589),#13041,.T.);
#50677=ADVANCED_FACE('',(#15590),#13042,.F.);
#50678=ADVANCED_FACE('',(#15591),#13043,.F.);
#50679=ADVANCED_FACE('',(#15592),#13044,.F.);
#50680=ADVANCED_FACE('',(#15593),#13045,.T.);
#50681=ADVANCED_FACE('',(#15594),#13046,.F.);
#50682=ADVANCED_FACE('',(#15595),#13047,.F.);
#50683=ADVANCED_FACE('',(#15596),#13048,.F.);
#50684=ADVANCED_FACE('',(#15597),#13049,.T.);
#50685=ADVANCED_FACE('',(#15598),#48306,.F.);
#50686=ADVANCED_FACE('',(#15599),#13050,.F.);
#50687=ADVANCED_FACE('',(#15600),#13051,.F.);
#50688=ADVANCED_FACE('',(#15601),#13052,.F.);
#50689=ADVANCED_FACE('',(#15602),#13053,.F.);
#50690=ADVANCED_FACE('',(#15603),#13054,.F.);
#50691=ADVANCED_FACE('',(#15604),#13055,.F.);
#50692=ADVANCED_FACE('',(#15605,#1031),#13056,.T.);
#50693=ADVANCED_FACE('',(#15606),#13057,.T.);
#50694=ADVANCED_FACE('',(#15607),#48307,.T.);
#50695=ADVANCED_FACE('',(#15608),#1191,.T.);
#50696=ADVANCED_FACE('',(#15609),#48308,.T.);
#50697=ADVANCED_FACE('',(#15610,#1032),#13058,.T.);
#50698=ADVANCED_FACE('',(#15611),#48309,.T.);
#50699=ADVANCED_FACE('',(#15612),#1192,.T.);
#50700=ADVANCED_FACE('',(#15613),#48310,.T.);
#50701=ADVANCED_FACE('',(#15614,#1033),#13059,.T.);
#50702=ADVANCED_FACE('',(#15615),#48311,.F.);
#50703=ADVANCED_FACE('',(#15616),#1193,.F.);
#50704=ADVANCED_FACE('',(#15617),#48312,.F.);
#50705=ADVANCED_FACE('',(#15618,#1034),#13060,.T.);
#50706=ADVANCED_FACE('',(#15619),#1194,.F.);
#50707=ADVANCED_FACE('',(#15620),#1195,.T.);
#50708=ADVANCED_FACE('',(#15621),#13061,.F.);
#50709=ADVANCED_FACE('',(#15622),#13062,.F.);
#50710=ADVANCED_FACE('',(#15623),#48313,.T.);
#50711=ADVANCED_FACE('',(#15624),#1196,.T.);
#50712=ADVANCED_FACE('',(#15625),#48314,.T.);
#50713=ADVANCED_FACE('',(#15626),#13063,.T.);
#50714=ADVANCED_FACE('',(#15627),#48315,.F.);
#50715=ADVANCED_FACE('',(#15628),#1197,.F.);
#50716=ADVANCED_FACE('',(#15629),#48316,.F.);
#50717=ADVANCED_FACE('',(#15630),#13064,.T.);
#50718=ADVANCED_FACE('',(#15631),#1198,.T.);
#50719=ADVANCED_FACE('',(#15632),#1199,.T.);
#50720=ADVANCED_FACE('',(#15633),#1200,.T.);
#50721=ADVANCED_FACE('',(#15634),#1201,.T.);
#50722=ADVANCED_FACE('',(#15635),#1202,.T.);
#50723=ADVANCED_FACE('',(#15636),#1203,.T.);
#50724=ADVANCED_FACE('',(#15637),#1204,.T.);
#50725=ADVANCED_FACE('',(#15638),#1205,.T.);
#50726=ADVANCED_FACE('',(#15639),#1206,.T.);
#50727=ADVANCED_FACE('',(#15640),#1207,.T.);
#50728=ADVANCED_FACE('',(#15641),#1208,.T.);
#50729=ADVANCED_FACE('',(#15642),#1209,.T.);
#50730=ADVANCED_FACE('',(#15643),#1210,.T.);
#50731=ADVANCED_FACE('',(#15644),#1211,.T.);
#50732=ADVANCED_FACE('',(#15645),#1212,.T.);
#50733=ADVANCED_FACE('',(#15646),#1213,.T.);
#50734=ADVANCED_FACE('',(#15647),#1214,.T.);
#50735=ADVANCED_FACE('',(#15648),#1215,.T.);
#50736=ADVANCED_FACE('',(#15649),#1216,.T.);
#50737=ADVANCED_FACE('',(#15650),#1217,.T.);
#50738=ADVANCED_FACE('',(#15651),#1218,.T.);
#50739=ADVANCED_FACE('',(#15652),#1219,.T.);
#50740=ADVANCED_FACE('',(#15653),#1220,.T.);
#50741=ADVANCED_FACE('',(#15654),#1221,.T.);
#50742=ADVANCED_FACE('',(#15655),#1222,.T.);
#50743=ADVANCED_FACE('',(#15656),#1223,.T.);
#50744=ADVANCED_FACE('',(#15657),#1224,.T.);
#50745=ADVANCED_FACE('',(#15658),#1225,.T.);
#50746=ADVANCED_FACE('',(#15659),#1226,.T.);
#50747=ADVANCED_FACE('',(#15660),#1227,.T.);
#50748=ADVANCED_FACE('',(#15661),#1228,.T.);
#50749=ADVANCED_FACE('',(#15662),#13065,.F.);
#50750=ADVANCED_FACE('',(#15663),#887,.F.);
#50751=ADVANCED_FACE('',(#15664),#13066,.T.);
#50752=ADVANCED_FACE('',(#15665),#1229,.T.);
#50753=ADVANCED_FACE('',(#15666),#888,.F.);
#50754=ADVANCED_FACE('',(#15667),#956,.F.);
#50755=ADVANCED_FACE('',(#15668),#1230,.T.);
#50756=ADVANCED_FACE('',(#15669,#1035),#13067,.T.);
#50757=ADVANCED_FACE('',(#15670),#13068,.F.);
#50758=ADVANCED_FACE('',(#15671),#13069,.F.);
#50759=ADVANCED_FACE('',(#15672),#13070,.F.);
#50760=ADVANCED_FACE('',(#15673),#13071,.T.);
#50761=ADVANCED_FACE('',(#15674),#13072,.F.);
#50762=ADVANCED_FACE('',(#15675),#13073,.F.);
#50763=ADVANCED_FACE('',(#15676),#13074,.F.);
#50764=ADVANCED_FACE('',(#15677),#13075,.T.);
#50765=ADVANCED_FACE('',(#15678),#13076,.F.);
#50766=ADVANCED_FACE('',(#15679),#13077,.F.);
#50767=ADVANCED_FACE('',(#15680),#13078,.F.);
#50768=ADVANCED_FACE('',(#15681),#13079,.T.);
#50769=ADVANCED_FACE('',(#15682),#13080,.F.);
#50770=ADVANCED_FACE('',(#15683),#13081,.F.);
#50771=ADVANCED_FACE('',(#15684),#13082,.F.);
#50772=ADVANCED_FACE('',(#15685),#13083,.T.);
#50773=ADVANCED_FACE('',(#15686),#13084,.F.);
#50774=ADVANCED_FACE('',(#15687),#13085,.F.);
#50775=ADVANCED_FACE('',(#15688),#13086,.F.);
#50776=ADVANCED_FACE('',(#15689),#13087,.T.);
#50777=ADVANCED_FACE('',(#15690),#13088,.F.);
#50778=ADVANCED_FACE('',(#15691),#13089,.F.);
#50779=ADVANCED_FACE('',(#15692),#13090,.F.);
#50780=ADVANCED_FACE('',(#15693),#13091,.T.);
#50781=ADVANCED_FACE('',(#15694),#13092,.F.);
#50782=ADVANCED_FACE('',(#15695),#13093,.F.);
#50783=ADVANCED_FACE('',(#15696),#13094,.F.);
#50784=ADVANCED_FACE('',(#15697),#13095,.T.);
#50785=ADVANCED_FACE('',(#15698),#13096,.F.);
#50786=ADVANCED_FACE('',(#15699),#13097,.F.);
#50787=ADVANCED_FACE('',(#15700),#13098,.F.);
#50788=ADVANCED_FACE('',(#15701),#13099,.T.);
#50789=ADVANCED_FACE('',(#15702),#13100,.F.);
#50790=ADVANCED_FACE('',(#15703),#13101,.F.);
#50791=ADVANCED_FACE('',(#15704),#13102,.F.);
#50792=ADVANCED_FACE('',(#15705),#13103,.T.);
#50793=ADVANCED_FACE('',(#15706),#13104,.F.);
#50794=ADVANCED_FACE('',(#15707),#13105,.F.);
#50795=ADVANCED_FACE('',(#15708),#13106,.F.);
#50796=ADVANCED_FACE('',(#15709),#13107,.T.);
#50797=ADVANCED_FACE('',(#15710),#13108,.F.);
#50798=ADVANCED_FACE('',(#15711),#13109,.F.);
#50799=ADVANCED_FACE('',(#15712),#13110,.F.);
#50800=ADVANCED_FACE('',(#15713),#13111,.T.);
#50801=ADVANCED_FACE('',(#15714),#13112,.F.);
#50802=ADVANCED_FACE('',(#15715),#13113,.F.);
#50803=ADVANCED_FACE('',(#15716),#13114,.F.);
#50804=ADVANCED_FACE('',(#15717),#13115,.T.);
#50805=ADVANCED_FACE('',(#15718),#13116,.F.);
#50806=ADVANCED_FACE('',(#15719),#13117,.F.);
#50807=ADVANCED_FACE('',(#15720),#13118,.F.);
#50808=ADVANCED_FACE('',(#15721),#13119,.T.);
#50809=ADVANCED_FACE('',(#15722),#13120,.F.);
#50810=ADVANCED_FACE('',(#15723),#13121,.F.);
#50811=ADVANCED_FACE('',(#15724),#13122,.F.);
#50812=ADVANCED_FACE('',(#15725),#13123,.T.);
#50813=ADVANCED_FACE('',(#15726),#13124,.F.);
#50814=ADVANCED_FACE('',(#15727),#13125,.F.);
#50815=ADVANCED_FACE('',(#15728),#13126,.F.);
#50816=ADVANCED_FACE('',(#15729),#13127,.T.);
#50817=ADVANCED_FACE('',(#15730),#13128,.F.);
#50818=ADVANCED_FACE('',(#15731),#13129,.F.);
#50819=ADVANCED_FACE('',(#15732),#13130,.F.);
#50820=ADVANCED_FACE('',(#15733),#13131,.T.);
#50821=ADVANCED_FACE('',(#15734),#13132,.F.);
#50822=ADVANCED_FACE('',(#15735),#13133,.F.);
#50823=ADVANCED_FACE('',(#15736),#13134,.F.);
#50824=ADVANCED_FACE('',(#15737),#13135,.T.);
#50825=ADVANCED_FACE('',(#15738),#13136,.F.);
#50826=ADVANCED_FACE('',(#15739),#13137,.F.);
#50827=ADVANCED_FACE('',(#15740),#13138,.F.);
#50828=ADVANCED_FACE('',(#15741),#13139,.T.);
#50829=ADVANCED_FACE('',(#15742),#13140,.F.);
#50830=ADVANCED_FACE('',(#15743),#13141,.F.);
#50831=ADVANCED_FACE('',(#15744),#13142,.F.);
#50832=ADVANCED_FACE('',(#15745),#13143,.T.);
#50833=ADVANCED_FACE('',(#15746),#13144,.F.);
#50834=ADVANCED_FACE('',(#15747),#13145,.F.);
#50835=ADVANCED_FACE('',(#15748),#13146,.F.);
#50836=ADVANCED_FACE('',(#15749),#13147,.T.);
#50837=ADVANCED_FACE('',(#15750),#13148,.F.);
#50838=ADVANCED_FACE('',(#15751),#13149,.F.);
#50839=ADVANCED_FACE('',(#15752),#13150,.F.);
#50840=ADVANCED_FACE('',(#15753),#13151,.T.);
#50841=ADVANCED_FACE('',(#15754),#13152,.F.);
#50842=ADVANCED_FACE('',(#15755),#13153,.F.);
#50843=ADVANCED_FACE('',(#15756),#13154,.F.);
#50844=ADVANCED_FACE('',(#15757),#13155,.T.);
#50845=ADVANCED_FACE('',(#15758),#13156,.F.);
#50846=ADVANCED_FACE('',(#15759),#13157,.F.);
#50847=ADVANCED_FACE('',(#15760),#13158,.F.);
#50848=ADVANCED_FACE('',(#15761),#13159,.T.);
#50849=ADVANCED_FACE('',(#15762),#13160,.F.);
#50850=ADVANCED_FACE('',(#15763),#13161,.F.);
#50851=ADVANCED_FACE('',(#15764),#13162,.F.);
#50852=ADVANCED_FACE('',(#15765),#13163,.T.);
#50853=ADVANCED_FACE('',(#15766),#13164,.F.);
#50854=ADVANCED_FACE('',(#15767),#13165,.F.);
#50855=ADVANCED_FACE('',(#15768),#13166,.F.);
#50856=ADVANCED_FACE('',(#15769),#13167,.T.);
#50857=ADVANCED_FACE('',(#15770),#13168,.F.);
#50858=ADVANCED_FACE('',(#15771),#13169,.F.);
#50859=ADVANCED_FACE('',(#15772),#13170,.F.);
#50860=ADVANCED_FACE('',(#15773),#13171,.T.);
#50861=ADVANCED_FACE('',(#15774),#13172,.F.);
#50862=ADVANCED_FACE('',(#15775),#13173,.F.);
#50863=ADVANCED_FACE('',(#15776),#13174,.F.);
#50864=ADVANCED_FACE('',(#15777),#13175,.T.);
#50865=ADVANCED_FACE('',(#15778),#13176,.F.);
#50866=ADVANCED_FACE('',(#15779),#13177,.F.);
#50867=ADVANCED_FACE('',(#15780),#13178,.F.);
#50868=ADVANCED_FACE('',(#15781),#13179,.T.);
#50869=ADVANCED_FACE('',(#15782),#13180,.F.);
#50870=ADVANCED_FACE('',(#15783),#13181,.F.);
#50871=ADVANCED_FACE('',(#15784),#13182,.F.);
#50872=ADVANCED_FACE('',(#15785),#13183,.T.);
#50873=ADVANCED_FACE('',(#15786),#13184,.F.);
#50874=ADVANCED_FACE('',(#15787),#13185,.F.);
#50875=ADVANCED_FACE('',(#15788),#13186,.F.);
#50876=ADVANCED_FACE('',(#15789),#13187,.T.);
#50877=ADVANCED_FACE('',(#15790),#13188,.F.);
#50878=ADVANCED_FACE('',(#15791),#13189,.F.);
#50879=ADVANCED_FACE('',(#15792),#13190,.F.);
#50880=ADVANCED_FACE('',(#15793),#13191,.T.);
#50881=ADVANCED_FACE('',(#15794),#13192,.F.);
#50882=ADVANCED_FACE('',(#15795),#13193,.F.);
#50883=ADVANCED_FACE('',(#15796),#13194,.F.);
#50884=ADVANCED_FACE('',(#15797),#13195,.T.);
#50885=ADVANCED_FACE('',(#15798),#13196,.F.);
#50886=ADVANCED_FACE('',(#15799),#13197,.F.);
#50887=ADVANCED_FACE('',(#15800),#13198,.F.);
#50888=ADVANCED_FACE('',(#15801),#13199,.T.);
#50889=ADVANCED_FACE('',(#15802),#13200,.F.);
#50890=ADVANCED_FACE('',(#15803),#13201,.F.);
#50891=ADVANCED_FACE('',(#15804),#13202,.F.);
#50892=ADVANCED_FACE('',(#15805),#13203,.T.);
#50893=ADVANCED_FACE('',(#15806),#13204,.F.);
#50894=ADVANCED_FACE('',(#15807),#13205,.F.);
#50895=ADVANCED_FACE('',(#15808),#13206,.F.);
#50896=ADVANCED_FACE('',(#15809),#13207,.T.);
#50897=ADVANCED_FACE('',(#15810),#13208,.F.);
#50898=ADVANCED_FACE('',(#15811),#13209,.F.);
#50899=ADVANCED_FACE('',(#15812),#13210,.F.);
#50900=ADVANCED_FACE('',(#15813),#13211,.T.);
#50901=ADVANCED_FACE('',(#15814),#48317,.F.);
#50902=ADVANCED_FACE('',(#15815),#13212,.F.);
#50903=ADVANCED_FACE('',(#15816),#13213,.F.);
#50904=ADVANCED_FACE('',(#15817),#13214,.F.);
#50905=ADVANCED_FACE('',(#15818),#13215,.F.);
#50906=ADVANCED_FACE('',(#15819),#13216,.F.);
#50907=ADVANCED_FACE('',(#15820),#13217,.F.);
#50908=ADVANCED_FACE('',(#15821,#1036),#13218,.T.);
#50909=ADVANCED_FACE('',(#15822),#13219,.T.);
#50910=ADVANCED_FACE('',(#15823),#48318,.T.);
#50911=ADVANCED_FACE('',(#15824),#1231,.T.);
#50912=ADVANCED_FACE('',(#15825),#48319,.T.);
#50913=ADVANCED_FACE('',(#15826,#1037),#13220,.T.);
#50914=ADVANCED_FACE('',(#15827),#957,.T.);
#50915=ADVANCED_FACE('',(#15828),#48320,.T.);
#50916=ADVANCED_FACE('',(#15829),#13221,.T.);
#50917=ADVANCED_FACE('',(#15830),#13222,.T.);
#50918=ADVANCED_FACE('',(#15831),#48321,.T.);
#50919=ADVANCED_FACE('',(#15832),#1232,.T.);
#50920=ADVANCED_FACE('',(#15833),#1233,.T.);
#50921=ADVANCED_FACE('',(#15834),#1234,.T.);
#50922=ADVANCED_FACE('',(#15835),#1235,.T.);
#50923=ADVANCED_FACE('',(#15836),#1236,.T.);
#50924=ADVANCED_FACE('',(#15837),#1237,.T.);
#50925=ADVANCED_FACE('',(#15838),#1238,.T.);
#50926=ADVANCED_FACE('',(#15839),#1239,.T.);
#50927=ADVANCED_FACE('',(#15840),#1240,.T.);
#50928=ADVANCED_FACE('',(#15841),#1241,.T.);
#50929=ADVANCED_FACE('',(#15842),#1242,.T.);
#50930=ADVANCED_FACE('',(#15843),#1243,.T.);
#50931=ADVANCED_FACE('',(#15844),#1244,.T.);
#50932=ADVANCED_FACE('',(#15845),#1245,.T.);
#50933=ADVANCED_FACE('',(#15846),#1246,.T.);
#50934=ADVANCED_FACE('',(#15847),#1247,.T.);
#50935=ADVANCED_FACE('',(#15848),#1248,.T.);
#50936=ADVANCED_FACE('',(#15849),#1249,.T.);
#50937=ADVANCED_FACE('',(#15850),#1250,.T.);
#50938=ADVANCED_FACE('',(#15851),#1251,.T.);
#50939=ADVANCED_FACE('',(#15852),#1252,.T.);
#50940=ADVANCED_FACE('',(#15853),#1253,.T.);
#50941=ADVANCED_FACE('',(#15854),#1254,.T.);
#50942=ADVANCED_FACE('',(#15855),#1255,.T.);
#50943=ADVANCED_FACE('',(#15856),#1256,.T.);
#50944=ADVANCED_FACE('',(#15857),#1257,.T.);
#50945=ADVANCED_FACE('',(#15858),#1258,.T.);
#50946=ADVANCED_FACE('',(#15859),#1259,.T.);
#50947=ADVANCED_FACE('',(#15860),#1260,.T.);
#50948=ADVANCED_FACE('',(#15861),#1261,.T.);
#50949=ADVANCED_FACE('',(#15862),#1262,.T.);
#50950=ADVANCED_FACE('',(#15863),#1263,.T.);
#50951=ADVANCED_FACE('',(#15864),#1264,.T.);
#50952=ADVANCED_FACE('',(#15865),#1265,.T.);
#50953=ADVANCED_FACE('',(#15866),#1266,.T.);
#50954=ADVANCED_FACE('',(#15867),#1267,.T.);
#50955=ADVANCED_FACE('',(#15868),#1268,.T.);
#50956=ADVANCED_FACE('',(#15869),#1269,.T.);
#50957=ADVANCED_FACE('',(#15870),#1270,.T.);
#50958=ADVANCED_FACE('',(#15871),#1271,.T.);
#50959=ADVANCED_FACE('',(#15872),#1272,.T.);
#50960=ADVANCED_FACE('',(#15873),#1273,.T.);
#50961=ADVANCED_FACE('',(#15874),#1274,.T.);
#50962=ADVANCED_FACE('',(#15875),#1275,.T.);
#50963=ADVANCED_FACE('',(#15876),#1276,.T.);
#50964=ADVANCED_FACE('',(#15877),#1277,.T.);
#50965=ADVANCED_FACE('',(#15878),#1278,.T.);
#50966=ADVANCED_FACE('',(#15879),#13223,.F.);
#50967=ADVANCED_FACE('',(#15880),#889,.F.);
#50968=ADVANCED_FACE('',(#15881),#13224,.T.);
#50969=ADVANCED_FACE('',(#15882),#1279,.T.);
#50970=ADVANCED_FACE('',(#15883),#890,.F.);
#50971=ADVANCED_FACE('',(#15884),#958,.F.);
#50972=ADVANCED_FACE('',(#15885),#1280,.T.);
#50973=ADVANCED_FACE('',(#15886,#1038),#13225,.T.);
#50974=ADVANCED_FACE('',(#15887),#48322,.T.);
#50975=ADVANCED_FACE('',(#15888),#13226,.T.);
#50976=ADVANCED_FACE('',(#15889),#13227,.T.);
#50977=ADVANCED_FACE('',(#15890),#13228,.T.);
#50978=ADVANCED_FACE('',(#15891),#1281,.T.);
#50979=ADVANCED_FACE('',(#15892),#13229,.T.);
#50980=ADVANCED_FACE('',(#15893),#48323,.T.);
#50981=ADVANCED_FACE('',(#15894),#13230,.T.);
#50982=ADVANCED_FACE('',(#15895),#13231,.T.);
#50983=ADVANCED_FACE('',(#15896),#13232,.T.);
#50984=ADVANCED_FACE('',(#15897),#13233,.T.);
#50985=ADVANCED_FACE('',(#15898,#1039),#13234,.F.);
#50986=ADVANCED_FACE('',(#15899),#48324,.T.);
#50987=ADVANCED_FACE('',(#15900),#1282,.T.);
#50988=ADVANCED_FACE('',(#15901),#48325,.T.);
#50989=ADVANCED_FACE('',(#15902,#1040),#13235,.T.);
#50990=ADVANCED_FACE('',(#15903),#48326,.F.);
#50991=ADVANCED_FACE('',(#15904),#1283,.F.);
#50992=ADVANCED_FACE('',(#15905),#48327,.F.);
#50993=ADVANCED_FACE('',(#15906,#1041),#13236,.T.);
#50994=ADVANCED_FACE('',(#15907),#1284,.T.);
#50995=ADVANCED_FACE('',(#15908),#13237,.F.);
#50996=ADVANCED_FACE('',(#15909),#13238,.F.);
#50997=ADVANCED_FACE('',(#15910),#48328,.T.);
#50998=ADVANCED_FACE('',(#15911),#1285,.T.);
#50999=ADVANCED_FACE('',(#15912),#48329,.T.);
#51000=ADVANCED_FACE('',(#15913),#13239,.T.);
#51001=ADVANCED_FACE('',(#15914),#48330,.F.);
#51002=ADVANCED_FACE('',(#15915),#1286,.F.);
#51003=ADVANCED_FACE('',(#15916),#48331,.F.);
#51004=ADVANCED_FACE('',(#15917),#13240,.T.);
#51005=ADVANCED_FACE('',(#15918),#48332,.F.);
#51006=ADVANCED_FACE('',(#15919),#1287,.F.);
#51007=ADVANCED_FACE('',(#15920),#48333,.F.);
#51008=ADVANCED_FACE('',(#15921),#48334,.T.);
#51009=ADVANCED_FACE('',(#15922),#13241,.T.);
#51010=ADVANCED_FACE('',(#15923),#13242,.T.);
#51011=ADVANCED_FACE('',(#15924),#13243,.T.);
#51012=ADVANCED_FACE('',(#15925),#48335,.T.);
#51013=ADVANCED_FACE('',(#15926),#13244,.T.);
#51014=ADVANCED_FACE('',(#15927),#13245,.T.);
#51015=ADVANCED_FACE('',(#15928),#13246,.T.);
#51016=ADVANCED_FACE('',(#15929,#1042),#13247,.T.);
#51017=ADVANCED_FACE('',(#15930,#1043),#13248,.F.);
#51018=CLOSED_SHELL('',(#48336,#48337,#48338,#48339,#48340,#48341,#48342,
#48343,#48344,#48345,#48346,#48347,#48348,#48349,#48350,#48351,#48352,#48353,
#48354,#48355,#48356,#48357,#48358,#48359,#48360,#48361,#48362,#48363,#48364,
#48365,#48366,#48367,#48368,#48369,#48370,#48371,#48372,#48373,#48374,#48375,
#48376,#48377,#48378,#48379,#48380,#48381,#48382,#48383,#48384,#48385,#48386,
#48387,#48388,#48389,#48390,#48391,#48392,#48393,#48394,#48395,#48396,#48397,
#48398,#48399,#48400,#48401,#48402,#48403,#48404,#48405,#48406,#48407,#48408,
#48409,#48410,#48411,#48412,#48413,#48414,#48415,#48416,#48417,#48418,#48419,
#48420,#48421,#48422,#48423,#48424,#48425,#48426,#48427,#48428,#48429,#48430,
#48431,#48432,#48433,#48434,#48435,#48436,#48437,#48438,#48439,#48440,#48441,
#48442,#48443,#48444,#48445,#48446,#48447,#48448,#48449,#48450,#48451,#48452,
#48453,#48454,#48455,#48456,#48457,#48458,#48459,#48460,#48461,#48462,#48463,
#48464,#48465,#48466,#48467,#48468,#48469,#48470,#48471,#48472,#48473,#48474,
#48475,#48476,#48477,#48478,#48479,#48480,#48481,#48482,#48483,#48484,#48485,
#48486,#48487,#48488,#48489,#48490,#48491,#48492,#48493,#48494,#48495,#48496,
#48497,#48498,#48499,#48500,#48501,#48502,#48503,#48504,#48505,#48506,#48507,
#48508,#48509,#48510,#48511,#48512,#48513,#48514,#48515,#48516,#48517,#48518,
#48519,#48520,#48521,#48522,#48523,#48524,#48525,#48526,#48527,#48528,#48529,
#48530,#48531,#48532,#48533,#48534,#48535,#48536,#48537,#48538,#48539,#48540,
#48541,#48542,#48543,#48544,#48545,#48546,#48547,#48548,#48549,#48550,#48551,
#48552,#48553,#48554,#48555,#48556,#48557,#48558,#48559,#48560,#48561,#48562,
#48563,#48564,#48565,#48566,#48567,#48568,#48569,#48570,#48571,#48572,#48573,
#48574,#48575,#48576,#48577,#48578,#48579,#48580,#48581,#48582,#48583,#48584,
#48585,#48586,#48587,#48588,#48589,#48590,#48591,#48592,#48593,#48594,#48595,
#48596,#48597,#48598,#48599,#48600,#48601,#48602,#48603,#48604,#48605,#48606,
#48607,#48608,#48609,#48610,#48611,#48612,#48613,#48614,#48615,#48616,#48617,
#48618,#48619,#48620,#48621,#48622,#48623,#48624,#48625,#48626,#48627,#48628,
#48629,#48630,#48631,#48632,#48633,#48634,#48635,#48636,#48637,#48638,#48639,
#48640,#48641,#48642,#48643,#48644,#48645,#48646,#48647,#48648,#48649,#48650,
#48651,#48652,#48653,#48654,#48655,#48656,#48657,#48658,#48659,#48660,#48661,
#48662,#48663,#48664,#48665,#48666,#48667,#48668,#48669,#48670,#48671,#48672,
#48673,#48674,#48675,#48676,#48677,#48678,#48679,#48680,#48681,#48682,#48683,
#48684,#48685,#48686,#48687,#48688,#48689,#48690,#48691,#48692,#48693,#48694,
#48695,#48696,#48697,#48698,#48699,#48700,#48701,#48702,#48703,#48704,#48705,
#48706,#48707,#48708,#48709,#48710,#48711,#48712,#48713,#48714,#48715,#48716,
#48717,#48718,#48719,#48720,#48721,#48722,#48723,#48724,#48725,#48726,#48727,
#48728,#48729,#48730,#48731,#48732,#48733,#48734,#48735,#48736,#48737,#48738,
#48739,#48740,#48741,#48742,#48743,#48744,#48745,#48746,#48747,#48748,#48749,
#48750,#48751,#48752,#48753,#48754,#48755,#48756,#48757,#48758,#48759,#48760,
#48761,#48762,#48763,#48764,#48765,#48766,#48767,#48768,#48769,#48770,#48771,
#48772,#48773,#48774,#48775,#48776,#48777,#48778,#48779,#48780,#48781,#48782,
#48783,#48784,#48785,#48786,#48787,#48788,#48789,#48790,#48791,#48792,#48793,
#48794,#48795,#48796,#48797,#48798,#48799,#48800,#48801,#48802,#48803,#48804,
#48805,#48806,#48807,#48808,#48809,#48810,#48811,#48812,#48813,#48814,#48815,
#48816,#48817,#48818,#48819,#48820,#48821,#48822,#48823,#48824,#48825,#48826,
#48827,#48828,#48829,#48830,#48831,#48832,#48833,#48834,#48835,#48836,#48837,
#48838,#48839,#48840,#48841,#48842,#48843,#48844,#48845,#48846,#48847,#48848,
#48849,#48850,#48851,#48852,#48853,#48854,#48855,#48856,#48857,#48858,#48859,
#48860,#48861,#48862,#48863,#48864,#48865,#48866,#48867,#48868,#48869,#48870,
#48871,#48872,#48873,#48874,#48875,#48876,#48877,#48878,#48879,#48880,#48881,
#48882,#48883,#48884,#48885,#48886,#48887,#48888,#48889,#48890,#48891,#48892,
#48893,#48894,#48895,#48896,#48897,#48898,#48899,#48900,#48901,#48902,#48903,
#48904,#48905,#48906,#48907,#48908,#48909,#48910,#48911,#48912,#48913,#48914,
#48915,#48916,#48917,#48918,#48919,#48920,#48921,#48922,#48923,#48924,#48925,
#48926,#48927,#48928,#48929,#48930,#48931,#48932,#48933,#48934,#48935,#48936,
#48937,#48938,#48939,#48940,#48941,#48942,#48943,#48944,#48945,#48946,#48947,
#48948,#48949,#48950,#48951,#48952,#48953,#48954,#48955,#48956,#48957,#48958,
#48959,#48960,#48961,#48962,#48963,#48964,#48965,#48966,#48967,#48968,#48969,
#48970,#48971,#48972,#48973,#48974,#48975,#48976,#48977,#48978,#48979,#48980,
#48981,#48982,#48983,#48984,#48985,#48986,#48987,#48988,#48989,#48990,#48991,
#48992,#48993,#48994,#48995,#48996,#48997,#48998,#48999,#49000,#49001,#49002,
#49003,#49004,#49005,#49006,#49007,#49008,#49009,#49010,#49011,#49012,#49013,
#49014,#49015,#49016,#49017,#49018,#49019,#49020,#49021,#49022,#49023,#49024,
#49025,#49026,#49027,#49028,#49029,#49030,#49031,#49032,#49033,#49034,#49035,
#49036,#49037,#49038,#49039,#49040,#49041,#49042,#49043,#49044,#49045,#49046,
#49047,#49048,#49049,#49050,#49051,#49052,#49053,#49054,#49055,#49056,#49057,
#49058,#49059,#49060,#49061,#49062,#49063,#49064,#49065,#49066,#49067,#49068,
#49069,#49070,#49071,#49072,#49073,#49074,#49075,#49076,#49077,#49078,#49079,
#49080,#49081,#49082,#49083,#49084,#49085,#49086,#49087,#49088,#49089,#49090,
#49091,#49092,#49093,#49094,#49095,#49096,#49097,#49098,#49099,#49100,#49101,
#49102,#49103,#49104,#49105,#49106,#49107,#49108,#49109,#49110,#49111,#49112,
#49113,#49114,#49115,#49116,#49117,#49118,#49119,#49120,#49121,#49122,#49123,
#49124,#49125,#49126,#49127,#49128,#49129,#49130,#49131,#49132,#49133,#49134,
#49135,#49136,#49137,#49138,#49139,#49140,#49141,#49142,#49143,#49144,#49145,
#49146,#49147,#49148,#49149,#49150,#49151,#49152,#49153,#49154,#49155,#49156,
#49157,#49158,#49159,#49160,#49161,#49162,#49163,#49164,#49165,#49166,#49167,
#49168,#49169,#49170,#49171,#49172,#49173,#49174,#49175,#49176,#49177,#49178,
#49179,#49180,#49181,#49182,#49183,#49184,#49185,#49186,#49187,#49188,#49189,
#49190,#49191,#49192,#49193,#49194,#49195,#49196,#49197,#49198,#49199,#49200,
#49201,#49202,#49203,#49204,#49205,#49206,#49207,#49208,#49209,#49210,#49211,
#49212,#49213,#49214,#49215,#49216,#49217,#49218,#49219,#49220,#49221,#49222,
#49223,#49224,#49225,#49226,#49227,#49228,#49229,#49230,#49231,#49232,#49233,
#49234,#49235,#49236,#49237,#49238,#49239,#49240,#49241,#49242,#49243,#49244,
#49245,#49246,#49247,#49248,#49249,#49250,#49251,#49252,#49253,#49254,#49255,
#49256,#49257,#49258,#49259,#49260,#49261,#49262,#49263,#49264,#49265,#49266,
#49267,#49268,#49269,#49270,#49271,#49272,#49273,#49274,#49275,#49276,#49277,
#49278,#49279,#49280,#49281,#49282,#49283,#49284,#49285,#49286,#49287,#49288,
#49289,#49290,#49291,#49292,#49293,#49294,#49295,#49296,#49297,#49298,#49299,
#49300,#49301,#49302,#49303,#49304,#49305,#49306,#49307,#49308,#49309,#49310,
#49311,#49312,#49313,#49314,#49315,#49316,#49317,#49318,#49319,#49320,#49321,
#49322,#49323,#49324,#49325,#49326,#49327,#49328,#49329,#49330,#49331,#49332,
#49333,#49334,#49335,#49336,#49337,#49338,#49339,#49340,#49341,#49342,#49343,
#49344,#49345,#49346,#49347,#49348,#49349,#49350,#49351,#49352,#49353,#49354,
#49355,#49356,#49357,#49358,#49359,#49360,#49361,#49362,#49363,#49364,#49365,
#49366,#49367,#49368,#49369,#49370,#49371,#49372,#49373,#49374,#49375,#49376,
#49377,#49378,#49379,#49380,#49381,#49382,#49383,#49384,#49385,#49386,#49387,
#49388,#49389,#49390,#49391,#49392,#49393,#49394,#49395,#49396,#49397,#49398,
#49399,#49400,#49401,#49402,#49403,#49404,#49405,#49406,#49407,#49408,#49409,
#49410,#49411,#49412,#49413,#49414,#49415,#49416,#49417,#49418,#49419,#49420,
#49421,#49422,#49423,#49424,#49425,#49426,#49427,#49428,#49429,#49430,#49431,
#49432,#49433,#49434,#49435,#49436,#49437,#49438,#49439,#49440,#49441,#49442,
#49443,#49444,#49445,#49446,#49447,#49448,#49449,#49450,#49451,#49452,#49453,
#49454,#49455,#49456,#49457,#49458,#49459,#49460,#49461,#49462,#49463,#49464,
#49465,#49466,#49467,#49468,#49469,#49470,#49471,#49472,#49473,#49474,#49475,
#49476,#49477,#49478,#49479,#49480,#49481,#49482,#49483,#49484,#49485,#49486,
#49487,#49488,#49489,#49490,#49491,#49492,#49493,#49494,#49495,#49496,#49497,
#49498,#49499,#49500,#49501,#49502,#49503,#49504,#49505,#49506,#49507,#49508,
#49509,#49510,#49511,#49512,#49513,#49514,#49515,#49516,#49517,#49518,#49519,
#49520,#49521,#49522,#49523,#49524,#49525,#49526,#49527,#49528,#49529,#49530,
#49531,#49532,#49533,#49534,#49535,#49536,#49537,#49538,#49539,#49540,#49541,
#49542,#49543,#49544,#49545,#49546,#49547,#49548,#49549,#49550,#49551,#49552,
#49553,#49554,#49555,#49556,#49557,#49558,#49559,#49560,#49561,#49562,#49563,
#49564,#49565,#49566,#49567,#49568,#49569,#49570,#49571,#49572,#49573,#49574,
#49575,#49576,#49577,#49578,#49579,#49580,#49581,#49582,#49583,#49584,#49585,
#49586,#49587,#49588,#49589,#49590,#49591,#49592,#49593,#49594,#49595,#49596,
#49597,#49598,#49599,#49600,#49601,#49602,#49603,#49604,#49605,#49606,#49607,
#49608,#49609,#49610,#49611,#49612,#49613,#49614,#49615,#49616,#49617,#49618,
#49619,#49620,#49621,#49622,#49623,#49624,#49625,#49626,#49627,#49628,#49629,
#49630,#49631,#49632,#49633,#49634,#49635,#49636,#49637,#49638,#49639,#49640,
#49641,#49642,#49643,#49644,#49645,#49646,#49647,#49648,#49649,#49650,#49651,
#49652,#49653,#49654,#49655,#49656,#49657,#49658,#49659,#49660,#49661,#49662,
#49663,#49664,#49665,#49666,#49667,#49668,#49669,#49670,#49671,#49672,#49673,
#49674,#49675,#49676,#49677,#49678,#49679,#49680,#49681,#49682,#49683,#49684,
#49685,#49686,#49687,#49688,#49689,#49690,#49691,#49692,#49693,#49694,#49695,
#49696,#49697,#49698,#49699,#49700,#49701,#49702,#49703,#49704,#49705,#49706,
#49707,#49708,#49709,#49710,#49711,#49712,#49713,#49714,#49715,#49716,#49717,
#49718,#49719,#49720,#49721));
#51019=CLOSED_SHELL('',(#49722,#49723,#49724,#49725,#49726,#49727,#49728,
#49729,#49730,#49731,#49732,#49733,#49734,#49735,#49736,#49737,#49738,#49739,
#49740,#49741,#49742,#49743,#49744,#49745,#49746,#49747,#49748,#49749,#49750,
#49751,#49752,#49753,#49754,#49755,#49756,#49757,#49758,#49759,#49760,#49761,
#49762,#49763,#49764,#49765,#49766,#49767,#49768,#49769,#49770,#49771,#49772,
#49773,#49774,#49775,#49776,#49777,#49778,#49779,#49780,#49781,#49782,#49783,
#49784,#49785,#49786,#49787,#49788,#49789,#49790,#49791,#49792,#49793,#49794,
#49795,#49796,#49797,#49798,#49799,#49800,#49801,#49802,#49803,#49804,#49805,
#49806,#49807,#49808,#49809,#49810,#49811,#49812,#49813,#49814,#49815,#49816,
#49817,#49818,#49819,#49820,#49821,#49822,#49823,#49824,#49825,#49826,#49827,
#49828,#49829,#49830,#49831,#49832,#49833,#49834,#49835,#49836,#49837,#49838,
#49839,#49840,#49841,#49842,#49843,#49844,#49845,#49846,#49847,#49848,#49849,
#49850,#49851,#49852,#49853,#49854,#49855,#49856,#49857,#49858,#49859,#49860,
#49861,#49862,#49863,#49864,#49865,#49866,#49867,#49868,#49869,#49870,#49871,
#49872,#49873,#49874,#49875,#49876,#49877,#49878,#49879,#49880,#49881,#49882,
#49883,#49884,#49885,#49886,#49887,#49888,#49889,#49890,#49891,#49892,#49893,
#49894,#49895,#49896,#49897,#49898,#49899,#49900,#49901,#49902,#49903,#49904,
#49905,#49906,#49907,#49908,#49909,#49910,#49911,#49912,#49913,#49914,#49915,
#49916,#49917,#49918,#49919,#49920,#49921,#49922,#49923,#49924,#49925,#49926,
#49927,#49928,#49929,#49930,#49931,#49932,#49933,#49934,#49935,#49936,#49937,
#49938,#49939,#49940,#49941,#49942,#49943,#49944,#49945,#49946,#49947,#49948,
#49949,#49950,#49951,#49952,#49953,#49954,#49955,#49956,#49957,#49958,#49959,
#49960,#49961,#49962,#49963,#49964,#49965,#49966,#49967,#49968,#49969,#49970,
#49971,#49972,#49973,#49974,#49975,#49976,#49977,#49978,#49979,#49980,#49981,
#49982,#49983,#49984,#49985,#49986,#49987,#49988,#49989,#49990,#49991,#49992,
#49993,#49994,#49995,#49996,#49997,#49998,#49999,#50000,#50001,#50002,#50003,
#50004,#50005,#50006,#50007,#50008,#50009,#50010,#50011,#50012,#50013,#50014,
#50015,#50016,#50017,#50018,#50019,#50020,#50021,#50022,#50023,#50024,#50025,
#50026,#50027,#50028,#50029,#50030,#50031,#50032,#50033,#50034,#50035,#50036,
#50037,#50038,#50039,#50040,#50041,#50042,#50043,#50044,#50045,#50046,#50047,
#50048,#50049,#50050,#50051,#50052,#50053,#50054,#50055,#50056,#50057,#50058,
#50059,#50060,#50061,#50062,#50063,#50064,#50065,#50066,#50067,#50068,#50069,
#50070,#50071,#50072,#50073,#50074,#50075,#50076,#50077,#50078,#50079,#50080,
#50081,#50082,#50083,#50084,#50085,#50086));
#51020=CLOSED_SHELL('',(#50087,#50088,#50089,#50090,#50091,#50092,#50093,
#50094,#50095,#50096,#50097,#50098,#50099,#50100,#50101,#50102,#50103,#50104,
#50105,#50106,#50107,#50108,#50109,#50110,#50111,#50112,#50113,#50114,#50115,
#50116,#50117,#50118,#50119));
#51021=CLOSED_SHELL('',(#50120,#50121,#50122,#50123,#50124,#50125,#50126,
#50127,#50128,#50129,#50130,#50131,#50132,#50133,#50134,#50135,#50136,#50137,
#50138,#50139,#50140,#50141,#50142,#50143,#50144,#50145,#50146,#50147,#50148,
#50149,#50150,#50151,#50152,#50153,#50154,#50155,#50156,#50157,#50158,#50159,
#50160,#50161,#50162,#50163,#50164,#50165,#50166,#50167,#50168,#50169,#50170,
#50171,#50172,#50173,#50174,#50175,#50176,#50177,#50178,#50179,#50180,#50181,
#50182,#50183,#50184,#50185,#50186,#50187,#50188,#50189,#50190,#50191,#50192,
#50193,#50194,#50195,#50196,#50197,#50198,#50199,#50200,#50201,#50202,#50203,
#50204,#50205,#50206,#50207,#50208,#50209,#50210,#50211,#50212,#50213,#50214,
#50215,#50216,#50217,#50218,#50219,#50220,#50221,#50222,#50223,#50224,#50225,
#50226,#50227,#50228,#50229,#50230,#50231,#50232,#50233,#50234,#50235,#50236,
#50237,#50238,#50239,#50240,#50241,#50242,#50243,#50244,#50245,#50246,#50247,
#50248,#50249,#50250,#50251,#50252,#50253,#50254,#50255,#50256,#50257,#50258,
#50259,#50260,#50261,#50262,#50263,#50264,#50265,#50266,#50267,#50268,#50269,
#50270,#50271,#50272,#50273,#50274,#50275,#50276,#50277,#50278,#50279,#50280,
#50281,#50282,#50283,#50284,#50285,#50286,#50287,#50288,#50289,#50290,#50291,
#50292,#50293,#50294,#50295,#50296,#50297,#50298,#50299,#50300,#50301,#50302,
#50303,#50304,#50305,#50306,#50307,#50308,#50309,#50310,#50311,#50312,#50313,
#50314,#50315,#50316,#50317,#50318,#50319,#50320,#50321,#50322,#50323,#50324,
#50325,#50326,#50327,#50328,#50329,#50330,#50331,#50332,#50333,#50334,#50335,
#50336,#50337,#50338,#50339,#50340,#50341,#50342,#50343,#50344,#50345,#50346,
#50347,#50348,#50349,#50350,#50351,#50352,#50353,#50354,#50355,#50356,#50357,
#50358,#50359,#50360,#50361,#50362,#50363,#50364,#50365,#50366,#50367,#50368,
#50369,#50370,#50371,#50372,#50373,#50374,#50375,#50376,#50377,#50378,#50379,
#50380,#50381,#50382,#50383,#50384,#50385,#50386,#50387,#50388,#50389,#50390,
#50391,#50392,#50393,#50394,#50395,#50396,#50397,#50398,#50399,#50400,#50401,
#50402,#50403,#50404,#50405,#50406,#50407,#50408,#50409,#50410,#50411,#50412,
#50413,#50414,#50415,#50416,#50417,#50418,#50419,#50420,#50421,#50422,#50423,
#50424,#50425,#50426,#50427,#50428,#50429,#50430,#50431,#50432,#50433,#50434,
#50435,#50436,#50437,#50438,#50439,#50440,#50441,#50442,#50443,#50444,#50445,
#50446,#50447,#50448,#50449,#50450,#50451,#50452,#50453,#50454,#50455,#50456,
#50457,#50458,#50459,#50460,#50461,#50462,#50463,#50464,#50465,#50466,#50467,
#50468,#50469,#50470,#50471,#50472,#50473,#50474,#50475,#50476,#50477,#50478,
#50479,#50480,#50481,#50482,#50483,#50484,#50485,#50486,#50487,#50488,#50489,
#50490,#50491,#50492));
#51022=CLOSED_SHELL('',(#50493,#50494,#50495,#50496,#50497,#50498,#50499,
#50500));
#51023=CLOSED_SHELL('',(#50501,#50502,#50503,#50504,#50505,#50506,#50507,
#50508,#50509,#50510,#50511,#50512,#50513,#50514,#50515,#50516,#50517,#50518,
#50519,#50520,#50521,#50522,#50523,#50524,#50525,#50526,#50527,#50528,#50529,
#50530,#50531,#50532,#50533,#50534,#50535,#50536,#50537,#50538,#50539,#50540,
#50541,#50542,#50543,#50544,#50545,#50546,#50547,#50548,#50549,#50550,#50551,
#50552,#50553,#50554,#50555,#50556,#50557,#50558,#50559,#50560,#50561,#50562,
#50563,#50564,#50565,#50566,#50567,#50568,#50569,#50570,#50571,#50572,#50573,
#50574,#50575,#50576,#50577,#50578,#50579,#50580,#50581,#50582,#50583,#50584,
#50585,#50586,#50587,#50588,#50589,#50590,#50591,#50592,#50593,#50594,#50595,
#50596,#50597,#50598,#50599,#50600,#50601,#50602,#50603,#50604,#50605,#50606,
#50607,#50608,#50609,#50610,#50611,#50612,#50613,#50614,#50615,#50616,#50617,
#50618,#50619,#50620,#50621,#50622,#50623,#50624,#50625,#50626,#50627,#50628,
#50629,#50630,#50631,#50632,#50633,#50634,#50635,#50636,#50637,#50638,#50639,
#50640,#50641,#50642,#50643,#50644,#50645,#50646,#50647,#50648,#50649,#50650,
#50651,#50652,#50653,#50654,#50655,#50656,#50657,#50658,#50659,#50660,#50661,
#50662,#50663,#50664,#50665,#50666,#50667,#50668,#50669,#50670,#50671,#50672,
#50673,#50674,#50675,#50676,#50677,#50678,#50679,#50680,#50681,#50682,#50683,
#50684,#50685,#50686,#50687,#50688,#50689,#50690,#50691,#50692,#50693,#50694,
#50695,#50696,#50697));
#51024=CLOSED_SHELL('',(#50698,#50699,#50700,#50701,#50702,#50703,#50704,
#50705));
#51025=CLOSED_SHELL('',(#50706,#50707,#50708,#50709,#50710,#50711,#50712,
#50713,#50714,#50715,#50716,#50717));
#51026=CLOSED_SHELL('',(#50718,#50719,#50720,#50721,#50722,#50723,#50724,
#50725,#50726,#50727,#50728,#50729,#50730,#50731,#50732,#50733,#50734,#50735,
#50736,#50737,#50738,#50739,#50740,#50741,#50742,#50743,#50744,#50745,#50746,
#50747,#50748,#50749,#50750,#50751,#50752,#50753,#50754,#50755,#50756,#50757,
#50758,#50759,#50760,#50761,#50762,#50763,#50764,#50765,#50766,#50767,#50768,
#50769,#50770,#50771,#50772,#50773,#50774,#50775,#50776,#50777,#50778,#50779,
#50780,#50781,#50782,#50783,#50784,#50785,#50786,#50787,#50788,#50789,#50790,
#50791,#50792,#50793,#50794,#50795,#50796,#50797,#50798,#50799,#50800,#50801,
#50802,#50803,#50804,#50805,#50806,#50807,#50808,#50809,#50810,#50811,#50812,
#50813,#50814,#50815,#50816,#50817,#50818,#50819,#50820,#50821,#50822,#50823,
#50824,#50825,#50826,#50827,#50828,#50829,#50830,#50831,#50832,#50833,#50834,
#50835,#50836,#50837,#50838,#50839,#50840,#50841,#50842,#50843,#50844,#50845,
#50846,#50847,#50848,#50849,#50850,#50851,#50852,#50853,#50854,#50855,#50856,
#50857,#50858,#50859,#50860,#50861,#50862,#50863,#50864,#50865,#50866,#50867,
#50868,#50869,#50870,#50871,#50872,#50873,#50874,#50875,#50876,#50877,#50878,
#50879,#50880,#50881,#50882,#50883,#50884,#50885,#50886,#50887,#50888,#50889,
#50890,#50891,#50892,#50893,#50894,#50895,#50896,#50897,#50898,#50899,#50900,
#50901,#50902,#50903,#50904,#50905,#50906,#50907,#50908,#50909,#50910,#50911,
#50912,#50913));
#51027=CLOSED_SHELL('',(#50914,#50915,#50916,#50917,#50918,#50919));
#51028=CLOSED_SHELL('',(#50920,#50921,#50922,#50923,#50924,#50925,#50926,
#50927,#50928,#50929,#50930,#50931,#50932,#50933,#50934,#50935,#50936,#50937,
#50938,#50939,#50940,#50941,#50942,#50943,#50944,#50945,#50946,#50947,#50948,
#50949,#50950,#50951,#50952,#50953,#50954,#50955,#50956,#50957,#50958,#50959,
#50960,#50961,#50962,#50963,#50964,#50965,#50966,#50967,#50968,#50969,#50970,
#50971,#50972,#50973,#50974,#50975,#50976,#50977,#50978,#50979,#50980,#50981,
#50982,#50983,#50984,#50985));
#51029=CLOSED_SHELL('',(#50986,#50987,#50988,#50989,#50990,#50991,#50992,
#50993));
#51030=CLOSED_SHELL('',(#50994,#50995,#50996,#50997,#50998,#50999,#51000,
#51001,#51002,#51003,#51004));
#51031=CLOSED_SHELL('',(#51005,#51006,#51007,#51008,#51009,#51010,#51011,
#51012,#51013,#51014,#51015,#51016,#51017));
#51032=DERIVED_UNIT_ELEMENT(#51060,1.);
#51033=DERIVED_UNIT_ELEMENT(#94303,-3.);
#51034=DERIVED_UNIT_ELEMENT(#51060,1.);
#51035=DERIVED_UNIT_ELEMENT(#94303,-3.);
#51036=DERIVED_UNIT_ELEMENT(#51060,1.);
#51037=DERIVED_UNIT_ELEMENT(#94303,-3.);
#51038=DERIVED_UNIT_ELEMENT(#51060,1.);
#51039=DERIVED_UNIT_ELEMENT(#94303,-3.);
#51040=DERIVED_UNIT_ELEMENT(#51060,1.);
#51041=DERIVED_UNIT_ELEMENT(#94303,-3.);
#51042=DERIVED_UNIT_ELEMENT(#51060,1.);
#51043=DERIVED_UNIT_ELEMENT(#94303,-3.);
#51044=DERIVED_UNIT_ELEMENT(#51060,1.);
#51045=DERIVED_UNIT_ELEMENT(#94303,-3.);
#51046=DERIVED_UNIT_ELEMENT(#51060,1.);
#51047=DERIVED_UNIT_ELEMENT(#94303,-3.);
#51048=DERIVED_UNIT_ELEMENT(#51060,1.);
#51049=DERIVED_UNIT_ELEMENT(#94303,-3.);
#51050=DERIVED_UNIT_ELEMENT(#51060,1.);
#51051=DERIVED_UNIT_ELEMENT(#94303,-3.);
#51052=DERIVED_UNIT_ELEMENT(#51060,1.);
#51053=DERIVED_UNIT_ELEMENT(#94303,-3.);
#51054=DERIVED_UNIT_ELEMENT(#51060,1.);
#51055=DERIVED_UNIT_ELEMENT(#94303,-3.);
#51056=DERIVED_UNIT_ELEMENT(#51060,1.);
#51057=DERIVED_UNIT_ELEMENT(#94303,-3.);
#51058=DERIVED_UNIT_ELEMENT(#51060,1.);
#51059=DERIVED_UNIT_ELEMENT(#94303,-3.);
#51060=(
MASS_UNIT()
NAMED_UNIT(*)
SI_UNIT(.KILO.,.GRAM.)
);
#51061=DERIVED_UNIT((#51032,#51033));
#51062=DERIVED_UNIT((#51034,#51035));
#51063=DERIVED_UNIT((#51036,#51037));
#51064=DERIVED_UNIT((#51038,#51039));
#51065=DERIVED_UNIT((#51040,#51041));
#51066=DERIVED_UNIT((#51042,#51043));
#51067=DERIVED_UNIT((#51044,#51045));
#51068=DERIVED_UNIT((#51046,#51047));
#51069=DERIVED_UNIT((#51048,#51049));
#51070=DERIVED_UNIT((#51050,#51051));
#51071=DERIVED_UNIT((#51052,#51053));
#51072=DERIVED_UNIT((#51054,#51055));
#51073=DERIVED_UNIT((#51056,#51057));
#51074=DERIVED_UNIT((#51058,#51059));
#51075=MEASURE_REPRESENTATION_ITEM('density measure',
POSITIVE_RATIO_MEASURE(7850.),#51061);
#51076=MEASURE_REPRESENTATION_ITEM('density measure',
POSITIVE_RATIO_MEASURE(7850.),#51062);
#51077=MEASURE_REPRESENTATION_ITEM('density measure',
POSITIVE_RATIO_MEASURE(7850.),#51063);
#51078=MEASURE_REPRESENTATION_ITEM('density measure',
POSITIVE_RATIO_MEASURE(7850.),#51064);
#51079=MEASURE_REPRESENTATION_ITEM('density measure',
POSITIVE_RATIO_MEASURE(7850.),#51065);
#51080=MEASURE_REPRESENTATION_ITEM('density measure',
POSITIVE_RATIO_MEASURE(7850.),#51066);
#51081=MEASURE_REPRESENTATION_ITEM('density measure',
POSITIVE_RATIO_MEASURE(7850.),#51067);
#51082=MEASURE_REPRESENTATION_ITEM('density measure',
POSITIVE_RATIO_MEASURE(7850.),#51068);
#51083=MEASURE_REPRESENTATION_ITEM('density measure',
POSITIVE_RATIO_MEASURE(7850.),#51069);
#51084=MEASURE_REPRESENTATION_ITEM('density measure',
POSITIVE_RATIO_MEASURE(7850.),#51070);
#51085=MEASURE_REPRESENTATION_ITEM('density measure',
POSITIVE_RATIO_MEASURE(7850.),#51071);
#51086=MEASURE_REPRESENTATION_ITEM('density measure',
POSITIVE_RATIO_MEASURE(7850.),#51072);
#51087=MEASURE_REPRESENTATION_ITEM('density measure',
POSITIVE_RATIO_MEASURE(7850.),#51073);
#51088=MEASURE_REPRESENTATION_ITEM('density measure',
POSITIVE_RATIO_MEASURE(7850.),#51074);
#51089=PROPERTY_DEFINITION_REPRESENTATION(#51159,#51117);
#51090=PROPERTY_DEFINITION_REPRESENTATION(#51160,#51118);
#51091=PROPERTY_DEFINITION_REPRESENTATION(#51161,#51119);
#51092=PROPERTY_DEFINITION_REPRESENTATION(#51162,#51120);
#51093=PROPERTY_DEFINITION_REPRESENTATION(#51163,#51121);
#51094=PROPERTY_DEFINITION_REPRESENTATION(#51164,#51122);
#51095=PROPERTY_DEFINITION_REPRESENTATION(#51165,#51123);
#51096=PROPERTY_DEFINITION_REPRESENTATION(#51166,#51124);
#51097=PROPERTY_DEFINITION_REPRESENTATION(#51167,#51125);
#51098=PROPERTY_DEFINITION_REPRESENTATION(#51168,#51126);
#51099=PROPERTY_DEFINITION_REPRESENTATION(#51169,#51127);
#51100=PROPERTY_DEFINITION_REPRESENTATION(#51170,#51128);
#51101=PROPERTY_DEFINITION_REPRESENTATION(#51171,#51129);
#51102=PROPERTY_DEFINITION_REPRESENTATION(#51172,#51130);
#51103=PROPERTY_DEFINITION_REPRESENTATION(#51173,#51131);
#51104=PROPERTY_DEFINITION_REPRESENTATION(#51174,#51132);
#51105=PROPERTY_DEFINITION_REPRESENTATION(#51175,#51133);
#51106=PROPERTY_DEFINITION_REPRESENTATION(#51176,#51134);
#51107=PROPERTY_DEFINITION_REPRESENTATION(#51177,#51135);
#51108=PROPERTY_DEFINITION_REPRESENTATION(#51178,#51136);
#51109=PROPERTY_DEFINITION_REPRESENTATION(#51179,#51137);
#51110=PROPERTY_DEFINITION_REPRESENTATION(#51180,#51138);
#51111=PROPERTY_DEFINITION_REPRESENTATION(#51181,#51139);
#51112=PROPERTY_DEFINITION_REPRESENTATION(#51182,#51140);
#51113=PROPERTY_DEFINITION_REPRESENTATION(#51183,#51141);
#51114=PROPERTY_DEFINITION_REPRESENTATION(#51184,#51142);
#51115=PROPERTY_DEFINITION_REPRESENTATION(#51185,#51143);
#51116=PROPERTY_DEFINITION_REPRESENTATION(#51186,#51144);
#51117=REPRESENTATION('material name',(#51145),#94287);
#51118=REPRESENTATION('density',(#51075),#94287);
#51119=REPRESENTATION('material name',(#51146),#94288);
#51120=REPRESENTATION('density',(#51076),#94288);
#51121=REPRESENTATION('material name',(#51147),#94289);
#51122=REPRESENTATION('density',(#51077),#94289);
#51123=REPRESENTATION('material name',(#51148),#94290);
#51124=REPRESENTATION('density',(#51078),#94290);
#51125=REPRESENTATION('material name',(#51149),#94291);
#51126=REPRESENTATION('density',(#51079),#94291);
#51127=REPRESENTATION('material name',(#51150),#94292);
#51128=REPRESENTATION('density',(#51080),#94292);
#51129=REPRESENTATION('material name',(#51151),#94293);
#51130=REPRESENTATION('density',(#51081),#94293);
#51131=REPRESENTATION('material name',(#51152),#94294);
#51132=REPRESENTATION('density',(#51082),#94294);
#51133=REPRESENTATION('material name',(#51153),#94295);
#51134=REPRESENTATION('density',(#51083),#94295);
#51135=REPRESENTATION('material name',(#51154),#94296);
#51136=REPRESENTATION('density',(#51084),#94296);
#51137=REPRESENTATION('material name',(#51155),#94297);
#51138=REPRESENTATION('density',(#51085),#94297);
#51139=REPRESENTATION('material name',(#51156),#94298);
#51140=REPRESENTATION('density',(#51086),#94298);
#51141=REPRESENTATION('material name',(#51157),#94299);
#51142=REPRESENTATION('density',(#51087),#94299);
#51143=REPRESENTATION('material name',(#51158),#94300);
#51144=REPRESENTATION('density',(#51088),#94300);
#51145=DESCRIPTIVE_REPRESENTATION_ITEM('Steel','Steel');
#51146=DESCRIPTIVE_REPRESENTATION_ITEM('Steel','Steel');
#51147=DESCRIPTIVE_REPRESENTATION_ITEM('Steel','Steel');
#51148=DESCRIPTIVE_REPRESENTATION_ITEM('Steel','Steel');
#51149=DESCRIPTIVE_REPRESENTATION_ITEM('Steel','Steel');
#51150=DESCRIPTIVE_REPRESENTATION_ITEM('Steel','Steel');
#51151=DESCRIPTIVE_REPRESENTATION_ITEM('Steel','Steel');
#51152=DESCRIPTIVE_REPRESENTATION_ITEM('Steel','Steel');
#51153=DESCRIPTIVE_REPRESENTATION_ITEM('Steel','Steel');
#51154=DESCRIPTIVE_REPRESENTATION_ITEM('Steel','Steel');
#51155=DESCRIPTIVE_REPRESENTATION_ITEM('Steel','Steel');
#51156=DESCRIPTIVE_REPRESENTATION_ITEM('Steel','Steel');
#51157=DESCRIPTIVE_REPRESENTATION_ITEM('Steel','Steel');
#51158=DESCRIPTIVE_REPRESENTATION_ITEM('Steel','Steel');
#51159=PROPERTY_DEFINITION('material property','material name',#94387);
#51160=PROPERTY_DEFINITION('material property','density of part',#94387);
#51161=PROPERTY_DEFINITION('material property','material name',#94388);
#51162=PROPERTY_DEFINITION('material property','density of part',#94388);
#51163=PROPERTY_DEFINITION('material property','material name',#94389);
#51164=PROPERTY_DEFINITION('material property','density of part',#94389);
#51165=PROPERTY_DEFINITION('material property','material name',#94390);
#51166=PROPERTY_DEFINITION('material property','density of part',#94390);
#51167=PROPERTY_DEFINITION('material property','material name',#94391);
#51168=PROPERTY_DEFINITION('material property','density of part',#94391);
#51169=PROPERTY_DEFINITION('material property','material name',#94392);
#51170=PROPERTY_DEFINITION('material property','density of part',#94392);
#51171=PROPERTY_DEFINITION('material property','material name',#94393);
#51172=PROPERTY_DEFINITION('material property','density of part',#94393);
#51173=PROPERTY_DEFINITION('material property','material name',#94394);
#51174=PROPERTY_DEFINITION('material property','density of part',#94394);
#51175=PROPERTY_DEFINITION('material property','material name',#94395);
#51176=PROPERTY_DEFINITION('material property','density of part',#94395);
#51177=PROPERTY_DEFINITION('material property','material name',#94396);
#51178=PROPERTY_DEFINITION('material property','density of part',#94396);
#51179=PROPERTY_DEFINITION('material property','material name',#94397);
#51180=PROPERTY_DEFINITION('material property','density of part',#94397);
#51181=PROPERTY_DEFINITION('material property','material name',#94398);
#51182=PROPERTY_DEFINITION('material property','density of part',#94398);
#51183=PROPERTY_DEFINITION('material property','material name',#94399);
#51184=PROPERTY_DEFINITION('material property','density of part',#94399);
#51185=PROPERTY_DEFINITION('material property','material name',#94400);
#51186=PROPERTY_DEFINITION('material property','density of part',#94400);
#51187=AXIS2_PLACEMENT_3D('',#68258,#55368,#55369);
#51188=AXIS2_PLACEMENT_3D('',#68259,#55370,#55371);
#51189=AXIS2_PLACEMENT_3D('',#68260,#55372,#55373);
#51190=AXIS2_PLACEMENT_3D('',#68263,#55374,#55375);
#51191=AXIS2_PLACEMENT_3D('',#68275,#55376,#55377);
#51192=AXIS2_PLACEMENT_3D('',#68278,#55378,#55379);
#51193=AXIS2_PLACEMENT_3D('',#68290,#55380,#55381);
#51194=AXIS2_PLACEMENT_3D('',#68293,#55382,#55383);
#51195=AXIS2_PLACEMENT_3D('',#68305,#55384,#55385);
#51196=AXIS2_PLACEMENT_3D('',#68308,#55386,#55387);
#51197=AXIS2_PLACEMENT_3D('',#68320,#55388,#55389);
#51198=AXIS2_PLACEMENT_3D('',#68323,#55390,#55391);
#51199=AXIS2_PLACEMENT_3D('',#68335,#55392,#55393);
#51200=AXIS2_PLACEMENT_3D('',#68338,#55394,#55395);
#51201=AXIS2_PLACEMENT_3D('',#68350,#55396,#55397);
#51202=AXIS2_PLACEMENT_3D('',#68353,#55398,#55399);
#51203=AXIS2_PLACEMENT_3D('',#68365,#55400,#55401);
#51204=AXIS2_PLACEMENT_3D('',#68368,#55402,#55403);
#51205=AXIS2_PLACEMENT_3D('',#68380,#55404,#55405);
#51206=AXIS2_PLACEMENT_3D('',#68383,#55406,#55407);
#51207=AXIS2_PLACEMENT_3D('',#68395,#55408,#55409);
#51208=AXIS2_PLACEMENT_3D('',#68398,#55410,#55411);
#51209=AXIS2_PLACEMENT_3D('',#68410,#55412,#55413);
#51210=AXIS2_PLACEMENT_3D('',#68413,#55414,#55415);
#51211=AXIS2_PLACEMENT_3D('',#68425,#55416,#55417);
#51212=AXIS2_PLACEMENT_3D('',#68428,#55418,#55419);
#51213=AXIS2_PLACEMENT_3D('',#68440,#55420,#55421);
#51214=AXIS2_PLACEMENT_3D('',#68443,#55422,#55423);
#51215=AXIS2_PLACEMENT_3D('',#68455,#55424,#55425);
#51216=AXIS2_PLACEMENT_3D('',#68458,#55426,#55427);
#51217=AXIS2_PLACEMENT_3D('',#68470,#55428,#55429);
#51218=AXIS2_PLACEMENT_3D('',#68473,#55430,#55431);
#51219=AXIS2_PLACEMENT_3D('',#68485,#55432,#55433);
#51220=AXIS2_PLACEMENT_3D('',#68488,#55434,#55435);
#51221=AXIS2_PLACEMENT_3D('',#68500,#55436,#55437);
#51222=AXIS2_PLACEMENT_3D('',#68503,#55438,#55439);
#51223=AXIS2_PLACEMENT_3D('',#68515,#55440,#55441);
#51224=AXIS2_PLACEMENT_3D('',#68518,#55442,#55443);
#51225=AXIS2_PLACEMENT_3D('',#68530,#55444,#55445);
#51226=AXIS2_PLACEMENT_3D('',#68533,#55446,#55447);
#51227=AXIS2_PLACEMENT_3D('',#68545,#55448,#55449);
#51228=AXIS2_PLACEMENT_3D('',#68548,#55450,#55451);
#51229=AXIS2_PLACEMENT_3D('',#68560,#55452,#55453);
#51230=AXIS2_PLACEMENT_3D('',#68563,#55454,#55455);
#51231=AXIS2_PLACEMENT_3D('',#68575,#55456,#55457);
#51232=AXIS2_PLACEMENT_3D('',#68578,#55458,#55459);
#51233=AXIS2_PLACEMENT_3D('',#68590,#55460,#55461);
#51234=AXIS2_PLACEMENT_3D('',#68593,#55462,#55463);
#51235=AXIS2_PLACEMENT_3D('',#68605,#55464,#55465);
#51236=AXIS2_PLACEMENT_3D('',#68608,#55466,#55467);
#51237=AXIS2_PLACEMENT_3D('',#68620,#55468,#55469);
#51238=AXIS2_PLACEMENT_3D('',#68623,#55470,#55471);
#51239=AXIS2_PLACEMENT_3D('',#68635,#55472,#55473);
#51240=AXIS2_PLACEMENT_3D('',#68638,#55474,#55475);
#51241=AXIS2_PLACEMENT_3D('',#68650,#55476,#55477);
#51242=AXIS2_PLACEMENT_3D('',#68653,#55478,#55479);
#51243=AXIS2_PLACEMENT_3D('',#68665,#55480,#55481);
#51244=AXIS2_PLACEMENT_3D('',#68668,#55482,#55483);
#51245=AXIS2_PLACEMENT_3D('',#68680,#55484,#55485);
#51246=AXIS2_PLACEMENT_3D('',#68683,#55486,#55487);
#51247=AXIS2_PLACEMENT_3D('',#68695,#55488,#55489);
#51248=AXIS2_PLACEMENT_3D('',#68698,#55490,#55491);
#51249=AXIS2_PLACEMENT_3D('',#68710,#55492,#55493);
#51250=AXIS2_PLACEMENT_3D('',#68713,#55494,#55495);
#51251=AXIS2_PLACEMENT_3D('',#68725,#55496,#55497);
#51252=AXIS2_PLACEMENT_3D('',#68728,#55498,#55499);
#51253=AXIS2_PLACEMENT_3D('',#68740,#55500,#55501);
#51254=AXIS2_PLACEMENT_3D('',#68743,#55502,#55503);
#51255=AXIS2_PLACEMENT_3D('',#68755,#55504,#55505);
#51256=AXIS2_PLACEMENT_3D('',#68758,#55506,#55507);
#51257=AXIS2_PLACEMENT_3D('',#68770,#55508,#55509);
#51258=AXIS2_PLACEMENT_3D('',#68773,#55510,#55511);
#51259=AXIS2_PLACEMENT_3D('',#68785,#55512,#55513);
#51260=AXIS2_PLACEMENT_3D('',#68788,#55514,#55515);
#51261=AXIS2_PLACEMENT_3D('',#68800,#55516,#55517);
#51262=AXIS2_PLACEMENT_3D('',#68864,#55548,#55549);
#51263=AXIS2_PLACEMENT_3D('',#68874,#55552,#55553);
#51264=AXIS2_PLACEMENT_3D('',#68876,#55555,#55556);
#51265=AXIS2_PLACEMENT_3D('',#68940,#55587,#55588);
#51266=AXIS2_PLACEMENT_3D('',#68950,#55591,#55592);
#51267=AXIS2_PLACEMENT_3D('',#68952,#55594,#55595);
#51268=AXIS2_PLACEMENT_3D('',#69016,#55626,#55627);
#51269=AXIS2_PLACEMENT_3D('',#69026,#55630,#55631);
#51270=AXIS2_PLACEMENT_3D('',#69028,#55633,#55634);
#51271=AXIS2_PLACEMENT_3D('',#69092,#55665,#55666);
#51272=AXIS2_PLACEMENT_3D('',#69102,#55669,#55670);
#51273=AXIS2_PLACEMENT_3D('',#69104,#55672,#55673);
#51274=AXIS2_PLACEMENT_3D('',#69168,#55704,#55705);
#51275=AXIS2_PLACEMENT_3D('',#69178,#55708,#55709);
#51276=AXIS2_PLACEMENT_3D('',#69180,#55711,#55712);
#51277=AXIS2_PLACEMENT_3D('',#69244,#55743,#55744);
#51278=AXIS2_PLACEMENT_3D('',#69254,#55747,#55748);
#51279=AXIS2_PLACEMENT_3D('',#69256,#55750,#55751);
#51280=AXIS2_PLACEMENT_3D('',#69320,#55782,#55783);
#51281=AXIS2_PLACEMENT_3D('',#69330,#55786,#55787);
#51282=AXIS2_PLACEMENT_3D('',#69332,#55789,#55790);
#51283=AXIS2_PLACEMENT_3D('',#69396,#55821,#55822);
#51284=AXIS2_PLACEMENT_3D('',#69406,#55825,#55826);
#51285=AXIS2_PLACEMENT_3D('',#69408,#55828,#55829);
#51286=AXIS2_PLACEMENT_3D('',#69472,#55860,#55861);
#51287=AXIS2_PLACEMENT_3D('',#69482,#55864,#55865);
#51288=AXIS2_PLACEMENT_3D('',#69484,#55867,#55868);
#51289=AXIS2_PLACEMENT_3D('',#69548,#55899,#55900);
#51290=AXIS2_PLACEMENT_3D('',#69558,#55903,#55904);
#51291=AXIS2_PLACEMENT_3D('',#69560,#55906,#55907);
#51292=AXIS2_PLACEMENT_3D('',#69624,#55938,#55939);
#51293=AXIS2_PLACEMENT_3D('',#69634,#55942,#55943);
#51294=AXIS2_PLACEMENT_3D('',#69636,#55945,#55946);
#51295=AXIS2_PLACEMENT_3D('',#69700,#55977,#55978);
#51296=AXIS2_PLACEMENT_3D('',#69710,#55981,#55982);
#51297=AXIS2_PLACEMENT_3D('',#69712,#55984,#55985);
#51298=AXIS2_PLACEMENT_3D('',#69776,#56016,#56017);
#51299=AXIS2_PLACEMENT_3D('',#69786,#56020,#56021);
#51300=AXIS2_PLACEMENT_3D('',#69788,#56023,#56024);
#51301=AXIS2_PLACEMENT_3D('',#69852,#56055,#56056);
#51302=AXIS2_PLACEMENT_3D('',#69862,#56059,#56060);
#51303=AXIS2_PLACEMENT_3D('',#69864,#56062,#56063);
#51304=AXIS2_PLACEMENT_3D('',#69928,#56094,#56095);
#51305=AXIS2_PLACEMENT_3D('',#69938,#56098,#56099);
#51306=AXIS2_PLACEMENT_3D('',#69940,#56101,#56102);
#51307=AXIS2_PLACEMENT_3D('',#70004,#56133,#56134);
#51308=AXIS2_PLACEMENT_3D('',#70014,#56137,#56138);
#51309=AXIS2_PLACEMENT_3D('',#70016,#56140,#56141);
#51310=AXIS2_PLACEMENT_3D('',#70080,#56172,#56173);
#51311=AXIS2_PLACEMENT_3D('',#70090,#56176,#56177);
#51312=AXIS2_PLACEMENT_3D('',#70092,#56179,#56180);
#51313=AXIS2_PLACEMENT_3D('',#70156,#56211,#56212);
#51314=AXIS2_PLACEMENT_3D('',#70166,#56215,#56216);
#51315=AXIS2_PLACEMENT_3D('',#70168,#56218,#56219);
#51316=AXIS2_PLACEMENT_3D('',#70232,#56250,#56251);
#51317=AXIS2_PLACEMENT_3D('',#70242,#56254,#56255);
#51318=AXIS2_PLACEMENT_3D('',#70244,#56257,#56258);
#51319=AXIS2_PLACEMENT_3D('',#70308,#56289,#56290);
#51320=AXIS2_PLACEMENT_3D('',#70318,#56293,#56294);
#51321=AXIS2_PLACEMENT_3D('',#70320,#56296,#56297);
#51322=AXIS2_PLACEMENT_3D('',#70384,#56328,#56329);
#51323=AXIS2_PLACEMENT_3D('',#70394,#56332,#56333);
#51324=AXIS2_PLACEMENT_3D('',#70396,#56335,#56336);
#51325=AXIS2_PLACEMENT_3D('',#70460,#56367,#56368);
#51326=AXIS2_PLACEMENT_3D('',#70470,#56371,#56372);
#51327=AXIS2_PLACEMENT_3D('',#70472,#56374,#56375);
#51328=AXIS2_PLACEMENT_3D('',#70536,#56406,#56407);
#51329=AXIS2_PLACEMENT_3D('',#70546,#56410,#56411);
#51330=AXIS2_PLACEMENT_3D('',#70548,#56413,#56414);
#51331=AXIS2_PLACEMENT_3D('',#70612,#56445,#56446);
#51332=AXIS2_PLACEMENT_3D('',#70622,#56449,#56450);
#51333=AXIS2_PLACEMENT_3D('',#70624,#56452,#56453);
#51334=AXIS2_PLACEMENT_3D('',#70688,#56484,#56485);
#51335=AXIS2_PLACEMENT_3D('',#70698,#56488,#56489);
#51336=AXIS2_PLACEMENT_3D('',#70700,#56491,#56492);
#51337=AXIS2_PLACEMENT_3D('',#70764,#56523,#56524);
#51338=AXIS2_PLACEMENT_3D('',#70774,#56527,#56528);
#51339=AXIS2_PLACEMENT_3D('',#70776,#56530,#56531);
#51340=AXIS2_PLACEMENT_3D('',#70840,#56562,#56563);
#51341=AXIS2_PLACEMENT_3D('',#70850,#56566,#56567);
#51342=AXIS2_PLACEMENT_3D('',#70852,#56569,#56570);
#51343=AXIS2_PLACEMENT_3D('',#70916,#56601,#56602);
#51344=AXIS2_PLACEMENT_3D('',#70926,#56605,#56606);
#51345=AXIS2_PLACEMENT_3D('',#70928,#56608,#56609);
#51346=AXIS2_PLACEMENT_3D('',#70992,#56640,#56641);
#51347=AXIS2_PLACEMENT_3D('',#71002,#56644,#56645);
#51348=AXIS2_PLACEMENT_3D('',#71004,#56647,#56648);
#51349=AXIS2_PLACEMENT_3D('',#71068,#56679,#56680);
#51350=AXIS2_PLACEMENT_3D('',#71078,#56683,#56684);
#51351=AXIS2_PLACEMENT_3D('',#71080,#56686,#56687);
#51352=AXIS2_PLACEMENT_3D('',#71144,#56718,#56719);
#51353=AXIS2_PLACEMENT_3D('',#71154,#56722,#56723);
#51354=AXIS2_PLACEMENT_3D('',#71156,#56725,#56726);
#51355=AXIS2_PLACEMENT_3D('',#71220,#56757,#56758);
#51356=AXIS2_PLACEMENT_3D('',#71230,#56761,#56762);
#51357=AXIS2_PLACEMENT_3D('',#71232,#56764,#56765);
#51358=AXIS2_PLACEMENT_3D('',#71296,#56796,#56797);
#51359=AXIS2_PLACEMENT_3D('',#71306,#56800,#56801);
#51360=AXIS2_PLACEMENT_3D('',#71308,#56803,#56804);
#51361=AXIS2_PLACEMENT_3D('',#71372,#56835,#56836);
#51362=AXIS2_PLACEMENT_3D('',#71382,#56839,#56840);
#51363=AXIS2_PLACEMENT_3D('',#71384,#56842,#56843);
#51364=AXIS2_PLACEMENT_3D('',#71448,#56874,#56875);
#51365=AXIS2_PLACEMENT_3D('',#71458,#56878,#56879);
#51366=AXIS2_PLACEMENT_3D('',#71460,#56881,#56882);
#51367=AXIS2_PLACEMENT_3D('',#71524,#56913,#56914);
#51368=AXIS2_PLACEMENT_3D('',#71534,#56917,#56918);
#51369=AXIS2_PLACEMENT_3D('',#71536,#56920,#56921);
#51370=AXIS2_PLACEMENT_3D('',#71539,#56922,#56923);
#51371=AXIS2_PLACEMENT_3D('',#71546,#56924,#56925);
#51372=AXIS2_PLACEMENT_3D('',#71549,#56926,#56927);
#51373=AXIS2_PLACEMENT_3D('',#71556,#56928,#56929);
#51374=AXIS2_PLACEMENT_3D('',#71559,#56930,#56931);
#51375=AXIS2_PLACEMENT_3D('',#71566,#56932,#56933);
#51376=AXIS2_PLACEMENT_3D('',#71569,#56934,#56935);
#51377=AXIS2_PLACEMENT_3D('',#71576,#56936,#56937);
#51378=AXIS2_PLACEMENT_3D('',#71579,#56938,#56939);
#51379=AXIS2_PLACEMENT_3D('',#71586,#56940,#56941);
#51380=AXIS2_PLACEMENT_3D('',#71589,#56942,#56943);
#51381=AXIS2_PLACEMENT_3D('',#71596,#56944,#56945);
#51382=AXIS2_PLACEMENT_3D('',#71599,#56946,#56947);
#51383=AXIS2_PLACEMENT_3D('',#71606,#56948,#56949);
#51384=AXIS2_PLACEMENT_3D('',#71609,#56950,#56951);
#51385=AXIS2_PLACEMENT_3D('',#71616,#56952,#56953);
#51386=AXIS2_PLACEMENT_3D('',#71619,#56954,#56955);
#51387=AXIS2_PLACEMENT_3D('',#71626,#56956,#56957);
#51388=AXIS2_PLACEMENT_3D('',#71629,#56958,#56959);
#51389=AXIS2_PLACEMENT_3D('',#71636,#56960,#56961);
#51390=AXIS2_PLACEMENT_3D('',#71639,#56962,#56963);
#51391=AXIS2_PLACEMENT_3D('',#71646,#56964,#56965);
#51392=AXIS2_PLACEMENT_3D('',#71649,#56966,#56967);
#51393=AXIS2_PLACEMENT_3D('',#71656,#56968,#56969);
#51394=AXIS2_PLACEMENT_3D('',#71659,#56970,#56971);
#51395=AXIS2_PLACEMENT_3D('',#71666,#56972,#56973);
#51396=AXIS2_PLACEMENT_3D('',#71669,#56974,#56975);
#51397=AXIS2_PLACEMENT_3D('',#71676,#56976,#56977);
#51398=AXIS2_PLACEMENT_3D('',#71679,#56978,#56979);
#51399=AXIS2_PLACEMENT_3D('',#71686,#56980,#56981);
#51400=AXIS2_PLACEMENT_3D('',#71689,#56982,#56983);
#51401=AXIS2_PLACEMENT_3D('',#71696,#56984,#56985);
#51402=AXIS2_PLACEMENT_3D('',#71699,#56986,#56987);
#51403=AXIS2_PLACEMENT_3D('',#71706,#56988,#56989);
#51404=AXIS2_PLACEMENT_3D('',#71709,#56990,#56991);
#51405=AXIS2_PLACEMENT_3D('',#71716,#56992,#56993);
#51406=AXIS2_PLACEMENT_3D('',#71719,#56994,#56995);
#51407=AXIS2_PLACEMENT_3D('',#71726,#56996,#56997);
#51408=AXIS2_PLACEMENT_3D('',#71729,#56998,#56999);
#51409=AXIS2_PLACEMENT_3D('',#71736,#57000,#57001);
#51410=AXIS2_PLACEMENT_3D('',#71739,#57002,#57003);
#51411=AXIS2_PLACEMENT_3D('',#71746,#57004,#57005);
#51412=AXIS2_PLACEMENT_3D('',#71749,#57006,#57007);
#51413=AXIS2_PLACEMENT_3D('',#71756,#57008,#57009);
#51414=AXIS2_PLACEMENT_3D('',#71759,#57010,#57011);
#51415=AXIS2_PLACEMENT_3D('',#71766,#57012,#57013);
#51416=AXIS2_PLACEMENT_3D('',#71769,#57014,#57015);
#51417=AXIS2_PLACEMENT_3D('',#71776,#57016,#57017);
#51418=AXIS2_PLACEMENT_3D('',#71779,#57018,#57019);
#51419=AXIS2_PLACEMENT_3D('',#71786,#57020,#57021);
#51420=AXIS2_PLACEMENT_3D('',#71789,#57022,#57023);
#51421=AXIS2_PLACEMENT_3D('',#71796,#57024,#57025);
#51422=AXIS2_PLACEMENT_3D('',#71799,#57026,#57027);
#51423=AXIS2_PLACEMENT_3D('',#71806,#57028,#57029);
#51424=AXIS2_PLACEMENT_3D('',#71809,#57030,#57031);
#51425=AXIS2_PLACEMENT_3D('',#71816,#57032,#57033);
#51426=AXIS2_PLACEMENT_3D('',#71819,#57034,#57035);
#51427=AXIS2_PLACEMENT_3D('',#71826,#57036,#57037);
#51428=AXIS2_PLACEMENT_3D('',#71829,#57038,#57039);
#51429=AXIS2_PLACEMENT_3D('',#71836,#57040,#57041);
#51430=AXIS2_PLACEMENT_3D('',#71839,#57042,#57043);
#51431=AXIS2_PLACEMENT_3D('',#71846,#57044,#57045);
#51432=AXIS2_PLACEMENT_3D('',#71849,#57046,#57047);
#51433=AXIS2_PLACEMENT_3D('',#71856,#57048,#57049);
#51434=AXIS2_PLACEMENT_3D('',#71859,#57050,#57051);
#51435=AXIS2_PLACEMENT_3D('',#71866,#57052,#57053);
#51436=AXIS2_PLACEMENT_3D('',#71869,#57054,#57055);
#51437=AXIS2_PLACEMENT_3D('',#71876,#57056,#57057);
#51438=AXIS2_PLACEMENT_3D('',#71879,#57058,#57059);
#51439=AXIS2_PLACEMENT_3D('',#71886,#57060,#57061);
#51440=AXIS2_PLACEMENT_3D('',#71889,#57062,#57063);
#51441=AXIS2_PLACEMENT_3D('',#71896,#57064,#57065);
#51442=AXIS2_PLACEMENT_3D('',#71906,#57068,#57069);
#51443=AXIS2_PLACEMENT_3D('',#71908,#57071,#57072);
#51444=AXIS2_PLACEMENT_3D('',#71918,#57075,#57076);
#51445=AXIS2_PLACEMENT_3D('',#71920,#57078,#57079);
#51446=AXIS2_PLACEMENT_3D('',#71930,#57082,#57083);
#51447=AXIS2_PLACEMENT_3D('',#71932,#57085,#57086);
#51448=AXIS2_PLACEMENT_3D('',#71942,#57089,#57090);
#51449=AXIS2_PLACEMENT_3D('',#71944,#57092,#57093);
#51450=AXIS2_PLACEMENT_3D('',#71954,#57096,#57097);
#51451=AXIS2_PLACEMENT_3D('',#71956,#57099,#57100);
#51452=AXIS2_PLACEMENT_3D('',#71966,#57103,#57104);
#51453=AXIS2_PLACEMENT_3D('',#71968,#57106,#57107);
#51454=AXIS2_PLACEMENT_3D('',#71978,#57110,#57111);
#51455=AXIS2_PLACEMENT_3D('',#71980,#57113,#57114);
#51456=AXIS2_PLACEMENT_3D('',#71990,#57117,#57118);
#51457=AXIS2_PLACEMENT_3D('',#71992,#57120,#57121);
#51458=AXIS2_PLACEMENT_3D('',#72002,#57124,#57125);
#51459=AXIS2_PLACEMENT_3D('',#72004,#57127,#57128);
#51460=AXIS2_PLACEMENT_3D('',#72014,#57131,#57132);
#51461=AXIS2_PLACEMENT_3D('',#72016,#57134,#57135);
#51462=AXIS2_PLACEMENT_3D('',#72026,#57138,#57139);
#51463=AXIS2_PLACEMENT_3D('',#72028,#57141,#57142);
#51464=AXIS2_PLACEMENT_3D('',#72038,#57145,#57146);
#51465=AXIS2_PLACEMENT_3D('',#72040,#57148,#57149);
#51466=AXIS2_PLACEMENT_3D('',#72050,#57152,#57153);
#51467=AXIS2_PLACEMENT_3D('',#72052,#57155,#57156);
#51468=AXIS2_PLACEMENT_3D('',#72062,#57159,#57160);
#51469=AXIS2_PLACEMENT_3D('',#72064,#57162,#57163);
#51470=AXIS2_PLACEMENT_3D('',#72074,#57166,#57167);
#51471=AXIS2_PLACEMENT_3D('',#72076,#57169,#57170);
#51472=AXIS2_PLACEMENT_3D('',#72086,#57173,#57174);
#51473=AXIS2_PLACEMENT_3D('',#72088,#57176,#57177);
#51474=AXIS2_PLACEMENT_3D('',#72098,#57180,#57181);
#51475=AXIS2_PLACEMENT_3D('',#72100,#57183,#57184);
#51476=AXIS2_PLACEMENT_3D('',#72110,#57187,#57188);
#51477=AXIS2_PLACEMENT_3D('',#72112,#57190,#57191);
#51478=AXIS2_PLACEMENT_3D('',#72122,#57194,#57195);
#51479=AXIS2_PLACEMENT_3D('',#72124,#57197,#57198);
#51480=AXIS2_PLACEMENT_3D('',#72134,#57201,#57202);
#51481=AXIS2_PLACEMENT_3D('',#72136,#57204,#57205);
#51482=AXIS2_PLACEMENT_3D('',#72146,#57208,#57209);
#51483=AXIS2_PLACEMENT_3D('',#72148,#57211,#57212);
#51484=AXIS2_PLACEMENT_3D('',#72158,#57215,#57216);
#51485=AXIS2_PLACEMENT_3D('',#72160,#57218,#57219);
#51486=AXIS2_PLACEMENT_3D('',#72170,#57222,#57223);
#51487=AXIS2_PLACEMENT_3D('',#72172,#57225,#57226);
#51488=AXIS2_PLACEMENT_3D('',#72182,#57229,#57230);
#51489=AXIS2_PLACEMENT_3D('',#72184,#57232,#57233);
#51490=AXIS2_PLACEMENT_3D('',#72194,#57236,#57237);
#51491=AXIS2_PLACEMENT_3D('',#72196,#57239,#57240);
#51492=AXIS2_PLACEMENT_3D('',#72206,#57243,#57244);
#51493=AXIS2_PLACEMENT_3D('',#72208,#57246,#57247);
#51494=AXIS2_PLACEMENT_3D('',#72218,#57250,#57251);
#51495=AXIS2_PLACEMENT_3D('',#72220,#57253,#57254);
#51496=AXIS2_PLACEMENT_3D('',#72230,#57257,#57258);
#51497=AXIS2_PLACEMENT_3D('',#72232,#57260,#57261);
#51498=AXIS2_PLACEMENT_3D('',#72242,#57264,#57265);
#51499=AXIS2_PLACEMENT_3D('',#72244,#57267,#57268);
#51500=AXIS2_PLACEMENT_3D('',#72254,#57271,#57272);
#51501=AXIS2_PLACEMENT_3D('',#72256,#57274,#57275);
#51502=AXIS2_PLACEMENT_3D('',#72266,#57278,#57279);
#51503=AXIS2_PLACEMENT_3D('',#72268,#57281,#57282);
#51504=AXIS2_PLACEMENT_3D('',#72278,#57285,#57286);
#51505=AXIS2_PLACEMENT_3D('',#72280,#57288,#57289);
#51506=AXIS2_PLACEMENT_3D('',#72290,#57292,#57293);
#51507=AXIS2_PLACEMENT_3D('',#72292,#57295,#57296);
#51508=AXIS2_PLACEMENT_3D('',#72302,#57299,#57300);
#51509=AXIS2_PLACEMENT_3D('',#72304,#57302,#57303);
#51510=AXIS2_PLACEMENT_3D('',#72314,#57306,#57307);
#51511=AXIS2_PLACEMENT_3D('',#72316,#57309,#57310);
#51512=AXIS2_PLACEMENT_3D('',#72326,#57313,#57314);
#51513=AXIS2_PLACEMENT_3D('',#72328,#57316,#57317);
#51514=AXIS2_PLACEMENT_3D('',#72332,#57320,#57321);
#51515=AXIS2_PLACEMENT_3D('',#72336,#57324,#57325);
#51516=AXIS2_PLACEMENT_3D('',#72340,#57328,#57329);
#51517=AXIS2_PLACEMENT_3D('',#72344,#57332,#57333);
#51518=AXIS2_PLACEMENT_3D('',#72348,#57336,#57337);
#51519=AXIS2_PLACEMENT_3D('',#72352,#57340,#57341);
#51520=AXIS2_PLACEMENT_3D('',#72356,#57344,#57345);
#51521=AXIS2_PLACEMENT_3D('',#72360,#57348,#57349);
#51522=AXIS2_PLACEMENT_3D('',#72364,#57352,#57353);
#51523=AXIS2_PLACEMENT_3D('',#72368,#57356,#57357);
#51524=AXIS2_PLACEMENT_3D('',#72372,#57360,#57361);
#51525=AXIS2_PLACEMENT_3D('',#72376,#57364,#57365);
#51526=AXIS2_PLACEMENT_3D('',#72380,#57368,#57369);
#51527=AXIS2_PLACEMENT_3D('',#72384,#57372,#57373);
#51528=AXIS2_PLACEMENT_3D('',#72388,#57376,#57377);
#51529=AXIS2_PLACEMENT_3D('',#72392,#57380,#57381);
#51530=AXIS2_PLACEMENT_3D('',#72396,#57384,#57385);
#51531=AXIS2_PLACEMENT_3D('',#72400,#57388,#57389);
#51532=AXIS2_PLACEMENT_3D('',#72404,#57392,#57393);
#51533=AXIS2_PLACEMENT_3D('',#72408,#57396,#57397);
#51534=AXIS2_PLACEMENT_3D('',#72412,#57400,#57401);
#51535=AXIS2_PLACEMENT_3D('',#72416,#57404,#57405);
#51536=AXIS2_PLACEMENT_3D('',#72420,#57408,#57409);
#51537=AXIS2_PLACEMENT_3D('',#72424,#57412,#57413);
#51538=AXIS2_PLACEMENT_3D('',#72428,#57416,#57417);
#51539=AXIS2_PLACEMENT_3D('',#72432,#57420,#57421);
#51540=AXIS2_PLACEMENT_3D('',#72436,#57424,#57425);
#51541=AXIS2_PLACEMENT_3D('',#72440,#57428,#57429);
#51542=AXIS2_PLACEMENT_3D('',#72444,#57432,#57433);
#51543=AXIS2_PLACEMENT_3D('',#72448,#57436,#57437);
#51544=AXIS2_PLACEMENT_3D('',#72452,#57440,#57441);
#51545=AXIS2_PLACEMENT_3D('',#72456,#57444,#57445);
#51546=AXIS2_PLACEMENT_3D('',#72460,#57448,#57449);
#51547=AXIS2_PLACEMENT_3D('',#72464,#57452,#57453);
#51548=AXIS2_PLACEMENT_3D('',#72468,#57456,#57457);
#51549=AXIS2_PLACEMENT_3D('',#72472,#57460,#57461);
#51550=AXIS2_PLACEMENT_3D('',#72476,#57463,#57464);
#51551=AXIS2_PLACEMENT_3D('',#72482,#57466,#57467);
#51552=AXIS2_PLACEMENT_3D('',#72486,#57469,#57470);
#51553=AXIS2_PLACEMENT_3D('',#72492,#57472,#57473);
#51554=AXIS2_PLACEMENT_3D('',#72496,#57475,#57476);
#51555=AXIS2_PLACEMENT_3D('',#72502,#57478,#57479);
#51556=AXIS2_PLACEMENT_3D('',#72506,#57481,#57482);
#51557=AXIS2_PLACEMENT_3D('',#72512,#57484,#57485);
#51558=AXIS2_PLACEMENT_3D('',#72516,#57487,#57488);
#51559=AXIS2_PLACEMENT_3D('',#72522,#57490,#57491);
#51560=AXIS2_PLACEMENT_3D('',#72526,#57493,#57494);
#51561=AXIS2_PLACEMENT_3D('',#72532,#57496,#57497);
#51562=AXIS2_PLACEMENT_3D('',#72536,#57499,#57500);
#51563=AXIS2_PLACEMENT_3D('',#72542,#57502,#57503);
#51564=AXIS2_PLACEMENT_3D('',#72546,#57505,#57506);
#51565=AXIS2_PLACEMENT_3D('',#72552,#57508,#57509);
#51566=AXIS2_PLACEMENT_3D('',#72556,#57511,#57512);
#51567=AXIS2_PLACEMENT_3D('',#72562,#57514,#57515);
#51568=AXIS2_PLACEMENT_3D('',#72566,#57517,#57518);
#51569=AXIS2_PLACEMENT_3D('',#72572,#57520,#57521);
#51570=AXIS2_PLACEMENT_3D('',#72576,#57523,#57524);
#51571=AXIS2_PLACEMENT_3D('',#72582,#57526,#57527);
#51572=AXIS2_PLACEMENT_3D('',#72586,#57529,#57530);
#51573=AXIS2_PLACEMENT_3D('',#72592,#57532,#57533);
#51574=AXIS2_PLACEMENT_3D('',#72596,#57535,#57536);
#51575=AXIS2_PLACEMENT_3D('',#72602,#57538,#57539);
#51576=AXIS2_PLACEMENT_3D('',#72606,#57541,#57542);
#51577=AXIS2_PLACEMENT_3D('',#72612,#57544,#57545);
#51578=AXIS2_PLACEMENT_3D('',#72616,#57547,#57548);
#51579=AXIS2_PLACEMENT_3D('',#72622,#57550,#57551);
#51580=AXIS2_PLACEMENT_3D('',#72626,#57553,#57554);
#51581=AXIS2_PLACEMENT_3D('',#72632,#57556,#57557);
#51582=AXIS2_PLACEMENT_3D('',#72636,#57559,#57560);
#51583=AXIS2_PLACEMENT_3D('',#72642,#57562,#57563);
#51584=AXIS2_PLACEMENT_3D('',#72646,#57565,#57566);
#51585=AXIS2_PLACEMENT_3D('',#72652,#57568,#57569);
#51586=AXIS2_PLACEMENT_3D('',#72656,#57571,#57572);
#51587=AXIS2_PLACEMENT_3D('',#72662,#57574,#57575);
#51588=AXIS2_PLACEMENT_3D('',#72666,#57577,#57578);
#51589=AXIS2_PLACEMENT_3D('',#72672,#57580,#57581);
#51590=AXIS2_PLACEMENT_3D('',#72676,#57583,#57584);
#51591=AXIS2_PLACEMENT_3D('',#72682,#57586,#57587);
#51592=AXIS2_PLACEMENT_3D('',#72686,#57589,#57590);
#51593=AXIS2_PLACEMENT_3D('',#72692,#57592,#57593);
#51594=AXIS2_PLACEMENT_3D('',#72696,#57595,#57596);
#51595=AXIS2_PLACEMENT_3D('',#72702,#57598,#57599);
#51596=AXIS2_PLACEMENT_3D('',#72706,#57601,#57602);
#51597=AXIS2_PLACEMENT_3D('',#72712,#57604,#57605);
#51598=AXIS2_PLACEMENT_3D('',#72716,#57607,#57608);
#51599=AXIS2_PLACEMENT_3D('',#72722,#57610,#57611);
#51600=AXIS2_PLACEMENT_3D('',#72726,#57613,#57614);
#51601=AXIS2_PLACEMENT_3D('',#72732,#57616,#57617);
#51602=AXIS2_PLACEMENT_3D('',#72736,#57619,#57620);
#51603=AXIS2_PLACEMENT_3D('',#72742,#57622,#57623);
#51604=AXIS2_PLACEMENT_3D('',#72746,#57625,#57626);
#51605=AXIS2_PLACEMENT_3D('',#72752,#57628,#57629);
#51606=AXIS2_PLACEMENT_3D('',#72756,#57631,#57632);
#51607=AXIS2_PLACEMENT_3D('',#72762,#57634,#57635);
#51608=AXIS2_PLACEMENT_3D('',#72766,#57637,#57638);
#51609=AXIS2_PLACEMENT_3D('',#72772,#57640,#57641);
#51610=AXIS2_PLACEMENT_3D('',#72776,#57643,#57644);
#51611=AXIS2_PLACEMENT_3D('',#72782,#57646,#57647);
#51612=AXIS2_PLACEMENT_3D('',#72786,#57649,#57650);
#51613=AXIS2_PLACEMENT_3D('',#72792,#57652,#57653);
#51614=AXIS2_PLACEMENT_3D('',#72796,#57655,#57656);
#51615=AXIS2_PLACEMENT_3D('',#72802,#57658,#57659);
#51616=AXIS2_PLACEMENT_3D('',#72806,#57661,#57662);
#51617=AXIS2_PLACEMENT_3D('',#72812,#57664,#57665);
#51618=AXIS2_PLACEMENT_3D('',#72816,#57667,#57668);
#51619=AXIS2_PLACEMENT_3D('',#72822,#57670,#57671);
#51620=AXIS2_PLACEMENT_3D('',#72828,#57673,#57674);
#51621=AXIS2_PLACEMENT_3D('',#72832,#57677,#57678);
#51622=AXIS2_PLACEMENT_3D('',#72836,#57681,#57682);
#51623=AXIS2_PLACEMENT_3D('',#72840,#57685,#57686);
#51624=AXIS2_PLACEMENT_3D('',#72844,#57689,#57690);
#51625=AXIS2_PLACEMENT_3D('',#72848,#57693,#57694);
#51626=AXIS2_PLACEMENT_3D('',#72852,#57697,#57698);
#51627=AXIS2_PLACEMENT_3D('',#72856,#57701,#57702);
#51628=AXIS2_PLACEMENT_3D('',#72860,#57705,#57706);
#51629=AXIS2_PLACEMENT_3D('',#72864,#57709,#57710);
#51630=AXIS2_PLACEMENT_3D('',#72868,#57713,#57714);
#51631=AXIS2_PLACEMENT_3D('',#72872,#57717,#57718);
#51632=AXIS2_PLACEMENT_3D('',#72876,#57721,#57722);
#51633=AXIS2_PLACEMENT_3D('',#72880,#57725,#57726);
#51634=AXIS2_PLACEMENT_3D('',#72884,#57729,#57730);
#51635=AXIS2_PLACEMENT_3D('',#72888,#57733,#57734);
#51636=AXIS2_PLACEMENT_3D('',#72892,#57737,#57738);
#51637=AXIS2_PLACEMENT_3D('',#72896,#57741,#57742);
#51638=AXIS2_PLACEMENT_3D('',#72900,#57745,#57746);
#51639=AXIS2_PLACEMENT_3D('',#72904,#57749,#57750);
#51640=AXIS2_PLACEMENT_3D('',#72908,#57753,#57754);
#51641=AXIS2_PLACEMENT_3D('',#72912,#57757,#57758);
#51642=AXIS2_PLACEMENT_3D('',#72916,#57761,#57762);
#51643=AXIS2_PLACEMENT_3D('',#72920,#57765,#57766);
#51644=AXIS2_PLACEMENT_3D('',#72924,#57769,#57770);
#51645=AXIS2_PLACEMENT_3D('',#72928,#57773,#57774);
#51646=AXIS2_PLACEMENT_3D('',#72932,#57777,#57778);
#51647=AXIS2_PLACEMENT_3D('',#72936,#57781,#57782);
#51648=AXIS2_PLACEMENT_3D('',#72940,#57785,#57786);
#51649=AXIS2_PLACEMENT_3D('',#72944,#57789,#57790);
#51650=AXIS2_PLACEMENT_3D('',#72948,#57793,#57794);
#51651=AXIS2_PLACEMENT_3D('',#72952,#57797,#57798);
#51652=AXIS2_PLACEMENT_3D('',#72956,#57801,#57802);
#51653=AXIS2_PLACEMENT_3D('',#72960,#57805,#57806);
#51654=AXIS2_PLACEMENT_3D('',#72964,#57809,#57810);
#51655=AXIS2_PLACEMENT_3D('',#72968,#57813,#57814);
#51656=AXIS2_PLACEMENT_3D('',#72972,#57817,#57818);
#51657=AXIS2_PLACEMENT_3D('',#72978,#57820,#57821);
#51658=AXIS2_PLACEMENT_3D('',#72984,#57823,#57824);
#51659=AXIS2_PLACEMENT_3D('',#72990,#57826,#57827);
#51660=AXIS2_PLACEMENT_3D('',#72996,#57829,#57830);
#51661=AXIS2_PLACEMENT_3D('',#73002,#57832,#57833);
#51662=AXIS2_PLACEMENT_3D('',#73008,#57835,#57836);
#51663=AXIS2_PLACEMENT_3D('',#73014,#57838,#57839);
#51664=AXIS2_PLACEMENT_3D('',#73020,#57841,#57842);
#51665=AXIS2_PLACEMENT_3D('',#73026,#57844,#57845);
#51666=AXIS2_PLACEMENT_3D('',#73032,#57847,#57848);
#51667=AXIS2_PLACEMENT_3D('',#73038,#57850,#57851);
#51668=AXIS2_PLACEMENT_3D('',#73044,#57853,#57854);
#51669=AXIS2_PLACEMENT_3D('',#73050,#57856,#57857);
#51670=AXIS2_PLACEMENT_3D('',#73056,#57859,#57860);
#51671=AXIS2_PLACEMENT_3D('',#73062,#57862,#57863);
#51672=AXIS2_PLACEMENT_3D('',#73068,#57865,#57866);
#51673=AXIS2_PLACEMENT_3D('',#73074,#57868,#57869);
#51674=AXIS2_PLACEMENT_3D('',#73084,#57871,#57872);
#51675=AXIS2_PLACEMENT_3D('',#73090,#57874,#57875);
#51676=AXIS2_PLACEMENT_3D('',#73096,#57877,#57878);
#51677=AXIS2_PLACEMENT_3D('',#73102,#57880,#57881);
#51678=AXIS2_PLACEMENT_3D('',#73108,#57883,#57884);
#51679=AXIS2_PLACEMENT_3D('',#73114,#57886,#57887);
#51680=AXIS2_PLACEMENT_3D('',#73120,#57889,#57890);
#51681=AXIS2_PLACEMENT_3D('',#73126,#57892,#57893);
#51682=AXIS2_PLACEMENT_3D('',#73132,#57895,#57896);
#51683=AXIS2_PLACEMENT_3D('',#73138,#57898,#57899);
#51684=AXIS2_PLACEMENT_3D('',#73144,#57901,#57902);
#51685=AXIS2_PLACEMENT_3D('',#73150,#57904,#57905);
#51686=AXIS2_PLACEMENT_3D('',#73156,#57907,#57908);
#51687=AXIS2_PLACEMENT_3D('',#73162,#57910,#57911);
#51688=AXIS2_PLACEMENT_3D('',#73168,#57913,#57914);
#51689=AXIS2_PLACEMENT_3D('',#73174,#57916,#57917);
#51690=AXIS2_PLACEMENT_3D('',#73180,#57919,#57920);
#51691=AXIS2_PLACEMENT_3D('',#73186,#57922,#57923);
#51692=AXIS2_PLACEMENT_3D('',#73192,#57925,#57926);
#51693=AXIS2_PLACEMENT_3D('',#73196,#57929,#57930);
#51694=AXIS2_PLACEMENT_3D('',#73198,#57931,#57932);
#51695=AXIS2_PLACEMENT_3D('',#73200,#57934,#57935);
#51696=AXIS2_PLACEMENT_3D('',#73202,#57936,#57937);
#51697=AXIS2_PLACEMENT_3D('',#73204,#57939,#57940);
#51698=AXIS2_PLACEMENT_3D('',#73206,#57941,#57942);
#51699=AXIS2_PLACEMENT_3D('',#73208,#57944,#57945);
#51700=AXIS2_PLACEMENT_3D('',#73210,#57946,#57947);
#51701=AXIS2_PLACEMENT_3D('',#73212,#57949,#57950);
#51702=AXIS2_PLACEMENT_3D('',#73214,#57951,#57952);
#51703=AXIS2_PLACEMENT_3D('',#73216,#57954,#57955);
#51704=AXIS2_PLACEMENT_3D('',#73220,#57958,#57959);
#51705=AXIS2_PLACEMENT_3D('',#73222,#57960,#57961);
#51706=AXIS2_PLACEMENT_3D('',#73224,#57963,#57964);
#51707=AXIS2_PLACEMENT_3D('',#73226,#57965,#57966);
#51708=AXIS2_PLACEMENT_3D('',#73228,#57968,#57969);
#51709=AXIS2_PLACEMENT_3D('',#73230,#57970,#57971);
#51710=AXIS2_PLACEMENT_3D('',#73232,#57973,#57974);
#51711=AXIS2_PLACEMENT_3D('',#73234,#57975,#57976);
#51712=AXIS2_PLACEMENT_3D('',#73236,#57978,#57979);
#51713=AXIS2_PLACEMENT_3D('',#73238,#57980,#57981);
#51714=AXIS2_PLACEMENT_3D('',#73240,#57983,#57984);
#51715=AXIS2_PLACEMENT_3D('',#73244,#57987,#57988);
#51716=AXIS2_PLACEMENT_3D('',#73246,#57989,#57990);
#51717=AXIS2_PLACEMENT_3D('',#73250,#57991,#57992);
#51718=AXIS2_PLACEMENT_3D('',#73254,#57995,#57996);
#51719=AXIS2_PLACEMENT_3D('',#73256,#57997,#57998);
#51720=AXIS2_PLACEMENT_3D('',#73258,#58000,#58001);
#51721=AXIS2_PLACEMENT_3D('',#73260,#58002,#58003);
#51722=AXIS2_PLACEMENT_3D('',#73262,#58005,#58006);
#51723=AXIS2_PLACEMENT_3D('',#73264,#58007,#58008);
#51724=AXIS2_PLACEMENT_3D('',#73266,#58010,#58011);
#51725=AXIS2_PLACEMENT_3D('',#73268,#58012,#58013);
#51726=AXIS2_PLACEMENT_3D('',#73270,#58015,#58016);
#51727=AXIS2_PLACEMENT_3D('',#73272,#58017,#58018);
#51728=AXIS2_PLACEMENT_3D('',#73274,#58020,#58021);
#51729=AXIS2_PLACEMENT_3D('',#73278,#58024,#58025);
#51730=AXIS2_PLACEMENT_3D('',#73280,#58026,#58027);
#51731=AXIS2_PLACEMENT_3D('',#73282,#58029,#58030);
#51732=AXIS2_PLACEMENT_3D('',#73284,#58031,#58032);
#51733=AXIS2_PLACEMENT_3D('',#73286,#58034,#58035);
#51734=AXIS2_PLACEMENT_3D('',#73288,#58036,#58037);
#51735=AXIS2_PLACEMENT_3D('',#73290,#58039,#58040);
#51736=AXIS2_PLACEMENT_3D('',#73292,#58041,#58042);
#51737=AXIS2_PLACEMENT_3D('',#73294,#58044,#58045);
#51738=AXIS2_PLACEMENT_3D('',#73296,#58046,#58047);
#51739=AXIS2_PLACEMENT_3D('',#73298,#58049,#58050);
#51740=AXIS2_PLACEMENT_3D('',#73300,#58052,#58053);
#51741=AXIS2_PLACEMENT_3D('',#73304,#58054,#58055);
#51742=AXIS2_PLACEMENT_3D('',#73306,#58056,#58057);
#51743=AXIS2_PLACEMENT_3D('',#73312,#58059,#58060);
#51744=AXIS2_PLACEMENT_3D('',#73316,#58061,#58062);
#51745=AXIS2_PLACEMENT_3D('',#73320,#58063,#58064);
#51746=AXIS2_PLACEMENT_3D('',#73324,#58065,#58066);
#51747=AXIS2_PLACEMENT_3D('',#73328,#58067,#58068);
#51748=AXIS2_PLACEMENT_3D('',#73332,#58069,#58070);
#51749=AXIS2_PLACEMENT_3D('',#73336,#58071,#58072);
#51750=AXIS2_PLACEMENT_3D('',#73340,#58073,#58074);
#51751=AXIS2_PLACEMENT_3D('',#73344,#58075,#58076);
#51752=AXIS2_PLACEMENT_3D('',#73348,#58077,#58078);
#51753=AXIS2_PLACEMENT_3D('',#73352,#58079,#58080);
#51754=AXIS2_PLACEMENT_3D('',#73356,#58081,#58082);
#51755=AXIS2_PLACEMENT_3D('',#73360,#58083,#58084);
#51756=AXIS2_PLACEMENT_3D('',#73364,#58085,#58086);
#51757=AXIS2_PLACEMENT_3D('',#73368,#58087,#58088);
#51758=AXIS2_PLACEMENT_3D('',#73372,#58089,#58090);
#51759=AXIS2_PLACEMENT_3D('',#73376,#58091,#58092);
#51760=AXIS2_PLACEMENT_3D('',#73380,#58093,#58094);
#51761=AXIS2_PLACEMENT_3D('',#73385,#58095,#58096);
#51762=AXIS2_PLACEMENT_3D('',#73386,#58097,#58098);
#51763=AXIS2_PLACEMENT_3D('',#73390,#58099,#58100);
#51764=AXIS2_PLACEMENT_3D('',#73394,#58101,#58102);
#51765=AXIS2_PLACEMENT_3D('',#73398,#58103,#58104);
#51766=AXIS2_PLACEMENT_3D('',#73402,#58105,#58106);
#51767=AXIS2_PLACEMENT_3D('',#73406,#58107,#58108);
#51768=AXIS2_PLACEMENT_3D('',#73410,#58109,#58110);
#51769=AXIS2_PLACEMENT_3D('',#73414,#58111,#58112);
#51770=AXIS2_PLACEMENT_3D('',#73418,#58113,#58114);
#51771=AXIS2_PLACEMENT_3D('',#73422,#58115,#58116);
#51772=AXIS2_PLACEMENT_3D('',#73426,#58117,#58118);
#51773=AXIS2_PLACEMENT_3D('',#73430,#58119,#58120);
#51774=AXIS2_PLACEMENT_3D('',#73434,#58121,#58122);
#51775=AXIS2_PLACEMENT_3D('',#73438,#58123,#58124);
#51776=AXIS2_PLACEMENT_3D('',#73442,#58125,#58126);
#51777=AXIS2_PLACEMENT_3D('',#73446,#58127,#58128);
#51778=AXIS2_PLACEMENT_3D('',#73450,#58129,#58130);
#51779=AXIS2_PLACEMENT_3D('',#73454,#58131,#58132);
#51780=AXIS2_PLACEMENT_3D('',#73456,#58133,#58134);
#51781=AXIS2_PLACEMENT_3D('',#73458,#58135,#58136);
#51782=AXIS2_PLACEMENT_3D('',#73462,#58138,#58139);
#51783=AXIS2_PLACEMENT_3D('',#73464,#58140,#58141);
#51784=AXIS2_PLACEMENT_3D('',#73466,#58142,#58143);
#51785=AXIS2_PLACEMENT_3D('',#73468,#58144,#58145);
#51786=AXIS2_PLACEMENT_3D('',#73470,#58146,#58147);
#51787=AXIS2_PLACEMENT_3D('',#73474,#58149,#58150);
#51788=AXIS2_PLACEMENT_3D('',#73476,#58151,#58152);
#51789=AXIS2_PLACEMENT_3D('',#73478,#58153,#58154);
#51790=AXIS2_PLACEMENT_3D('',#73480,#58155,#58156);
#51791=AXIS2_PLACEMENT_3D('',#73482,#58157,#58158);
#51792=AXIS2_PLACEMENT_3D('',#73484,#58160,#58161);
#51793=AXIS2_PLACEMENT_3D('',#73486,#58163,#58164);
#51794=AXIS2_PLACEMENT_3D('',#73488,#58166,#58167);
#51795=AXIS2_PLACEMENT_3D('',#73490,#58169,#58170);
#51796=AXIS2_PLACEMENT_3D('',#73492,#58172,#58173);
#51797=AXIS2_PLACEMENT_3D('',#73494,#58175,#58176);
#51798=AXIS2_PLACEMENT_3D('',#73496,#58178,#58179);
#51799=AXIS2_PLACEMENT_3D('',#73498,#58181,#58182);
#51800=AXIS2_PLACEMENT_3D('',#73500,#58184,#58185);
#51801=AXIS2_PLACEMENT_3D('',#73502,#58187,#58188);
#51802=AXIS2_PLACEMENT_3D('',#73504,#58190,#58191);
#51803=AXIS2_PLACEMENT_3D('',#73506,#58193,#58194);
#51804=AXIS2_PLACEMENT_3D('',#73508,#58196,#58197);
#51805=AXIS2_PLACEMENT_3D('',#73510,#58199,#58200);
#51806=AXIS2_PLACEMENT_3D('',#73514,#58201,#58202);
#51807=AXIS2_PLACEMENT_3D('',#73518,#58205,#58206);
#51808=AXIS2_PLACEMENT_3D('',#73520,#58207,#58208);
#51809=AXIS2_PLACEMENT_3D('',#73522,#58210,#58211);
#51810=AXIS2_PLACEMENT_3D('',#73524,#58212,#58213);
#51811=AXIS2_PLACEMENT_3D('',#73526,#58215,#58216);
#51812=AXIS2_PLACEMENT_3D('',#73528,#58217,#58218);
#51813=AXIS2_PLACEMENT_3D('',#73530,#58220,#58221);
#51814=AXIS2_PLACEMENT_3D('',#73532,#58222,#58223);
#51815=AXIS2_PLACEMENT_3D('',#73534,#58225,#58226);
#51816=AXIS2_PLACEMENT_3D('',#73536,#58227,#58228);
#51817=AXIS2_PLACEMENT_3D('',#73538,#58230,#58231);
#51818=AXIS2_PLACEMENT_3D('',#73542,#58234,#58235);
#51819=AXIS2_PLACEMENT_3D('',#73544,#58236,#58237);
#51820=AXIS2_PLACEMENT_3D('',#73546,#58239,#58240);
#51821=AXIS2_PLACEMENT_3D('',#73548,#58241,#58242);
#51822=AXIS2_PLACEMENT_3D('',#73550,#58244,#58245);
#51823=AXIS2_PLACEMENT_3D('',#73552,#58246,#58247);
#51824=AXIS2_PLACEMENT_3D('',#73554,#58249,#58250);
#51825=AXIS2_PLACEMENT_3D('',#73556,#58251,#58252);
#51826=AXIS2_PLACEMENT_3D('',#73558,#58254,#58255);
#51827=AXIS2_PLACEMENT_3D('',#73560,#58256,#58257);
#51828=AXIS2_PLACEMENT_3D('',#73562,#58259,#58260);
#51829=AXIS2_PLACEMENT_3D('',#73564,#58262,#58263);
#51830=AXIS2_PLACEMENT_3D('',#73565,#58264,#58265);
#51831=AXIS2_PLACEMENT_3D('',#73567,#58266,#58267);
#51832=AXIS2_PLACEMENT_3D('',#73569,#58268,#58269);
#51833=AXIS2_PLACEMENT_3D('',#73573,#58271,#58272);
#51834=AXIS2_PLACEMENT_3D('',#73575,#58273,#58274);
#51835=AXIS2_PLACEMENT_3D('',#73577,#58275,#58276);
#51836=AXIS2_PLACEMENT_3D('',#73579,#58277,#58278);
#51837=AXIS2_PLACEMENT_3D('',#73581,#58279,#58280);
#51838=AXIS2_PLACEMENT_3D('',#73585,#58282,#58283);
#51839=AXIS2_PLACEMENT_3D('',#73587,#58284,#58285);
#51840=AXIS2_PLACEMENT_3D('',#73589,#58286,#58287);
#51841=AXIS2_PLACEMENT_3D('',#73591,#58288,#58289);
#51842=AXIS2_PLACEMENT_3D('',#73593,#58290,#58291);
#51843=AXIS2_PLACEMENT_3D('',#73595,#58293,#58294);
#51844=AXIS2_PLACEMENT_3D('',#73597,#58296,#58297);
#51845=AXIS2_PLACEMENT_3D('',#73599,#58299,#58300);
#51846=AXIS2_PLACEMENT_3D('',#73601,#58302,#58303);
#51847=AXIS2_PLACEMENT_3D('',#73603,#58305,#58306);
#51848=AXIS2_PLACEMENT_3D('',#73605,#58308,#58309);
#51849=AXIS2_PLACEMENT_3D('',#73607,#58311,#58312);
#51850=AXIS2_PLACEMENT_3D('',#73609,#58314,#58315);
#51851=AXIS2_PLACEMENT_3D('',#73611,#58317,#58318);
#51852=AXIS2_PLACEMENT_3D('',#73613,#58320,#58321);
#51853=AXIS2_PLACEMENT_3D('',#73615,#58323,#58324);
#51854=AXIS2_PLACEMENT_3D('',#73617,#58326,#58327);
#51855=AXIS2_PLACEMENT_3D('',#73619,#58329,#58330);
#51856=AXIS2_PLACEMENT_3D('',#73621,#58332,#58333);
#51857=AXIS2_PLACEMENT_3D('',#73625,#58334,#58335);
#51858=AXIS2_PLACEMENT_3D('',#73629,#58338,#58339);
#51859=AXIS2_PLACEMENT_3D('',#73631,#58340,#58341);
#51860=AXIS2_PLACEMENT_3D('',#73633,#58343,#58344);
#51861=AXIS2_PLACEMENT_3D('',#73635,#58345,#58346);
#51862=AXIS2_PLACEMENT_3D('',#73637,#58348,#58349);
#51863=AXIS2_PLACEMENT_3D('',#73639,#58350,#58351);
#51864=AXIS2_PLACEMENT_3D('',#73641,#58353,#58354);
#51865=AXIS2_PLACEMENT_3D('',#73643,#58355,#58356);
#51866=AXIS2_PLACEMENT_3D('',#73645,#58358,#58359);
#51867=AXIS2_PLACEMENT_3D('',#73647,#58360,#58361);
#51868=AXIS2_PLACEMENT_3D('',#73649,#58363,#58364);
#51869=AXIS2_PLACEMENT_3D('',#73653,#58367,#58368);
#51870=AXIS2_PLACEMENT_3D('',#73655,#58369,#58370);
#51871=AXIS2_PLACEMENT_3D('',#73657,#58372,#58373);
#51872=AXIS2_PLACEMENT_3D('',#73659,#58374,#58375);
#51873=AXIS2_PLACEMENT_3D('',#73661,#58377,#58378);
#51874=AXIS2_PLACEMENT_3D('',#73663,#58379,#58380);
#51875=AXIS2_PLACEMENT_3D('',#73665,#58382,#58383);
#51876=AXIS2_PLACEMENT_3D('',#73667,#58384,#58385);
#51877=AXIS2_PLACEMENT_3D('',#73669,#58387,#58388);
#51878=AXIS2_PLACEMENT_3D('',#73671,#58389,#58390);
#51879=AXIS2_PLACEMENT_3D('',#73673,#58392,#58393);
#51880=AXIS2_PLACEMENT_3D('',#73675,#58395,#58396);
#51881=AXIS2_PLACEMENT_3D('',#73676,#58397,#58398);
#51882=AXIS2_PLACEMENT_3D('',#73678,#58399,#58400);
#51883=AXIS2_PLACEMENT_3D('',#73680,#58401,#58402);
#51884=AXIS2_PLACEMENT_3D('',#73684,#58404,#58405);
#51885=AXIS2_PLACEMENT_3D('',#73686,#58406,#58407);
#51886=AXIS2_PLACEMENT_3D('',#73688,#58408,#58409);
#51887=AXIS2_PLACEMENT_3D('',#73690,#58410,#58411);
#51888=AXIS2_PLACEMENT_3D('',#73692,#58412,#58413);
#51889=AXIS2_PLACEMENT_3D('',#73696,#58415,#58416);
#51890=AXIS2_PLACEMENT_3D('',#73698,#58417,#58418);
#51891=AXIS2_PLACEMENT_3D('',#73700,#58419,#58420);
#51892=AXIS2_PLACEMENT_3D('',#73702,#58421,#58422);
#51893=AXIS2_PLACEMENT_3D('',#73704,#58423,#58424);
#51894=AXIS2_PLACEMENT_3D('',#73706,#58426,#58427);
#51895=AXIS2_PLACEMENT_3D('',#73708,#58429,#58430);
#51896=AXIS2_PLACEMENT_3D('',#73710,#58432,#58433);
#51897=AXIS2_PLACEMENT_3D('',#73712,#58435,#58436);
#51898=AXIS2_PLACEMENT_3D('',#73714,#58438,#58439);
#51899=AXIS2_PLACEMENT_3D('',#73716,#58441,#58442);
#51900=AXIS2_PLACEMENT_3D('',#73718,#58444,#58445);
#51901=AXIS2_PLACEMENT_3D('',#73720,#58447,#58448);
#51902=AXIS2_PLACEMENT_3D('',#73722,#58450,#58451);
#51903=AXIS2_PLACEMENT_3D('',#73724,#58453,#58454);
#51904=AXIS2_PLACEMENT_3D('',#73726,#58456,#58457);
#51905=AXIS2_PLACEMENT_3D('',#73728,#58459,#58460);
#51906=AXIS2_PLACEMENT_3D('',#73730,#58462,#58463);
#51907=AXIS2_PLACEMENT_3D('',#73732,#58465,#58466);
#51908=AXIS2_PLACEMENT_3D('',#73736,#58467,#58468);
#51909=AXIS2_PLACEMENT_3D('',#73740,#58471,#58472);
#51910=AXIS2_PLACEMENT_3D('',#73742,#58473,#58474);
#51911=AXIS2_PLACEMENT_3D('',#73744,#58476,#58477);
#51912=AXIS2_PLACEMENT_3D('',#73746,#58478,#58479);
#51913=AXIS2_PLACEMENT_3D('',#73748,#58481,#58482);
#51914=AXIS2_PLACEMENT_3D('',#73750,#58483,#58484);
#51915=AXIS2_PLACEMENT_3D('',#73752,#58486,#58487);
#51916=AXIS2_PLACEMENT_3D('',#73754,#58488,#58489);
#51917=AXIS2_PLACEMENT_3D('',#73756,#58491,#58492);
#51918=AXIS2_PLACEMENT_3D('',#73758,#58493,#58494);
#51919=AXIS2_PLACEMENT_3D('',#73760,#58496,#58497);
#51920=AXIS2_PLACEMENT_3D('',#73764,#58500,#58501);
#51921=AXIS2_PLACEMENT_3D('',#73766,#58502,#58503);
#51922=AXIS2_PLACEMENT_3D('',#73768,#58505,#58506);
#51923=AXIS2_PLACEMENT_3D('',#73770,#58507,#58508);
#51924=AXIS2_PLACEMENT_3D('',#73772,#58510,#58511);
#51925=AXIS2_PLACEMENT_3D('',#73774,#58512,#58513);
#51926=AXIS2_PLACEMENT_3D('',#73776,#58515,#58516);
#51927=AXIS2_PLACEMENT_3D('',#73778,#58517,#58518);
#51928=AXIS2_PLACEMENT_3D('',#73780,#58520,#58521);
#51929=AXIS2_PLACEMENT_3D('',#73782,#58522,#58523);
#51930=AXIS2_PLACEMENT_3D('',#73784,#58525,#58526);
#51931=AXIS2_PLACEMENT_3D('',#73786,#58528,#58529);
#51932=AXIS2_PLACEMENT_3D('',#73787,#58530,#58531);
#51933=AXIS2_PLACEMENT_3D('',#73789,#58532,#58533);
#51934=AXIS2_PLACEMENT_3D('',#73791,#58534,#58535);
#51935=AXIS2_PLACEMENT_3D('',#73795,#58537,#58538);
#51936=AXIS2_PLACEMENT_3D('',#73797,#58539,#58540);
#51937=AXIS2_PLACEMENT_3D('',#73799,#58541,#58542);
#51938=AXIS2_PLACEMENT_3D('',#73801,#58543,#58544);
#51939=AXIS2_PLACEMENT_3D('',#73803,#58545,#58546);
#51940=AXIS2_PLACEMENT_3D('',#73807,#58548,#58549);
#51941=AXIS2_PLACEMENT_3D('',#73809,#58550,#58551);
#51942=AXIS2_PLACEMENT_3D('',#73811,#58552,#58553);
#51943=AXIS2_PLACEMENT_3D('',#73813,#58554,#58555);
#51944=AXIS2_PLACEMENT_3D('',#73815,#58556,#58557);
#51945=AXIS2_PLACEMENT_3D('',#73817,#58559,#58560);
#51946=AXIS2_PLACEMENT_3D('',#73819,#58562,#58563);
#51947=AXIS2_PLACEMENT_3D('',#73821,#58565,#58566);
#51948=AXIS2_PLACEMENT_3D('',#73823,#58568,#58569);
#51949=AXIS2_PLACEMENT_3D('',#73825,#58571,#58572);
#51950=AXIS2_PLACEMENT_3D('',#73827,#58574,#58575);
#51951=AXIS2_PLACEMENT_3D('',#73829,#58577,#58578);
#51952=AXIS2_PLACEMENT_3D('',#73831,#58580,#58581);
#51953=AXIS2_PLACEMENT_3D('',#73833,#58583,#58584);
#51954=AXIS2_PLACEMENT_3D('',#73835,#58586,#58587);
#51955=AXIS2_PLACEMENT_3D('',#73837,#58589,#58590);
#51956=AXIS2_PLACEMENT_3D('',#73839,#58592,#58593);
#51957=AXIS2_PLACEMENT_3D('',#73841,#58595,#58596);
#51958=AXIS2_PLACEMENT_3D('',#73843,#58598,#58599);
#51959=AXIS2_PLACEMENT_3D('',#73847,#58600,#58601);
#51960=AXIS2_PLACEMENT_3D('',#73851,#58604,#58605);
#51961=AXIS2_PLACEMENT_3D('',#73853,#58606,#58607);
#51962=AXIS2_PLACEMENT_3D('',#73855,#58609,#58610);
#51963=AXIS2_PLACEMENT_3D('',#73857,#58611,#58612);
#51964=AXIS2_PLACEMENT_3D('',#73859,#58614,#58615);
#51965=AXIS2_PLACEMENT_3D('',#73861,#58616,#58617);
#51966=AXIS2_PLACEMENT_3D('',#73863,#58619,#58620);
#51967=AXIS2_PLACEMENT_3D('',#73865,#58621,#58622);
#51968=AXIS2_PLACEMENT_3D('',#73867,#58624,#58625);
#51969=AXIS2_PLACEMENT_3D('',#73869,#58626,#58627);
#51970=AXIS2_PLACEMENT_3D('',#73871,#58629,#58630);
#51971=AXIS2_PLACEMENT_3D('',#73875,#58633,#58634);
#51972=AXIS2_PLACEMENT_3D('',#73877,#58635,#58636);
#51973=AXIS2_PLACEMENT_3D('',#73879,#58638,#58639);
#51974=AXIS2_PLACEMENT_3D('',#73881,#58640,#58641);
#51975=AXIS2_PLACEMENT_3D('',#73883,#58643,#58644);
#51976=AXIS2_PLACEMENT_3D('',#73885,#58645,#58646);
#51977=AXIS2_PLACEMENT_3D('',#73887,#58648,#58649);
#51978=AXIS2_PLACEMENT_3D('',#73889,#58650,#58651);
#51979=AXIS2_PLACEMENT_3D('',#73891,#58653,#58654);
#51980=AXIS2_PLACEMENT_3D('',#73893,#58655,#58656);
#51981=AXIS2_PLACEMENT_3D('',#73895,#58658,#58659);
#51982=AXIS2_PLACEMENT_3D('',#73897,#58661,#58662);
#51983=AXIS2_PLACEMENT_3D('',#73898,#58663,#58664);
#51984=AXIS2_PLACEMENT_3D('',#73900,#58665,#58666);
#51985=AXIS2_PLACEMENT_3D('',#73902,#58667,#58668);
#51986=AXIS2_PLACEMENT_3D('',#73906,#58670,#58671);
#51987=AXIS2_PLACEMENT_3D('',#73908,#58672,#58673);
#51988=AXIS2_PLACEMENT_3D('',#73910,#58674,#58675);
#51989=AXIS2_PLACEMENT_3D('',#73912,#58676,#58677);
#51990=AXIS2_PLACEMENT_3D('',#73914,#58678,#58679);
#51991=AXIS2_PLACEMENT_3D('',#73918,#58681,#58682);
#51992=AXIS2_PLACEMENT_3D('',#73920,#58683,#58684);
#51993=AXIS2_PLACEMENT_3D('',#73922,#58685,#58686);
#51994=AXIS2_PLACEMENT_3D('',#73924,#58687,#58688);
#51995=AXIS2_PLACEMENT_3D('',#73926,#58689,#58690);
#51996=AXIS2_PLACEMENT_3D('',#73928,#58692,#58693);
#51997=AXIS2_PLACEMENT_3D('',#73930,#58695,#58696);
#51998=AXIS2_PLACEMENT_3D('',#73932,#58698,#58699);
#51999=AXIS2_PLACEMENT_3D('',#73934,#58701,#58702);
#52000=AXIS2_PLACEMENT_3D('',#73936,#58704,#58705);
#52001=AXIS2_PLACEMENT_3D('',#73938,#58707,#58708);
#52002=AXIS2_PLACEMENT_3D('',#73940,#58710,#58711);
#52003=AXIS2_PLACEMENT_3D('',#73942,#58713,#58714);
#52004=AXIS2_PLACEMENT_3D('',#73944,#58716,#58717);
#52005=AXIS2_PLACEMENT_3D('',#73946,#58719,#58720);
#52006=AXIS2_PLACEMENT_3D('',#73948,#58722,#58723);
#52007=AXIS2_PLACEMENT_3D('',#73950,#58725,#58726);
#52008=AXIS2_PLACEMENT_3D('',#73952,#58728,#58729);
#52009=AXIS2_PLACEMENT_3D('',#73954,#58731,#58732);
#52010=AXIS2_PLACEMENT_3D('',#73958,#58733,#58734);
#52011=AXIS2_PLACEMENT_3D('',#73962,#58737,#58738);
#52012=AXIS2_PLACEMENT_3D('',#73964,#58739,#58740);
#52013=AXIS2_PLACEMENT_3D('',#73966,#58742,#58743);
#52014=AXIS2_PLACEMENT_3D('',#73968,#58744,#58745);
#52015=AXIS2_PLACEMENT_3D('',#73970,#58747,#58748);
#52016=AXIS2_PLACEMENT_3D('',#73972,#58749,#58750);
#52017=AXIS2_PLACEMENT_3D('',#73974,#58752,#58753);
#52018=AXIS2_PLACEMENT_3D('',#73976,#58754,#58755);
#52019=AXIS2_PLACEMENT_3D('',#73978,#58757,#58758);
#52020=AXIS2_PLACEMENT_3D('',#73980,#58759,#58760);
#52021=AXIS2_PLACEMENT_3D('',#73982,#58762,#58763);
#52022=AXIS2_PLACEMENT_3D('',#73986,#58766,#58767);
#52023=AXIS2_PLACEMENT_3D('',#73988,#58768,#58769);
#52024=AXIS2_PLACEMENT_3D('',#73990,#58771,#58772);
#52025=AXIS2_PLACEMENT_3D('',#73992,#58773,#58774);
#52026=AXIS2_PLACEMENT_3D('',#73994,#58776,#58777);
#52027=AXIS2_PLACEMENT_3D('',#73996,#58778,#58779);
#52028=AXIS2_PLACEMENT_3D('',#73998,#58781,#58782);
#52029=AXIS2_PLACEMENT_3D('',#74000,#58783,#58784);
#52030=AXIS2_PLACEMENT_3D('',#74002,#58786,#58787);
#52031=AXIS2_PLACEMENT_3D('',#74004,#58788,#58789);
#52032=AXIS2_PLACEMENT_3D('',#74006,#58791,#58792);
#52033=AXIS2_PLACEMENT_3D('',#74008,#58794,#58795);
#52034=AXIS2_PLACEMENT_3D('',#74009,#58796,#58797);
#52035=AXIS2_PLACEMENT_3D('',#74011,#58798,#58799);
#52036=AXIS2_PLACEMENT_3D('',#74013,#58800,#58801);
#52037=AXIS2_PLACEMENT_3D('',#74017,#58803,#58804);
#52038=AXIS2_PLACEMENT_3D('',#74019,#58805,#58806);
#52039=AXIS2_PLACEMENT_3D('',#74021,#58807,#58808);
#52040=AXIS2_PLACEMENT_3D('',#74023,#58809,#58810);
#52041=AXIS2_PLACEMENT_3D('',#74025,#58811,#58812);
#52042=AXIS2_PLACEMENT_3D('',#74029,#58814,#58815);
#52043=AXIS2_PLACEMENT_3D('',#74031,#58816,#58817);
#52044=AXIS2_PLACEMENT_3D('',#74033,#58818,#58819);
#52045=AXIS2_PLACEMENT_3D('',#74035,#58820,#58821);
#52046=AXIS2_PLACEMENT_3D('',#74037,#58822,#58823);
#52047=AXIS2_PLACEMENT_3D('',#74039,#58825,#58826);
#52048=AXIS2_PLACEMENT_3D('',#74041,#58828,#58829);
#52049=AXIS2_PLACEMENT_3D('',#74043,#58831,#58832);
#52050=AXIS2_PLACEMENT_3D('',#74045,#58834,#58835);
#52051=AXIS2_PLACEMENT_3D('',#74047,#58837,#58838);
#52052=AXIS2_PLACEMENT_3D('',#74049,#58840,#58841);
#52053=AXIS2_PLACEMENT_3D('',#74051,#58843,#58844);
#52054=AXIS2_PLACEMENT_3D('',#74053,#58846,#58847);
#52055=AXIS2_PLACEMENT_3D('',#74055,#58849,#58850);
#52056=AXIS2_PLACEMENT_3D('',#74057,#58852,#58853);
#52057=AXIS2_PLACEMENT_3D('',#74059,#58855,#58856);
#52058=AXIS2_PLACEMENT_3D('',#74061,#58858,#58859);
#52059=AXIS2_PLACEMENT_3D('',#74063,#58861,#58862);
#52060=AXIS2_PLACEMENT_3D('',#74065,#58864,#58865);
#52061=AXIS2_PLACEMENT_3D('',#74069,#58866,#58867);
#52062=AXIS2_PLACEMENT_3D('',#74073,#58870,#58871);
#52063=AXIS2_PLACEMENT_3D('',#74075,#58872,#58873);
#52064=AXIS2_PLACEMENT_3D('',#74077,#58875,#58876);
#52065=AXIS2_PLACEMENT_3D('',#74079,#58877,#58878);
#52066=AXIS2_PLACEMENT_3D('',#74081,#58880,#58881);
#52067=AXIS2_PLACEMENT_3D('',#74083,#58882,#58883);
#52068=AXIS2_PLACEMENT_3D('',#74085,#58885,#58886);
#52069=AXIS2_PLACEMENT_3D('',#74087,#58887,#58888);
#52070=AXIS2_PLACEMENT_3D('',#74089,#58890,#58891);
#52071=AXIS2_PLACEMENT_3D('',#74091,#58892,#58893);
#52072=AXIS2_PLACEMENT_3D('',#74093,#58895,#58896);
#52073=AXIS2_PLACEMENT_3D('',#74097,#58899,#58900);
#52074=AXIS2_PLACEMENT_3D('',#74099,#58901,#58902);
#52075=AXIS2_PLACEMENT_3D('',#74101,#58904,#58905);
#52076=AXIS2_PLACEMENT_3D('',#74103,#58906,#58907);
#52077=AXIS2_PLACEMENT_3D('',#74105,#58909,#58910);
#52078=AXIS2_PLACEMENT_3D('',#74107,#58911,#58912);
#52079=AXIS2_PLACEMENT_3D('',#74109,#58914,#58915);
#52080=AXIS2_PLACEMENT_3D('',#74111,#58916,#58917);
#52081=AXIS2_PLACEMENT_3D('',#74113,#58919,#58920);
#52082=AXIS2_PLACEMENT_3D('',#74115,#58921,#58922);
#52083=AXIS2_PLACEMENT_3D('',#74117,#58924,#58925);
#52084=AXIS2_PLACEMENT_3D('',#74119,#58927,#58928);
#52085=AXIS2_PLACEMENT_3D('',#74120,#58929,#58930);
#52086=AXIS2_PLACEMENT_3D('',#74122,#58931,#58932);
#52087=AXIS2_PLACEMENT_3D('',#74124,#58933,#58934);
#52088=AXIS2_PLACEMENT_3D('',#74128,#58936,#58937);
#52089=AXIS2_PLACEMENT_3D('',#74130,#58938,#58939);
#52090=AXIS2_PLACEMENT_3D('',#74132,#58940,#58941);
#52091=AXIS2_PLACEMENT_3D('',#74134,#58942,#58943);
#52092=AXIS2_PLACEMENT_3D('',#74136,#58944,#58945);
#52093=AXIS2_PLACEMENT_3D('',#74140,#58947,#58948);
#52094=AXIS2_PLACEMENT_3D('',#74142,#58949,#58950);
#52095=AXIS2_PLACEMENT_3D('',#74144,#58951,#58952);
#52096=AXIS2_PLACEMENT_3D('',#74146,#58953,#58954);
#52097=AXIS2_PLACEMENT_3D('',#74148,#58955,#58956);
#52098=AXIS2_PLACEMENT_3D('',#74150,#58958,#58959);
#52099=AXIS2_PLACEMENT_3D('',#74152,#58961,#58962);
#52100=AXIS2_PLACEMENT_3D('',#74154,#58964,#58965);
#52101=AXIS2_PLACEMENT_3D('',#74156,#58967,#58968);
#52102=AXIS2_PLACEMENT_3D('',#74158,#58970,#58971);
#52103=AXIS2_PLACEMENT_3D('',#74160,#58973,#58974);
#52104=AXIS2_PLACEMENT_3D('',#74162,#58976,#58977);
#52105=AXIS2_PLACEMENT_3D('',#74164,#58979,#58980);
#52106=AXIS2_PLACEMENT_3D('',#74166,#58982,#58983);
#52107=AXIS2_PLACEMENT_3D('',#74168,#58985,#58986);
#52108=AXIS2_PLACEMENT_3D('',#74170,#58988,#58989);
#52109=AXIS2_PLACEMENT_3D('',#74172,#58991,#58992);
#52110=AXIS2_PLACEMENT_3D('',#74174,#58994,#58995);
#52111=AXIS2_PLACEMENT_3D('',#74176,#58997,#58998);
#52112=AXIS2_PLACEMENT_3D('',#74180,#58999,#59000);
#52113=AXIS2_PLACEMENT_3D('',#74184,#59003,#59004);
#52114=AXIS2_PLACEMENT_3D('',#74186,#59005,#59006);
#52115=AXIS2_PLACEMENT_3D('',#74188,#59008,#59009);
#52116=AXIS2_PLACEMENT_3D('',#74190,#59010,#59011);
#52117=AXIS2_PLACEMENT_3D('',#74192,#59013,#59014);
#52118=AXIS2_PLACEMENT_3D('',#74194,#59015,#59016);
#52119=AXIS2_PLACEMENT_3D('',#74196,#59018,#59019);
#52120=AXIS2_PLACEMENT_3D('',#74198,#59020,#59021);
#52121=AXIS2_PLACEMENT_3D('',#74200,#59023,#59024);
#52122=AXIS2_PLACEMENT_3D('',#74202,#59025,#59026);
#52123=AXIS2_PLACEMENT_3D('',#74204,#59028,#59029);
#52124=AXIS2_PLACEMENT_3D('',#74208,#59032,#59033);
#52125=AXIS2_PLACEMENT_3D('',#74210,#59034,#59035);
#52126=AXIS2_PLACEMENT_3D('',#74212,#59037,#59038);
#52127=AXIS2_PLACEMENT_3D('',#74214,#59039,#59040);
#52128=AXIS2_PLACEMENT_3D('',#74216,#59042,#59043);
#52129=AXIS2_PLACEMENT_3D('',#74218,#59044,#59045);
#52130=AXIS2_PLACEMENT_3D('',#74220,#59047,#59048);
#52131=AXIS2_PLACEMENT_3D('',#74222,#59049,#59050);
#52132=AXIS2_PLACEMENT_3D('',#74224,#59052,#59053);
#52133=AXIS2_PLACEMENT_3D('',#74226,#59054,#59055);
#52134=AXIS2_PLACEMENT_3D('',#74228,#59057,#59058);
#52135=AXIS2_PLACEMENT_3D('',#74230,#59060,#59061);
#52136=AXIS2_PLACEMENT_3D('',#74231,#59062,#59063);
#52137=AXIS2_PLACEMENT_3D('',#74233,#59064,#59065);
#52138=AXIS2_PLACEMENT_3D('',#74235,#59066,#59067);
#52139=AXIS2_PLACEMENT_3D('',#74239,#59069,#59070);
#52140=AXIS2_PLACEMENT_3D('',#74241,#59071,#59072);
#52141=AXIS2_PLACEMENT_3D('',#74243,#59073,#59074);
#52142=AXIS2_PLACEMENT_3D('',#74245,#59075,#59076);
#52143=AXIS2_PLACEMENT_3D('',#74247,#59077,#59078);
#52144=AXIS2_PLACEMENT_3D('',#74251,#59080,#59081);
#52145=AXIS2_PLACEMENT_3D('',#74253,#59082,#59083);
#52146=AXIS2_PLACEMENT_3D('',#74255,#59084,#59085);
#52147=AXIS2_PLACEMENT_3D('',#74257,#59086,#59087);
#52148=AXIS2_PLACEMENT_3D('',#74259,#59088,#59089);
#52149=AXIS2_PLACEMENT_3D('',#74261,#59091,#59092);
#52150=AXIS2_PLACEMENT_3D('',#74263,#59094,#59095);
#52151=AXIS2_PLACEMENT_3D('',#74265,#59097,#59098);
#52152=AXIS2_PLACEMENT_3D('',#74267,#59100,#59101);
#52153=AXIS2_PLACEMENT_3D('',#74269,#59103,#59104);
#52154=AXIS2_PLACEMENT_3D('',#74271,#59106,#59107);
#52155=AXIS2_PLACEMENT_3D('',#74273,#59109,#59110);
#52156=AXIS2_PLACEMENT_3D('',#74275,#59112,#59113);
#52157=AXIS2_PLACEMENT_3D('',#74277,#59115,#59116);
#52158=AXIS2_PLACEMENT_3D('',#74279,#59118,#59119);
#52159=AXIS2_PLACEMENT_3D('',#74281,#59121,#59122);
#52160=AXIS2_PLACEMENT_3D('',#74283,#59124,#59125);
#52161=AXIS2_PLACEMENT_3D('',#74285,#59127,#59128);
#52162=AXIS2_PLACEMENT_3D('',#74287,#59130,#59131);
#52163=AXIS2_PLACEMENT_3D('',#74291,#59132,#59133);
#52164=AXIS2_PLACEMENT_3D('',#74295,#59136,#59137);
#52165=AXIS2_PLACEMENT_3D('',#74297,#59138,#59139);
#52166=AXIS2_PLACEMENT_3D('',#74299,#59141,#59142);
#52167=AXIS2_PLACEMENT_3D('',#74301,#59143,#59144);
#52168=AXIS2_PLACEMENT_3D('',#74303,#59146,#59147);
#52169=AXIS2_PLACEMENT_3D('',#74305,#59148,#59149);
#52170=AXIS2_PLACEMENT_3D('',#74307,#59151,#59152);
#52171=AXIS2_PLACEMENT_3D('',#74309,#59153,#59154);
#52172=AXIS2_PLACEMENT_3D('',#74311,#59156,#59157);
#52173=AXIS2_PLACEMENT_3D('',#74313,#59158,#59159);
#52174=AXIS2_PLACEMENT_3D('',#74315,#59161,#59162);
#52175=AXIS2_PLACEMENT_3D('',#74319,#59165,#59166);
#52176=AXIS2_PLACEMENT_3D('',#74321,#59167,#59168);
#52177=AXIS2_PLACEMENT_3D('',#74323,#59170,#59171);
#52178=AXIS2_PLACEMENT_3D('',#74325,#59172,#59173);
#52179=AXIS2_PLACEMENT_3D('',#74327,#59175,#59176);
#52180=AXIS2_PLACEMENT_3D('',#74329,#59177,#59178);
#52181=AXIS2_PLACEMENT_3D('',#74331,#59180,#59181);
#52182=AXIS2_PLACEMENT_3D('',#74333,#59182,#59183);
#52183=AXIS2_PLACEMENT_3D('',#74335,#59185,#59186);
#52184=AXIS2_PLACEMENT_3D('',#74337,#59187,#59188);
#52185=AXIS2_PLACEMENT_3D('',#74339,#59190,#59191);
#52186=AXIS2_PLACEMENT_3D('',#74341,#59193,#59194);
#52187=AXIS2_PLACEMENT_3D('',#74342,#59195,#59196);
#52188=AXIS2_PLACEMENT_3D('',#74344,#59197,#59198);
#52189=AXIS2_PLACEMENT_3D('',#74346,#59199,#59200);
#52190=AXIS2_PLACEMENT_3D('',#74350,#59202,#59203);
#52191=AXIS2_PLACEMENT_3D('',#74352,#59204,#59205);
#52192=AXIS2_PLACEMENT_3D('',#74354,#59206,#59207);
#52193=AXIS2_PLACEMENT_3D('',#74356,#59208,#59209);
#52194=AXIS2_PLACEMENT_3D('',#74358,#59210,#59211);
#52195=AXIS2_PLACEMENT_3D('',#74362,#59213,#59214);
#52196=AXIS2_PLACEMENT_3D('',#74364,#59215,#59216);
#52197=AXIS2_PLACEMENT_3D('',#74366,#59217,#59218);
#52198=AXIS2_PLACEMENT_3D('',#74368,#59219,#59220);
#52199=AXIS2_PLACEMENT_3D('',#74370,#59221,#59222);
#52200=AXIS2_PLACEMENT_3D('',#74372,#59224,#59225);
#52201=AXIS2_PLACEMENT_3D('',#74374,#59227,#59228);
#52202=AXIS2_PLACEMENT_3D('',#74376,#59230,#59231);
#52203=AXIS2_PLACEMENT_3D('',#74378,#59233,#59234);
#52204=AXIS2_PLACEMENT_3D('',#74380,#59236,#59237);
#52205=AXIS2_PLACEMENT_3D('',#74382,#59239,#59240);
#52206=AXIS2_PLACEMENT_3D('',#74384,#59242,#59243);
#52207=AXIS2_PLACEMENT_3D('',#74386,#59245,#59246);
#52208=AXIS2_PLACEMENT_3D('',#74388,#59248,#59249);
#52209=AXIS2_PLACEMENT_3D('',#74390,#59251,#59252);
#52210=AXIS2_PLACEMENT_3D('',#74392,#59254,#59255);
#52211=AXIS2_PLACEMENT_3D('',#74394,#59257,#59258);
#52212=AXIS2_PLACEMENT_3D('',#74396,#59260,#59261);
#52213=AXIS2_PLACEMENT_3D('',#74398,#59263,#59264);
#52214=AXIS2_PLACEMENT_3D('',#74402,#59265,#59266);
#52215=AXIS2_PLACEMENT_3D('',#74406,#59269,#59270);
#52216=AXIS2_PLACEMENT_3D('',#74408,#59271,#59272);
#52217=AXIS2_PLACEMENT_3D('',#74410,#59274,#59275);
#52218=AXIS2_PLACEMENT_3D('',#74412,#59276,#59277);
#52219=AXIS2_PLACEMENT_3D('',#74414,#59279,#59280);
#52220=AXIS2_PLACEMENT_3D('',#74416,#59281,#59282);
#52221=AXIS2_PLACEMENT_3D('',#74418,#59284,#59285);
#52222=AXIS2_PLACEMENT_3D('',#74420,#59286,#59287);
#52223=AXIS2_PLACEMENT_3D('',#74422,#59289,#59290);
#52224=AXIS2_PLACEMENT_3D('',#74424,#59291,#59292);
#52225=AXIS2_PLACEMENT_3D('',#74426,#59294,#59295);
#52226=AXIS2_PLACEMENT_3D('',#74430,#59298,#59299);
#52227=AXIS2_PLACEMENT_3D('',#74432,#59300,#59301);
#52228=AXIS2_PLACEMENT_3D('',#74434,#59303,#59304);
#52229=AXIS2_PLACEMENT_3D('',#74436,#59305,#59306);
#52230=AXIS2_PLACEMENT_3D('',#74438,#59308,#59309);
#52231=AXIS2_PLACEMENT_3D('',#74440,#59310,#59311);
#52232=AXIS2_PLACEMENT_3D('',#74442,#59313,#59314);
#52233=AXIS2_PLACEMENT_3D('',#74444,#59315,#59316);
#52234=AXIS2_PLACEMENT_3D('',#74446,#59318,#59319);
#52235=AXIS2_PLACEMENT_3D('',#74448,#59320,#59321);
#52236=AXIS2_PLACEMENT_3D('',#74450,#59323,#59324);
#52237=AXIS2_PLACEMENT_3D('',#74452,#59326,#59327);
#52238=AXIS2_PLACEMENT_3D('',#74453,#59328,#59329);
#52239=AXIS2_PLACEMENT_3D('',#74455,#59330,#59331);
#52240=AXIS2_PLACEMENT_3D('',#74457,#59332,#59333);
#52241=AXIS2_PLACEMENT_3D('',#74461,#59335,#59336);
#52242=AXIS2_PLACEMENT_3D('',#74463,#59337,#59338);
#52243=AXIS2_PLACEMENT_3D('',#74465,#59339,#59340);
#52244=AXIS2_PLACEMENT_3D('',#74467,#59341,#59342);
#52245=AXIS2_PLACEMENT_3D('',#74469,#59343,#59344);
#52246=AXIS2_PLACEMENT_3D('',#74473,#59346,#59347);
#52247=AXIS2_PLACEMENT_3D('',#74475,#59348,#59349);
#52248=AXIS2_PLACEMENT_3D('',#74477,#59350,#59351);
#52249=AXIS2_PLACEMENT_3D('',#74479,#59352,#59353);
#52250=AXIS2_PLACEMENT_3D('',#74481,#59354,#59355);
#52251=AXIS2_PLACEMENT_3D('',#74483,#59357,#59358);
#52252=AXIS2_PLACEMENT_3D('',#74485,#59360,#59361);
#52253=AXIS2_PLACEMENT_3D('',#74487,#59363,#59364);
#52254=AXIS2_PLACEMENT_3D('',#74489,#59366,#59367);
#52255=AXIS2_PLACEMENT_3D('',#74491,#59369,#59370);
#52256=AXIS2_PLACEMENT_3D('',#74493,#59372,#59373);
#52257=AXIS2_PLACEMENT_3D('',#74495,#59375,#59376);
#52258=AXIS2_PLACEMENT_3D('',#74497,#59378,#59379);
#52259=AXIS2_PLACEMENT_3D('',#74499,#59381,#59382);
#52260=AXIS2_PLACEMENT_3D('',#74501,#59384,#59385);
#52261=AXIS2_PLACEMENT_3D('',#74503,#59387,#59388);
#52262=AXIS2_PLACEMENT_3D('',#74505,#59390,#59391);
#52263=AXIS2_PLACEMENT_3D('',#74507,#59393,#59394);
#52264=AXIS2_PLACEMENT_3D('',#74509,#59396,#59397);
#52265=AXIS2_PLACEMENT_3D('',#74513,#59398,#59399);
#52266=AXIS2_PLACEMENT_3D('',#74517,#59402,#59403);
#52267=AXIS2_PLACEMENT_3D('',#74519,#59404,#59405);
#52268=AXIS2_PLACEMENT_3D('',#74521,#59407,#59408);
#52269=AXIS2_PLACEMENT_3D('',#74523,#59409,#59410);
#52270=AXIS2_PLACEMENT_3D('',#74525,#59412,#59413);
#52271=AXIS2_PLACEMENT_3D('',#74527,#59414,#59415);
#52272=AXIS2_PLACEMENT_3D('',#74529,#59417,#59418);
#52273=AXIS2_PLACEMENT_3D('',#74531,#59419,#59420);
#52274=AXIS2_PLACEMENT_3D('',#74533,#59422,#59423);
#52275=AXIS2_PLACEMENT_3D('',#74535,#59424,#59425);
#52276=AXIS2_PLACEMENT_3D('',#74537,#59427,#59428);
#52277=AXIS2_PLACEMENT_3D('',#74541,#59431,#59432);
#52278=AXIS2_PLACEMENT_3D('',#74543,#59433,#59434);
#52279=AXIS2_PLACEMENT_3D('',#74545,#59436,#59437);
#52280=AXIS2_PLACEMENT_3D('',#74547,#59438,#59439);
#52281=AXIS2_PLACEMENT_3D('',#74549,#59441,#59442);
#52282=AXIS2_PLACEMENT_3D('',#74551,#59443,#59444);
#52283=AXIS2_PLACEMENT_3D('',#74553,#59446,#59447);
#52284=AXIS2_PLACEMENT_3D('',#74555,#59448,#59449);
#52285=AXIS2_PLACEMENT_3D('',#74557,#59451,#59452);
#52286=AXIS2_PLACEMENT_3D('',#74559,#59453,#59454);
#52287=AXIS2_PLACEMENT_3D('',#74561,#59456,#59457);
#52288=AXIS2_PLACEMENT_3D('',#74563,#59459,#59460);
#52289=AXIS2_PLACEMENT_3D('',#74564,#59461,#59462);
#52290=AXIS2_PLACEMENT_3D('',#74566,#59463,#59464);
#52291=AXIS2_PLACEMENT_3D('',#74568,#59465,#59466);
#52292=AXIS2_PLACEMENT_3D('',#74572,#59468,#59469);
#52293=AXIS2_PLACEMENT_3D('',#74574,#59470,#59471);
#52294=AXIS2_PLACEMENT_3D('',#74576,#59472,#59473);
#52295=AXIS2_PLACEMENT_3D('',#74578,#59474,#59475);
#52296=AXIS2_PLACEMENT_3D('',#74580,#59476,#59477);
#52297=AXIS2_PLACEMENT_3D('',#74584,#59479,#59480);
#52298=AXIS2_PLACEMENT_3D('',#74586,#59481,#59482);
#52299=AXIS2_PLACEMENT_3D('',#74588,#59483,#59484);
#52300=AXIS2_PLACEMENT_3D('',#74590,#59485,#59486);
#52301=AXIS2_PLACEMENT_3D('',#74592,#59487,#59488);
#52302=AXIS2_PLACEMENT_3D('',#74594,#59490,#59491);
#52303=AXIS2_PLACEMENT_3D('',#74596,#59493,#59494);
#52304=AXIS2_PLACEMENT_3D('',#74598,#59496,#59497);
#52305=AXIS2_PLACEMENT_3D('',#74600,#59499,#59500);
#52306=AXIS2_PLACEMENT_3D('',#74602,#59502,#59503);
#52307=AXIS2_PLACEMENT_3D('',#74604,#59505,#59506);
#52308=AXIS2_PLACEMENT_3D('',#74606,#59508,#59509);
#52309=AXIS2_PLACEMENT_3D('',#74608,#59511,#59512);
#52310=AXIS2_PLACEMENT_3D('',#74610,#59514,#59515);
#52311=AXIS2_PLACEMENT_3D('',#74612,#59517,#59518);
#52312=AXIS2_PLACEMENT_3D('',#74614,#59520,#59521);
#52313=AXIS2_PLACEMENT_3D('',#74616,#59523,#59524);
#52314=AXIS2_PLACEMENT_3D('',#74618,#59526,#59527);
#52315=AXIS2_PLACEMENT_3D('',#74620,#59529,#59530);
#52316=AXIS2_PLACEMENT_3D('',#74624,#59531,#59532);
#52317=AXIS2_PLACEMENT_3D('',#74628,#59535,#59536);
#52318=AXIS2_PLACEMENT_3D('',#74630,#59537,#59538);
#52319=AXIS2_PLACEMENT_3D('',#74632,#59540,#59541);
#52320=AXIS2_PLACEMENT_3D('',#74634,#59542,#59543);
#52321=AXIS2_PLACEMENT_3D('',#74636,#59545,#59546);
#52322=AXIS2_PLACEMENT_3D('',#74638,#59547,#59548);
#52323=AXIS2_PLACEMENT_3D('',#74640,#59550,#59551);
#52324=AXIS2_PLACEMENT_3D('',#74642,#59552,#59553);
#52325=AXIS2_PLACEMENT_3D('',#74644,#59555,#59556);
#52326=AXIS2_PLACEMENT_3D('',#74646,#59557,#59558);
#52327=AXIS2_PLACEMENT_3D('',#74648,#59560,#59561);
#52328=AXIS2_PLACEMENT_3D('',#74652,#59564,#59565);
#52329=AXIS2_PLACEMENT_3D('',#74654,#59566,#59567);
#52330=AXIS2_PLACEMENT_3D('',#74656,#59569,#59570);
#52331=AXIS2_PLACEMENT_3D('',#74658,#59571,#59572);
#52332=AXIS2_PLACEMENT_3D('',#74660,#59574,#59575);
#52333=AXIS2_PLACEMENT_3D('',#74662,#59576,#59577);
#52334=AXIS2_PLACEMENT_3D('',#74664,#59579,#59580);
#52335=AXIS2_PLACEMENT_3D('',#74666,#59581,#59582);
#52336=AXIS2_PLACEMENT_3D('',#74668,#59584,#59585);
#52337=AXIS2_PLACEMENT_3D('',#74670,#59586,#59587);
#52338=AXIS2_PLACEMENT_3D('',#74672,#59589,#59590);
#52339=AXIS2_PLACEMENT_3D('',#74674,#59592,#59593);
#52340=AXIS2_PLACEMENT_3D('',#74675,#59594,#59595);
#52341=AXIS2_PLACEMENT_3D('',#74677,#59596,#59597);
#52342=AXIS2_PLACEMENT_3D('',#74679,#59598,#59599);
#52343=AXIS2_PLACEMENT_3D('',#74683,#59601,#59602);
#52344=AXIS2_PLACEMENT_3D('',#74685,#59603,#59604);
#52345=AXIS2_PLACEMENT_3D('',#74687,#59605,#59606);
#52346=AXIS2_PLACEMENT_3D('',#74689,#59607,#59608);
#52347=AXIS2_PLACEMENT_3D('',#74691,#59609,#59610);
#52348=AXIS2_PLACEMENT_3D('',#74695,#59612,#59613);
#52349=AXIS2_PLACEMENT_3D('',#74697,#59614,#59615);
#52350=AXIS2_PLACEMENT_3D('',#74699,#59616,#59617);
#52351=AXIS2_PLACEMENT_3D('',#74701,#59618,#59619);
#52352=AXIS2_PLACEMENT_3D('',#74703,#59620,#59621);
#52353=AXIS2_PLACEMENT_3D('',#74705,#59623,#59624);
#52354=AXIS2_PLACEMENT_3D('',#74707,#59626,#59627);
#52355=AXIS2_PLACEMENT_3D('',#74709,#59629,#59630);
#52356=AXIS2_PLACEMENT_3D('',#74711,#59632,#59633);
#52357=AXIS2_PLACEMENT_3D('',#74713,#59635,#59636);
#52358=AXIS2_PLACEMENT_3D('',#74715,#59638,#59639);
#52359=AXIS2_PLACEMENT_3D('',#74717,#59641,#59642);
#52360=AXIS2_PLACEMENT_3D('',#74719,#59644,#59645);
#52361=AXIS2_PLACEMENT_3D('',#74721,#59647,#59648);
#52362=AXIS2_PLACEMENT_3D('',#74723,#59650,#59651);
#52363=AXIS2_PLACEMENT_3D('',#74725,#59653,#59654);
#52364=AXIS2_PLACEMENT_3D('',#74727,#59656,#59657);
#52365=AXIS2_PLACEMENT_3D('',#74729,#59659,#59660);
#52366=AXIS2_PLACEMENT_3D('',#74731,#59662,#59663);
#52367=AXIS2_PLACEMENT_3D('',#74735,#59664,#59665);
#52368=AXIS2_PLACEMENT_3D('',#74739,#59668,#59669);
#52369=AXIS2_PLACEMENT_3D('',#74741,#59670,#59671);
#52370=AXIS2_PLACEMENT_3D('',#74743,#59673,#59674);
#52371=AXIS2_PLACEMENT_3D('',#74745,#59675,#59676);
#52372=AXIS2_PLACEMENT_3D('',#74747,#59678,#59679);
#52373=AXIS2_PLACEMENT_3D('',#74749,#59680,#59681);
#52374=AXIS2_PLACEMENT_3D('',#74751,#59683,#59684);
#52375=AXIS2_PLACEMENT_3D('',#74753,#59685,#59686);
#52376=AXIS2_PLACEMENT_3D('',#74755,#59688,#59689);
#52377=AXIS2_PLACEMENT_3D('',#74757,#59690,#59691);
#52378=AXIS2_PLACEMENT_3D('',#74759,#59693,#59694);
#52379=AXIS2_PLACEMENT_3D('',#74763,#59697,#59698);
#52380=AXIS2_PLACEMENT_3D('',#74765,#59699,#59700);
#52381=AXIS2_PLACEMENT_3D('',#74767,#59702,#59703);
#52382=AXIS2_PLACEMENT_3D('',#74769,#59704,#59705);
#52383=AXIS2_PLACEMENT_3D('',#74771,#59707,#59708);
#52384=AXIS2_PLACEMENT_3D('',#74773,#59709,#59710);
#52385=AXIS2_PLACEMENT_3D('',#74775,#59712,#59713);
#52386=AXIS2_PLACEMENT_3D('',#74777,#59714,#59715);
#52387=AXIS2_PLACEMENT_3D('',#74779,#59717,#59718);
#52388=AXIS2_PLACEMENT_3D('',#74781,#59719,#59720);
#52389=AXIS2_PLACEMENT_3D('',#74783,#59722,#59723);
#52390=AXIS2_PLACEMENT_3D('',#74785,#59725,#59726);
#52391=AXIS2_PLACEMENT_3D('',#74786,#59727,#59728);
#52392=AXIS2_PLACEMENT_3D('',#74788,#59729,#59730);
#52393=AXIS2_PLACEMENT_3D('',#74790,#59731,#59732);
#52394=AXIS2_PLACEMENT_3D('',#74794,#59734,#59735);
#52395=AXIS2_PLACEMENT_3D('',#74796,#59736,#59737);
#52396=AXIS2_PLACEMENT_3D('',#74798,#59738,#59739);
#52397=AXIS2_PLACEMENT_3D('',#74800,#59740,#59741);
#52398=AXIS2_PLACEMENT_3D('',#74802,#59742,#59743);
#52399=AXIS2_PLACEMENT_3D('',#74806,#59745,#59746);
#52400=AXIS2_PLACEMENT_3D('',#74808,#59747,#59748);
#52401=AXIS2_PLACEMENT_3D('',#74810,#59749,#59750);
#52402=AXIS2_PLACEMENT_3D('',#74812,#59751,#59752);
#52403=AXIS2_PLACEMENT_3D('',#74814,#59753,#59754);
#52404=AXIS2_PLACEMENT_3D('',#74816,#59756,#59757);
#52405=AXIS2_PLACEMENT_3D('',#74818,#59759,#59760);
#52406=AXIS2_PLACEMENT_3D('',#74820,#59762,#59763);
#52407=AXIS2_PLACEMENT_3D('',#74822,#59765,#59766);
#52408=AXIS2_PLACEMENT_3D('',#74824,#59768,#59769);
#52409=AXIS2_PLACEMENT_3D('',#74826,#59771,#59772);
#52410=AXIS2_PLACEMENT_3D('',#74828,#59774,#59775);
#52411=AXIS2_PLACEMENT_3D('',#74830,#59777,#59778);
#52412=AXIS2_PLACEMENT_3D('',#74832,#59780,#59781);
#52413=AXIS2_PLACEMENT_3D('',#74834,#59783,#59784);
#52414=AXIS2_PLACEMENT_3D('',#74836,#59786,#59787);
#52415=AXIS2_PLACEMENT_3D('',#74838,#59789,#59790);
#52416=AXIS2_PLACEMENT_3D('',#74840,#59792,#59793);
#52417=AXIS2_PLACEMENT_3D('',#74842,#59795,#59796);
#52418=AXIS2_PLACEMENT_3D('',#74846,#59797,#59798);
#52419=AXIS2_PLACEMENT_3D('',#74850,#59801,#59802);
#52420=AXIS2_PLACEMENT_3D('',#74852,#59803,#59804);
#52421=AXIS2_PLACEMENT_3D('',#74854,#59806,#59807);
#52422=AXIS2_PLACEMENT_3D('',#74856,#59808,#59809);
#52423=AXIS2_PLACEMENT_3D('',#74858,#59811,#59812);
#52424=AXIS2_PLACEMENT_3D('',#74860,#59813,#59814);
#52425=AXIS2_PLACEMENT_3D('',#74862,#59816,#59817);
#52426=AXIS2_PLACEMENT_3D('',#74864,#59818,#59819);
#52427=AXIS2_PLACEMENT_3D('',#74866,#59821,#59822);
#52428=AXIS2_PLACEMENT_3D('',#74868,#59823,#59824);
#52429=AXIS2_PLACEMENT_3D('',#74870,#59826,#59827);
#52430=AXIS2_PLACEMENT_3D('',#74874,#59830,#59831);
#52431=AXIS2_PLACEMENT_3D('',#74876,#59832,#59833);
#52432=AXIS2_PLACEMENT_3D('',#74878,#59835,#59836);
#52433=AXIS2_PLACEMENT_3D('',#74880,#59837,#59838);
#52434=AXIS2_PLACEMENT_3D('',#74882,#59840,#59841);
#52435=AXIS2_PLACEMENT_3D('',#74884,#59842,#59843);
#52436=AXIS2_PLACEMENT_3D('',#74886,#59845,#59846);
#52437=AXIS2_PLACEMENT_3D('',#74888,#59847,#59848);
#52438=AXIS2_PLACEMENT_3D('',#74890,#59850,#59851);
#52439=AXIS2_PLACEMENT_3D('',#74892,#59852,#59853);
#52440=AXIS2_PLACEMENT_3D('',#74894,#59855,#59856);
#52441=AXIS2_PLACEMENT_3D('',#74896,#59858,#59859);
#52442=AXIS2_PLACEMENT_3D('',#74897,#59860,#59861);
#52443=AXIS2_PLACEMENT_3D('',#74899,#59862,#59863);
#52444=AXIS2_PLACEMENT_3D('',#74901,#59864,#59865);
#52445=AXIS2_PLACEMENT_3D('',#74905,#59867,#59868);
#52446=AXIS2_PLACEMENT_3D('',#74907,#59869,#59870);
#52447=AXIS2_PLACEMENT_3D('',#74909,#59871,#59872);
#52448=AXIS2_PLACEMENT_3D('',#74911,#59873,#59874);
#52449=AXIS2_PLACEMENT_3D('',#74913,#59875,#59876);
#52450=AXIS2_PLACEMENT_3D('',#74917,#59878,#59879);
#52451=AXIS2_PLACEMENT_3D('',#74919,#59880,#59881);
#52452=AXIS2_PLACEMENT_3D('',#74921,#59882,#59883);
#52453=AXIS2_PLACEMENT_3D('',#74923,#59884,#59885);
#52454=AXIS2_PLACEMENT_3D('',#74925,#59886,#59887);
#52455=AXIS2_PLACEMENT_3D('',#74927,#59889,#59890);
#52456=AXIS2_PLACEMENT_3D('',#74929,#59892,#59893);
#52457=AXIS2_PLACEMENT_3D('',#74931,#59895,#59896);
#52458=AXIS2_PLACEMENT_3D('',#74933,#59898,#59899);
#52459=AXIS2_PLACEMENT_3D('',#74935,#59901,#59902);
#52460=AXIS2_PLACEMENT_3D('',#74937,#59904,#59905);
#52461=AXIS2_PLACEMENT_3D('',#74939,#59907,#59908);
#52462=AXIS2_PLACEMENT_3D('',#74941,#59910,#59911);
#52463=AXIS2_PLACEMENT_3D('',#74943,#59913,#59914);
#52464=AXIS2_PLACEMENT_3D('',#74945,#59916,#59917);
#52465=AXIS2_PLACEMENT_3D('',#74947,#59919,#59920);
#52466=AXIS2_PLACEMENT_3D('',#74949,#59922,#59923);
#52467=AXIS2_PLACEMENT_3D('',#74951,#59925,#59926);
#52468=AXIS2_PLACEMENT_3D('',#74953,#59928,#59929);
#52469=AXIS2_PLACEMENT_3D('',#74957,#59930,#59931);
#52470=AXIS2_PLACEMENT_3D('',#74961,#59934,#59935);
#52471=AXIS2_PLACEMENT_3D('',#74963,#59936,#59937);
#52472=AXIS2_PLACEMENT_3D('',#74965,#59939,#59940);
#52473=AXIS2_PLACEMENT_3D('',#74967,#59941,#59942);
#52474=AXIS2_PLACEMENT_3D('',#74969,#59944,#59945);
#52475=AXIS2_PLACEMENT_3D('',#74971,#59946,#59947);
#52476=AXIS2_PLACEMENT_3D('',#74973,#59949,#59950);
#52477=AXIS2_PLACEMENT_3D('',#74975,#59951,#59952);
#52478=AXIS2_PLACEMENT_3D('',#74977,#59954,#59955);
#52479=AXIS2_PLACEMENT_3D('',#74979,#59956,#59957);
#52480=AXIS2_PLACEMENT_3D('',#74981,#59959,#59960);
#52481=AXIS2_PLACEMENT_3D('',#74985,#59963,#59964);
#52482=AXIS2_PLACEMENT_3D('',#74987,#59965,#59966);
#52483=AXIS2_PLACEMENT_3D('',#74989,#59968,#59969);
#52484=AXIS2_PLACEMENT_3D('',#74991,#59970,#59971);
#52485=AXIS2_PLACEMENT_3D('',#74993,#59973,#59974);
#52486=AXIS2_PLACEMENT_3D('',#74995,#59975,#59976);
#52487=AXIS2_PLACEMENT_3D('',#74997,#59978,#59979);
#52488=AXIS2_PLACEMENT_3D('',#74999,#59980,#59981);
#52489=AXIS2_PLACEMENT_3D('',#75001,#59983,#59984);
#52490=AXIS2_PLACEMENT_3D('',#75003,#59985,#59986);
#52491=AXIS2_PLACEMENT_3D('',#75005,#59988,#59989);
#52492=AXIS2_PLACEMENT_3D('',#75007,#59991,#59992);
#52493=AXIS2_PLACEMENT_3D('',#75008,#59993,#59994);
#52494=AXIS2_PLACEMENT_3D('',#75010,#59995,#59996);
#52495=AXIS2_PLACEMENT_3D('',#75012,#59997,#59998);
#52496=AXIS2_PLACEMENT_3D('',#75016,#60000,#60001);
#52497=AXIS2_PLACEMENT_3D('',#75018,#60002,#60003);
#52498=AXIS2_PLACEMENT_3D('',#75020,#60004,#60005);
#52499=AXIS2_PLACEMENT_3D('',#75022,#60006,#60007);
#52500=AXIS2_PLACEMENT_3D('',#75024,#60008,#60009);
#52501=AXIS2_PLACEMENT_3D('',#75028,#60011,#60012);
#52502=AXIS2_PLACEMENT_3D('',#75030,#60013,#60014);
#52503=AXIS2_PLACEMENT_3D('',#75032,#60015,#60016);
#52504=AXIS2_PLACEMENT_3D('',#75034,#60017,#60018);
#52505=AXIS2_PLACEMENT_3D('',#75036,#60019,#60020);
#52506=AXIS2_PLACEMENT_3D('',#75038,#60022,#60023);
#52507=AXIS2_PLACEMENT_3D('',#75040,#60025,#60026);
#52508=AXIS2_PLACEMENT_3D('',#75042,#60028,#60029);
#52509=AXIS2_PLACEMENT_3D('',#75044,#60031,#60032);
#52510=AXIS2_PLACEMENT_3D('',#75046,#60034,#60035);
#52511=AXIS2_PLACEMENT_3D('',#75048,#60037,#60038);
#52512=AXIS2_PLACEMENT_3D('',#75050,#60040,#60041);
#52513=AXIS2_PLACEMENT_3D('',#75052,#60043,#60044);
#52514=AXIS2_PLACEMENT_3D('',#75054,#60046,#60047);
#52515=AXIS2_PLACEMENT_3D('',#75056,#60049,#60050);
#52516=AXIS2_PLACEMENT_3D('',#75058,#60052,#60053);
#52517=AXIS2_PLACEMENT_3D('',#75060,#60055,#60056);
#52518=AXIS2_PLACEMENT_3D('',#75062,#60058,#60059);
#52519=AXIS2_PLACEMENT_3D('',#75064,#60061,#60062);
#52520=AXIS2_PLACEMENT_3D('',#75068,#60063,#60064);
#52521=AXIS2_PLACEMENT_3D('',#75072,#60067,#60068);
#52522=AXIS2_PLACEMENT_3D('',#75074,#60069,#60070);
#52523=AXIS2_PLACEMENT_3D('',#75076,#60072,#60073);
#52524=AXIS2_PLACEMENT_3D('',#75078,#60074,#60075);
#52525=AXIS2_PLACEMENT_3D('',#75080,#60077,#60078);
#52526=AXIS2_PLACEMENT_3D('',#75082,#60079,#60080);
#52527=AXIS2_PLACEMENT_3D('',#75084,#60082,#60083);
#52528=AXIS2_PLACEMENT_3D('',#75086,#60084,#60085);
#52529=AXIS2_PLACEMENT_3D('',#75088,#60087,#60088);
#52530=AXIS2_PLACEMENT_3D('',#75090,#60089,#60090);
#52531=AXIS2_PLACEMENT_3D('',#75092,#60092,#60093);
#52532=AXIS2_PLACEMENT_3D('',#75096,#60096,#60097);
#52533=AXIS2_PLACEMENT_3D('',#75098,#60098,#60099);
#52534=AXIS2_PLACEMENT_3D('',#75100,#60101,#60102);
#52535=AXIS2_PLACEMENT_3D('',#75102,#60103,#60104);
#52536=AXIS2_PLACEMENT_3D('',#75104,#60106,#60107);
#52537=AXIS2_PLACEMENT_3D('',#75106,#60108,#60109);
#52538=AXIS2_PLACEMENT_3D('',#75108,#60111,#60112);
#52539=AXIS2_PLACEMENT_3D('',#75110,#60113,#60114);
#52540=AXIS2_PLACEMENT_3D('',#75112,#60116,#60117);
#52541=AXIS2_PLACEMENT_3D('',#75114,#60118,#60119);
#52542=AXIS2_PLACEMENT_3D('',#75116,#60121,#60122);
#52543=AXIS2_PLACEMENT_3D('',#75118,#60124,#60125);
#52544=AXIS2_PLACEMENT_3D('',#75119,#60126,#60127);
#52545=AXIS2_PLACEMENT_3D('',#75121,#60128,#60129);
#52546=AXIS2_PLACEMENT_3D('',#75123,#60130,#60131);
#52547=AXIS2_PLACEMENT_3D('',#75127,#60133,#60134);
#52548=AXIS2_PLACEMENT_3D('',#75129,#60135,#60136);
#52549=AXIS2_PLACEMENT_3D('',#75131,#60137,#60138);
#52550=AXIS2_PLACEMENT_3D('',#75133,#60139,#60140);
#52551=AXIS2_PLACEMENT_3D('',#75135,#60141,#60142);
#52552=AXIS2_PLACEMENT_3D('',#75139,#60144,#60145);
#52553=AXIS2_PLACEMENT_3D('',#75141,#60146,#60147);
#52554=AXIS2_PLACEMENT_3D('',#75143,#60148,#60149);
#52555=AXIS2_PLACEMENT_3D('',#75145,#60150,#60151);
#52556=AXIS2_PLACEMENT_3D('',#75147,#60152,#60153);
#52557=AXIS2_PLACEMENT_3D('',#75149,#60155,#60156);
#52558=AXIS2_PLACEMENT_3D('',#75151,#60158,#60159);
#52559=AXIS2_PLACEMENT_3D('',#75153,#60161,#60162);
#52560=AXIS2_PLACEMENT_3D('',#75155,#60164,#60165);
#52561=AXIS2_PLACEMENT_3D('',#75157,#60167,#60168);
#52562=AXIS2_PLACEMENT_3D('',#75159,#60170,#60171);
#52563=AXIS2_PLACEMENT_3D('',#75161,#60173,#60174);
#52564=AXIS2_PLACEMENT_3D('',#75163,#60176,#60177);
#52565=AXIS2_PLACEMENT_3D('',#75165,#60179,#60180);
#52566=AXIS2_PLACEMENT_3D('',#75167,#60182,#60183);
#52567=AXIS2_PLACEMENT_3D('',#75169,#60185,#60186);
#52568=AXIS2_PLACEMENT_3D('',#75171,#60188,#60189);
#52569=AXIS2_PLACEMENT_3D('',#75173,#60191,#60192);
#52570=AXIS2_PLACEMENT_3D('',#75175,#60194,#60195);
#52571=AXIS2_PLACEMENT_3D('',#75179,#60196,#60197);
#52572=AXIS2_PLACEMENT_3D('',#75183,#60200,#60201);
#52573=AXIS2_PLACEMENT_3D('',#75185,#60202,#60203);
#52574=AXIS2_PLACEMENT_3D('',#75187,#60205,#60206);
#52575=AXIS2_PLACEMENT_3D('',#75189,#60207,#60208);
#52576=AXIS2_PLACEMENT_3D('',#75191,#60210,#60211);
#52577=AXIS2_PLACEMENT_3D('',#75193,#60212,#60213);
#52578=AXIS2_PLACEMENT_3D('',#75195,#60215,#60216);
#52579=AXIS2_PLACEMENT_3D('',#75197,#60217,#60218);
#52580=AXIS2_PLACEMENT_3D('',#75199,#60220,#60221);
#52581=AXIS2_PLACEMENT_3D('',#75201,#60222,#60223);
#52582=AXIS2_PLACEMENT_3D('',#75203,#60225,#60226);
#52583=AXIS2_PLACEMENT_3D('',#75207,#60229,#60230);
#52584=AXIS2_PLACEMENT_3D('',#75209,#60231,#60232);
#52585=AXIS2_PLACEMENT_3D('',#75211,#60234,#60235);
#52586=AXIS2_PLACEMENT_3D('',#75213,#60236,#60237);
#52587=AXIS2_PLACEMENT_3D('',#75215,#60239,#60240);
#52588=AXIS2_PLACEMENT_3D('',#75217,#60241,#60242);
#52589=AXIS2_PLACEMENT_3D('',#75219,#60244,#60245);
#52590=AXIS2_PLACEMENT_3D('',#75221,#60246,#60247);
#52591=AXIS2_PLACEMENT_3D('',#75223,#60249,#60250);
#52592=AXIS2_PLACEMENT_3D('',#75225,#60251,#60252);
#52593=AXIS2_PLACEMENT_3D('',#75227,#60254,#60255);
#52594=AXIS2_PLACEMENT_3D('',#75229,#60257,#60258);
#52595=AXIS2_PLACEMENT_3D('',#75230,#60259,#60260);
#52596=AXIS2_PLACEMENT_3D('',#75232,#60261,#60262);
#52597=AXIS2_PLACEMENT_3D('',#75234,#60263,#60264);
#52598=AXIS2_PLACEMENT_3D('',#75238,#60266,#60267);
#52599=AXIS2_PLACEMENT_3D('',#75240,#60268,#60269);
#52600=AXIS2_PLACEMENT_3D('',#75242,#60270,#60271);
#52601=AXIS2_PLACEMENT_3D('',#75244,#60272,#60273);
#52602=AXIS2_PLACEMENT_3D('',#75246,#60274,#60275);
#52603=AXIS2_PLACEMENT_3D('',#75250,#60277,#60278);
#52604=AXIS2_PLACEMENT_3D('',#75252,#60279,#60280);
#52605=AXIS2_PLACEMENT_3D('',#75254,#60281,#60282);
#52606=AXIS2_PLACEMENT_3D('',#75256,#60283,#60284);
#52607=AXIS2_PLACEMENT_3D('',#75258,#60285,#60286);
#52608=AXIS2_PLACEMENT_3D('',#75260,#60288,#60289);
#52609=AXIS2_PLACEMENT_3D('',#75262,#60291,#60292);
#52610=AXIS2_PLACEMENT_3D('',#75264,#60294,#60295);
#52611=AXIS2_PLACEMENT_3D('',#75266,#60297,#60298);
#52612=AXIS2_PLACEMENT_3D('',#75268,#60300,#60301);
#52613=AXIS2_PLACEMENT_3D('',#75270,#60303,#60304);
#52614=AXIS2_PLACEMENT_3D('',#75272,#60306,#60307);
#52615=AXIS2_PLACEMENT_3D('',#75274,#60309,#60310);
#52616=AXIS2_PLACEMENT_3D('',#75276,#60312,#60313);
#52617=AXIS2_PLACEMENT_3D('',#75278,#60315,#60316);
#52618=AXIS2_PLACEMENT_3D('',#75280,#60318,#60319);
#52619=AXIS2_PLACEMENT_3D('',#75282,#60321,#60322);
#52620=AXIS2_PLACEMENT_3D('',#75284,#60324,#60325);
#52621=AXIS2_PLACEMENT_3D('',#75286,#60327,#60328);
#52622=AXIS2_PLACEMENT_3D('',#75290,#60329,#60330);
#52623=AXIS2_PLACEMENT_3D('',#75294,#60333,#60334);
#52624=AXIS2_PLACEMENT_3D('',#75296,#60335,#60336);
#52625=AXIS2_PLACEMENT_3D('',#75298,#60338,#60339);
#52626=AXIS2_PLACEMENT_3D('',#75300,#60340,#60341);
#52627=AXIS2_PLACEMENT_3D('',#75302,#60343,#60344);
#52628=AXIS2_PLACEMENT_3D('',#75304,#60345,#60346);
#52629=AXIS2_PLACEMENT_3D('',#75306,#60348,#60349);
#52630=AXIS2_PLACEMENT_3D('',#75308,#60350,#60351);
#52631=AXIS2_PLACEMENT_3D('',#75310,#60353,#60354);
#52632=AXIS2_PLACEMENT_3D('',#75312,#60355,#60356);
#52633=AXIS2_PLACEMENT_3D('',#75314,#60358,#60359);
#52634=AXIS2_PLACEMENT_3D('',#75318,#60362,#60363);
#52635=AXIS2_PLACEMENT_3D('',#75320,#60364,#60365);
#52636=AXIS2_PLACEMENT_3D('',#75322,#60367,#60368);
#52637=AXIS2_PLACEMENT_3D('',#75324,#60369,#60370);
#52638=AXIS2_PLACEMENT_3D('',#75326,#60372,#60373);
#52639=AXIS2_PLACEMENT_3D('',#75328,#60374,#60375);
#52640=AXIS2_PLACEMENT_3D('',#75330,#60377,#60378);
#52641=AXIS2_PLACEMENT_3D('',#75332,#60379,#60380);
#52642=AXIS2_PLACEMENT_3D('',#75334,#60382,#60383);
#52643=AXIS2_PLACEMENT_3D('',#75336,#60384,#60385);
#52644=AXIS2_PLACEMENT_3D('',#75338,#60387,#60388);
#52645=AXIS2_PLACEMENT_3D('',#75340,#60390,#60391);
#52646=AXIS2_PLACEMENT_3D('',#75341,#60392,#60393);
#52647=AXIS2_PLACEMENT_3D('',#75343,#60394,#60395);
#52648=AXIS2_PLACEMENT_3D('',#75345,#60396,#60397);
#52649=AXIS2_PLACEMENT_3D('',#75349,#60399,#60400);
#52650=AXIS2_PLACEMENT_3D('',#75351,#60401,#60402);
#52651=AXIS2_PLACEMENT_3D('',#75353,#60403,#60404);
#52652=AXIS2_PLACEMENT_3D('',#75355,#60405,#60406);
#52653=AXIS2_PLACEMENT_3D('',#75357,#60407,#60408);
#52654=AXIS2_PLACEMENT_3D('',#75361,#60410,#60411);
#52655=AXIS2_PLACEMENT_3D('',#75363,#60412,#60413);
#52656=AXIS2_PLACEMENT_3D('',#75365,#60414,#60415);
#52657=AXIS2_PLACEMENT_3D('',#75367,#60416,#60417);
#52658=AXIS2_PLACEMENT_3D('',#75369,#60418,#60419);
#52659=AXIS2_PLACEMENT_3D('',#75371,#60421,#60422);
#52660=AXIS2_PLACEMENT_3D('',#75373,#60424,#60425);
#52661=AXIS2_PLACEMENT_3D('',#75375,#60427,#60428);
#52662=AXIS2_PLACEMENT_3D('',#75377,#60430,#60431);
#52663=AXIS2_PLACEMENT_3D('',#75379,#60433,#60434);
#52664=AXIS2_PLACEMENT_3D('',#75381,#60436,#60437);
#52665=AXIS2_PLACEMENT_3D('',#75383,#60439,#60440);
#52666=AXIS2_PLACEMENT_3D('',#75385,#60442,#60443);
#52667=AXIS2_PLACEMENT_3D('',#75387,#60445,#60446);
#52668=AXIS2_PLACEMENT_3D('',#75389,#60448,#60449);
#52669=AXIS2_PLACEMENT_3D('',#75391,#60451,#60452);
#52670=AXIS2_PLACEMENT_3D('',#75393,#60454,#60455);
#52671=AXIS2_PLACEMENT_3D('',#75395,#60457,#60458);
#52672=AXIS2_PLACEMENT_3D('',#75397,#60460,#60461);
#52673=AXIS2_PLACEMENT_3D('',#75401,#60462,#60463);
#52674=AXIS2_PLACEMENT_3D('',#75405,#60466,#60467);
#52675=AXIS2_PLACEMENT_3D('',#75407,#60468,#60469);
#52676=AXIS2_PLACEMENT_3D('',#75409,#60471,#60472);
#52677=AXIS2_PLACEMENT_3D('',#75411,#60473,#60474);
#52678=AXIS2_PLACEMENT_3D('',#75413,#60476,#60477);
#52679=AXIS2_PLACEMENT_3D('',#75415,#60478,#60479);
#52680=AXIS2_PLACEMENT_3D('',#75417,#60481,#60482);
#52681=AXIS2_PLACEMENT_3D('',#75419,#60483,#60484);
#52682=AXIS2_PLACEMENT_3D('',#75421,#60486,#60487);
#52683=AXIS2_PLACEMENT_3D('',#75423,#60488,#60489);
#52684=AXIS2_PLACEMENT_3D('',#75425,#60491,#60492);
#52685=AXIS2_PLACEMENT_3D('',#75429,#60495,#60496);
#52686=AXIS2_PLACEMENT_3D('',#75431,#60497,#60498);
#52687=AXIS2_PLACEMENT_3D('',#75433,#60500,#60501);
#52688=AXIS2_PLACEMENT_3D('',#75435,#60502,#60503);
#52689=AXIS2_PLACEMENT_3D('',#75437,#60505,#60506);
#52690=AXIS2_PLACEMENT_3D('',#75439,#60507,#60508);
#52691=AXIS2_PLACEMENT_3D('',#75441,#60510,#60511);
#52692=AXIS2_PLACEMENT_3D('',#75443,#60512,#60513);
#52693=AXIS2_PLACEMENT_3D('',#75445,#60515,#60516);
#52694=AXIS2_PLACEMENT_3D('',#75447,#60517,#60518);
#52695=AXIS2_PLACEMENT_3D('',#75449,#60520,#60521);
#52696=AXIS2_PLACEMENT_3D('',#75451,#60523,#60524);
#52697=AXIS2_PLACEMENT_3D('',#75452,#60525,#60526);
#52698=AXIS2_PLACEMENT_3D('',#75454,#60527,#60528);
#52699=AXIS2_PLACEMENT_3D('',#75456,#60529,#60530);
#52700=AXIS2_PLACEMENT_3D('',#75460,#60532,#60533);
#52701=AXIS2_PLACEMENT_3D('',#75462,#60534,#60535);
#52702=AXIS2_PLACEMENT_3D('',#75464,#60536,#60537);
#52703=AXIS2_PLACEMENT_3D('',#75466,#60538,#60539);
#52704=AXIS2_PLACEMENT_3D('',#75468,#60540,#60541);
#52705=AXIS2_PLACEMENT_3D('',#75472,#60543,#60544);
#52706=AXIS2_PLACEMENT_3D('',#75474,#60545,#60546);
#52707=AXIS2_PLACEMENT_3D('',#75476,#60547,#60548);
#52708=AXIS2_PLACEMENT_3D('',#75478,#60549,#60550);
#52709=AXIS2_PLACEMENT_3D('',#75480,#60551,#60552);
#52710=AXIS2_PLACEMENT_3D('',#75482,#60554,#60555);
#52711=AXIS2_PLACEMENT_3D('',#75484,#60557,#60558);
#52712=AXIS2_PLACEMENT_3D('',#75486,#60560,#60561);
#52713=AXIS2_PLACEMENT_3D('',#75488,#60563,#60564);
#52714=AXIS2_PLACEMENT_3D('',#75490,#60566,#60567);
#52715=AXIS2_PLACEMENT_3D('',#75492,#60569,#60570);
#52716=AXIS2_PLACEMENT_3D('',#75494,#60572,#60573);
#52717=AXIS2_PLACEMENT_3D('',#75496,#60575,#60576);
#52718=AXIS2_PLACEMENT_3D('',#75498,#60578,#60579);
#52719=AXIS2_PLACEMENT_3D('',#75500,#60581,#60582);
#52720=AXIS2_PLACEMENT_3D('',#75502,#60584,#60585);
#52721=AXIS2_PLACEMENT_3D('',#75504,#60587,#60588);
#52722=AXIS2_PLACEMENT_3D('',#75506,#60590,#60591);
#52723=AXIS2_PLACEMENT_3D('',#75508,#60593,#60594);
#52724=AXIS2_PLACEMENT_3D('',#75512,#60595,#60596);
#52725=AXIS2_PLACEMENT_3D('',#75516,#60599,#60600);
#52726=AXIS2_PLACEMENT_3D('',#75518,#60601,#60602);
#52727=AXIS2_PLACEMENT_3D('',#75520,#60604,#60605);
#52728=AXIS2_PLACEMENT_3D('',#75522,#60606,#60607);
#52729=AXIS2_PLACEMENT_3D('',#75524,#60609,#60610);
#52730=AXIS2_PLACEMENT_3D('',#75526,#60611,#60612);
#52731=AXIS2_PLACEMENT_3D('',#75528,#60614,#60615);
#52732=AXIS2_PLACEMENT_3D('',#75530,#60616,#60617);
#52733=AXIS2_PLACEMENT_3D('',#75532,#60619,#60620);
#52734=AXIS2_PLACEMENT_3D('',#75534,#60621,#60622);
#52735=AXIS2_PLACEMENT_3D('',#75536,#60624,#60625);
#52736=AXIS2_PLACEMENT_3D('',#75540,#60628,#60629);
#52737=AXIS2_PLACEMENT_3D('',#75542,#60630,#60631);
#52738=AXIS2_PLACEMENT_3D('',#75544,#60633,#60634);
#52739=AXIS2_PLACEMENT_3D('',#75546,#60635,#60636);
#52740=AXIS2_PLACEMENT_3D('',#75548,#60638,#60639);
#52741=AXIS2_PLACEMENT_3D('',#75550,#60640,#60641);
#52742=AXIS2_PLACEMENT_3D('',#75552,#60643,#60644);
#52743=AXIS2_PLACEMENT_3D('',#75554,#60645,#60646);
#52744=AXIS2_PLACEMENT_3D('',#75556,#60648,#60649);
#52745=AXIS2_PLACEMENT_3D('',#75558,#60650,#60651);
#52746=AXIS2_PLACEMENT_3D('',#75560,#60653,#60654);
#52747=AXIS2_PLACEMENT_3D('',#75562,#60656,#60657);
#52748=AXIS2_PLACEMENT_3D('',#75563,#60658,#60659);
#52749=AXIS2_PLACEMENT_3D('',#75565,#60660,#60661);
#52750=AXIS2_PLACEMENT_3D('',#75567,#60662,#60663);
#52751=AXIS2_PLACEMENT_3D('',#75571,#60665,#60666);
#52752=AXIS2_PLACEMENT_3D('',#75573,#60667,#60668);
#52753=AXIS2_PLACEMENT_3D('',#75575,#60669,#60670);
#52754=AXIS2_PLACEMENT_3D('',#75577,#60671,#60672);
#52755=AXIS2_PLACEMENT_3D('',#75579,#60673,#60674);
#52756=AXIS2_PLACEMENT_3D('',#75583,#60676,#60677);
#52757=AXIS2_PLACEMENT_3D('',#75585,#60678,#60679);
#52758=AXIS2_PLACEMENT_3D('',#75587,#60680,#60681);
#52759=AXIS2_PLACEMENT_3D('',#75589,#60682,#60683);
#52760=AXIS2_PLACEMENT_3D('',#75591,#60684,#60685);
#52761=AXIS2_PLACEMENT_3D('',#75593,#60687,#60688);
#52762=AXIS2_PLACEMENT_3D('',#75595,#60690,#60691);
#52763=AXIS2_PLACEMENT_3D('',#75597,#60693,#60694);
#52764=AXIS2_PLACEMENT_3D('',#75599,#60696,#60697);
#52765=AXIS2_PLACEMENT_3D('',#75601,#60699,#60700);
#52766=AXIS2_PLACEMENT_3D('',#75603,#60702,#60703);
#52767=AXIS2_PLACEMENT_3D('',#75605,#60705,#60706);
#52768=AXIS2_PLACEMENT_3D('',#75607,#60708,#60709);
#52769=AXIS2_PLACEMENT_3D('',#75609,#60711,#60712);
#52770=AXIS2_PLACEMENT_3D('',#75611,#60714,#60715);
#52771=AXIS2_PLACEMENT_3D('',#75613,#60717,#60718);
#52772=AXIS2_PLACEMENT_3D('',#75615,#60720,#60721);
#52773=AXIS2_PLACEMENT_3D('',#75617,#60723,#60724);
#52774=AXIS2_PLACEMENT_3D('',#75619,#60726,#60727);
#52775=AXIS2_PLACEMENT_3D('',#75623,#60728,#60729);
#52776=AXIS2_PLACEMENT_3D('',#75627,#60732,#60733);
#52777=AXIS2_PLACEMENT_3D('',#75629,#60734,#60735);
#52778=AXIS2_PLACEMENT_3D('',#75631,#60737,#60738);
#52779=AXIS2_PLACEMENT_3D('',#75633,#60739,#60740);
#52780=AXIS2_PLACEMENT_3D('',#75635,#60742,#60743);
#52781=AXIS2_PLACEMENT_3D('',#75637,#60744,#60745);
#52782=AXIS2_PLACEMENT_3D('',#75639,#60747,#60748);
#52783=AXIS2_PLACEMENT_3D('',#75641,#60749,#60750);
#52784=AXIS2_PLACEMENT_3D('',#75643,#60752,#60753);
#52785=AXIS2_PLACEMENT_3D('',#75645,#60754,#60755);
#52786=AXIS2_PLACEMENT_3D('',#75647,#60757,#60758);
#52787=AXIS2_PLACEMENT_3D('',#75651,#60761,#60762);
#52788=AXIS2_PLACEMENT_3D('',#75653,#60763,#60764);
#52789=AXIS2_PLACEMENT_3D('',#75655,#60766,#60767);
#52790=AXIS2_PLACEMENT_3D('',#75657,#60768,#60769);
#52791=AXIS2_PLACEMENT_3D('',#75659,#60771,#60772);
#52792=AXIS2_PLACEMENT_3D('',#75661,#60773,#60774);
#52793=AXIS2_PLACEMENT_3D('',#75663,#60776,#60777);
#52794=AXIS2_PLACEMENT_3D('',#75665,#60778,#60779);
#52795=AXIS2_PLACEMENT_3D('',#75667,#60781,#60782);
#52796=AXIS2_PLACEMENT_3D('',#75669,#60783,#60784);
#52797=AXIS2_PLACEMENT_3D('',#75671,#60786,#60787);
#52798=AXIS2_PLACEMENT_3D('',#75673,#60789,#60790);
#52799=AXIS2_PLACEMENT_3D('',#75674,#60791,#60792);
#52800=AXIS2_PLACEMENT_3D('',#75676,#60793,#60794);
#52801=AXIS2_PLACEMENT_3D('',#75678,#60795,#60796);
#52802=AXIS2_PLACEMENT_3D('',#75682,#60798,#60799);
#52803=AXIS2_PLACEMENT_3D('',#75684,#60800,#60801);
#52804=AXIS2_PLACEMENT_3D('',#75686,#60802,#60803);
#52805=AXIS2_PLACEMENT_3D('',#75688,#60804,#60805);
#52806=AXIS2_PLACEMENT_3D('',#75690,#60806,#60807);
#52807=AXIS2_PLACEMENT_3D('',#75694,#60809,#60810);
#52808=AXIS2_PLACEMENT_3D('',#75696,#60811,#60812);
#52809=AXIS2_PLACEMENT_3D('',#75698,#60813,#60814);
#52810=AXIS2_PLACEMENT_3D('',#75700,#60815,#60816);
#52811=AXIS2_PLACEMENT_3D('',#75702,#60817,#60818);
#52812=AXIS2_PLACEMENT_3D('',#75704,#60820,#60821);
#52813=AXIS2_PLACEMENT_3D('',#75706,#60823,#60824);
#52814=AXIS2_PLACEMENT_3D('',#75708,#60826,#60827);
#52815=AXIS2_PLACEMENT_3D('',#75710,#60829,#60830);
#52816=AXIS2_PLACEMENT_3D('',#75712,#60832,#60833);
#52817=AXIS2_PLACEMENT_3D('',#75714,#60835,#60836);
#52818=AXIS2_PLACEMENT_3D('',#75716,#60838,#60839);
#52819=AXIS2_PLACEMENT_3D('',#75718,#60841,#60842);
#52820=AXIS2_PLACEMENT_3D('',#75720,#60844,#60845);
#52821=AXIS2_PLACEMENT_3D('',#75722,#60847,#60848);
#52822=AXIS2_PLACEMENT_3D('',#75724,#60850,#60851);
#52823=AXIS2_PLACEMENT_3D('',#75726,#60853,#60854);
#52824=AXIS2_PLACEMENT_3D('',#75728,#60856,#60857);
#52825=AXIS2_PLACEMENT_3D('',#75730,#60859,#60860);
#52826=AXIS2_PLACEMENT_3D('',#75734,#60861,#60862);
#52827=AXIS2_PLACEMENT_3D('',#75738,#60865,#60866);
#52828=AXIS2_PLACEMENT_3D('',#75740,#60867,#60868);
#52829=AXIS2_PLACEMENT_3D('',#75742,#60870,#60871);
#52830=AXIS2_PLACEMENT_3D('',#75744,#60872,#60873);
#52831=AXIS2_PLACEMENT_3D('',#75746,#60875,#60876);
#52832=AXIS2_PLACEMENT_3D('',#75748,#60877,#60878);
#52833=AXIS2_PLACEMENT_3D('',#75750,#60880,#60881);
#52834=AXIS2_PLACEMENT_3D('',#75752,#60882,#60883);
#52835=AXIS2_PLACEMENT_3D('',#75754,#60885,#60886);
#52836=AXIS2_PLACEMENT_3D('',#75756,#60887,#60888);
#52837=AXIS2_PLACEMENT_3D('',#75758,#60890,#60891);
#52838=AXIS2_PLACEMENT_3D('',#75762,#60894,#60895);
#52839=AXIS2_PLACEMENT_3D('',#75764,#60896,#60897);
#52840=AXIS2_PLACEMENT_3D('',#75766,#60899,#60900);
#52841=AXIS2_PLACEMENT_3D('',#75768,#60901,#60902);
#52842=AXIS2_PLACEMENT_3D('',#75770,#60904,#60905);
#52843=AXIS2_PLACEMENT_3D('',#75772,#60906,#60907);
#52844=AXIS2_PLACEMENT_3D('',#75774,#60909,#60910);
#52845=AXIS2_PLACEMENT_3D('',#75776,#60911,#60912);
#52846=AXIS2_PLACEMENT_3D('',#75778,#60914,#60915);
#52847=AXIS2_PLACEMENT_3D('',#75780,#60916,#60917);
#52848=AXIS2_PLACEMENT_3D('',#75782,#60919,#60920);
#52849=AXIS2_PLACEMENT_3D('',#75784,#60922,#60923);
#52850=AXIS2_PLACEMENT_3D('',#75785,#60924,#60925);
#52851=AXIS2_PLACEMENT_3D('',#75787,#60926,#60927);
#52852=AXIS2_PLACEMENT_3D('',#75789,#60928,#60929);
#52853=AXIS2_PLACEMENT_3D('',#75793,#60931,#60932);
#52854=AXIS2_PLACEMENT_3D('',#75795,#60933,#60934);
#52855=AXIS2_PLACEMENT_3D('',#75797,#60935,#60936);
#52856=AXIS2_PLACEMENT_3D('',#75799,#60937,#60938);
#52857=AXIS2_PLACEMENT_3D('',#75801,#60939,#60940);
#52858=AXIS2_PLACEMENT_3D('',#75805,#60942,#60943);
#52859=AXIS2_PLACEMENT_3D('',#75807,#60944,#60945);
#52860=AXIS2_PLACEMENT_3D('',#75809,#60946,#60947);
#52861=AXIS2_PLACEMENT_3D('',#75811,#60948,#60949);
#52862=AXIS2_PLACEMENT_3D('',#75813,#60950,#60951);
#52863=AXIS2_PLACEMENT_3D('',#75815,#60953,#60954);
#52864=AXIS2_PLACEMENT_3D('',#75817,#60956,#60957);
#52865=AXIS2_PLACEMENT_3D('',#75819,#60959,#60960);
#52866=AXIS2_PLACEMENT_3D('',#75821,#60962,#60963);
#52867=AXIS2_PLACEMENT_3D('',#75823,#60965,#60966);
#52868=AXIS2_PLACEMENT_3D('',#75825,#60968,#60969);
#52869=AXIS2_PLACEMENT_3D('',#75827,#60971,#60972);
#52870=AXIS2_PLACEMENT_3D('',#75829,#60974,#60975);
#52871=AXIS2_PLACEMENT_3D('',#75831,#60977,#60978);
#52872=AXIS2_PLACEMENT_3D('',#75833,#60980,#60981);
#52873=AXIS2_PLACEMENT_3D('',#75835,#60983,#60984);
#52874=AXIS2_PLACEMENT_3D('',#75837,#60986,#60987);
#52875=AXIS2_PLACEMENT_3D('',#75839,#60989,#60990);
#52876=AXIS2_PLACEMENT_3D('',#75841,#60992,#60993);
#52877=AXIS2_PLACEMENT_3D('',#75845,#60994,#60995);
#52878=AXIS2_PLACEMENT_3D('',#75849,#60998,#60999);
#52879=AXIS2_PLACEMENT_3D('',#75851,#61000,#61001);
#52880=AXIS2_PLACEMENT_3D('',#75853,#61003,#61004);
#52881=AXIS2_PLACEMENT_3D('',#75855,#61005,#61006);
#52882=AXIS2_PLACEMENT_3D('',#75857,#61008,#61009);
#52883=AXIS2_PLACEMENT_3D('',#75859,#61010,#61011);
#52884=AXIS2_PLACEMENT_3D('',#75861,#61013,#61014);
#52885=AXIS2_PLACEMENT_3D('',#75863,#61015,#61016);
#52886=AXIS2_PLACEMENT_3D('',#75865,#61018,#61019);
#52887=AXIS2_PLACEMENT_3D('',#75867,#61020,#61021);
#52888=AXIS2_PLACEMENT_3D('',#75869,#61023,#61024);
#52889=AXIS2_PLACEMENT_3D('',#75873,#61027,#61028);
#52890=AXIS2_PLACEMENT_3D('',#75875,#61029,#61030);
#52891=AXIS2_PLACEMENT_3D('',#75877,#61032,#61033);
#52892=AXIS2_PLACEMENT_3D('',#75879,#61034,#61035);
#52893=AXIS2_PLACEMENT_3D('',#75881,#61037,#61038);
#52894=AXIS2_PLACEMENT_3D('',#75883,#61039,#61040);
#52895=AXIS2_PLACEMENT_3D('',#75885,#61042,#61043);
#52896=AXIS2_PLACEMENT_3D('',#75887,#61044,#61045);
#52897=AXIS2_PLACEMENT_3D('',#75889,#61047,#61048);
#52898=AXIS2_PLACEMENT_3D('',#75891,#61049,#61050);
#52899=AXIS2_PLACEMENT_3D('',#75893,#61052,#61053);
#52900=AXIS2_PLACEMENT_3D('',#75895,#61055,#61056);
#52901=AXIS2_PLACEMENT_3D('',#75896,#61057,#61058);
#52902=AXIS2_PLACEMENT_3D('',#75898,#61059,#61060);
#52903=AXIS2_PLACEMENT_3D('',#75900,#61061,#61062);
#52904=AXIS2_PLACEMENT_3D('',#75904,#61064,#61065);
#52905=AXIS2_PLACEMENT_3D('',#75906,#61066,#61067);
#52906=AXIS2_PLACEMENT_3D('',#75908,#61068,#61069);
#52907=AXIS2_PLACEMENT_3D('',#75910,#61070,#61071);
#52908=AXIS2_PLACEMENT_3D('',#75912,#61072,#61073);
#52909=AXIS2_PLACEMENT_3D('',#75916,#61075,#61076);
#52910=AXIS2_PLACEMENT_3D('',#75918,#61077,#61078);
#52911=AXIS2_PLACEMENT_3D('',#75920,#61079,#61080);
#52912=AXIS2_PLACEMENT_3D('',#75922,#61081,#61082);
#52913=AXIS2_PLACEMENT_3D('',#75924,#61083,#61084);
#52914=AXIS2_PLACEMENT_3D('',#75926,#61086,#61087);
#52915=AXIS2_PLACEMENT_3D('',#75928,#61089,#61090);
#52916=AXIS2_PLACEMENT_3D('',#75930,#61092,#61093);
#52917=AXIS2_PLACEMENT_3D('',#75932,#61095,#61096);
#52918=AXIS2_PLACEMENT_3D('',#75934,#61098,#61099);
#52919=AXIS2_PLACEMENT_3D('',#75936,#61101,#61102);
#52920=AXIS2_PLACEMENT_3D('',#75938,#61104,#61105);
#52921=AXIS2_PLACEMENT_3D('',#75940,#61107,#61108);
#52922=AXIS2_PLACEMENT_3D('',#75942,#61110,#61111);
#52923=AXIS2_PLACEMENT_3D('',#75944,#61113,#61114);
#52924=AXIS2_PLACEMENT_3D('',#75946,#61116,#61117);
#52925=AXIS2_PLACEMENT_3D('',#75948,#61119,#61120);
#52926=AXIS2_PLACEMENT_3D('',#75950,#61122,#61123);
#52927=AXIS2_PLACEMENT_3D('',#75952,#61125,#61126);
#52928=AXIS2_PLACEMENT_3D('',#75956,#61127,#61128);
#52929=AXIS2_PLACEMENT_3D('',#75960,#61131,#61132);
#52930=AXIS2_PLACEMENT_3D('',#75962,#61133,#61134);
#52931=AXIS2_PLACEMENT_3D('',#75964,#61136,#61137);
#52932=AXIS2_PLACEMENT_3D('',#75966,#61138,#61139);
#52933=AXIS2_PLACEMENT_3D('',#75968,#61141,#61142);
#52934=AXIS2_PLACEMENT_3D('',#75970,#61143,#61144);
#52935=AXIS2_PLACEMENT_3D('',#75972,#61146,#61147);
#52936=AXIS2_PLACEMENT_3D('',#75974,#61148,#61149);
#52937=AXIS2_PLACEMENT_3D('',#75976,#61151,#61152);
#52938=AXIS2_PLACEMENT_3D('',#75978,#61153,#61154);
#52939=AXIS2_PLACEMENT_3D('',#75980,#61156,#61157);
#52940=AXIS2_PLACEMENT_3D('',#75984,#61160,#61161);
#52941=AXIS2_PLACEMENT_3D('',#75986,#61162,#61163);
#52942=AXIS2_PLACEMENT_3D('',#75988,#61165,#61166);
#52943=AXIS2_PLACEMENT_3D('',#75990,#61167,#61168);
#52944=AXIS2_PLACEMENT_3D('',#75992,#61170,#61171);
#52945=AXIS2_PLACEMENT_3D('',#75994,#61172,#61173);
#52946=AXIS2_PLACEMENT_3D('',#75996,#61175,#61176);
#52947=AXIS2_PLACEMENT_3D('',#75998,#61177,#61178);
#52948=AXIS2_PLACEMENT_3D('',#76000,#61180,#61181);
#52949=AXIS2_PLACEMENT_3D('',#76002,#61182,#61183);
#52950=AXIS2_PLACEMENT_3D('',#76004,#61185,#61186);
#52951=AXIS2_PLACEMENT_3D('',#76006,#61188,#61189);
#52952=AXIS2_PLACEMENT_3D('',#76007,#61190,#61191);
#52953=AXIS2_PLACEMENT_3D('',#76009,#61192,#61193);
#52954=AXIS2_PLACEMENT_3D('',#76011,#61194,#61195);
#52955=AXIS2_PLACEMENT_3D('',#76015,#61197,#61198);
#52956=AXIS2_PLACEMENT_3D('',#76017,#61199,#61200);
#52957=AXIS2_PLACEMENT_3D('',#76019,#61201,#61202);
#52958=AXIS2_PLACEMENT_3D('',#76021,#61203,#61204);
#52959=AXIS2_PLACEMENT_3D('',#76023,#61205,#61206);
#52960=AXIS2_PLACEMENT_3D('',#76027,#61208,#61209);
#52961=AXIS2_PLACEMENT_3D('',#76029,#61210,#61211);
#52962=AXIS2_PLACEMENT_3D('',#76031,#61212,#61213);
#52963=AXIS2_PLACEMENT_3D('',#76033,#61214,#61215);
#52964=AXIS2_PLACEMENT_3D('',#76035,#61216,#61217);
#52965=AXIS2_PLACEMENT_3D('',#76037,#61219,#61220);
#52966=AXIS2_PLACEMENT_3D('',#76039,#61222,#61223);
#52967=AXIS2_PLACEMENT_3D('',#76041,#61225,#61226);
#52968=AXIS2_PLACEMENT_3D('',#76043,#61228,#61229);
#52969=AXIS2_PLACEMENT_3D('',#76045,#61231,#61232);
#52970=AXIS2_PLACEMENT_3D('',#76047,#61234,#61235);
#52971=AXIS2_PLACEMENT_3D('',#76049,#61237,#61238);
#52972=AXIS2_PLACEMENT_3D('',#76051,#61240,#61241);
#52973=AXIS2_PLACEMENT_3D('',#76053,#61243,#61244);
#52974=AXIS2_PLACEMENT_3D('',#76055,#61246,#61247);
#52975=AXIS2_PLACEMENT_3D('',#76057,#61249,#61250);
#52976=AXIS2_PLACEMENT_3D('',#76059,#61252,#61253);
#52977=AXIS2_PLACEMENT_3D('',#76061,#61255,#61256);
#52978=AXIS2_PLACEMENT_3D('',#76063,#61258,#61259);
#52979=AXIS2_PLACEMENT_3D('',#76067,#61260,#61261);
#52980=AXIS2_PLACEMENT_3D('',#76071,#61264,#61265);
#52981=AXIS2_PLACEMENT_3D('',#76073,#61266,#61267);
#52982=AXIS2_PLACEMENT_3D('',#76075,#61269,#61270);
#52983=AXIS2_PLACEMENT_3D('',#76077,#61271,#61272);
#52984=AXIS2_PLACEMENT_3D('',#76079,#61274,#61275);
#52985=AXIS2_PLACEMENT_3D('',#76081,#61276,#61277);
#52986=AXIS2_PLACEMENT_3D('',#76083,#61279,#61280);
#52987=AXIS2_PLACEMENT_3D('',#76085,#61281,#61282);
#52988=AXIS2_PLACEMENT_3D('',#76087,#61284,#61285);
#52989=AXIS2_PLACEMENT_3D('',#76089,#61286,#61287);
#52990=AXIS2_PLACEMENT_3D('',#76091,#61289,#61290);
#52991=AXIS2_PLACEMENT_3D('',#76095,#61293,#61294);
#52992=AXIS2_PLACEMENT_3D('',#76097,#61295,#61296);
#52993=AXIS2_PLACEMENT_3D('',#76099,#61298,#61299);
#52994=AXIS2_PLACEMENT_3D('',#76101,#61300,#61301);
#52995=AXIS2_PLACEMENT_3D('',#76103,#61303,#61304);
#52996=AXIS2_PLACEMENT_3D('',#76105,#61305,#61306);
#52997=AXIS2_PLACEMENT_3D('',#76107,#61308,#61309);
#52998=AXIS2_PLACEMENT_3D('',#76109,#61310,#61311);
#52999=AXIS2_PLACEMENT_3D('',#76111,#61313,#61314);
#53000=AXIS2_PLACEMENT_3D('',#76113,#61315,#61316);
#53001=AXIS2_PLACEMENT_3D('',#76115,#61318,#61319);
#53002=AXIS2_PLACEMENT_3D('',#76117,#61321,#61322);
#53003=AXIS2_PLACEMENT_3D('',#76118,#61323,#61324);
#53004=AXIS2_PLACEMENT_3D('',#76120,#61325,#61326);
#53005=AXIS2_PLACEMENT_3D('',#76122,#61327,#61328);
#53006=AXIS2_PLACEMENT_3D('',#76126,#61330,#61331);
#53007=AXIS2_PLACEMENT_3D('',#76128,#61332,#61333);
#53008=AXIS2_PLACEMENT_3D('',#76130,#61334,#61335);
#53009=AXIS2_PLACEMENT_3D('',#76132,#61336,#61337);
#53010=AXIS2_PLACEMENT_3D('',#76134,#61338,#61339);
#53011=AXIS2_PLACEMENT_3D('',#76138,#61341,#61342);
#53012=AXIS2_PLACEMENT_3D('',#76140,#61343,#61344);
#53013=AXIS2_PLACEMENT_3D('',#76142,#61345,#61346);
#53014=AXIS2_PLACEMENT_3D('',#76144,#61347,#61348);
#53015=AXIS2_PLACEMENT_3D('',#76146,#61349,#61350);
#53016=AXIS2_PLACEMENT_3D('',#76148,#61352,#61353);
#53017=AXIS2_PLACEMENT_3D('',#76150,#61355,#61356);
#53018=AXIS2_PLACEMENT_3D('',#76152,#61358,#61359);
#53019=AXIS2_PLACEMENT_3D('',#76154,#61361,#61362);
#53020=AXIS2_PLACEMENT_3D('',#76156,#61364,#61365);
#53021=AXIS2_PLACEMENT_3D('',#76158,#61367,#61368);
#53022=AXIS2_PLACEMENT_3D('',#76160,#61370,#61371);
#53023=AXIS2_PLACEMENT_3D('',#76162,#61373,#61374);
#53024=AXIS2_PLACEMENT_3D('',#76164,#61376,#61377);
#53025=AXIS2_PLACEMENT_3D('',#76166,#61379,#61380);
#53026=AXIS2_PLACEMENT_3D('',#76168,#61382,#61383);
#53027=AXIS2_PLACEMENT_3D('',#76170,#61385,#61386);
#53028=AXIS2_PLACEMENT_3D('',#76172,#61388,#61389);
#53029=AXIS2_PLACEMENT_3D('',#76174,#61391,#61392);
#53030=AXIS2_PLACEMENT_3D('',#76178,#61393,#61394);
#53031=AXIS2_PLACEMENT_3D('',#76182,#61397,#61398);
#53032=AXIS2_PLACEMENT_3D('',#76184,#61399,#61400);
#53033=AXIS2_PLACEMENT_3D('',#76186,#61402,#61403);
#53034=AXIS2_PLACEMENT_3D('',#76188,#61404,#61405);
#53035=AXIS2_PLACEMENT_3D('',#76190,#61407,#61408);
#53036=AXIS2_PLACEMENT_3D('',#76192,#61409,#61410);
#53037=AXIS2_PLACEMENT_3D('',#76194,#61412,#61413);
#53038=AXIS2_PLACEMENT_3D('',#76196,#61414,#61415);
#53039=AXIS2_PLACEMENT_3D('',#76198,#61417,#61418);
#53040=AXIS2_PLACEMENT_3D('',#76200,#61419,#61420);
#53041=AXIS2_PLACEMENT_3D('',#76202,#61422,#61423);
#53042=AXIS2_PLACEMENT_3D('',#76206,#61426,#61427);
#53043=AXIS2_PLACEMENT_3D('',#76208,#61428,#61429);
#53044=AXIS2_PLACEMENT_3D('',#76210,#61431,#61432);
#53045=AXIS2_PLACEMENT_3D('',#76212,#61433,#61434);
#53046=AXIS2_PLACEMENT_3D('',#76214,#61436,#61437);
#53047=AXIS2_PLACEMENT_3D('',#76216,#61438,#61439);
#53048=AXIS2_PLACEMENT_3D('',#76218,#61441,#61442);
#53049=AXIS2_PLACEMENT_3D('',#76220,#61443,#61444);
#53050=AXIS2_PLACEMENT_3D('',#76222,#61446,#61447);
#53051=AXIS2_PLACEMENT_3D('',#76224,#61448,#61449);
#53052=AXIS2_PLACEMENT_3D('',#76226,#61451,#61452);
#53053=AXIS2_PLACEMENT_3D('',#76228,#61454,#61455);
#53054=AXIS2_PLACEMENT_3D('',#76229,#61456,#61457);
#53055=AXIS2_PLACEMENT_3D('',#76231,#61458,#61459);
#53056=AXIS2_PLACEMENT_3D('',#76233,#61460,#61461);
#53057=AXIS2_PLACEMENT_3D('',#76237,#61463,#61464);
#53058=AXIS2_PLACEMENT_3D('',#76239,#61465,#61466);
#53059=AXIS2_PLACEMENT_3D('',#76241,#61467,#61468);
#53060=AXIS2_PLACEMENT_3D('',#76243,#61469,#61470);
#53061=AXIS2_PLACEMENT_3D('',#76245,#61471,#61472);
#53062=AXIS2_PLACEMENT_3D('',#76249,#61474,#61475);
#53063=AXIS2_PLACEMENT_3D('',#76251,#61476,#61477);
#53064=AXIS2_PLACEMENT_3D('',#76253,#61478,#61479);
#53065=AXIS2_PLACEMENT_3D('',#76255,#61480,#61481);
#53066=AXIS2_PLACEMENT_3D('',#76257,#61482,#61483);
#53067=AXIS2_PLACEMENT_3D('',#76259,#61485,#61486);
#53068=AXIS2_PLACEMENT_3D('',#76261,#61488,#61489);
#53069=AXIS2_PLACEMENT_3D('',#76263,#61491,#61492);
#53070=AXIS2_PLACEMENT_3D('',#76265,#61494,#61495);
#53071=AXIS2_PLACEMENT_3D('',#76267,#61497,#61498);
#53072=AXIS2_PLACEMENT_3D('',#76269,#61500,#61501);
#53073=AXIS2_PLACEMENT_3D('',#76271,#61503,#61504);
#53074=AXIS2_PLACEMENT_3D('',#76273,#61506,#61507);
#53075=AXIS2_PLACEMENT_3D('',#76275,#61509,#61510);
#53076=AXIS2_PLACEMENT_3D('',#76277,#61512,#61513);
#53077=AXIS2_PLACEMENT_3D('',#76279,#61515,#61516);
#53078=AXIS2_PLACEMENT_3D('',#76281,#61518,#61519);
#53079=AXIS2_PLACEMENT_3D('',#76283,#61521,#61522);
#53080=AXIS2_PLACEMENT_3D('',#76285,#61524,#61525);
#53081=AXIS2_PLACEMENT_3D('',#76289,#61526,#61527);
#53082=AXIS2_PLACEMENT_3D('',#76293,#61530,#61531);
#53083=AXIS2_PLACEMENT_3D('',#76295,#61532,#61533);
#53084=AXIS2_PLACEMENT_3D('',#76297,#61535,#61536);
#53085=AXIS2_PLACEMENT_3D('',#76299,#61537,#61538);
#53086=AXIS2_PLACEMENT_3D('',#76301,#61540,#61541);
#53087=AXIS2_PLACEMENT_3D('',#76303,#61542,#61543);
#53088=AXIS2_PLACEMENT_3D('',#76305,#61545,#61546);
#53089=AXIS2_PLACEMENT_3D('',#76307,#61547,#61548);
#53090=AXIS2_PLACEMENT_3D('',#76309,#61550,#61551);
#53091=AXIS2_PLACEMENT_3D('',#76311,#61552,#61553);
#53092=AXIS2_PLACEMENT_3D('',#76313,#61555,#61556);
#53093=AXIS2_PLACEMENT_3D('',#76317,#61559,#61560);
#53094=AXIS2_PLACEMENT_3D('',#76319,#61561,#61562);
#53095=AXIS2_PLACEMENT_3D('',#76321,#61564,#61565);
#53096=AXIS2_PLACEMENT_3D('',#76323,#61566,#61567);
#53097=AXIS2_PLACEMENT_3D('',#76325,#61569,#61570);
#53098=AXIS2_PLACEMENT_3D('',#76327,#61571,#61572);
#53099=AXIS2_PLACEMENT_3D('',#76329,#61574,#61575);
#53100=AXIS2_PLACEMENT_3D('',#76331,#61576,#61577);
#53101=AXIS2_PLACEMENT_3D('',#76333,#61579,#61580);
#53102=AXIS2_PLACEMENT_3D('',#76335,#61581,#61582);
#53103=AXIS2_PLACEMENT_3D('',#76337,#61584,#61585);
#53104=AXIS2_PLACEMENT_3D('',#76339,#61587,#61588);
#53105=AXIS2_PLACEMENT_3D('',#76340,#61589,#61590);
#53106=AXIS2_PLACEMENT_3D('',#76342,#61591,#61592);
#53107=AXIS2_PLACEMENT_3D('',#76344,#61593,#61594);
#53108=AXIS2_PLACEMENT_3D('',#76348,#61596,#61597);
#53109=AXIS2_PLACEMENT_3D('',#76350,#61598,#61599);
#53110=AXIS2_PLACEMENT_3D('',#76352,#61600,#61601);
#53111=AXIS2_PLACEMENT_3D('',#76354,#61602,#61603);
#53112=AXIS2_PLACEMENT_3D('',#76356,#61604,#61605);
#53113=AXIS2_PLACEMENT_3D('',#76360,#61607,#61608);
#53114=AXIS2_PLACEMENT_3D('',#76362,#61609,#61610);
#53115=AXIS2_PLACEMENT_3D('',#76364,#61611,#61612);
#53116=AXIS2_PLACEMENT_3D('',#76366,#61613,#61614);
#53117=AXIS2_PLACEMENT_3D('',#76368,#61615,#61616);
#53118=AXIS2_PLACEMENT_3D('',#76370,#61618,#61619);
#53119=AXIS2_PLACEMENT_3D('',#76372,#61621,#61622);
#53120=AXIS2_PLACEMENT_3D('',#76374,#61624,#61625);
#53121=AXIS2_PLACEMENT_3D('',#76376,#61627,#61628);
#53122=AXIS2_PLACEMENT_3D('',#76378,#61630,#61631);
#53123=AXIS2_PLACEMENT_3D('',#76380,#61633,#61634);
#53124=AXIS2_PLACEMENT_3D('',#76382,#61636,#61637);
#53125=AXIS2_PLACEMENT_3D('',#76384,#61639,#61640);
#53126=AXIS2_PLACEMENT_3D('',#76386,#61642,#61643);
#53127=AXIS2_PLACEMENT_3D('',#76388,#61645,#61646);
#53128=AXIS2_PLACEMENT_3D('',#76390,#61648,#61649);
#53129=AXIS2_PLACEMENT_3D('',#76392,#61651,#61652);
#53130=AXIS2_PLACEMENT_3D('',#76394,#61654,#61655);
#53131=AXIS2_PLACEMENT_3D('',#76396,#61657,#61658);
#53132=AXIS2_PLACEMENT_3D('',#76400,#61659,#61660);
#53133=AXIS2_PLACEMENT_3D('',#76404,#61663,#61664);
#53134=AXIS2_PLACEMENT_3D('',#76406,#61665,#61666);
#53135=AXIS2_PLACEMENT_3D('',#76408,#61668,#61669);
#53136=AXIS2_PLACEMENT_3D('',#76410,#61670,#61671);
#53137=AXIS2_PLACEMENT_3D('',#76412,#61673,#61674);
#53138=AXIS2_PLACEMENT_3D('',#76414,#61675,#61676);
#53139=AXIS2_PLACEMENT_3D('',#76416,#61678,#61679);
#53140=AXIS2_PLACEMENT_3D('',#76418,#61680,#61681);
#53141=AXIS2_PLACEMENT_3D('',#76420,#61683,#61684);
#53142=AXIS2_PLACEMENT_3D('',#76422,#61685,#61686);
#53143=AXIS2_PLACEMENT_3D('',#76424,#61688,#61689);
#53144=AXIS2_PLACEMENT_3D('',#76428,#61692,#61693);
#53145=AXIS2_PLACEMENT_3D('',#76430,#61694,#61695);
#53146=AXIS2_PLACEMENT_3D('',#76432,#61697,#61698);
#53147=AXIS2_PLACEMENT_3D('',#76434,#61699,#61700);
#53148=AXIS2_PLACEMENT_3D('',#76436,#61702,#61703);
#53149=AXIS2_PLACEMENT_3D('',#76438,#61704,#61705);
#53150=AXIS2_PLACEMENT_3D('',#76440,#61707,#61708);
#53151=AXIS2_PLACEMENT_3D('',#76442,#61709,#61710);
#53152=AXIS2_PLACEMENT_3D('',#76444,#61712,#61713);
#53153=AXIS2_PLACEMENT_3D('',#76446,#61714,#61715);
#53154=AXIS2_PLACEMENT_3D('',#76448,#61717,#61718);
#53155=AXIS2_PLACEMENT_3D('',#76450,#61720,#61721);
#53156=AXIS2_PLACEMENT_3D('',#76451,#61722,#61723);
#53157=AXIS2_PLACEMENT_3D('',#76453,#61724,#61725);
#53158=AXIS2_PLACEMENT_3D('',#76455,#61726,#61727);
#53159=AXIS2_PLACEMENT_3D('',#76459,#61729,#61730);
#53160=AXIS2_PLACEMENT_3D('',#76461,#61731,#61732);
#53161=AXIS2_PLACEMENT_3D('',#76463,#61733,#61734);
#53162=AXIS2_PLACEMENT_3D('',#76465,#61735,#61736);
#53163=AXIS2_PLACEMENT_3D('',#76467,#61737,#61738);
#53164=AXIS2_PLACEMENT_3D('',#76471,#61740,#61741);
#53165=AXIS2_PLACEMENT_3D('',#76473,#61742,#61743);
#53166=AXIS2_PLACEMENT_3D('',#76475,#61744,#61745);
#53167=AXIS2_PLACEMENT_3D('',#76477,#61746,#61747);
#53168=AXIS2_PLACEMENT_3D('',#76479,#61748,#61749);
#53169=AXIS2_PLACEMENT_3D('',#76481,#61751,#61752);
#53170=AXIS2_PLACEMENT_3D('',#76483,#61754,#61755);
#53171=AXIS2_PLACEMENT_3D('',#76485,#61757,#61758);
#53172=AXIS2_PLACEMENT_3D('',#76487,#61760,#61761);
#53173=AXIS2_PLACEMENT_3D('',#76489,#61763,#61764);
#53174=AXIS2_PLACEMENT_3D('',#76491,#61766,#61767);
#53175=AXIS2_PLACEMENT_3D('',#76493,#61769,#61770);
#53176=AXIS2_PLACEMENT_3D('',#76495,#61772,#61773);
#53177=AXIS2_PLACEMENT_3D('',#76497,#61775,#61776);
#53178=AXIS2_PLACEMENT_3D('',#76499,#61778,#61779);
#53179=AXIS2_PLACEMENT_3D('',#76501,#61781,#61782);
#53180=AXIS2_PLACEMENT_3D('',#76503,#61784,#61785);
#53181=AXIS2_PLACEMENT_3D('',#76505,#61787,#61788);
#53182=AXIS2_PLACEMENT_3D('',#76507,#61790,#61791);
#53183=AXIS2_PLACEMENT_3D('',#76511,#61792,#61793);
#53184=AXIS2_PLACEMENT_3D('',#76515,#61796,#61797);
#53185=AXIS2_PLACEMENT_3D('',#76517,#61798,#61799);
#53186=AXIS2_PLACEMENT_3D('',#76519,#61801,#61802);
#53187=AXIS2_PLACEMENT_3D('',#76521,#61803,#61804);
#53188=AXIS2_PLACEMENT_3D('',#76523,#61806,#61807);
#53189=AXIS2_PLACEMENT_3D('',#76525,#61808,#61809);
#53190=AXIS2_PLACEMENT_3D('',#76527,#61811,#61812);
#53191=AXIS2_PLACEMENT_3D('',#76529,#61813,#61814);
#53192=AXIS2_PLACEMENT_3D('',#76531,#61816,#61817);
#53193=AXIS2_PLACEMENT_3D('',#76533,#61818,#61819);
#53194=AXIS2_PLACEMENT_3D('',#76535,#61821,#61822);
#53195=AXIS2_PLACEMENT_3D('',#76539,#61825,#61826);
#53196=AXIS2_PLACEMENT_3D('',#76541,#61827,#61828);
#53197=AXIS2_PLACEMENT_3D('',#76543,#61830,#61831);
#53198=AXIS2_PLACEMENT_3D('',#76545,#61832,#61833);
#53199=AXIS2_PLACEMENT_3D('',#76547,#61835,#61836);
#53200=AXIS2_PLACEMENT_3D('',#76549,#61837,#61838);
#53201=AXIS2_PLACEMENT_3D('',#76551,#61840,#61841);
#53202=AXIS2_PLACEMENT_3D('',#76553,#61842,#61843);
#53203=AXIS2_PLACEMENT_3D('',#76555,#61845,#61846);
#53204=AXIS2_PLACEMENT_3D('',#76557,#61847,#61848);
#53205=AXIS2_PLACEMENT_3D('',#76559,#61850,#61851);
#53206=AXIS2_PLACEMENT_3D('',#76561,#61853,#61854);
#53207=AXIS2_PLACEMENT_3D('',#76562,#61855,#61856);
#53208=AXIS2_PLACEMENT_3D('',#76564,#61857,#61858);
#53209=AXIS2_PLACEMENT_3D('',#76566,#61859,#61860);
#53210=AXIS2_PLACEMENT_3D('',#76570,#61862,#61863);
#53211=AXIS2_PLACEMENT_3D('',#76572,#61864,#61865);
#53212=AXIS2_PLACEMENT_3D('',#76574,#61866,#61867);
#53213=AXIS2_PLACEMENT_3D('',#76576,#61868,#61869);
#53214=AXIS2_PLACEMENT_3D('',#76578,#61870,#61871);
#53215=AXIS2_PLACEMENT_3D('',#76582,#61873,#61874);
#53216=AXIS2_PLACEMENT_3D('',#76584,#61875,#61876);
#53217=AXIS2_PLACEMENT_3D('',#76586,#61877,#61878);
#53218=AXIS2_PLACEMENT_3D('',#76588,#61879,#61880);
#53219=AXIS2_PLACEMENT_3D('',#76590,#61881,#61882);
#53220=AXIS2_PLACEMENT_3D('',#76592,#61884,#61885);
#53221=AXIS2_PLACEMENT_3D('',#76594,#61887,#61888);
#53222=AXIS2_PLACEMENT_3D('',#76596,#61890,#61891);
#53223=AXIS2_PLACEMENT_3D('',#76598,#61893,#61894);
#53224=AXIS2_PLACEMENT_3D('',#76600,#61896,#61897);
#53225=AXIS2_PLACEMENT_3D('',#76602,#61899,#61900);
#53226=AXIS2_PLACEMENT_3D('',#76604,#61902,#61903);
#53227=AXIS2_PLACEMENT_3D('',#76606,#61905,#61906);
#53228=AXIS2_PLACEMENT_3D('',#76608,#61908,#61909);
#53229=AXIS2_PLACEMENT_3D('',#76610,#61911,#61912);
#53230=AXIS2_PLACEMENT_3D('',#76612,#61914,#61915);
#53231=AXIS2_PLACEMENT_3D('',#76614,#61917,#61918);
#53232=AXIS2_PLACEMENT_3D('',#76616,#61920,#61921);
#53233=AXIS2_PLACEMENT_3D('',#76618,#61923,#61924);
#53234=AXIS2_PLACEMENT_3D('',#76622,#61925,#61926);
#53235=AXIS2_PLACEMENT_3D('',#76626,#61929,#61930);
#53236=AXIS2_PLACEMENT_3D('',#76628,#61931,#61932);
#53237=AXIS2_PLACEMENT_3D('',#76630,#61934,#61935);
#53238=AXIS2_PLACEMENT_3D('',#76632,#61936,#61937);
#53239=AXIS2_PLACEMENT_3D('',#76634,#61939,#61940);
#53240=AXIS2_PLACEMENT_3D('',#76636,#61941,#61942);
#53241=AXIS2_PLACEMENT_3D('',#76638,#61944,#61945);
#53242=AXIS2_PLACEMENT_3D('',#76640,#61946,#61947);
#53243=AXIS2_PLACEMENT_3D('',#76642,#61949,#61950);
#53244=AXIS2_PLACEMENT_3D('',#76644,#61951,#61952);
#53245=AXIS2_PLACEMENT_3D('',#76646,#61954,#61955);
#53246=AXIS2_PLACEMENT_3D('',#76650,#61958,#61959);
#53247=AXIS2_PLACEMENT_3D('',#76652,#61960,#61961);
#53248=AXIS2_PLACEMENT_3D('',#76654,#61963,#61964);
#53249=AXIS2_PLACEMENT_3D('',#76656,#61965,#61966);
#53250=AXIS2_PLACEMENT_3D('',#76658,#61968,#61969);
#53251=AXIS2_PLACEMENT_3D('',#76660,#61970,#61971);
#53252=AXIS2_PLACEMENT_3D('',#76662,#61973,#61974);
#53253=AXIS2_PLACEMENT_3D('',#76664,#61975,#61976);
#53254=AXIS2_PLACEMENT_3D('',#76666,#61978,#61979);
#53255=AXIS2_PLACEMENT_3D('',#76668,#61980,#61981);
#53256=AXIS2_PLACEMENT_3D('',#76670,#61983,#61984);
#53257=AXIS2_PLACEMENT_3D('',#76672,#61986,#61987);
#53258=AXIS2_PLACEMENT_3D('',#76673,#61988,#61989);
#53259=AXIS2_PLACEMENT_3D('',#76675,#61990,#61991);
#53260=AXIS2_PLACEMENT_3D('',#76677,#61992,#61993);
#53261=AXIS2_PLACEMENT_3D('',#76681,#61995,#61996);
#53262=AXIS2_PLACEMENT_3D('',#76683,#61997,#61998);
#53263=AXIS2_PLACEMENT_3D('',#76685,#61999,#62000);
#53264=AXIS2_PLACEMENT_3D('',#76687,#62001,#62002);
#53265=AXIS2_PLACEMENT_3D('',#76689,#62003,#62004);
#53266=AXIS2_PLACEMENT_3D('',#76693,#62006,#62007);
#53267=AXIS2_PLACEMENT_3D('',#76695,#62008,#62009);
#53268=AXIS2_PLACEMENT_3D('',#76697,#62010,#62011);
#53269=AXIS2_PLACEMENT_3D('',#76699,#62012,#62013);
#53270=AXIS2_PLACEMENT_3D('',#76701,#62014,#62015);
#53271=AXIS2_PLACEMENT_3D('',#76703,#62017,#62018);
#53272=AXIS2_PLACEMENT_3D('',#76705,#62020,#62021);
#53273=AXIS2_PLACEMENT_3D('',#76707,#62023,#62024);
#53274=AXIS2_PLACEMENT_3D('',#76709,#62026,#62027);
#53275=AXIS2_PLACEMENT_3D('',#76711,#62029,#62030);
#53276=AXIS2_PLACEMENT_3D('',#76713,#62032,#62033);
#53277=AXIS2_PLACEMENT_3D('',#76715,#62035,#62036);
#53278=AXIS2_PLACEMENT_3D('',#76717,#62038,#62039);
#53279=AXIS2_PLACEMENT_3D('',#76719,#62041,#62042);
#53280=AXIS2_PLACEMENT_3D('',#76721,#62044,#62045);
#53281=AXIS2_PLACEMENT_3D('',#76723,#62047,#62048);
#53282=AXIS2_PLACEMENT_3D('',#76725,#62050,#62051);
#53283=AXIS2_PLACEMENT_3D('',#76727,#62053,#62054);
#53284=AXIS2_PLACEMENT_3D('',#76729,#62056,#62057);
#53285=AXIS2_PLACEMENT_3D('',#76733,#62058,#62059);
#53286=AXIS2_PLACEMENT_3D('',#76737,#62062,#62063);
#53287=AXIS2_PLACEMENT_3D('',#76739,#62064,#62065);
#53288=AXIS2_PLACEMENT_3D('',#76741,#62067,#62068);
#53289=AXIS2_PLACEMENT_3D('',#76743,#62069,#62070);
#53290=AXIS2_PLACEMENT_3D('',#76745,#62072,#62073);
#53291=AXIS2_PLACEMENT_3D('',#76747,#62074,#62075);
#53292=AXIS2_PLACEMENT_3D('',#76749,#62077,#62078);
#53293=AXIS2_PLACEMENT_3D('',#76751,#62079,#62080);
#53294=AXIS2_PLACEMENT_3D('',#76753,#62082,#62083);
#53295=AXIS2_PLACEMENT_3D('',#76755,#62084,#62085);
#53296=AXIS2_PLACEMENT_3D('',#76757,#62087,#62088);
#53297=AXIS2_PLACEMENT_3D('',#76761,#62091,#62092);
#53298=AXIS2_PLACEMENT_3D('',#76763,#62093,#62094);
#53299=AXIS2_PLACEMENT_3D('',#76765,#62096,#62097);
#53300=AXIS2_PLACEMENT_3D('',#76767,#62098,#62099);
#53301=AXIS2_PLACEMENT_3D('',#76769,#62101,#62102);
#53302=AXIS2_PLACEMENT_3D('',#76771,#62103,#62104);
#53303=AXIS2_PLACEMENT_3D('',#76773,#62106,#62107);
#53304=AXIS2_PLACEMENT_3D('',#76775,#62108,#62109);
#53305=AXIS2_PLACEMENT_3D('',#76777,#62111,#62112);
#53306=AXIS2_PLACEMENT_3D('',#76779,#62113,#62114);
#53307=AXIS2_PLACEMENT_3D('',#76781,#62116,#62117);
#53308=AXIS2_PLACEMENT_3D('',#76783,#62119,#62120);
#53309=AXIS2_PLACEMENT_3D('',#76784,#62121,#62122);
#53310=AXIS2_PLACEMENT_3D('',#76786,#62123,#62124);
#53311=AXIS2_PLACEMENT_3D('',#76788,#62125,#62126);
#53312=AXIS2_PLACEMENT_3D('',#76792,#62128,#62129);
#53313=AXIS2_PLACEMENT_3D('',#76794,#62130,#62131);
#53314=AXIS2_PLACEMENT_3D('',#76796,#62132,#62133);
#53315=AXIS2_PLACEMENT_3D('',#76798,#62134,#62135);
#53316=AXIS2_PLACEMENT_3D('',#76800,#62136,#62137);
#53317=AXIS2_PLACEMENT_3D('',#76804,#62139,#62140);
#53318=AXIS2_PLACEMENT_3D('',#76806,#62141,#62142);
#53319=AXIS2_PLACEMENT_3D('',#76808,#62143,#62144);
#53320=AXIS2_PLACEMENT_3D('',#76810,#62145,#62146);
#53321=AXIS2_PLACEMENT_3D('',#76812,#62147,#62148);
#53322=AXIS2_PLACEMENT_3D('',#76814,#62150,#62151);
#53323=AXIS2_PLACEMENT_3D('',#76816,#62153,#62154);
#53324=AXIS2_PLACEMENT_3D('',#76818,#62156,#62157);
#53325=AXIS2_PLACEMENT_3D('',#76820,#62159,#62160);
#53326=AXIS2_PLACEMENT_3D('',#76822,#62162,#62163);
#53327=AXIS2_PLACEMENT_3D('',#76824,#62165,#62166);
#53328=AXIS2_PLACEMENT_3D('',#76826,#62168,#62169);
#53329=AXIS2_PLACEMENT_3D('',#76828,#62171,#62172);
#53330=AXIS2_PLACEMENT_3D('',#76830,#62174,#62175);
#53331=AXIS2_PLACEMENT_3D('',#76832,#62177,#62178);
#53332=AXIS2_PLACEMENT_3D('',#76834,#62180,#62181);
#53333=AXIS2_PLACEMENT_3D('',#76836,#62183,#62184);
#53334=AXIS2_PLACEMENT_3D('',#76838,#62186,#62187);
#53335=AXIS2_PLACEMENT_3D('',#76840,#62189,#62190);
#53336=AXIS2_PLACEMENT_3D('',#76844,#62191,#62192);
#53337=AXIS2_PLACEMENT_3D('',#76848,#62195,#62196);
#53338=AXIS2_PLACEMENT_3D('',#76850,#62197,#62198);
#53339=AXIS2_PLACEMENT_3D('',#76852,#62200,#62201);
#53340=AXIS2_PLACEMENT_3D('',#76854,#62202,#62203);
#53341=AXIS2_PLACEMENT_3D('',#76856,#62205,#62206);
#53342=AXIS2_PLACEMENT_3D('',#76858,#62207,#62208);
#53343=AXIS2_PLACEMENT_3D('',#76860,#62210,#62211);
#53344=AXIS2_PLACEMENT_3D('',#76862,#62212,#62213);
#53345=AXIS2_PLACEMENT_3D('',#76864,#62215,#62216);
#53346=AXIS2_PLACEMENT_3D('',#76866,#62217,#62218);
#53347=AXIS2_PLACEMENT_3D('',#76868,#62220,#62221);
#53348=AXIS2_PLACEMENT_3D('',#76872,#62224,#62225);
#53349=AXIS2_PLACEMENT_3D('',#76874,#62226,#62227);
#53350=AXIS2_PLACEMENT_3D('',#76876,#62229,#62230);
#53351=AXIS2_PLACEMENT_3D('',#76878,#62231,#62232);
#53352=AXIS2_PLACEMENT_3D('',#76880,#62234,#62235);
#53353=AXIS2_PLACEMENT_3D('',#76882,#62236,#62237);
#53354=AXIS2_PLACEMENT_3D('',#76884,#62239,#62240);
#53355=AXIS2_PLACEMENT_3D('',#76886,#62241,#62242);
#53356=AXIS2_PLACEMENT_3D('',#76888,#62244,#62245);
#53357=AXIS2_PLACEMENT_3D('',#76890,#62246,#62247);
#53358=AXIS2_PLACEMENT_3D('',#76892,#62249,#62250);
#53359=AXIS2_PLACEMENT_3D('',#76894,#62252,#62253);
#53360=AXIS2_PLACEMENT_3D('',#76895,#62254,#62255);
#53361=AXIS2_PLACEMENT_3D('',#76897,#62256,#62257);
#53362=AXIS2_PLACEMENT_3D('',#76899,#62258,#62259);
#53363=AXIS2_PLACEMENT_3D('',#76903,#62261,#62262);
#53364=AXIS2_PLACEMENT_3D('',#76905,#62263,#62264);
#53365=AXIS2_PLACEMENT_3D('',#76907,#62265,#62266);
#53366=AXIS2_PLACEMENT_3D('',#76909,#62267,#62268);
#53367=AXIS2_PLACEMENT_3D('',#76911,#62269,#62270);
#53368=AXIS2_PLACEMENT_3D('',#76915,#62272,#62273);
#53369=AXIS2_PLACEMENT_3D('',#76917,#62274,#62275);
#53370=AXIS2_PLACEMENT_3D('',#76919,#62276,#62277);
#53371=AXIS2_PLACEMENT_3D('',#76921,#62278,#62279);
#53372=AXIS2_PLACEMENT_3D('',#76923,#62280,#62281);
#53373=AXIS2_PLACEMENT_3D('',#76925,#62283,#62284);
#53374=AXIS2_PLACEMENT_3D('',#76927,#62286,#62287);
#53375=AXIS2_PLACEMENT_3D('',#76929,#62289,#62290);
#53376=AXIS2_PLACEMENT_3D('',#76931,#62292,#62293);
#53377=AXIS2_PLACEMENT_3D('',#76933,#62295,#62296);
#53378=AXIS2_PLACEMENT_3D('',#76935,#62298,#62299);
#53379=AXIS2_PLACEMENT_3D('',#76937,#62301,#62302);
#53380=AXIS2_PLACEMENT_3D('',#76939,#62304,#62305);
#53381=AXIS2_PLACEMENT_3D('',#76941,#62307,#62308);
#53382=AXIS2_PLACEMENT_3D('',#76943,#62310,#62311);
#53383=AXIS2_PLACEMENT_3D('',#76945,#62313,#62314);
#53384=AXIS2_PLACEMENT_3D('',#76947,#62316,#62317);
#53385=AXIS2_PLACEMENT_3D('',#76949,#62319,#62320);
#53386=AXIS2_PLACEMENT_3D('',#76951,#62322,#62323);
#53387=AXIS2_PLACEMENT_3D('',#76955,#62324,#62325);
#53388=AXIS2_PLACEMENT_3D('',#76959,#62328,#62329);
#53389=AXIS2_PLACEMENT_3D('',#76961,#62330,#62331);
#53390=AXIS2_PLACEMENT_3D('',#76963,#62333,#62334);
#53391=AXIS2_PLACEMENT_3D('',#76965,#62335,#62336);
#53392=AXIS2_PLACEMENT_3D('',#76967,#62338,#62339);
#53393=AXIS2_PLACEMENT_3D('',#76969,#62340,#62341);
#53394=AXIS2_PLACEMENT_3D('',#76971,#62343,#62344);
#53395=AXIS2_PLACEMENT_3D('',#76973,#62345,#62346);
#53396=AXIS2_PLACEMENT_3D('',#76975,#62348,#62349);
#53397=AXIS2_PLACEMENT_3D('',#76977,#62350,#62351);
#53398=AXIS2_PLACEMENT_3D('',#76979,#62353,#62354);
#53399=AXIS2_PLACEMENT_3D('',#76983,#62357,#62358);
#53400=AXIS2_PLACEMENT_3D('',#76985,#62359,#62360);
#53401=AXIS2_PLACEMENT_3D('',#76987,#62362,#62363);
#53402=AXIS2_PLACEMENT_3D('',#76989,#62364,#62365);
#53403=AXIS2_PLACEMENT_3D('',#76991,#62367,#62368);
#53404=AXIS2_PLACEMENT_3D('',#76993,#62369,#62370);
#53405=AXIS2_PLACEMENT_3D('',#76995,#62372,#62373);
#53406=AXIS2_PLACEMENT_3D('',#76997,#62374,#62375);
#53407=AXIS2_PLACEMENT_3D('',#76999,#62377,#62378);
#53408=AXIS2_PLACEMENT_3D('',#77001,#62379,#62380);
#53409=AXIS2_PLACEMENT_3D('',#77003,#62382,#62383);
#53410=AXIS2_PLACEMENT_3D('',#77005,#62385,#62386);
#53411=AXIS2_PLACEMENT_3D('',#77006,#62387,#62388);
#53412=AXIS2_PLACEMENT_3D('',#77008,#62389,#62390);
#53413=AXIS2_PLACEMENT_3D('',#77010,#62391,#62392);
#53414=AXIS2_PLACEMENT_3D('',#77014,#62394,#62395);
#53415=AXIS2_PLACEMENT_3D('',#77016,#62396,#62397);
#53416=AXIS2_PLACEMENT_3D('',#77018,#62398,#62399);
#53417=AXIS2_PLACEMENT_3D('',#77020,#62400,#62401);
#53418=AXIS2_PLACEMENT_3D('',#77022,#62402,#62403);
#53419=AXIS2_PLACEMENT_3D('',#77026,#62405,#62406);
#53420=AXIS2_PLACEMENT_3D('',#77028,#62407,#62408);
#53421=AXIS2_PLACEMENT_3D('',#77030,#62409,#62410);
#53422=AXIS2_PLACEMENT_3D('',#77032,#62411,#62412);
#53423=AXIS2_PLACEMENT_3D('',#77034,#62413,#62414);
#53424=AXIS2_PLACEMENT_3D('',#77036,#62416,#62417);
#53425=AXIS2_PLACEMENT_3D('',#77038,#62419,#62420);
#53426=AXIS2_PLACEMENT_3D('',#77040,#62422,#62423);
#53427=AXIS2_PLACEMENT_3D('',#77042,#62425,#62426);
#53428=AXIS2_PLACEMENT_3D('',#77044,#62428,#62429);
#53429=AXIS2_PLACEMENT_3D('',#77046,#62431,#62432);
#53430=AXIS2_PLACEMENT_3D('',#77048,#62434,#62435);
#53431=AXIS2_PLACEMENT_3D('',#77050,#62437,#62438);
#53432=AXIS2_PLACEMENT_3D('',#77052,#62440,#62441);
#53433=AXIS2_PLACEMENT_3D('',#77054,#62443,#62444);
#53434=AXIS2_PLACEMENT_3D('',#77056,#62446,#62447);
#53435=AXIS2_PLACEMENT_3D('',#77058,#62449,#62450);
#53436=AXIS2_PLACEMENT_3D('',#77060,#62452,#62453);
#53437=AXIS2_PLACEMENT_3D('',#77062,#62455,#62456);
#53438=AXIS2_PLACEMENT_3D('',#77066,#62457,#62458);
#53439=AXIS2_PLACEMENT_3D('',#77070,#62461,#62462);
#53440=AXIS2_PLACEMENT_3D('',#77072,#62463,#62464);
#53441=AXIS2_PLACEMENT_3D('',#77074,#62466,#62467);
#53442=AXIS2_PLACEMENT_3D('',#77076,#62468,#62469);
#53443=AXIS2_PLACEMENT_3D('',#77078,#62471,#62472);
#53444=AXIS2_PLACEMENT_3D('',#77080,#62473,#62474);
#53445=AXIS2_PLACEMENT_3D('',#77082,#62476,#62477);
#53446=AXIS2_PLACEMENT_3D('',#77084,#62478,#62479);
#53447=AXIS2_PLACEMENT_3D('',#77086,#62481,#62482);
#53448=AXIS2_PLACEMENT_3D('',#77088,#62483,#62484);
#53449=AXIS2_PLACEMENT_3D('',#77090,#62486,#62487);
#53450=AXIS2_PLACEMENT_3D('',#77094,#62490,#62491);
#53451=AXIS2_PLACEMENT_3D('',#77096,#62492,#62493);
#53452=AXIS2_PLACEMENT_3D('',#77098,#62495,#62496);
#53453=AXIS2_PLACEMENT_3D('',#77100,#62497,#62498);
#53454=AXIS2_PLACEMENT_3D('',#77102,#62500,#62501);
#53455=AXIS2_PLACEMENT_3D('',#77104,#62502,#62503);
#53456=AXIS2_PLACEMENT_3D('',#77106,#62505,#62506);
#53457=AXIS2_PLACEMENT_3D('',#77108,#62507,#62508);
#53458=AXIS2_PLACEMENT_3D('',#77110,#62510,#62511);
#53459=AXIS2_PLACEMENT_3D('',#77112,#62512,#62513);
#53460=AXIS2_PLACEMENT_3D('',#77114,#62515,#62516);
#53461=AXIS2_PLACEMENT_3D('',#77116,#62518,#62519);
#53462=AXIS2_PLACEMENT_3D('',#77117,#62520,#62521);
#53463=AXIS2_PLACEMENT_3D('',#77119,#62522,#62523);
#53464=AXIS2_PLACEMENT_3D('',#77121,#62524,#62525);
#53465=AXIS2_PLACEMENT_3D('',#77125,#62527,#62528);
#53466=AXIS2_PLACEMENT_3D('',#77127,#62529,#62530);
#53467=AXIS2_PLACEMENT_3D('',#77129,#62531,#62532);
#53468=AXIS2_PLACEMENT_3D('',#77131,#62533,#62534);
#53469=AXIS2_PLACEMENT_3D('',#77133,#62535,#62536);
#53470=AXIS2_PLACEMENT_3D('',#77137,#62538,#62539);
#53471=AXIS2_PLACEMENT_3D('',#77139,#62540,#62541);
#53472=AXIS2_PLACEMENT_3D('',#77141,#62542,#62543);
#53473=AXIS2_PLACEMENT_3D('',#77143,#62544,#62545);
#53474=AXIS2_PLACEMENT_3D('',#77145,#62546,#62547);
#53475=AXIS2_PLACEMENT_3D('',#77147,#62549,#62550);
#53476=AXIS2_PLACEMENT_3D('',#77149,#62552,#62553);
#53477=AXIS2_PLACEMENT_3D('',#77151,#62555,#62556);
#53478=AXIS2_PLACEMENT_3D('',#77153,#62558,#62559);
#53479=AXIS2_PLACEMENT_3D('',#77155,#62561,#62562);
#53480=AXIS2_PLACEMENT_3D('',#77157,#62564,#62565);
#53481=AXIS2_PLACEMENT_3D('',#77159,#62567,#62568);
#53482=AXIS2_PLACEMENT_3D('',#77161,#62570,#62571);
#53483=AXIS2_PLACEMENT_3D('',#77163,#62573,#62574);
#53484=AXIS2_PLACEMENT_3D('',#77165,#62576,#62577);
#53485=AXIS2_PLACEMENT_3D('',#77167,#62579,#62580);
#53486=AXIS2_PLACEMENT_3D('',#77169,#62582,#62583);
#53487=AXIS2_PLACEMENT_3D('',#77171,#62585,#62586);
#53488=AXIS2_PLACEMENT_3D('',#77173,#62588,#62589);
#53489=AXIS2_PLACEMENT_3D('',#77177,#62590,#62591);
#53490=AXIS2_PLACEMENT_3D('',#77181,#62594,#62595);
#53491=AXIS2_PLACEMENT_3D('',#77183,#62596,#62597);
#53492=AXIS2_PLACEMENT_3D('',#77185,#62599,#62600);
#53493=AXIS2_PLACEMENT_3D('',#77187,#62601,#62602);
#53494=AXIS2_PLACEMENT_3D('',#77189,#62604,#62605);
#53495=AXIS2_PLACEMENT_3D('',#77191,#62606,#62607);
#53496=AXIS2_PLACEMENT_3D('',#77193,#62609,#62610);
#53497=AXIS2_PLACEMENT_3D('',#77195,#62611,#62612);
#53498=AXIS2_PLACEMENT_3D('',#77197,#62614,#62615);
#53499=AXIS2_PLACEMENT_3D('',#77199,#62616,#62617);
#53500=AXIS2_PLACEMENT_3D('',#77201,#62619,#62620);
#53501=AXIS2_PLACEMENT_3D('',#77205,#62623,#62624);
#53502=AXIS2_PLACEMENT_3D('',#77207,#62625,#62626);
#53503=AXIS2_PLACEMENT_3D('',#77209,#62628,#62629);
#53504=AXIS2_PLACEMENT_3D('',#77211,#62630,#62631);
#53505=AXIS2_PLACEMENT_3D('',#77213,#62633,#62634);
#53506=AXIS2_PLACEMENT_3D('',#77215,#62635,#62636);
#53507=AXIS2_PLACEMENT_3D('',#77217,#62638,#62639);
#53508=AXIS2_PLACEMENT_3D('',#77219,#62640,#62641);
#53509=AXIS2_PLACEMENT_3D('',#77221,#62643,#62644);
#53510=AXIS2_PLACEMENT_3D('',#77223,#62645,#62646);
#53511=AXIS2_PLACEMENT_3D('',#77225,#62648,#62649);
#53512=AXIS2_PLACEMENT_3D('',#77227,#62651,#62652);
#53513=AXIS2_PLACEMENT_3D('',#77228,#62653,#62654);
#53514=AXIS2_PLACEMENT_3D('',#77230,#62655,#62656);
#53515=AXIS2_PLACEMENT_3D('',#77232,#62657,#62658);
#53516=AXIS2_PLACEMENT_3D('',#77236,#62660,#62661);
#53517=AXIS2_PLACEMENT_3D('',#77238,#62662,#62663);
#53518=AXIS2_PLACEMENT_3D('',#77240,#62664,#62665);
#53519=AXIS2_PLACEMENT_3D('',#77242,#62666,#62667);
#53520=AXIS2_PLACEMENT_3D('',#77244,#62668,#62669);
#53521=AXIS2_PLACEMENT_3D('',#77248,#62671,#62672);
#53522=AXIS2_PLACEMENT_3D('',#77250,#62673,#62674);
#53523=AXIS2_PLACEMENT_3D('',#77252,#62675,#62676);
#53524=AXIS2_PLACEMENT_3D('',#77254,#62677,#62678);
#53525=AXIS2_PLACEMENT_3D('',#77256,#62679,#62680);
#53526=AXIS2_PLACEMENT_3D('',#77258,#62682,#62683);
#53527=AXIS2_PLACEMENT_3D('',#77262,#62686,#62687);
#53528=AXIS2_PLACEMENT_3D('',#77264,#62688,#62689);
#53529=AXIS2_PLACEMENT_3D('',#77266,#62691,#62692);
#53530=AXIS2_PLACEMENT_3D('',#77268,#62693,#62694);
#53531=AXIS2_PLACEMENT_3D('',#77270,#62696,#62697);
#53532=AXIS2_PLACEMENT_3D('',#77272,#62698,#62699);
#53533=AXIS2_PLACEMENT_3D('',#77274,#62701,#62702);
#53534=AXIS2_PLACEMENT_3D('',#77276,#62703,#62704);
#53535=AXIS2_PLACEMENT_3D('',#77278,#62706,#62707);
#53536=AXIS2_PLACEMENT_3D('',#77280,#62708,#62709);
#53537=AXIS2_PLACEMENT_3D('',#77282,#62711,#62712);
#53538=AXIS2_PLACEMENT_3D('',#77286,#62715,#62716);
#53539=AXIS2_PLACEMENT_3D('',#77288,#62717,#62718);
#53540=AXIS2_PLACEMENT_3D('',#77290,#62720,#62721);
#53541=AXIS2_PLACEMENT_3D('',#77292,#62722,#62723);
#53542=AXIS2_PLACEMENT_3D('',#77294,#62725,#62726);
#53543=AXIS2_PLACEMENT_3D('',#77296,#62727,#62728);
#53544=AXIS2_PLACEMENT_3D('',#77298,#62730,#62731);
#53545=AXIS2_PLACEMENT_3D('',#77300,#62732,#62733);
#53546=AXIS2_PLACEMENT_3D('',#77302,#62735,#62736);
#53547=AXIS2_PLACEMENT_3D('',#77304,#62737,#62738);
#53548=AXIS2_PLACEMENT_3D('',#77306,#62740,#62741);
#53549=AXIS2_PLACEMENT_3D('',#77310,#62744,#62745);
#53550=AXIS2_PLACEMENT_3D('',#77311,#62746,#62747);
#53551=AXIS2_PLACEMENT_3D('',#77312,#62748,#62749);
#53552=AXIS2_PLACEMENT_3D('',#77314,#62751,#62752);
#53553=AXIS2_PLACEMENT_3D('',#77316,#62754,#62755);
#53554=AXIS2_PLACEMENT_3D('',#77318,#62757,#62758);
#53555=AXIS2_PLACEMENT_3D('',#77320,#62760,#62761);
#53556=AXIS2_PLACEMENT_3D('',#77322,#62763,#62764);
#53557=AXIS2_PLACEMENT_3D('',#77324,#62766,#62767);
#53558=AXIS2_PLACEMENT_3D('',#77326,#62769,#62770);
#53559=AXIS2_PLACEMENT_3D('',#77328,#62772,#62773);
#53560=AXIS2_PLACEMENT_3D('',#77330,#62775,#62776);
#53561=AXIS2_PLACEMENT_3D('',#77332,#62778,#62779);
#53562=AXIS2_PLACEMENT_3D('',#77334,#62781,#62782);
#53563=AXIS2_PLACEMENT_3D('',#77336,#62784,#62785);
#53564=AXIS2_PLACEMENT_3D('',#77338,#62787,#62788);
#53565=AXIS2_PLACEMENT_3D('',#77342,#62789,#62790);
#53566=AXIS2_PLACEMENT_3D('',#77343,#62791,#62792);
#53567=AXIS2_PLACEMENT_3D('',#77346,#62794,#62795);
#53568=AXIS2_PLACEMENT_3D('',#77347,#62796,#62797);
#53569=AXIS2_PLACEMENT_3D('',#77349,#62798,#62799);
#53570=AXIS2_PLACEMENT_3D('',#77353,#62801,#62802);
#53571=AXIS2_PLACEMENT_3D('',#77354,#62803,#62804);
#53572=AXIS2_PLACEMENT_3D('',#77355,#62805,#62806);
#53573=AXIS2_PLACEMENT_3D('',#77359,#62808,#62809);
#53574=AXIS2_PLACEMENT_3D('',#77360,#62810,#62811);
#53575=AXIS2_PLACEMENT_3D('',#77361,#62812,#62813);
#53576=AXIS2_PLACEMENT_3D('',#77362,#62814,#62815);
#53577=AXIS2_PLACEMENT_3D('',#77364,#62816,#62817);
#53578=AXIS2_PLACEMENT_3D('',#77366,#62818,#62819);
#53579=AXIS2_PLACEMENT_3D('',#77367,#62820,#62821);
#53580=AXIS2_PLACEMENT_3D('',#77368,#62822,#62823);
#53581=AXIS2_PLACEMENT_3D('',#77371,#62825,#62826);
#53582=AXIS2_PLACEMENT_3D('',#77372,#62827,#62828);
#53583=AXIS2_PLACEMENT_3D('',#77375,#62829,#62830);
#53584=AXIS2_PLACEMENT_3D('',#77377,#62831,#62832);
#53585=AXIS2_PLACEMENT_3D('',#77378,#62833,#62834);
#53586=AXIS2_PLACEMENT_3D('',#77379,#62835,#62836);
#53587=AXIS2_PLACEMENT_3D('',#77380,#62837,#62838);
#53588=AXIS2_PLACEMENT_3D('',#77384,#62840,#62841);
#53589=AXIS2_PLACEMENT_3D('',#77385,#62842,#62843);
#53590=AXIS2_PLACEMENT_3D('',#77386,#62844,#62845);
#53591=AXIS2_PLACEMENT_3D('',#77388,#62846,#62847);
#53592=AXIS2_PLACEMENT_3D('',#77389,#62848,#62849);
#53593=AXIS2_PLACEMENT_3D('',#77391,#62850,#62851);
#53594=AXIS2_PLACEMENT_3D('',#77392,#62852,#62853);
#53595=AXIS2_PLACEMENT_3D('',#77393,#62854,#62855);
#53596=AXIS2_PLACEMENT_3D('',#77395,#62856,#62857);
#53597=AXIS2_PLACEMENT_3D('',#77396,#62858,#62859);
#53598=AXIS2_PLACEMENT_3D('',#77397,#62860,#62861);
#53599=AXIS2_PLACEMENT_3D('',#77399,#62862,#62863);
#53600=AXIS2_PLACEMENT_3D('',#77400,#62864,#62865);
#53601=AXIS2_PLACEMENT_3D('',#77402,#62866,#62867);
#53602=AXIS2_PLACEMENT_3D('',#77404,#62869,#62870);
#53603=AXIS2_PLACEMENT_3D('',#77406,#62871,#62872);
#53604=AXIS2_PLACEMENT_3D('',#77408,#62874,#62875);
#53605=AXIS2_PLACEMENT_3D('',#77410,#62877,#62878);
#53606=AXIS2_PLACEMENT_3D('',#77412,#62879,#62880);
#53607=AXIS2_PLACEMENT_3D('',#77414,#62882,#62883);
#53608=AXIS2_PLACEMENT_3D('',#77416,#62885,#62886);
#53609=AXIS2_PLACEMENT_3D('',#77417,#62887,#62888);
#53610=AXIS2_PLACEMENT_3D('',#77434,#62893,#62894);
#53611=AXIS2_PLACEMENT_3D('',#77451,#62899,#62900);
#53612=AXIS2_PLACEMENT_3D('',#77454,#62903,#62904);
#53613=AXIS2_PLACEMENT_3D('',#77456,#62905,#62906);
#53614=AXIS2_PLACEMENT_3D('',#77459,#62908,#62909);
#53615=AXIS2_PLACEMENT_3D('',#77460,#62910,#62911);
#53616=AXIS2_PLACEMENT_3D('',#77462,#62912,#62913);
#53617=AXIS2_PLACEMENT_3D('',#77468,#62914,#62915);
#53618=AXIS2_PLACEMENT_3D('',#77482,#62916,#62917);
#53619=AXIS2_PLACEMENT_3D('',#77496,#62918,#62919);
#53620=AXIS2_PLACEMENT_3D('',#77510,#62920,#62921);
#53621=AXIS2_PLACEMENT_3D('',#77524,#62922,#62923);
#53622=AXIS2_PLACEMENT_3D('',#77538,#62924,#62925);
#53623=AXIS2_PLACEMENT_3D('',#77552,#62926,#62927);
#53624=AXIS2_PLACEMENT_3D('',#77566,#62928,#62929);
#53625=AXIS2_PLACEMENT_3D('',#77580,#62930,#62931);
#53626=AXIS2_PLACEMENT_3D('',#77594,#62932,#62933);
#53627=AXIS2_PLACEMENT_3D('',#77608,#62934,#62935);
#53628=AXIS2_PLACEMENT_3D('',#77621,#62936,#62937);
#53629=AXIS2_PLACEMENT_3D('',#77622,#62938,#62939);
#53630=AXIS2_PLACEMENT_3D('',#77624,#62940,#62941);
#53631=AXIS2_PLACEMENT_3D('',#77632,#62945,#62946);
#53632=AXIS2_PLACEMENT_3D('',#77639,#62950,#62951);
#53633=AXIS2_PLACEMENT_3D('',#77641,#62952,#62953);
#53634=AXIS2_PLACEMENT_3D('',#77642,#62954,#62955);
#53635=AXIS2_PLACEMENT_3D('',#77644,#62956,#62957);
#53636=AXIS2_PLACEMENT_3D('',#77658,#62958,#62959);
#53637=AXIS2_PLACEMENT_3D('',#77672,#62960,#62961);
#53638=AXIS2_PLACEMENT_3D('',#77686,#62962,#62963);
#53639=AXIS2_PLACEMENT_3D('',#77700,#62964,#62965);
#53640=AXIS2_PLACEMENT_3D('',#77714,#62966,#62967);
#53641=AXIS2_PLACEMENT_3D('',#77728,#62968,#62969);
#53642=AXIS2_PLACEMENT_3D('',#77742,#62970,#62971);
#53643=AXIS2_PLACEMENT_3D('',#77756,#62972,#62973);
#53644=AXIS2_PLACEMENT_3D('',#77770,#62974,#62975);
#53645=AXIS2_PLACEMENT_3D('',#77784,#62976,#62977);
#53646=AXIS2_PLACEMENT_3D('',#77798,#62978,#62979);
#53647=AXIS2_PLACEMENT_3D('',#77802,#62980,#62981);
#53648=AXIS2_PLACEMENT_3D('',#77808,#62982,#62983);
#53649=AXIS2_PLACEMENT_3D('',#77822,#62984,#62985);
#53650=AXIS2_PLACEMENT_3D('',#77836,#62986,#62987);
#53651=AXIS2_PLACEMENT_3D('',#77850,#62988,#62989);
#53652=AXIS2_PLACEMENT_3D('',#77864,#62990,#62991);
#53653=AXIS2_PLACEMENT_3D('',#77878,#62992,#62993);
#53654=AXIS2_PLACEMENT_3D('',#77892,#62994,#62995);
#53655=AXIS2_PLACEMENT_3D('',#77906,#62996,#62997);
#53656=AXIS2_PLACEMENT_3D('',#77920,#62998,#62999);
#53657=AXIS2_PLACEMENT_3D('',#77934,#63000,#63001);
#53658=AXIS2_PLACEMENT_3D('',#77948,#63002,#63003);
#53659=AXIS2_PLACEMENT_3D('',#77960,#63004,#63005);
#53660=AXIS2_PLACEMENT_3D('',#77965,#63009,#63010);
#53661=AXIS2_PLACEMENT_3D('',#77979,#63014,#63015);
#53662=AXIS2_PLACEMENT_3D('',#77981,#63017,#63018);
#53663=AXIS2_PLACEMENT_3D('',#77983,#63019,#63020);
#53664=AXIS2_PLACEMENT_3D('',#77989,#63021,#63022);
#53665=AXIS2_PLACEMENT_3D('',#78003,#63023,#63024);
#53666=AXIS2_PLACEMENT_3D('',#78017,#63025,#63026);
#53667=AXIS2_PLACEMENT_3D('',#78031,#63027,#63028);
#53668=AXIS2_PLACEMENT_3D('',#78045,#63029,#63030);
#53669=AXIS2_PLACEMENT_3D('',#78059,#63031,#63032);
#53670=AXIS2_PLACEMENT_3D('',#78073,#63033,#63034);
#53671=AXIS2_PLACEMENT_3D('',#78087,#63035,#63036);
#53672=AXIS2_PLACEMENT_3D('',#78101,#63037,#63038);
#53673=AXIS2_PLACEMENT_3D('',#78115,#63039,#63040);
#53674=AXIS2_PLACEMENT_3D('',#78129,#63041,#63042);
#53675=AXIS2_PLACEMENT_3D('',#78142,#63043,#63044);
#53676=AXIS2_PLACEMENT_3D('',#78143,#63045,#63046);
#53677=AXIS2_PLACEMENT_3D('',#78157,#63047,#63048);
#53678=AXIS2_PLACEMENT_3D('',#78171,#63049,#63050);
#53679=AXIS2_PLACEMENT_3D('',#78185,#63051,#63052);
#53680=AXIS2_PLACEMENT_3D('',#78199,#63053,#63054);
#53681=AXIS2_PLACEMENT_3D('',#78213,#63055,#63056);
#53682=AXIS2_PLACEMENT_3D('',#78227,#63057,#63058);
#53683=AXIS2_PLACEMENT_3D('',#78241,#63059,#63060);
#53684=AXIS2_PLACEMENT_3D('',#78255,#63061,#63062);
#53685=AXIS2_PLACEMENT_3D('',#78269,#63063,#63064);
#53686=AXIS2_PLACEMENT_3D('',#78283,#63065,#63066);
#53687=AXIS2_PLACEMENT_3D('',#78297,#63067,#63068);
#53688=AXIS2_PLACEMENT_3D('',#78302,#63069,#63070);
#53689=AXIS2_PLACEMENT_3D('',#78303,#63071,#63072);
#53690=AXIS2_PLACEMENT_3D('',#78305,#63074,#63075);
#53691=AXIS2_PLACEMENT_3D('',#78307,#63076,#63077);
#53692=AXIS2_PLACEMENT_3D('',#78321,#63078,#63079);
#53693=AXIS2_PLACEMENT_3D('',#78335,#63080,#63081);
#53694=AXIS2_PLACEMENT_3D('',#78349,#63082,#63083);
#53695=AXIS2_PLACEMENT_3D('',#78363,#63084,#63085);
#53696=AXIS2_PLACEMENT_3D('',#78377,#63086,#63087);
#53697=AXIS2_PLACEMENT_3D('',#78391,#63088,#63089);
#53698=AXIS2_PLACEMENT_3D('',#78405,#63090,#63091);
#53699=AXIS2_PLACEMENT_3D('',#78419,#63092,#63093);
#53700=AXIS2_PLACEMENT_3D('',#78433,#63094,#63095);
#53701=AXIS2_PLACEMENT_3D('',#78447,#63096,#63097);
#53702=AXIS2_PLACEMENT_3D('',#78461,#63098,#63099);
#53703=AXIS2_PLACEMENT_3D('',#78465,#63100,#63101);
#53704=AXIS2_PLACEMENT_3D('',#78470,#63105,#63106);
#53705=AXIS2_PLACEMENT_3D('',#78475,#63110,#63111);
#53706=AXIS2_PLACEMENT_3D('',#78477,#63113,#63114);
#53707=AXIS2_PLACEMENT_3D('',#78479,#63116,#63117);
#53708=AXIS2_PLACEMENT_3D('',#78493,#63118,#63119);
#53709=AXIS2_PLACEMENT_3D('',#78494,#63120,#63121);
#53710=AXIS2_PLACEMENT_3D('',#78508,#63122,#63123);
#53711=AXIS2_PLACEMENT_3D('',#78509,#63124,#63125);
#53712=AXIS2_PLACEMENT_3D('',#78523,#63126,#63127);
#53713=AXIS2_PLACEMENT_3D('',#78524,#63128,#63129);
#53714=AXIS2_PLACEMENT_3D('',#78538,#63130,#63131);
#53715=AXIS2_PLACEMENT_3D('',#78539,#63132,#63133);
#53716=AXIS2_PLACEMENT_3D('',#78553,#63134,#63135);
#53717=AXIS2_PLACEMENT_3D('',#78554,#63136,#63137);
#53718=AXIS2_PLACEMENT_3D('',#78568,#63138,#63139);
#53719=AXIS2_PLACEMENT_3D('',#78569,#63140,#63141);
#53720=AXIS2_PLACEMENT_3D('',#78583,#63142,#63143);
#53721=AXIS2_PLACEMENT_3D('',#78584,#63144,#63145);
#53722=AXIS2_PLACEMENT_3D('',#78598,#63146,#63147);
#53723=AXIS2_PLACEMENT_3D('',#78599,#63148,#63149);
#53724=AXIS2_PLACEMENT_3D('',#78613,#63150,#63151);
#53725=AXIS2_PLACEMENT_3D('',#78614,#63152,#63153);
#53726=AXIS2_PLACEMENT_3D('',#78628,#63154,#63155);
#53727=AXIS2_PLACEMENT_3D('',#78629,#63156,#63157);
#53728=AXIS2_PLACEMENT_3D('',#78643,#63158,#63159);
#53729=AXIS2_PLACEMENT_3D('',#78644,#63160,#63161);
#53730=AXIS2_PLACEMENT_3D('',#78658,#63162,#63163);
#53731=AXIS2_PLACEMENT_3D('',#78659,#63164,#63165);
#53732=AXIS2_PLACEMENT_3D('',#78673,#63166,#63167);
#53733=AXIS2_PLACEMENT_3D('',#78674,#63168,#63169);
#53734=AXIS2_PLACEMENT_3D('',#78688,#63170,#63171);
#53735=AXIS2_PLACEMENT_3D('',#78689,#63172,#63173);
#53736=AXIS2_PLACEMENT_3D('',#78703,#63174,#63175);
#53737=AXIS2_PLACEMENT_3D('',#78704,#63176,#63177);
#53738=AXIS2_PLACEMENT_3D('',#78718,#63178,#63179);
#53739=AXIS2_PLACEMENT_3D('',#78719,#63180,#63181);
#53740=AXIS2_PLACEMENT_3D('',#78733,#63182,#63183);
#53741=AXIS2_PLACEMENT_3D('',#78734,#63184,#63185);
#53742=AXIS2_PLACEMENT_3D('',#78748,#63186,#63187);
#53743=AXIS2_PLACEMENT_3D('',#78749,#63188,#63189);
#53744=AXIS2_PLACEMENT_3D('',#78763,#63190,#63191);
#53745=AXIS2_PLACEMENT_3D('',#78764,#63192,#63193);
#53746=AXIS2_PLACEMENT_3D('',#78778,#63194,#63195);
#53747=AXIS2_PLACEMENT_3D('',#78779,#63196,#63197);
#53748=AXIS2_PLACEMENT_3D('',#78793,#63198,#63199);
#53749=AXIS2_PLACEMENT_3D('',#78794,#63200,#63201);
#53750=AXIS2_PLACEMENT_3D('',#78808,#63202,#63203);
#53751=AXIS2_PLACEMENT_3D('',#78809,#63204,#63205);
#53752=AXIS2_PLACEMENT_3D('',#78823,#63206,#63207);
#53753=AXIS2_PLACEMENT_3D('',#78824,#63208,#63209);
#53754=AXIS2_PLACEMENT_3D('',#78838,#63210,#63211);
#53755=AXIS2_PLACEMENT_3D('',#78839,#63212,#63213);
#53756=AXIS2_PLACEMENT_3D('',#78853,#63214,#63215);
#53757=AXIS2_PLACEMENT_3D('',#78854,#63216,#63217);
#53758=AXIS2_PLACEMENT_3D('',#78868,#63218,#63219);
#53759=AXIS2_PLACEMENT_3D('',#78869,#63220,#63221);
#53760=AXIS2_PLACEMENT_3D('',#78883,#63222,#63223);
#53761=AXIS2_PLACEMENT_3D('',#78884,#63224,#63225);
#53762=AXIS2_PLACEMENT_3D('',#78898,#63226,#63227);
#53763=AXIS2_PLACEMENT_3D('',#78899,#63228,#63229);
#53764=AXIS2_PLACEMENT_3D('',#78913,#63230,#63231);
#53765=AXIS2_PLACEMENT_3D('',#78914,#63232,#63233);
#53766=AXIS2_PLACEMENT_3D('',#78928,#63234,#63235);
#53767=AXIS2_PLACEMENT_3D('',#78929,#63236,#63237);
#53768=AXIS2_PLACEMENT_3D('',#78943,#63238,#63239);
#53769=AXIS2_PLACEMENT_3D('',#78944,#63240,#63241);
#53770=AXIS2_PLACEMENT_3D('',#78958,#63242,#63243);
#53771=AXIS2_PLACEMENT_3D('',#78959,#63244,#63245);
#53772=AXIS2_PLACEMENT_3D('',#78973,#63246,#63247);
#53773=AXIS2_PLACEMENT_3D('',#78974,#63248,#63249);
#53774=AXIS2_PLACEMENT_3D('',#78988,#63256,#63257);
#53775=AXIS2_PLACEMENT_3D('',#78994,#63259,#63260);
#53776=AXIS2_PLACEMENT_3D('',#79008,#63267,#63268);
#53777=AXIS2_PLACEMENT_3D('',#79014,#63270,#63271);
#53778=AXIS2_PLACEMENT_3D('',#79028,#63278,#63279);
#53779=AXIS2_PLACEMENT_3D('',#79034,#63281,#63282);
#53780=AXIS2_PLACEMENT_3D('',#79048,#63289,#63290);
#53781=AXIS2_PLACEMENT_3D('',#79054,#63292,#63293);
#53782=AXIS2_PLACEMENT_3D('',#79068,#63300,#63301);
#53783=AXIS2_PLACEMENT_3D('',#79074,#63303,#63304);
#53784=AXIS2_PLACEMENT_3D('',#79088,#63311,#63312);
#53785=AXIS2_PLACEMENT_3D('',#79094,#63314,#63315);
#53786=AXIS2_PLACEMENT_3D('',#79108,#63322,#63323);
#53787=AXIS2_PLACEMENT_3D('',#79114,#63325,#63326);
#53788=AXIS2_PLACEMENT_3D('',#79128,#63333,#63334);
#53789=AXIS2_PLACEMENT_3D('',#79134,#63336,#63337);
#53790=AXIS2_PLACEMENT_3D('',#79148,#63344,#63345);
#53791=AXIS2_PLACEMENT_3D('',#79154,#63347,#63348);
#53792=AXIS2_PLACEMENT_3D('',#79168,#63355,#63356);
#53793=AXIS2_PLACEMENT_3D('',#79174,#63358,#63359);
#53794=AXIS2_PLACEMENT_3D('',#79188,#63366,#63367);
#53795=AXIS2_PLACEMENT_3D('',#79194,#63369,#63370);
#53796=AXIS2_PLACEMENT_3D('',#79208,#63377,#63378);
#53797=AXIS2_PLACEMENT_3D('',#79214,#63380,#63381);
#53798=AXIS2_PLACEMENT_3D('',#79228,#63388,#63389);
#53799=AXIS2_PLACEMENT_3D('',#79234,#63391,#63392);
#53800=AXIS2_PLACEMENT_3D('',#79248,#63399,#63400);
#53801=AXIS2_PLACEMENT_3D('',#79254,#63402,#63403);
#53802=AXIS2_PLACEMENT_3D('',#79268,#63410,#63411);
#53803=AXIS2_PLACEMENT_3D('',#79274,#63413,#63414);
#53804=AXIS2_PLACEMENT_3D('',#79288,#63421,#63422);
#53805=AXIS2_PLACEMENT_3D('',#79294,#63424,#63425);
#53806=AXIS2_PLACEMENT_3D('',#79308,#63432,#63433);
#53807=AXIS2_PLACEMENT_3D('',#79314,#63435,#63436);
#53808=AXIS2_PLACEMENT_3D('',#79328,#63443,#63444);
#53809=AXIS2_PLACEMENT_3D('',#79334,#63446,#63447);
#53810=AXIS2_PLACEMENT_3D('',#79348,#63454,#63455);
#53811=AXIS2_PLACEMENT_3D('',#79354,#63457,#63458);
#53812=AXIS2_PLACEMENT_3D('',#79368,#63465,#63466);
#53813=AXIS2_PLACEMENT_3D('',#79374,#63468,#63469);
#53814=AXIS2_PLACEMENT_3D('',#79388,#63476,#63477);
#53815=AXIS2_PLACEMENT_3D('',#79394,#63479,#63480);
#53816=AXIS2_PLACEMENT_3D('',#79408,#63487,#63488);
#53817=AXIS2_PLACEMENT_3D('',#79414,#63490,#63491);
#53818=AXIS2_PLACEMENT_3D('',#79428,#63498,#63499);
#53819=AXIS2_PLACEMENT_3D('',#79434,#63501,#63502);
#53820=AXIS2_PLACEMENT_3D('',#79448,#63509,#63510);
#53821=AXIS2_PLACEMENT_3D('',#79454,#63512,#63513);
#53822=AXIS2_PLACEMENT_3D('',#79468,#63520,#63521);
#53823=AXIS2_PLACEMENT_3D('',#79474,#63523,#63524);
#53824=AXIS2_PLACEMENT_3D('',#79488,#63531,#63532);
#53825=AXIS2_PLACEMENT_3D('',#79494,#63534,#63535);
#53826=AXIS2_PLACEMENT_3D('',#79508,#63542,#63543);
#53827=AXIS2_PLACEMENT_3D('',#79514,#63545,#63546);
#53828=AXIS2_PLACEMENT_3D('',#79528,#63553,#63554);
#53829=AXIS2_PLACEMENT_3D('',#79534,#63556,#63557);
#53830=AXIS2_PLACEMENT_3D('',#79548,#63564,#63565);
#53831=AXIS2_PLACEMENT_3D('',#79554,#63567,#63568);
#53832=AXIS2_PLACEMENT_3D('',#79568,#63575,#63576);
#53833=AXIS2_PLACEMENT_3D('',#79574,#63578,#63579);
#53834=AXIS2_PLACEMENT_3D('',#79588,#63586,#63587);
#53835=AXIS2_PLACEMENT_3D('',#79594,#63589,#63590);
#53836=AXIS2_PLACEMENT_3D('',#79608,#63597,#63598);
#53837=AXIS2_PLACEMENT_3D('',#79614,#63600,#63601);
#53838=AXIS2_PLACEMENT_3D('',#79628,#63608,#63609);
#53839=AXIS2_PLACEMENT_3D('',#79634,#63611,#63612);
#53840=AXIS2_PLACEMENT_3D('',#79639,#63613,#63614);
#53841=AXIS2_PLACEMENT_3D('',#79640,#63615,#63616);
#53842=AXIS2_PLACEMENT_3D('',#79645,#63617,#63618);
#53843=AXIS2_PLACEMENT_3D('',#79646,#63619,#63620);
#53844=AXIS2_PLACEMENT_3D('',#79651,#63621,#63622);
#53845=AXIS2_PLACEMENT_3D('',#79652,#63623,#63624);
#53846=AXIS2_PLACEMENT_3D('',#79657,#63625,#63626);
#53847=AXIS2_PLACEMENT_3D('',#79658,#63627,#63628);
#53848=AXIS2_PLACEMENT_3D('',#79663,#63629,#63630);
#53849=AXIS2_PLACEMENT_3D('',#79664,#63631,#63632);
#53850=AXIS2_PLACEMENT_3D('',#79669,#63633,#63634);
#53851=AXIS2_PLACEMENT_3D('',#79670,#63635,#63636);
#53852=AXIS2_PLACEMENT_3D('',#79675,#63637,#63638);
#53853=AXIS2_PLACEMENT_3D('',#79676,#63639,#63640);
#53854=AXIS2_PLACEMENT_3D('',#79681,#63641,#63642);
#53855=AXIS2_PLACEMENT_3D('',#79682,#63643,#63644);
#53856=AXIS2_PLACEMENT_3D('',#79687,#63645,#63646);
#53857=AXIS2_PLACEMENT_3D('',#79688,#63647,#63648);
#53858=AXIS2_PLACEMENT_3D('',#79693,#63649,#63650);
#53859=AXIS2_PLACEMENT_3D('',#79694,#63651,#63652);
#53860=AXIS2_PLACEMENT_3D('',#79699,#63653,#63654);
#53861=AXIS2_PLACEMENT_3D('',#79700,#63655,#63656);
#53862=AXIS2_PLACEMENT_3D('',#79705,#63657,#63658);
#53863=AXIS2_PLACEMENT_3D('',#79706,#63659,#63660);
#53864=AXIS2_PLACEMENT_3D('',#79711,#63661,#63662);
#53865=AXIS2_PLACEMENT_3D('',#79712,#63663,#63664);
#53866=AXIS2_PLACEMENT_3D('',#79717,#63665,#63666);
#53867=AXIS2_PLACEMENT_3D('',#79718,#63667,#63668);
#53868=AXIS2_PLACEMENT_3D('',#79723,#63669,#63670);
#53869=AXIS2_PLACEMENT_3D('',#79724,#63671,#63672);
#53870=AXIS2_PLACEMENT_3D('',#79729,#63673,#63674);
#53871=AXIS2_PLACEMENT_3D('',#79730,#63675,#63676);
#53872=AXIS2_PLACEMENT_3D('',#79735,#63677,#63678);
#53873=AXIS2_PLACEMENT_3D('',#79736,#63679,#63680);
#53874=AXIS2_PLACEMENT_3D('',#79741,#63681,#63682);
#53875=AXIS2_PLACEMENT_3D('',#79742,#63683,#63684);
#53876=AXIS2_PLACEMENT_3D('',#79747,#63685,#63686);
#53877=AXIS2_PLACEMENT_3D('',#79748,#63687,#63688);
#53878=AXIS2_PLACEMENT_3D('',#79753,#63689,#63690);
#53879=AXIS2_PLACEMENT_3D('',#79754,#63691,#63692);
#53880=AXIS2_PLACEMENT_3D('',#79759,#63693,#63694);
#53881=AXIS2_PLACEMENT_3D('',#79760,#63695,#63696);
#53882=AXIS2_PLACEMENT_3D('',#79765,#63697,#63698);
#53883=AXIS2_PLACEMENT_3D('',#79766,#63699,#63700);
#53884=AXIS2_PLACEMENT_3D('',#79771,#63701,#63702);
#53885=AXIS2_PLACEMENT_3D('',#79772,#63703,#63704);
#53886=AXIS2_PLACEMENT_3D('',#79777,#63705,#63706);
#53887=AXIS2_PLACEMENT_3D('',#79778,#63707,#63708);
#53888=AXIS2_PLACEMENT_3D('',#79783,#63709,#63710);
#53889=AXIS2_PLACEMENT_3D('',#79784,#63711,#63712);
#53890=AXIS2_PLACEMENT_3D('',#79789,#63713,#63714);
#53891=AXIS2_PLACEMENT_3D('',#79790,#63715,#63716);
#53892=AXIS2_PLACEMENT_3D('',#79795,#63717,#63718);
#53893=AXIS2_PLACEMENT_3D('',#79796,#63719,#63720);
#53894=AXIS2_PLACEMENT_3D('',#79801,#63721,#63722);
#53895=AXIS2_PLACEMENT_3D('',#79802,#63723,#63724);
#53896=AXIS2_PLACEMENT_3D('',#79807,#63725,#63726);
#53897=AXIS2_PLACEMENT_3D('',#79808,#63727,#63728);
#53898=AXIS2_PLACEMENT_3D('',#79813,#63729,#63730);
#53899=AXIS2_PLACEMENT_3D('',#79814,#63731,#63732);
#53900=AXIS2_PLACEMENT_3D('',#79819,#63733,#63734);
#53901=AXIS2_PLACEMENT_3D('',#79820,#63735,#63736);
#53902=AXIS2_PLACEMENT_3D('',#79825,#63737,#63738);
#53903=AXIS2_PLACEMENT_3D('',#79826,#63739,#63740);
#53904=AXIS2_PLACEMENT_3D('',#79831,#63741,#63742);
#53905=AXIS2_PLACEMENT_3D('',#79832,#63743,#63744);
#53906=AXIS2_PLACEMENT_3D('',#79840,#63750,#63751);
#53907=AXIS2_PLACEMENT_3D('',#79848,#63757,#63758);
#53908=AXIS2_PLACEMENT_3D('',#79856,#63764,#63765);
#53909=AXIS2_PLACEMENT_3D('',#79864,#63771,#63772);
#53910=AXIS2_PLACEMENT_3D('',#79872,#63778,#63779);
#53911=AXIS2_PLACEMENT_3D('',#79880,#63785,#63786);
#53912=AXIS2_PLACEMENT_3D('',#79888,#63792,#63793);
#53913=AXIS2_PLACEMENT_3D('',#79896,#63799,#63800);
#53914=AXIS2_PLACEMENT_3D('',#79904,#63806,#63807);
#53915=AXIS2_PLACEMENT_3D('',#79912,#63813,#63814);
#53916=AXIS2_PLACEMENT_3D('',#79919,#63819,#63820);
#53917=AXIS2_PLACEMENT_3D('',#79927,#63826,#63827);
#53918=AXIS2_PLACEMENT_3D('',#79935,#63833,#63834);
#53919=AXIS2_PLACEMENT_3D('',#79943,#63840,#63841);
#53920=AXIS2_PLACEMENT_3D('',#79951,#63847,#63848);
#53921=AXIS2_PLACEMENT_3D('',#79959,#63854,#63855);
#53922=AXIS2_PLACEMENT_3D('',#79967,#63861,#63862);
#53923=AXIS2_PLACEMENT_3D('',#79975,#63868,#63869);
#53924=AXIS2_PLACEMENT_3D('',#79983,#63875,#63876);
#53925=AXIS2_PLACEMENT_3D('',#79991,#63882,#63883);
#53926=AXIS2_PLACEMENT_3D('',#79999,#63889,#63890);
#53927=AXIS2_PLACEMENT_3D('',#80006,#63895,#63896);
#53928=AXIS2_PLACEMENT_3D('',#80014,#63902,#63903);
#53929=AXIS2_PLACEMENT_3D('',#80022,#63909,#63910);
#53930=AXIS2_PLACEMENT_3D('',#80030,#63916,#63917);
#53931=AXIS2_PLACEMENT_3D('',#80038,#63923,#63924);
#53932=AXIS2_PLACEMENT_3D('',#80046,#63930,#63931);
#53933=AXIS2_PLACEMENT_3D('',#80054,#63937,#63938);
#53934=AXIS2_PLACEMENT_3D('',#80062,#63944,#63945);
#53935=AXIS2_PLACEMENT_3D('',#80070,#63951,#63952);
#53936=AXIS2_PLACEMENT_3D('',#80078,#63958,#63959);
#53937=AXIS2_PLACEMENT_3D('',#80086,#63965,#63966);
#53938=AXIS2_PLACEMENT_3D('',#80093,#63971,#63972);
#53939=AXIS2_PLACEMENT_3D('',#80095,#63974,#63975);
#53940=AXIS2_PLACEMENT_3D('',#80097,#63977,#63978);
#53941=AXIS2_PLACEMENT_3D('',#80098,#63979,#63980);
#53942=AXIS2_PLACEMENT_3D('',#80099,#63981,#63982);
#53943=AXIS2_PLACEMENT_3D('',#80100,#63983,#63984);
#53944=AXIS2_PLACEMENT_3D('',#80101,#63985,#63986);
#53945=AXIS2_PLACEMENT_3D('',#80103,#63988,#63989);
#53946=AXIS2_PLACEMENT_3D('',#80105,#63991,#63992);
#53947=AXIS2_PLACEMENT_3D('',#80106,#63993,#63994);
#53948=AXIS2_PLACEMENT_3D('',#80107,#63995,#63996);
#53949=AXIS2_PLACEMENT_3D('',#80108,#63997,#63998);
#53950=AXIS2_PLACEMENT_3D('',#80110,#64000,#64001);
#53951=AXIS2_PLACEMENT_3D('',#80112,#64003,#64004);
#53952=AXIS2_PLACEMENT_3D('',#80113,#64005,#64006);
#53953=AXIS2_PLACEMENT_3D('',#80114,#64007,#64008);
#53954=AXIS2_PLACEMENT_3D('',#80115,#64009,#64010);
#53955=AXIS2_PLACEMENT_3D('',#80117,#64012,#64013);
#53956=AXIS2_PLACEMENT_3D('',#80119,#64015,#64016);
#53957=AXIS2_PLACEMENT_3D('',#80120,#64017,#64018);
#53958=AXIS2_PLACEMENT_3D('',#80121,#64019,#64020);
#53959=AXIS2_PLACEMENT_3D('',#80122,#64021,#64022);
#53960=AXIS2_PLACEMENT_3D('',#80124,#64024,#64025);
#53961=AXIS2_PLACEMENT_3D('',#80126,#64027,#64028);
#53962=AXIS2_PLACEMENT_3D('',#80127,#64029,#64030);
#53963=AXIS2_PLACEMENT_3D('',#80128,#64031,#64032);
#53964=AXIS2_PLACEMENT_3D('',#80129,#64033,#64034);
#53965=AXIS2_PLACEMENT_3D('',#80131,#64036,#64037);
#53966=AXIS2_PLACEMENT_3D('',#80133,#64039,#64040);
#53967=AXIS2_PLACEMENT_3D('',#80134,#64041,#64042);
#53968=AXIS2_PLACEMENT_3D('',#80135,#64043,#64044);
#53969=AXIS2_PLACEMENT_3D('',#80136,#64045,#64046);
#53970=AXIS2_PLACEMENT_3D('',#80138,#64048,#64049);
#53971=AXIS2_PLACEMENT_3D('',#80140,#64051,#64052);
#53972=AXIS2_PLACEMENT_3D('',#80141,#64053,#64054);
#53973=AXIS2_PLACEMENT_3D('',#80142,#64055,#64056);
#53974=AXIS2_PLACEMENT_3D('',#80143,#64057,#64058);
#53975=AXIS2_PLACEMENT_3D('',#80145,#64060,#64061);
#53976=AXIS2_PLACEMENT_3D('',#80147,#64063,#64064);
#53977=AXIS2_PLACEMENT_3D('',#80148,#64065,#64066);
#53978=AXIS2_PLACEMENT_3D('',#80149,#64067,#64068);
#53979=AXIS2_PLACEMENT_3D('',#80150,#64069,#64070);
#53980=AXIS2_PLACEMENT_3D('',#80152,#64072,#64073);
#53981=AXIS2_PLACEMENT_3D('',#80154,#64075,#64076);
#53982=AXIS2_PLACEMENT_3D('',#80155,#64077,#64078);
#53983=AXIS2_PLACEMENT_3D('',#80156,#64079,#64080);
#53984=AXIS2_PLACEMENT_3D('',#80157,#64081,#64082);
#53985=AXIS2_PLACEMENT_3D('',#80159,#64084,#64085);
#53986=AXIS2_PLACEMENT_3D('',#80161,#64087,#64088);
#53987=AXIS2_PLACEMENT_3D('',#80162,#64089,#64090);
#53988=AXIS2_PLACEMENT_3D('',#80163,#64091,#64092);
#53989=AXIS2_PLACEMENT_3D('',#80164,#64093,#64094);
#53990=AXIS2_PLACEMENT_3D('',#80166,#64096,#64097);
#53991=AXIS2_PLACEMENT_3D('',#80168,#64099,#64100);
#53992=AXIS2_PLACEMENT_3D('',#80169,#64101,#64102);
#53993=AXIS2_PLACEMENT_3D('',#80170,#64103,#64104);
#53994=AXIS2_PLACEMENT_3D('',#80171,#64105,#64106);
#53995=AXIS2_PLACEMENT_3D('',#80173,#64108,#64109);
#53996=AXIS2_PLACEMENT_3D('',#80175,#64111,#64112);
#53997=AXIS2_PLACEMENT_3D('',#80176,#64113,#64114);
#53998=AXIS2_PLACEMENT_3D('',#80177,#64115,#64116);
#53999=AXIS2_PLACEMENT_3D('',#80178,#64117,#64118);
#54000=AXIS2_PLACEMENT_3D('',#80180,#64120,#64121);
#54001=AXIS2_PLACEMENT_3D('',#80182,#64123,#64124);
#54002=AXIS2_PLACEMENT_3D('',#80183,#64125,#64126);
#54003=AXIS2_PLACEMENT_3D('',#80184,#64127,#64128);
#54004=AXIS2_PLACEMENT_3D('',#80185,#64129,#64130);
#54005=AXIS2_PLACEMENT_3D('',#80187,#64132,#64133);
#54006=AXIS2_PLACEMENT_3D('',#80189,#64135,#64136);
#54007=AXIS2_PLACEMENT_3D('',#80190,#64137,#64138);
#54008=AXIS2_PLACEMENT_3D('',#80191,#64139,#64140);
#54009=AXIS2_PLACEMENT_3D('',#80192,#64141,#64142);
#54010=AXIS2_PLACEMENT_3D('',#80194,#64144,#64145);
#54011=AXIS2_PLACEMENT_3D('',#80196,#64147,#64148);
#54012=AXIS2_PLACEMENT_3D('',#80197,#64149,#64150);
#54013=AXIS2_PLACEMENT_3D('',#80198,#64151,#64152);
#54014=AXIS2_PLACEMENT_3D('',#80199,#64153,#64154);
#54015=AXIS2_PLACEMENT_3D('',#80201,#64156,#64157);
#54016=AXIS2_PLACEMENT_3D('',#80203,#64159,#64160);
#54017=AXIS2_PLACEMENT_3D('',#80204,#64161,#64162);
#54018=AXIS2_PLACEMENT_3D('',#80205,#64163,#64164);
#54019=AXIS2_PLACEMENT_3D('',#80206,#64165,#64166);
#54020=AXIS2_PLACEMENT_3D('',#80208,#64168,#64169);
#54021=AXIS2_PLACEMENT_3D('',#80210,#64171,#64172);
#54022=AXIS2_PLACEMENT_3D('',#80211,#64173,#64174);
#54023=AXIS2_PLACEMENT_3D('',#80212,#64175,#64176);
#54024=AXIS2_PLACEMENT_3D('',#80213,#64177,#64178);
#54025=AXIS2_PLACEMENT_3D('',#80215,#64180,#64181);
#54026=AXIS2_PLACEMENT_3D('',#80217,#64183,#64184);
#54027=AXIS2_PLACEMENT_3D('',#80218,#64185,#64186);
#54028=AXIS2_PLACEMENT_3D('',#80219,#64187,#64188);
#54029=AXIS2_PLACEMENT_3D('',#80220,#64189,#64190);
#54030=AXIS2_PLACEMENT_3D('',#80222,#64192,#64193);
#54031=AXIS2_PLACEMENT_3D('',#80224,#64195,#64196);
#54032=AXIS2_PLACEMENT_3D('',#80225,#64197,#64198);
#54033=AXIS2_PLACEMENT_3D('',#80226,#64199,#64200);
#54034=AXIS2_PLACEMENT_3D('',#80227,#64201,#64202);
#54035=AXIS2_PLACEMENT_3D('',#80229,#64204,#64205);
#54036=AXIS2_PLACEMENT_3D('',#80231,#64207,#64208);
#54037=AXIS2_PLACEMENT_3D('',#80232,#64209,#64210);
#54038=AXIS2_PLACEMENT_3D('',#80233,#64211,#64212);
#54039=AXIS2_PLACEMENT_3D('',#80234,#64213,#64214);
#54040=AXIS2_PLACEMENT_3D('',#80236,#64216,#64217);
#54041=AXIS2_PLACEMENT_3D('',#80238,#64219,#64220);
#54042=AXIS2_PLACEMENT_3D('',#80239,#64221,#64222);
#54043=AXIS2_PLACEMENT_3D('',#80240,#64223,#64224);
#54044=AXIS2_PLACEMENT_3D('',#80241,#64225,#64226);
#54045=AXIS2_PLACEMENT_3D('',#80243,#64228,#64229);
#54046=AXIS2_PLACEMENT_3D('',#80245,#64231,#64232);
#54047=AXIS2_PLACEMENT_3D('',#80246,#64233,#64234);
#54048=AXIS2_PLACEMENT_3D('',#80247,#64235,#64236);
#54049=AXIS2_PLACEMENT_3D('',#80248,#64237,#64238);
#54050=AXIS2_PLACEMENT_3D('',#80250,#64240,#64241);
#54051=AXIS2_PLACEMENT_3D('',#80252,#64243,#64244);
#54052=AXIS2_PLACEMENT_3D('',#80253,#64245,#64246);
#54053=AXIS2_PLACEMENT_3D('',#80254,#64247,#64248);
#54054=AXIS2_PLACEMENT_3D('',#80255,#64249,#64250);
#54055=AXIS2_PLACEMENT_3D('',#80257,#64252,#64253);
#54056=AXIS2_PLACEMENT_3D('',#80259,#64255,#64256);
#54057=AXIS2_PLACEMENT_3D('',#80260,#64257,#64258);
#54058=AXIS2_PLACEMENT_3D('',#80261,#64259,#64260);
#54059=AXIS2_PLACEMENT_3D('',#80262,#64261,#64262);
#54060=AXIS2_PLACEMENT_3D('',#80264,#64264,#64265);
#54061=AXIS2_PLACEMENT_3D('',#80266,#64267,#64268);
#54062=AXIS2_PLACEMENT_3D('',#80267,#64269,#64270);
#54063=AXIS2_PLACEMENT_3D('',#80268,#64271,#64272);
#54064=AXIS2_PLACEMENT_3D('',#80269,#64273,#64274);
#54065=AXIS2_PLACEMENT_3D('',#80271,#64276,#64277);
#54066=AXIS2_PLACEMENT_3D('',#80273,#64279,#64280);
#54067=AXIS2_PLACEMENT_3D('',#80274,#64281,#64282);
#54068=AXIS2_PLACEMENT_3D('',#80275,#64283,#64284);
#54069=AXIS2_PLACEMENT_3D('',#80276,#64285,#64286);
#54070=AXIS2_PLACEMENT_3D('',#80278,#64288,#64289);
#54071=AXIS2_PLACEMENT_3D('',#80280,#64291,#64292);
#54072=AXIS2_PLACEMENT_3D('',#80281,#64293,#64294);
#54073=AXIS2_PLACEMENT_3D('',#80282,#64295,#64296);
#54074=AXIS2_PLACEMENT_3D('',#80283,#64297,#64298);
#54075=AXIS2_PLACEMENT_3D('',#80285,#64300,#64301);
#54076=AXIS2_PLACEMENT_3D('',#80287,#64303,#64304);
#54077=AXIS2_PLACEMENT_3D('',#80288,#64305,#64306);
#54078=AXIS2_PLACEMENT_3D('',#80289,#64307,#64308);
#54079=AXIS2_PLACEMENT_3D('',#80290,#64309,#64310);
#54080=AXIS2_PLACEMENT_3D('',#80292,#64312,#64313);
#54081=AXIS2_PLACEMENT_3D('',#80294,#64315,#64316);
#54082=AXIS2_PLACEMENT_3D('',#80295,#64317,#64318);
#54083=AXIS2_PLACEMENT_3D('',#80296,#64319,#64320);
#54084=AXIS2_PLACEMENT_3D('',#80297,#64321,#64322);
#54085=AXIS2_PLACEMENT_3D('',#80299,#64324,#64325);
#54086=AXIS2_PLACEMENT_3D('',#80301,#64327,#64328);
#54087=AXIS2_PLACEMENT_3D('',#80302,#64329,#64330);
#54088=AXIS2_PLACEMENT_3D('',#80303,#64331,#64332);
#54089=AXIS2_PLACEMENT_3D('',#80304,#64333,#64334);
#54090=AXIS2_PLACEMENT_3D('',#80306,#64336,#64337);
#54091=AXIS2_PLACEMENT_3D('',#80308,#64339,#64340);
#54092=AXIS2_PLACEMENT_3D('',#80309,#64341,#64342);
#54093=AXIS2_PLACEMENT_3D('',#80310,#64343,#64344);
#54094=AXIS2_PLACEMENT_3D('',#80311,#64345,#64346);
#54095=AXIS2_PLACEMENT_3D('',#80313,#64348,#64349);
#54096=AXIS2_PLACEMENT_3D('',#80315,#64351,#64352);
#54097=AXIS2_PLACEMENT_3D('',#80316,#64353,#64354);
#54098=AXIS2_PLACEMENT_3D('',#80317,#64355,#64356);
#54099=AXIS2_PLACEMENT_3D('',#80318,#64357,#64358);
#54100=AXIS2_PLACEMENT_3D('',#80320,#64360,#64361);
#54101=AXIS2_PLACEMENT_3D('',#80322,#64363,#64364);
#54102=AXIS2_PLACEMENT_3D('',#80323,#64365,#64366);
#54103=AXIS2_PLACEMENT_3D('',#80324,#64367,#64368);
#54104=AXIS2_PLACEMENT_3D('',#80327,#64369,#64370);
#54105=AXIS2_PLACEMENT_3D('',#80329,#64371,#64372);
#54106=AXIS2_PLACEMENT_3D('',#80330,#64373,#64374);
#54107=AXIS2_PLACEMENT_3D('',#80331,#64375,#64376);
#54108=AXIS2_PLACEMENT_3D('',#80332,#64377,#64378);
#54109=AXIS2_PLACEMENT_3D('',#80334,#64379,#64380);
#54110=AXIS2_PLACEMENT_3D('',#80335,#64381,#64382);
#54111=AXIS2_PLACEMENT_3D('',#80337,#64383,#64384);
#54112=AXIS2_PLACEMENT_3D('',#80339,#64386,#64387);
#54113=AXIS2_PLACEMENT_3D('',#80341,#64388,#64389);
#54114=AXIS2_PLACEMENT_3D('',#80343,#64390,#64391);
#54115=AXIS2_PLACEMENT_3D('',#80345,#64392,#64393);
#54116=AXIS2_PLACEMENT_3D('',#80346,#64394,#64395);
#54117=AXIS2_PLACEMENT_3D('',#80347,#64396,#64397);
#54118=AXIS2_PLACEMENT_3D('',#80349,#64398,#64399);
#54119=AXIS2_PLACEMENT_3D('',#80350,#64400,#64401);
#54120=AXIS2_PLACEMENT_3D('',#80352,#64403,#64404);
#54121=AXIS2_PLACEMENT_3D('',#80354,#64405,#64406);
#54122=AXIS2_PLACEMENT_3D('',#80356,#64407,#64408);
#54123=AXIS2_PLACEMENT_3D('',#80357,#64409,#64410);
#54124=AXIS2_PLACEMENT_3D('',#80358,#64411,#64412);
#54125=AXIS2_PLACEMENT_3D('',#80360,#64413,#64414);
#54126=AXIS2_PLACEMENT_3D('',#80362,#64416,#64417);
#54127=AXIS2_PLACEMENT_3D('',#80365,#64418,#64419);
#54128=AXIS2_PLACEMENT_3D('',#80366,#64420,#64421);
#54129=AXIS2_PLACEMENT_3D('',#80367,#64422,#64423);
#54130=AXIS2_PLACEMENT_3D('',#80368,#64424,#64425);
#54131=AXIS2_PLACEMENT_3D('',#80371,#64427,#64428);
#54132=AXIS2_PLACEMENT_3D('',#80372,#64429,#64430);
#54133=AXIS2_PLACEMENT_3D('',#80374,#64431,#64432);
#54134=AXIS2_PLACEMENT_3D('',#80377,#64434,#64435);
#54135=AXIS2_PLACEMENT_3D('',#80378,#64436,#64437);
#54136=AXIS2_PLACEMENT_3D('',#80381,#64439,#64440);
#54137=AXIS2_PLACEMENT_3D('',#80382,#64441,#64442);
#54138=AXIS2_PLACEMENT_3D('',#80383,#64443,#64444);
#54139=AXIS2_PLACEMENT_3D('',#80384,#64445,#64446);
#54140=AXIS2_PLACEMENT_3D('',#80386,#64447,#64448);
#54141=AXIS2_PLACEMENT_3D('',#80387,#64449,#64450);
#54142=AXIS2_PLACEMENT_3D('',#80389,#64452,#64453);
#54143=AXIS2_PLACEMENT_3D('',#80390,#64454,#64455);
#54144=AXIS2_PLACEMENT_3D('',#80392,#64456,#64457);
#54145=AXIS2_PLACEMENT_3D('',#80395,#64459,#64460);
#54146=AXIS2_PLACEMENT_3D('',#80396,#64461,#64462);
#54147=AXIS2_PLACEMENT_3D('',#80398,#64463,#64464);
#54148=AXIS2_PLACEMENT_3D('',#80400,#64465,#64466);
#54149=AXIS2_PLACEMENT_3D('',#80402,#64467,#64468);
#54150=AXIS2_PLACEMENT_3D('',#80404,#64469,#64470);
#54151=AXIS2_PLACEMENT_3D('',#80406,#64471,#64472);
#54152=AXIS2_PLACEMENT_3D('',#80408,#64473,#64474);
#54153=AXIS2_PLACEMENT_3D('',#80410,#64475,#64476);
#54154=AXIS2_PLACEMENT_3D('',#80411,#64477,#64478);
#54155=AXIS2_PLACEMENT_3D('',#80413,#64479,#64480);
#54156=AXIS2_PLACEMENT_3D('',#80415,#64482,#64483);
#54157=AXIS2_PLACEMENT_3D('',#80418,#64485,#64486);
#54158=AXIS2_PLACEMENT_3D('',#80419,#64487,#64488);
#54159=AXIS2_PLACEMENT_3D('',#80421,#64489,#64490);
#54160=AXIS2_PLACEMENT_3D('',#80423,#64492,#64493);
#54161=AXIS2_PLACEMENT_3D('',#80425,#64494,#64495);
#54162=AXIS2_PLACEMENT_3D('',#80428,#64497,#64498);
#54163=AXIS2_PLACEMENT_3D('',#80429,#64499,#64500);
#54164=AXIS2_PLACEMENT_3D('',#80431,#64501,#64502);
#54165=AXIS2_PLACEMENT_3D('',#80434,#64504,#64505);
#54166=AXIS2_PLACEMENT_3D('',#80435,#64506,#64507);
#54167=AXIS2_PLACEMENT_3D('',#80437,#64508,#64509);
#54168=AXIS2_PLACEMENT_3D('',#80440,#64511,#64512);
#54169=AXIS2_PLACEMENT_3D('',#80441,#64513,#64514);
#54170=AXIS2_PLACEMENT_3D('',#80443,#64515,#64516);
#54171=AXIS2_PLACEMENT_3D('',#80446,#64518,#64519);
#54172=AXIS2_PLACEMENT_3D('',#80447,#64520,#64521);
#54173=AXIS2_PLACEMENT_3D('',#80449,#64522,#64523);
#54174=AXIS2_PLACEMENT_3D('',#80451,#64525,#64526);
#54175=AXIS2_PLACEMENT_3D('',#80452,#64527,#64528);
#54176=AXIS2_PLACEMENT_3D('',#80454,#64529,#64530);
#54177=AXIS2_PLACEMENT_3D('',#80456,#64532,#64533);
#54178=AXIS2_PLACEMENT_3D('',#80457,#64534,#64535);
#54179=AXIS2_PLACEMENT_3D('',#80459,#64536,#64537);
#54180=AXIS2_PLACEMENT_3D('',#80461,#64539,#64540);
#54181=AXIS2_PLACEMENT_3D('',#80462,#64541,#64542);
#54182=AXIS2_PLACEMENT_3D('',#80464,#64543,#64544);
#54183=AXIS2_PLACEMENT_3D('',#80466,#64546,#64547);
#54184=AXIS2_PLACEMENT_3D('',#80467,#64548,#64549);
#54185=AXIS2_PLACEMENT_3D('',#80471,#64551,#64552);
#54186=AXIS2_PLACEMENT_3D('',#80472,#64553,#64554);
#54187=AXIS2_PLACEMENT_3D('',#80475,#64556,#64557);
#54188=AXIS2_PLACEMENT_3D('',#80476,#64558,#64559);
#54189=AXIS2_PLACEMENT_3D('',#80479,#64561,#64562);
#54190=AXIS2_PLACEMENT_3D('',#80480,#64563,#64564);
#54191=AXIS2_PLACEMENT_3D('',#80482,#64565,#64566);
#54192=AXIS2_PLACEMENT_3D('',#80484,#64567,#64568);
#54193=AXIS2_PLACEMENT_3D('',#80485,#64569,#64570);
#54194=AXIS2_PLACEMENT_3D('',#80486,#64571,#64572);
#54195=AXIS2_PLACEMENT_3D('',#80488,#64573,#64574);
#54196=AXIS2_PLACEMENT_3D('',#80490,#64576,#64577);
#54197=AXIS2_PLACEMENT_3D('',#80492,#64578,#64579);
#54198=AXIS2_PLACEMENT_3D('',#80493,#64580,#64581);
#54199=AXIS2_PLACEMENT_3D('',#80495,#64582,#64583);
#54200=AXIS2_PLACEMENT_3D('',#80497,#64585,#64586);
#54201=AXIS2_PLACEMENT_3D('',#80499,#64587,#64588);
#54202=AXIS2_PLACEMENT_3D('',#80501,#64590,#64591);
#54203=AXIS2_PLACEMENT_3D('',#80503,#64592,#64593);
#54204=AXIS2_PLACEMENT_3D('',#80504,#64594,#64595);
#54205=AXIS2_PLACEMENT_3D('',#80506,#64596,#64597);
#54206=AXIS2_PLACEMENT_3D('',#80508,#64599,#64600);
#54207=AXIS2_PLACEMENT_3D('',#80510,#64601,#64602);
#54208=AXIS2_PLACEMENT_3D('',#80512,#64604,#64605);
#54209=AXIS2_PLACEMENT_3D('',#80514,#64607,#64608);
#54210=AXIS2_PLACEMENT_3D('',#80516,#64609,#64610);
#54211=AXIS2_PLACEMENT_3D('',#80517,#64611,#64612);
#54212=AXIS2_PLACEMENT_3D('',#80519,#64613,#64614);
#54213=AXIS2_PLACEMENT_3D('',#80521,#64616,#64617);
#54214=AXIS2_PLACEMENT_3D('',#80523,#64618,#64619);
#54215=AXIS2_PLACEMENT_3D('',#80525,#64621,#64622);
#54216=AXIS2_PLACEMENT_3D('',#80526,#64623,#64624);
#54217=AXIS2_PLACEMENT_3D('',#80527,#64625,#64626);
#54218=AXIS2_PLACEMENT_3D('',#80536,#64631,#64632);
#54219=AXIS2_PLACEMENT_3D('',#80542,#64636,#64637);
#54220=AXIS2_PLACEMENT_3D('',#80548,#64641,#64642);
#54221=AXIS2_PLACEMENT_3D('',#80554,#64646,#64647);
#54222=AXIS2_PLACEMENT_3D('',#80560,#64651,#64652);
#54223=AXIS2_PLACEMENT_3D('',#80566,#64656,#64657);
#54224=AXIS2_PLACEMENT_3D('',#80572,#64661,#64662);
#54225=AXIS2_PLACEMENT_3D('',#80578,#64666,#64667);
#54226=AXIS2_PLACEMENT_3D('',#80584,#64671,#64672);
#54227=AXIS2_PLACEMENT_3D('',#80590,#64676,#64677);
#54228=AXIS2_PLACEMENT_3D('',#80596,#64681,#64682);
#54229=AXIS2_PLACEMENT_3D('',#80599,#64685,#64686);
#54230=AXIS2_PLACEMENT_3D('',#80600,#64687,#64688);
#54231=AXIS2_PLACEMENT_3D('',#80609,#64693,#64694);
#54232=AXIS2_PLACEMENT_3D('',#80615,#64698,#64699);
#54233=AXIS2_PLACEMENT_3D('',#80621,#64703,#64704);
#54234=AXIS2_PLACEMENT_3D('',#80624,#64707,#64708);
#54235=AXIS2_PLACEMENT_3D('',#80823,#64723,#64724);
#54236=AXIS2_PLACEMENT_3D('',#81099,#64746,#64747);
#54237=AXIS2_PLACEMENT_3D('',#81132,#64752,#64753);
#54238=AXIS2_PLACEMENT_3D('',#81256,#64763,#64764);
#54239=AXIS2_PLACEMENT_3D('',#81412,#64778,#64779);
#54240=AXIS2_PLACEMENT_3D('',#81445,#64784,#64785);
#54241=AXIS2_PLACEMENT_3D('',#81446,#64786,#64787);
#54242=AXIS2_PLACEMENT_3D('',#81455,#64792,#64793);
#54243=AXIS2_PLACEMENT_3D('',#81461,#64797,#64798);
#54244=AXIS2_PLACEMENT_3D('',#81467,#64802,#64803);
#54245=AXIS2_PLACEMENT_3D('',#81473,#64807,#64808);
#54246=AXIS2_PLACEMENT_3D('',#81479,#64812,#64813);
#54247=AXIS2_PLACEMENT_3D('',#81482,#64816,#64817);
#54248=AXIS2_PLACEMENT_3D('',#81483,#64818,#64819);
#54249=AXIS2_PLACEMENT_3D('',#81492,#64824,#64825);
#54250=AXIS2_PLACEMENT_3D('',#81498,#64829,#64830);
#54251=AXIS2_PLACEMENT_3D('',#81504,#64834,#64835);
#54252=AXIS2_PLACEMENT_3D('',#81510,#64839,#64840);
#54253=AXIS2_PLACEMENT_3D('',#81516,#64844,#64845);
#54254=AXIS2_PLACEMENT_3D('',#81522,#64849,#64850);
#54255=AXIS2_PLACEMENT_3D('',#81528,#64854,#64855);
#54256=AXIS2_PLACEMENT_3D('',#81531,#64858,#64859);
#54257=AXIS2_PLACEMENT_3D('',#81595,#64865,#64866);
#54258=AXIS2_PLACEMENT_3D('',#81601,#64870,#64871);
#54259=AXIS2_PLACEMENT_3D('',#81607,#64875,#64876);
#54260=AXIS2_PLACEMENT_3D('',#81703,#64886,#64887);
#54261=AXIS2_PLACEMENT_3D('',#81709,#64891,#64892);
#54262=AXIS2_PLACEMENT_3D('',#81715,#64896,#64897);
#54263=AXIS2_PLACEMENT_3D('',#81733,#64901,#64902);
#54264=AXIS2_PLACEMENT_3D('',#81734,#64903,#64904);
#54265=AXIS2_PLACEMENT_3D('',#81803,#64913,#64914);
#54266=AXIS2_PLACEMENT_3D('',#81809,#64918,#64919);
#54267=AXIS2_PLACEMENT_3D('',#81815,#64923,#64924);
#54268=AXIS2_PLACEMENT_3D('',#81926,#64935,#64936);
#54269=AXIS2_PLACEMENT_3D('',#81932,#64940,#64941);
#54270=AXIS2_PLACEMENT_3D('',#81938,#64945,#64946);
#54271=AXIS2_PLACEMENT_3D('',#81944,#64950,#64951);
#54272=AXIS2_PLACEMENT_3D('',#81947,#64954,#64955);
#54273=AXIS2_PLACEMENT_3D('',#81948,#64956,#64957);
#54274=AXIS2_PLACEMENT_3D('',#81957,#64962,#64963);
#54275=AXIS2_PLACEMENT_3D('',#81963,#64967,#64968);
#54276=AXIS2_PLACEMENT_3D('',#81969,#64972,#64973);
#54277=AXIS2_PLACEMENT_3D('',#81975,#64977,#64978);
#54278=AXIS2_PLACEMENT_3D('',#81981,#64982,#64983);
#54279=AXIS2_PLACEMENT_3D('',#81987,#64987,#64988);
#54280=AXIS2_PLACEMENT_3D('',#81993,#64992,#64993);
#54281=AXIS2_PLACEMENT_3D('',#81996,#64996,#64997);
#54282=AXIS2_PLACEMENT_3D('',#82030,#65001,#65002);
#54283=AXIS2_PLACEMENT_3D('',#82066,#65008,#65009);
#54284=AXIS2_PLACEMENT_3D('',#82072,#65013,#65014);
#54285=AXIS2_PLACEMENT_3D('',#82078,#65018,#65019);
#54286=AXIS2_PLACEMENT_3D('',#82084,#65023,#65024);
#54287=AXIS2_PLACEMENT_3D('',#82087,#65027,#65028);
#54288=AXIS2_PLACEMENT_3D('',#82268,#65041,#65042);
#54289=AXIS2_PLACEMENT_3D('',#82302,#65046,#65047);
#54290=AXIS2_PLACEMENT_3D('',#82338,#65053,#65054);
#54291=AXIS2_PLACEMENT_3D('',#82344,#65058,#65059);
#54292=AXIS2_PLACEMENT_3D('',#82350,#65063,#65064);
#54293=AXIS2_PLACEMENT_3D('',#82356,#65068,#65069);
#54294=AXIS2_PLACEMENT_3D('',#82359,#65072,#65073);
#54295=AXIS2_PLACEMENT_3D('',#82360,#65074,#65075);
#54296=AXIS2_PLACEMENT_3D('',#82369,#65080,#65081);
#54297=AXIS2_PLACEMENT_3D('',#82375,#65085,#65086);
#54298=AXIS2_PLACEMENT_3D('',#82381,#65090,#65091);
#54299=AXIS2_PLACEMENT_3D('',#82384,#65094,#65095);
#54300=AXIS2_PLACEMENT_3D('',#82463,#65102,#65103);
#54301=AXIS2_PLACEMENT_3D('',#82469,#65107,#65108);
#54302=AXIS2_PLACEMENT_3D('',#82475,#65112,#65113);
#54303=AXIS2_PLACEMENT_3D('',#82481,#65117,#65118);
#54304=AXIS2_PLACEMENT_3D('',#82487,#65122,#65123);
#54305=AXIS2_PLACEMENT_3D('',#82493,#65127,#65128);
#54306=AXIS2_PLACEMENT_3D('',#82619,#65140,#65141);
#54307=AXIS2_PLACEMENT_3D('',#82652,#65146,#65147);
#54308=AXIS2_PLACEMENT_3D('',#82818,#65159,#65160);
#54309=AXIS2_PLACEMENT_3D('',#82987,#65173,#65174);
#54310=AXIS2_PLACEMENT_3D('',#83035,#65180,#65181);
#54311=AXIS2_PLACEMENT_3D('',#83036,#65182,#65183);
#54312=AXIS2_PLACEMENT_3D('',#83045,#65188,#65189);
#54313=AXIS2_PLACEMENT_3D('',#83051,#65193,#65194);
#54314=AXIS2_PLACEMENT_3D('',#83057,#65198,#65199);
#54315=AXIS2_PLACEMENT_3D('',#83063,#65203,#65204);
#54316=AXIS2_PLACEMENT_3D('',#83069,#65208,#65209);
#54317=AXIS2_PLACEMENT_3D('',#83075,#65213,#65214);
#54318=AXIS2_PLACEMENT_3D('',#83081,#65218,#65219);
#54319=AXIS2_PLACEMENT_3D('',#83087,#65223,#65224);
#54320=AXIS2_PLACEMENT_3D('',#83093,#65228,#65229);
#54321=AXIS2_PLACEMENT_3D('',#83099,#65233,#65234);
#54322=AXIS2_PLACEMENT_3D('',#83105,#65238,#65239);
#54323=AXIS2_PLACEMENT_3D('',#83108,#65242,#65243);
#54324=AXIS2_PLACEMENT_3D('',#83109,#65244,#65245);
#54325=AXIS2_PLACEMENT_3D('',#83118,#65250,#65251);
#54326=AXIS2_PLACEMENT_3D('',#83124,#65255,#65256);
#54327=AXIS2_PLACEMENT_3D('',#83130,#65260,#65261);
#54328=AXIS2_PLACEMENT_3D('',#83133,#65264,#65265);
#54329=AXIS2_PLACEMENT_3D('',#83299,#65277,#65278);
#54330=AXIS2_PLACEMENT_3D('',#83300,#65279,#65280);
#54331=AXIS2_PLACEMENT_3D('',#83309,#65285,#65286);
#54332=AXIS2_PLACEMENT_3D('',#83315,#65290,#65291);
#54333=AXIS2_PLACEMENT_3D('',#83321,#65295,#65296);
#54334=AXIS2_PLACEMENT_3D('',#83327,#65300,#65301);
#54335=AXIS2_PLACEMENT_3D('',#83333,#65305,#65306);
#54336=AXIS2_PLACEMENT_3D('',#83339,#65310,#65311);
#54337=AXIS2_PLACEMENT_3D('',#83345,#65315,#65316);
#54338=AXIS2_PLACEMENT_3D('',#83351,#65320,#65321);
#54339=AXIS2_PLACEMENT_3D('',#83357,#65325,#65326);
#54340=AXIS2_PLACEMENT_3D('',#83363,#65330,#65331);
#54341=AXIS2_PLACEMENT_3D('',#83369,#65335,#65336);
#54342=AXIS2_PLACEMENT_3D('',#83372,#65339,#65340);
#54343=AXIS2_PLACEMENT_3D('',#83373,#65341,#65342);
#54344=AXIS2_PLACEMENT_3D('',#83382,#65347,#65348);
#54345=AXIS2_PLACEMENT_3D('',#83388,#65352,#65353);
#54346=AXIS2_PLACEMENT_3D('',#83394,#65357,#65358);
#54347=AXIS2_PLACEMENT_3D('',#83400,#65362,#65363);
#54348=AXIS2_PLACEMENT_3D('',#83406,#65367,#65368);
#54349=AXIS2_PLACEMENT_3D('',#83409,#65371,#65372);
#54350=AXIS2_PLACEMENT_3D('',#83533,#65382,#65383);
#54351=AXIS2_PLACEMENT_3D('',#83539,#65387,#65388);
#54352=AXIS2_PLACEMENT_3D('',#83545,#65392,#65393);
#54353=AXIS2_PLACEMENT_3D('',#83563,#65397,#65398);
#54354=AXIS2_PLACEMENT_3D('',#83564,#65399,#65400);
#54355=AXIS2_PLACEMENT_3D('',#83633,#65409,#65410);
#54356=AXIS2_PLACEMENT_3D('',#83639,#65414,#65415);
#54357=AXIS2_PLACEMENT_3D('',#83645,#65419,#65420);
#54358=AXIS2_PLACEMENT_3D('',#83756,#65431,#65432);
#54359=AXIS2_PLACEMENT_3D('',#83762,#65436,#65437);
#54360=AXIS2_PLACEMENT_3D('',#83768,#65441,#65442);
#54361=AXIS2_PLACEMENT_3D('',#83774,#65446,#65447);
#54362=AXIS2_PLACEMENT_3D('',#83777,#65450,#65451);
#54363=AXIS2_PLACEMENT_3D('',#83778,#65452,#65453);
#54364=AXIS2_PLACEMENT_3D('',#83787,#65458,#65459);
#54365=AXIS2_PLACEMENT_3D('',#83793,#65463,#65464);
#54366=AXIS2_PLACEMENT_3D('',#83799,#65468,#65469);
#54367=AXIS2_PLACEMENT_3D('',#83802,#65472,#65473);
#54368=AXIS2_PLACEMENT_3D('',#83803,#65474,#65475);
#54369=AXIS2_PLACEMENT_3D('',#83805,#65476,#65477);
#54370=AXIS2_PLACEMENT_3D('',#83808,#65479,#65480);
#54371=AXIS2_PLACEMENT_3D('',#83809,#65481,#65482);
#54372=AXIS2_PLACEMENT_3D('',#83811,#65483,#65484);
#54373=AXIS2_PLACEMENT_3D('',#83813,#65486,#65487);
#54374=AXIS2_PLACEMENT_3D('',#83818,#65489,#65490);
#54375=AXIS2_PLACEMENT_3D('',#83822,#65492,#65493);
#54376=AXIS2_PLACEMENT_3D('',#83826,#65495,#65496);
#54377=AXIS2_PLACEMENT_3D('',#83829,#65498,#65499);
#54378=AXIS2_PLACEMENT_3D('',#83831,#65500,#65501);
#54379=AXIS2_PLACEMENT_3D('',#83833,#65502,#65503);
#54380=AXIS2_PLACEMENT_3D('',#83835,#65504,#65505);
#54381=AXIS2_PLACEMENT_3D('',#83837,#65506,#65507);
#54382=AXIS2_PLACEMENT_3D('',#83839,#65508,#65509);
#54383=AXIS2_PLACEMENT_3D('',#83841,#65510,#65511);
#54384=AXIS2_PLACEMENT_3D('',#83843,#65512,#65513);
#54385=AXIS2_PLACEMENT_3D('',#83845,#65514,#65515);
#54386=AXIS2_PLACEMENT_3D('',#83847,#65516,#65517);
#54387=AXIS2_PLACEMENT_3D('',#83849,#65518,#65519);
#54388=AXIS2_PLACEMENT_3D('',#83850,#65520,#65521);
#54389=AXIS2_PLACEMENT_3D('',#83852,#65522,#65523);
#54390=AXIS2_PLACEMENT_3D('',#83854,#65525,#65526);
#54391=AXIS2_PLACEMENT_3D('',#83857,#65527,#65528);
#54392=AXIS2_PLACEMENT_3D('',#83861,#65530,#65531);
#54393=AXIS2_PLACEMENT_3D('',#83865,#65533,#65534);
#54394=AXIS2_PLACEMENT_3D('',#83869,#65536,#65537);
#54395=AXIS2_PLACEMENT_3D('',#83872,#65539,#65540);
#54396=AXIS2_PLACEMENT_3D('',#83874,#65541,#65542);
#54397=AXIS2_PLACEMENT_3D('',#83876,#65543,#65544);
#54398=AXIS2_PLACEMENT_3D('',#83877,#65545,#65546);
#54399=AXIS2_PLACEMENT_3D('',#83880,#65548,#65549);
#54400=AXIS2_PLACEMENT_3D('',#83881,#65550,#65551);
#54401=AXIS2_PLACEMENT_3D('',#83883,#65552,#65553);
#54402=AXIS2_PLACEMENT_3D('',#83885,#65555,#65556);
#54403=AXIS2_PLACEMENT_3D('',#83887,#65558,#65559);
#54404=AXIS2_PLACEMENT_3D('',#83890,#65561,#65562);
#54405=AXIS2_PLACEMENT_3D('',#83891,#65563,#65564);
#54406=AXIS2_PLACEMENT_3D('',#83893,#65565,#65566);
#54407=AXIS2_PLACEMENT_3D('',#83895,#65568,#65569);
#54408=AXIS2_PLACEMENT_3D('',#83897,#65571,#65572);
#54409=AXIS2_PLACEMENT_3D('',#83900,#65574,#65575);
#54410=AXIS2_PLACEMENT_3D('',#83901,#65576,#65577);
#54411=AXIS2_PLACEMENT_3D('',#83903,#65578,#65579);
#54412=AXIS2_PLACEMENT_3D('',#83905,#65581,#65582);
#54413=AXIS2_PLACEMENT_3D('',#83907,#65584,#65585);
#54414=AXIS2_PLACEMENT_3D('',#83909,#65586,#65587);
#54415=AXIS2_PLACEMENT_3D('',#83912,#65589,#65590);
#54416=AXIS2_PLACEMENT_3D('',#83914,#65592,#65593);
#54417=AXIS2_PLACEMENT_3D('',#83916,#65594,#65595);
#54418=AXIS2_PLACEMENT_3D('',#83919,#65597,#65598);
#54419=AXIS2_PLACEMENT_3D('',#83921,#65600,#65601);
#54420=AXIS2_PLACEMENT_3D('',#83923,#65602,#65603);
#54421=AXIS2_PLACEMENT_3D('',#83926,#65605,#65606);
#54422=AXIS2_PLACEMENT_3D('',#83929,#65608,#65609);
#54423=AXIS2_PLACEMENT_3D('',#83930,#65610,#65611);
#54424=AXIS2_PLACEMENT_3D('',#83932,#65613,#65614);
#54425=AXIS2_PLACEMENT_3D('',#83934,#65615,#65616);
#54426=AXIS2_PLACEMENT_3D('',#83937,#65618,#65619);
#54427=AXIS2_PLACEMENT_3D('',#83940,#65621,#65622);
#54428=AXIS2_PLACEMENT_3D('',#83941,#65623,#65624);
#54429=AXIS2_PLACEMENT_3D('',#83943,#65626,#65627);
#54430=AXIS2_PLACEMENT_3D('',#83945,#65628,#65629);
#54431=AXIS2_PLACEMENT_3D('',#83948,#65631,#65632);
#54432=AXIS2_PLACEMENT_3D('',#83951,#65634,#65635);
#54433=AXIS2_PLACEMENT_3D('',#83952,#65636,#65637);
#54434=AXIS2_PLACEMENT_3D('',#83954,#65639,#65640);
#54435=AXIS2_PLACEMENT_3D('',#83956,#65641,#65642);
#54436=AXIS2_PLACEMENT_3D('',#83959,#65644,#65645);
#54437=AXIS2_PLACEMENT_3D('',#83962,#65647,#65648);
#54438=AXIS2_PLACEMENT_3D('',#83963,#65649,#65650);
#54439=AXIS2_PLACEMENT_3D('',#83965,#65652,#65653);
#54440=AXIS2_PLACEMENT_3D('',#83967,#65654,#65655);
#54441=AXIS2_PLACEMENT_3D('',#83969,#65657,#65658);
#54442=AXIS2_PLACEMENT_3D('',#83970,#65659,#65660);
#54443=AXIS2_PLACEMENT_3D('',#83974,#65662,#65663);
#54444=AXIS2_PLACEMENT_3D('',#83976,#65665,#65666);
#54445=AXIS2_PLACEMENT_3D('',#83980,#65669,#65670);
#54446=AXIS2_PLACEMENT_3D('',#83983,#65672,#65673);
#54447=AXIS2_PLACEMENT_3D('',#83984,#65674,#65675);
#54448=AXIS2_PLACEMENT_3D('',#83988,#65678,#65679);
#54449=AXIS2_PLACEMENT_3D('',#83991,#65681,#65682);
#54450=AXIS2_PLACEMENT_3D('',#83992,#65683,#65684);
#54451=AXIS2_PLACEMENT_3D('',#83996,#65687,#65688);
#54452=AXIS2_PLACEMENT_3D('',#83999,#65690,#65691);
#54453=AXIS2_PLACEMENT_3D('',#84000,#65692,#65693);
#54454=AXIS2_PLACEMENT_3D('',#84002,#65695,#65696);
#54455=AXIS2_PLACEMENT_3D('',#84008,#65700,#65701);
#54456=AXIS2_PLACEMENT_3D('',#84011,#65703,#65704);
#54457=AXIS2_PLACEMENT_3D('',#84012,#65705,#65706);
#54458=AXIS2_PLACEMENT_3D('',#84016,#65709,#65710);
#54459=AXIS2_PLACEMENT_3D('',#84019,#65712,#65713);
#54460=AXIS2_PLACEMENT_3D('',#84020,#65714,#65715);
#54461=AXIS2_PLACEMENT_3D('',#84023,#65718,#65719);
#54462=AXIS2_PLACEMENT_3D('',#84025,#65721,#65722);
#54463=AXIS2_PLACEMENT_3D('',#84027,#65724,#65725);
#54464=AXIS2_PLACEMENT_3D('',#84029,#65727,#65728);
#54465=AXIS2_PLACEMENT_3D('',#84033,#65731,#65732);
#54466=AXIS2_PLACEMENT_3D('',#84036,#65734,#65735);
#54467=AXIS2_PLACEMENT_3D('',#84037,#65736,#65737);
#54468=AXIS2_PLACEMENT_3D('',#84041,#65740,#65741);
#54469=AXIS2_PLACEMENT_3D('',#84042,#65742,#65743);
#54470=AXIS2_PLACEMENT_3D('',#84043,#65744,#65745);
#54471=AXIS2_PLACEMENT_3D('',#84045,#65747,#65748);
#54472=AXIS2_PLACEMENT_3D('',#84047,#65750,#65751);
#54473=AXIS2_PLACEMENT_3D('',#84049,#65753,#65754);
#54474=AXIS2_PLACEMENT_3D('',#84050,#65755,#65756);
#54475=AXIS2_PLACEMENT_3D('',#84051,#65757,#65758);
#54476=AXIS2_PLACEMENT_3D('',#84053,#65759,#65760);
#54477=AXIS2_PLACEMENT_3D('',#84056,#65762,#65763);
#54478=AXIS2_PLACEMENT_3D('',#84057,#65764,#65765);
#54479=AXIS2_PLACEMENT_3D('',#84060,#65767,#65768);
#54480=AXIS2_PLACEMENT_3D('',#84061,#65769,#65770);
#54481=AXIS2_PLACEMENT_3D('',#84063,#65771,#65772);
#54482=AXIS2_PLACEMENT_3D('',#84064,#65773,#65774);
#54483=AXIS2_PLACEMENT_3D('',#84066,#65775,#65776);
#54484=AXIS2_PLACEMENT_3D('',#84068,#65778,#65779);
#54485=AXIS2_PLACEMENT_3D('',#84070,#65780,#65781);
#54486=AXIS2_PLACEMENT_3D('',#84072,#65783,#65784);
#54487=AXIS2_PLACEMENT_3D('',#84074,#65785,#65786);
#54488=AXIS2_PLACEMENT_3D('',#84076,#65788,#65789);
#54489=AXIS2_PLACEMENT_3D('',#84078,#65790,#65791);
#54490=AXIS2_PLACEMENT_3D('',#84079,#65792,#65793);
#54491=AXIS2_PLACEMENT_3D('',#84081,#65795,#65796);
#54492=AXIS2_PLACEMENT_3D('',#84082,#65797,#65798);
#54493=AXIS2_PLACEMENT_3D('',#84098,#65800,#65801);
#54494=AXIS2_PLACEMENT_3D('',#84109,#65802,#65803);
#54495=AXIS2_PLACEMENT_3D('',#84157,#65805,#65806);
#54496=AXIS2_PLACEMENT_3D('',#84205,#65808,#65809);
#54497=AXIS2_PLACEMENT_3D('',#84259,#65811,#65812);
#54498=AXIS2_PLACEMENT_3D('',#84307,#65814,#65815);
#54499=AXIS2_PLACEMENT_3D('',#84355,#65817,#65818);
#54500=AXIS2_PLACEMENT_3D('',#84409,#65820,#65821);
#54501=AXIS2_PLACEMENT_3D('',#84457,#65823,#65824);
#54502=AXIS2_PLACEMENT_3D('',#84505,#65826,#65827);
#54503=AXIS2_PLACEMENT_3D('',#84559,#65829,#65830);
#54504=AXIS2_PLACEMENT_3D('',#84607,#65832,#65833);
#54505=AXIS2_PLACEMENT_3D('',#84655,#65835,#65836);
#54506=AXIS2_PLACEMENT_3D('',#84709,#65838,#65839);
#54507=AXIS2_PLACEMENT_3D('',#84757,#65841,#65842);
#54508=AXIS2_PLACEMENT_3D('',#84805,#65844,#65845);
#54509=AXIS2_PLACEMENT_3D('',#84859,#65847,#65848);
#54510=AXIS2_PLACEMENT_3D('',#84868,#65850,#65851);
#54511=AXIS2_PLACEMENT_3D('',#84869,#65852,#65853);
#54512=AXIS2_PLACEMENT_3D('',#84885,#65855,#65856);
#54513=AXIS2_PLACEMENT_3D('',#84896,#65857,#65858);
#54514=AXIS2_PLACEMENT_3D('',#84921,#65860,#65861);
#54515=AXIS2_PLACEMENT_3D('',#84945,#65863,#65864);
#54516=AXIS2_PLACEMENT_3D('',#84970,#65866,#65867);
#54517=AXIS2_PLACEMENT_3D('',#84995,#65869,#65870);
#54518=AXIS2_PLACEMENT_3D('',#85019,#65872,#65873);
#54519=AXIS2_PLACEMENT_3D('',#85044,#65875,#65876);
#54520=AXIS2_PLACEMENT_3D('',#85069,#65878,#65879);
#54521=AXIS2_PLACEMENT_3D('',#85093,#65881,#65882);
#54522=AXIS2_PLACEMENT_3D('',#85118,#65884,#65885);
#54523=AXIS2_PLACEMENT_3D('',#85143,#65887,#65888);
#54524=AXIS2_PLACEMENT_3D('',#85167,#65890,#65891);
#54525=AXIS2_PLACEMENT_3D('',#85192,#65893,#65894);
#54526=AXIS2_PLACEMENT_3D('',#85217,#65896,#65897);
#54527=AXIS2_PLACEMENT_3D('',#85241,#65899,#65900);
#54528=AXIS2_PLACEMENT_3D('',#85350,#65901,#65902);
#54529=AXIS2_PLACEMENT_3D('',#85352,#65903,#65904);
#54530=AXIS2_PLACEMENT_3D('',#86016,#65905,#65906);
#54531=AXIS2_PLACEMENT_3D('',#86018,#65907,#65908);
#54532=AXIS2_PLACEMENT_3D('',#86019,#65909,#65910);
#54533=AXIS2_PLACEMENT_3D('',#86127,#65911,#65912);
#54534=AXIS2_PLACEMENT_3D('',#86128,#65913,#65914);
#54535=AXIS2_PLACEMENT_3D('',#86579,#65915,#65916);
#54536=AXIS2_PLACEMENT_3D('',#86581,#65917,#65918);
#54537=AXIS2_PLACEMENT_3D('',#86582,#65919,#65920);
#54538=AXIS2_PLACEMENT_3D('',#86583,#65921,#65922);
#54539=AXIS2_PLACEMENT_3D('',#86584,#65923,#65924);
#54540=AXIS2_PLACEMENT_3D('',#86585,#65925,#65926);
#54541=AXIS2_PLACEMENT_3D('',#86587,#65927,#65928);
#54542=AXIS2_PLACEMENT_3D('',#86588,#65929,#65930);
#54543=AXIS2_PLACEMENT_3D('',#86597,#65935,#65936);
#54544=AXIS2_PLACEMENT_3D('',#86599,#65937,#65938);
#54545=AXIS2_PLACEMENT_3D('',#86601,#65940,#65941);
#54546=AXIS2_PLACEMENT_3D('',#86605,#65944,#65945);
#54547=AXIS2_PLACEMENT_3D('',#86606,#65946,#65947);
#54548=AXIS2_PLACEMENT_3D('',#86607,#65948,#65949);
#54549=AXIS2_PLACEMENT_3D('',#86616,#65954,#65955);
#54550=AXIS2_PLACEMENT_3D('',#86618,#65956,#65957);
#54551=AXIS2_PLACEMENT_3D('',#86620,#65959,#65960);
#54552=AXIS2_PLACEMENT_3D('',#86624,#65963,#65964);
#54553=AXIS2_PLACEMENT_3D('',#86625,#65965,#65966);
#54554=AXIS2_PLACEMENT_3D('',#86626,#65967,#65968);
#54555=AXIS2_PLACEMENT_3D('',#86635,#65973,#65974);
#54556=AXIS2_PLACEMENT_3D('',#86637,#65975,#65976);
#54557=AXIS2_PLACEMENT_3D('',#86639,#65978,#65979);
#54558=AXIS2_PLACEMENT_3D('',#86643,#65982,#65983);
#54559=AXIS2_PLACEMENT_3D('',#86644,#65984,#65985);
#54560=AXIS2_PLACEMENT_3D('',#86645,#65986,#65987);
#54561=AXIS2_PLACEMENT_3D('',#86654,#65992,#65993);
#54562=AXIS2_PLACEMENT_3D('',#86656,#65994,#65995);
#54563=AXIS2_PLACEMENT_3D('',#86658,#65997,#65998);
#54564=AXIS2_PLACEMENT_3D('',#86662,#66001,#66002);
#54565=AXIS2_PLACEMENT_3D('',#86663,#66003,#66004);
#54566=AXIS2_PLACEMENT_3D('',#86664,#66005,#66006);
#54567=AXIS2_PLACEMENT_3D('',#86673,#66011,#66012);
#54568=AXIS2_PLACEMENT_3D('',#86675,#66013,#66014);
#54569=AXIS2_PLACEMENT_3D('',#86677,#66016,#66017);
#54570=AXIS2_PLACEMENT_3D('',#86681,#66020,#66021);
#54571=AXIS2_PLACEMENT_3D('',#86682,#66022,#66023);
#54572=AXIS2_PLACEMENT_3D('',#86683,#66024,#66025);
#54573=AXIS2_PLACEMENT_3D('',#86692,#66030,#66031);
#54574=AXIS2_PLACEMENT_3D('',#86694,#66032,#66033);
#54575=AXIS2_PLACEMENT_3D('',#86696,#66035,#66036);
#54576=AXIS2_PLACEMENT_3D('',#86700,#66039,#66040);
#54577=AXIS2_PLACEMENT_3D('',#86701,#66041,#66042);
#54578=AXIS2_PLACEMENT_3D('',#86702,#66043,#66044);
#54579=AXIS2_PLACEMENT_3D('',#86711,#66049,#66050);
#54580=AXIS2_PLACEMENT_3D('',#86713,#66051,#66052);
#54581=AXIS2_PLACEMENT_3D('',#86715,#66054,#66055);
#54582=AXIS2_PLACEMENT_3D('',#86719,#66058,#66059);
#54583=AXIS2_PLACEMENT_3D('',#86720,#66060,#66061);
#54584=AXIS2_PLACEMENT_3D('',#86721,#66062,#66063);
#54585=AXIS2_PLACEMENT_3D('',#86730,#66068,#66069);
#54586=AXIS2_PLACEMENT_3D('',#86732,#66070,#66071);
#54587=AXIS2_PLACEMENT_3D('',#86734,#66073,#66074);
#54588=AXIS2_PLACEMENT_3D('',#86738,#66077,#66078);
#54589=AXIS2_PLACEMENT_3D('',#86739,#66079,#66080);
#54590=AXIS2_PLACEMENT_3D('',#86740,#66081,#66082);
#54591=AXIS2_PLACEMENT_3D('',#86749,#66087,#66088);
#54592=AXIS2_PLACEMENT_3D('',#86751,#66089,#66090);
#54593=AXIS2_PLACEMENT_3D('',#86753,#66092,#66093);
#54594=AXIS2_PLACEMENT_3D('',#86757,#66096,#66097);
#54595=AXIS2_PLACEMENT_3D('',#86758,#66098,#66099);
#54596=AXIS2_PLACEMENT_3D('',#86759,#66100,#66101);
#54597=AXIS2_PLACEMENT_3D('',#86768,#66106,#66107);
#54598=AXIS2_PLACEMENT_3D('',#86770,#66108,#66109);
#54599=AXIS2_PLACEMENT_3D('',#86772,#66111,#66112);
#54600=AXIS2_PLACEMENT_3D('',#86776,#66115,#66116);
#54601=AXIS2_PLACEMENT_3D('',#86777,#66117,#66118);
#54602=AXIS2_PLACEMENT_3D('',#86778,#66119,#66120);
#54603=AXIS2_PLACEMENT_3D('',#86787,#66125,#66126);
#54604=AXIS2_PLACEMENT_3D('',#86789,#66127,#66128);
#54605=AXIS2_PLACEMENT_3D('',#86791,#66130,#66131);
#54606=AXIS2_PLACEMENT_3D('',#86795,#66134,#66135);
#54607=AXIS2_PLACEMENT_3D('',#86796,#66136,#66137);
#54608=AXIS2_PLACEMENT_3D('',#86797,#66138,#66139);
#54609=AXIS2_PLACEMENT_3D('',#86806,#66144,#66145);
#54610=AXIS2_PLACEMENT_3D('',#86808,#66146,#66147);
#54611=AXIS2_PLACEMENT_3D('',#86810,#66149,#66150);
#54612=AXIS2_PLACEMENT_3D('',#86814,#66153,#66154);
#54613=AXIS2_PLACEMENT_3D('',#86815,#66155,#66156);
#54614=AXIS2_PLACEMENT_3D('',#86816,#66157,#66158);
#54615=AXIS2_PLACEMENT_3D('',#86825,#66163,#66164);
#54616=AXIS2_PLACEMENT_3D('',#86827,#66165,#66166);
#54617=AXIS2_PLACEMENT_3D('',#86829,#66168,#66169);
#54618=AXIS2_PLACEMENT_3D('',#86833,#66172,#66173);
#54619=AXIS2_PLACEMENT_3D('',#86834,#66174,#66175);
#54620=AXIS2_PLACEMENT_3D('',#86835,#66176,#66177);
#54621=AXIS2_PLACEMENT_3D('',#86844,#66182,#66183);
#54622=AXIS2_PLACEMENT_3D('',#86846,#66184,#66185);
#54623=AXIS2_PLACEMENT_3D('',#86848,#66187,#66188);
#54624=AXIS2_PLACEMENT_3D('',#86852,#66191,#66192);
#54625=AXIS2_PLACEMENT_3D('',#86853,#66193,#66194);
#54626=AXIS2_PLACEMENT_3D('',#86854,#66195,#66196);
#54627=AXIS2_PLACEMENT_3D('',#86863,#66201,#66202);
#54628=AXIS2_PLACEMENT_3D('',#86865,#66203,#66204);
#54629=AXIS2_PLACEMENT_3D('',#86867,#66206,#66207);
#54630=AXIS2_PLACEMENT_3D('',#86871,#66210,#66211);
#54631=AXIS2_PLACEMENT_3D('',#86872,#66212,#66213);
#54632=AXIS2_PLACEMENT_3D('',#86873,#66214,#66215);
#54633=AXIS2_PLACEMENT_3D('',#86882,#66220,#66221);
#54634=AXIS2_PLACEMENT_3D('',#86884,#66222,#66223);
#54635=AXIS2_PLACEMENT_3D('',#86886,#66225,#66226);
#54636=AXIS2_PLACEMENT_3D('',#86890,#66229,#66230);
#54637=AXIS2_PLACEMENT_3D('',#86891,#66231,#66232);
#54638=AXIS2_PLACEMENT_3D('',#86892,#66233,#66234);
#54639=AXIS2_PLACEMENT_3D('',#86901,#66239,#66240);
#54640=AXIS2_PLACEMENT_3D('',#86903,#66241,#66242);
#54641=AXIS2_PLACEMENT_3D('',#86905,#66244,#66245);
#54642=AXIS2_PLACEMENT_3D('',#86909,#66248,#66249);
#54643=AXIS2_PLACEMENT_3D('',#86910,#66250,#66251);
#54644=AXIS2_PLACEMENT_3D('',#86911,#66252,#66253);
#54645=AXIS2_PLACEMENT_3D('',#86920,#66258,#66259);
#54646=AXIS2_PLACEMENT_3D('',#86922,#66260,#66261);
#54647=AXIS2_PLACEMENT_3D('',#86925,#66263,#66264);
#54648=AXIS2_PLACEMENT_3D('',#86926,#66265,#66266);
#54649=AXIS2_PLACEMENT_3D('',#86930,#66269,#66270);
#54650=AXIS2_PLACEMENT_3D('',#86932,#66271,#66272);
#54651=AXIS2_PLACEMENT_3D('',#86933,#66273,#66274);
#54652=AXIS2_PLACEMENT_3D('',#86934,#66275,#66276);
#54653=AXIS2_PLACEMENT_3D('',#86943,#66281,#66282);
#54654=AXIS2_PLACEMENT_3D('',#86945,#66283,#66284);
#54655=AXIS2_PLACEMENT_3D('',#86947,#66286,#66287);
#54656=AXIS2_PLACEMENT_3D('',#86951,#66290,#66291);
#54657=AXIS2_PLACEMENT_3D('',#86952,#66292,#66293);
#54658=AXIS2_PLACEMENT_3D('',#86953,#66294,#66295);
#54659=AXIS2_PLACEMENT_3D('',#86962,#66300,#66301);
#54660=AXIS2_PLACEMENT_3D('',#86964,#66302,#66303);
#54661=AXIS2_PLACEMENT_3D('',#86966,#66305,#66306);
#54662=AXIS2_PLACEMENT_3D('',#86970,#66309,#66310);
#54663=AXIS2_PLACEMENT_3D('',#86971,#66311,#66312);
#54664=AXIS2_PLACEMENT_3D('',#86972,#66313,#66314);
#54665=AXIS2_PLACEMENT_3D('',#86981,#66319,#66320);
#54666=AXIS2_PLACEMENT_3D('',#86983,#66321,#66322);
#54667=AXIS2_PLACEMENT_3D('',#86985,#66324,#66325);
#54668=AXIS2_PLACEMENT_3D('',#86989,#66328,#66329);
#54669=AXIS2_PLACEMENT_3D('',#86990,#66330,#66331);
#54670=AXIS2_PLACEMENT_3D('',#86991,#66332,#66333);
#54671=AXIS2_PLACEMENT_3D('',#87000,#66338,#66339);
#54672=AXIS2_PLACEMENT_3D('',#87002,#66340,#66341);
#54673=AXIS2_PLACEMENT_3D('',#87004,#66343,#66344);
#54674=AXIS2_PLACEMENT_3D('',#87008,#66347,#66348);
#54675=AXIS2_PLACEMENT_3D('',#87009,#66349,#66350);
#54676=AXIS2_PLACEMENT_3D('',#87010,#66351,#66352);
#54677=AXIS2_PLACEMENT_3D('',#87019,#66357,#66358);
#54678=AXIS2_PLACEMENT_3D('',#87021,#66359,#66360);
#54679=AXIS2_PLACEMENT_3D('',#87023,#66362,#66363);
#54680=AXIS2_PLACEMENT_3D('',#87027,#66366,#66367);
#54681=AXIS2_PLACEMENT_3D('',#87028,#66368,#66369);
#54682=AXIS2_PLACEMENT_3D('',#87029,#66370,#66371);
#54683=AXIS2_PLACEMENT_3D('',#87038,#66376,#66377);
#54684=AXIS2_PLACEMENT_3D('',#87040,#66378,#66379);
#54685=AXIS2_PLACEMENT_3D('',#87042,#66381,#66382);
#54686=AXIS2_PLACEMENT_3D('',#87046,#66385,#66386);
#54687=AXIS2_PLACEMENT_3D('',#87047,#66387,#66388);
#54688=AXIS2_PLACEMENT_3D('',#87048,#66389,#66390);
#54689=AXIS2_PLACEMENT_3D('',#87057,#66395,#66396);
#54690=AXIS2_PLACEMENT_3D('',#87059,#66397,#66398);
#54691=AXIS2_PLACEMENT_3D('',#87061,#66400,#66401);
#54692=AXIS2_PLACEMENT_3D('',#87065,#66404,#66405);
#54693=AXIS2_PLACEMENT_3D('',#87066,#66406,#66407);
#54694=AXIS2_PLACEMENT_3D('',#87067,#66408,#66409);
#54695=AXIS2_PLACEMENT_3D('',#87076,#66414,#66415);
#54696=AXIS2_PLACEMENT_3D('',#87078,#66416,#66417);
#54697=AXIS2_PLACEMENT_3D('',#87080,#66419,#66420);
#54698=AXIS2_PLACEMENT_3D('',#87084,#66423,#66424);
#54699=AXIS2_PLACEMENT_3D('',#87085,#66425,#66426);
#54700=AXIS2_PLACEMENT_3D('',#87086,#66427,#66428);
#54701=AXIS2_PLACEMENT_3D('',#87095,#66433,#66434);
#54702=AXIS2_PLACEMENT_3D('',#87097,#66435,#66436);
#54703=AXIS2_PLACEMENT_3D('',#87099,#66438,#66439);
#54704=AXIS2_PLACEMENT_3D('',#87103,#66442,#66443);
#54705=AXIS2_PLACEMENT_3D('',#87104,#66444,#66445);
#54706=AXIS2_PLACEMENT_3D('',#87105,#66446,#66447);
#54707=AXIS2_PLACEMENT_3D('',#87114,#66452,#66453);
#54708=AXIS2_PLACEMENT_3D('',#87116,#66454,#66455);
#54709=AXIS2_PLACEMENT_3D('',#87118,#66457,#66458);
#54710=AXIS2_PLACEMENT_3D('',#87122,#66461,#66462);
#54711=AXIS2_PLACEMENT_3D('',#87123,#66463,#66464);
#54712=AXIS2_PLACEMENT_3D('',#87124,#66465,#66466);
#54713=AXIS2_PLACEMENT_3D('',#87133,#66471,#66472);
#54714=AXIS2_PLACEMENT_3D('',#87135,#66473,#66474);
#54715=AXIS2_PLACEMENT_3D('',#87137,#66476,#66477);
#54716=AXIS2_PLACEMENT_3D('',#87141,#66480,#66481);
#54717=AXIS2_PLACEMENT_3D('',#87142,#66482,#66483);
#54718=AXIS2_PLACEMENT_3D('',#87143,#66484,#66485);
#54719=AXIS2_PLACEMENT_3D('',#87152,#66490,#66491);
#54720=AXIS2_PLACEMENT_3D('',#87154,#66492,#66493);
#54721=AXIS2_PLACEMENT_3D('',#87156,#66495,#66496);
#54722=AXIS2_PLACEMENT_3D('',#87160,#66499,#66500);
#54723=AXIS2_PLACEMENT_3D('',#87161,#66501,#66502);
#54724=AXIS2_PLACEMENT_3D('',#87162,#66503,#66504);
#54725=AXIS2_PLACEMENT_3D('',#87171,#66509,#66510);
#54726=AXIS2_PLACEMENT_3D('',#87173,#66511,#66512);
#54727=AXIS2_PLACEMENT_3D('',#87175,#66514,#66515);
#54728=AXIS2_PLACEMENT_3D('',#87179,#66518,#66519);
#54729=AXIS2_PLACEMENT_3D('',#87180,#66520,#66521);
#54730=AXIS2_PLACEMENT_3D('',#87181,#66522,#66523);
#54731=AXIS2_PLACEMENT_3D('',#87190,#66528,#66529);
#54732=AXIS2_PLACEMENT_3D('',#87192,#66530,#66531);
#54733=AXIS2_PLACEMENT_3D('',#87194,#66533,#66534);
#54734=AXIS2_PLACEMENT_3D('',#87198,#66537,#66538);
#54735=AXIS2_PLACEMENT_3D('',#87199,#66539,#66540);
#54736=AXIS2_PLACEMENT_3D('',#87200,#66541,#66542);
#54737=AXIS2_PLACEMENT_3D('',#87209,#66547,#66548);
#54738=AXIS2_PLACEMENT_3D('',#87211,#66549,#66550);
#54739=AXIS2_PLACEMENT_3D('',#87213,#66552,#66553);
#54740=AXIS2_PLACEMENT_3D('',#87217,#66556,#66557);
#54741=AXIS2_PLACEMENT_3D('',#87218,#66558,#66559);
#54742=AXIS2_PLACEMENT_3D('',#87219,#66560,#66561);
#54743=AXIS2_PLACEMENT_3D('',#87228,#66566,#66567);
#54744=AXIS2_PLACEMENT_3D('',#87230,#66568,#66569);
#54745=AXIS2_PLACEMENT_3D('',#87232,#66571,#66572);
#54746=AXIS2_PLACEMENT_3D('',#87236,#66575,#66576);
#54747=AXIS2_PLACEMENT_3D('',#87237,#66577,#66578);
#54748=AXIS2_PLACEMENT_3D('',#87238,#66579,#66580);
#54749=AXIS2_PLACEMENT_3D('',#87247,#66585,#66586);
#54750=AXIS2_PLACEMENT_3D('',#87249,#66587,#66588);
#54751=AXIS2_PLACEMENT_3D('',#87251,#66590,#66591);
#54752=AXIS2_PLACEMENT_3D('',#87255,#66594,#66595);
#54753=AXIS2_PLACEMENT_3D('',#87256,#66596,#66597);
#54754=AXIS2_PLACEMENT_3D('',#87257,#66598,#66599);
#54755=AXIS2_PLACEMENT_3D('',#87260,#66600,#66601);
#54756=AXIS2_PLACEMENT_3D('',#87264,#66604,#66605);
#54757=AXIS2_PLACEMENT_3D('',#87270,#66609,#66610);
#54758=AXIS2_PLACEMENT_3D('',#87274,#66613,#66614);
#54759=AXIS2_PLACEMENT_3D('',#87275,#66615,#66616);
#54760=AXIS2_PLACEMENT_3D('',#87276,#66617,#66618);
#54761=AXIS2_PLACEMENT_3D('',#87280,#66620,#66621);
#54762=AXIS2_PLACEMENT_3D('',#87281,#66622,#66623);
#54763=AXIS2_PLACEMENT_3D('',#87290,#66628,#66629);
#54764=AXIS2_PLACEMENT_3D('',#87296,#66633,#66634);
#54765=AXIS2_PLACEMENT_3D('',#87302,#66638,#66639);
#54766=AXIS2_PLACEMENT_3D('',#87308,#66643,#66644);
#54767=AXIS2_PLACEMENT_3D('',#87314,#66648,#66649);
#54768=AXIS2_PLACEMENT_3D('',#87317,#66652,#66653);
#54769=AXIS2_PLACEMENT_3D('',#87318,#66654,#66655);
#54770=AXIS2_PLACEMENT_3D('',#87320,#66656,#66657);
#54771=AXIS2_PLACEMENT_3D('',#87321,#66658,#66659);
#54772=AXIS2_PLACEMENT_3D('',#87323,#66661,#66662);
#54773=AXIS2_PLACEMENT_3D('',#87324,#66663,#66664);
#54774=AXIS2_PLACEMENT_3D('',#87325,#66665,#66666);
#54775=AXIS2_PLACEMENT_3D('',#87326,#66667,#66668);
#54776=AXIS2_PLACEMENT_3D('',#87327,#66669,#66670);
#54777=AXIS2_PLACEMENT_3D('',#87328,#66671,#66672);
#54778=AXIS2_PLACEMENT_3D('',#87329,#66673,#66674);
#54779=AXIS2_PLACEMENT_3D('',#87330,#66675,#66676);
#54780=AXIS2_PLACEMENT_3D('',#87331,#66677,#66678);
#54781=AXIS2_PLACEMENT_3D('',#87332,#66679,#66680);
#54782=AXIS2_PLACEMENT_3D('',#87333,#66681,#66682);
#54783=AXIS2_PLACEMENT_3D('',#87334,#66683,#66684);
#54784=AXIS2_PLACEMENT_3D('',#87335,#66685,#66686);
#54785=AXIS2_PLACEMENT_3D('',#87336,#66687,#66688);
#54786=AXIS2_PLACEMENT_3D('',#87337,#66689,#66690);
#54787=AXIS2_PLACEMENT_3D('',#87338,#66691,#66692);
#54788=AXIS2_PLACEMENT_3D('',#87339,#66693,#66694);
#54789=AXIS2_PLACEMENT_3D('',#87340,#66695,#66696);
#54790=AXIS2_PLACEMENT_3D('',#87342,#66698,#66699);
#54791=AXIS2_PLACEMENT_3D('',#87343,#66700,#66701);
#54792=AXIS2_PLACEMENT_3D('',#87344,#66702,#66703);
#54793=AXIS2_PLACEMENT_3D('',#87345,#66704,#66705);
#54794=AXIS2_PLACEMENT_3D('',#87346,#66706,#66707);
#54795=AXIS2_PLACEMENT_3D('',#87347,#66708,#66709);
#54796=AXIS2_PLACEMENT_3D('',#87348,#66710,#66711);
#54797=AXIS2_PLACEMENT_3D('',#87349,#66712,#66713);
#54798=AXIS2_PLACEMENT_3D('',#87350,#66714,#66715);
#54799=AXIS2_PLACEMENT_3D('',#87351,#66716,#66717);
#54800=AXIS2_PLACEMENT_3D('',#87352,#66718,#66719);
#54801=AXIS2_PLACEMENT_3D('',#87353,#66720,#66721);
#54802=AXIS2_PLACEMENT_3D('',#87354,#66722,#66723);
#54803=AXIS2_PLACEMENT_3D('',#87355,#66724,#66725);
#54804=AXIS2_PLACEMENT_3D('',#87356,#66726,#66727);
#54805=AXIS2_PLACEMENT_3D('',#87357,#66728,#66729);
#54806=AXIS2_PLACEMENT_3D('',#87358,#66730,#66731);
#54807=AXIS2_PLACEMENT_3D('',#87359,#66732,#66733);
#54808=AXIS2_PLACEMENT_3D('',#87360,#66734,#66735);
#54809=AXIS2_PLACEMENT_3D('',#87361,#66736,#66737);
#54810=AXIS2_PLACEMENT_3D('',#87363,#66738,#66739);
#54811=AXIS2_PLACEMENT_3D('',#87365,#66741,#66742);
#54812=AXIS2_PLACEMENT_3D('',#87366,#66743,#66744);
#54813=AXIS2_PLACEMENT_3D('',#87367,#66745,#66746);
#54814=AXIS2_PLACEMENT_3D('',#87369,#66747,#66748);
#54815=AXIS2_PLACEMENT_3D('',#87372,#66750,#66751);
#54816=AXIS2_PLACEMENT_3D('',#87373,#66752,#66753);
#54817=AXIS2_PLACEMENT_3D('',#87375,#66754,#66755);
#54818=AXIS2_PLACEMENT_3D('',#87377,#66757,#66758);
#54819=AXIS2_PLACEMENT_3D('',#87379,#66759,#66760);
#54820=AXIS2_PLACEMENT_3D('',#87381,#66762,#66763);
#54821=AXIS2_PLACEMENT_3D('',#87383,#66764,#66765);
#54822=AXIS2_PLACEMENT_3D('',#87384,#66766,#66767);
#54823=AXIS2_PLACEMENT_3D('',#87387,#66769,#66770);
#54824=AXIS2_PLACEMENT_3D('',#87388,#66771,#66772);
#54825=AXIS2_PLACEMENT_3D('',#87391,#66774,#66775);
#54826=AXIS2_PLACEMENT_3D('',#87392,#66776,#66777);
#54827=AXIS2_PLACEMENT_3D('',#87395,#66779,#66780);
#54828=AXIS2_PLACEMENT_3D('',#87396,#66781,#66782);
#54829=AXIS2_PLACEMENT_3D('',#87397,#66783,#66784);
#54830=AXIS2_PLACEMENT_3D('',#87398,#66785,#66786);
#54831=AXIS2_PLACEMENT_3D('',#87403,#66788,#66789);
#54832=AXIS2_PLACEMENT_3D('',#87405,#66790,#66791);
#54833=AXIS2_PLACEMENT_3D('',#87406,#66792,#66793);
#54834=AXIS2_PLACEMENT_3D('',#87407,#66794,#66795);
#54835=AXIS2_PLACEMENT_3D('',#87412,#66797,#66798);
#54836=AXIS2_PLACEMENT_3D('',#87414,#66799,#66800);
#54837=AXIS2_PLACEMENT_3D('',#87415,#66801,#66802);
#54838=AXIS2_PLACEMENT_3D('',#87416,#66803,#66804);
#54839=AXIS2_PLACEMENT_3D('',#87428,#66806,#66807);
#54840=AXIS2_PLACEMENT_3D('',#87438,#66809,#66810);
#54841=AXIS2_PLACEMENT_3D('',#87445,#66811,#66812);
#54842=AXIS2_PLACEMENT_3D('',#87460,#66815,#66816);
#54843=AXIS2_PLACEMENT_3D('',#87461,#66817,#66818);
#54844=AXIS2_PLACEMENT_3D('',#87462,#66819,#66820);
#54845=AXIS2_PLACEMENT_3D('',#87463,#66821,#66822);
#54846=AXIS2_PLACEMENT_3D('',#87464,#66823,#66824);
#54847=AXIS2_PLACEMENT_3D('',#87465,#66825,#66826);
#54848=AXIS2_PLACEMENT_3D('',#87466,#66827,#66828);
#54849=AXIS2_PLACEMENT_3D('',#87467,#66829,#66830);
#54850=AXIS2_PLACEMENT_3D('',#87468,#66831,#66832);
#54851=AXIS2_PLACEMENT_3D('',#87469,#66833,#66834);
#54852=AXIS2_PLACEMENT_3D('',#87470,#66835,#66836);
#54853=AXIS2_PLACEMENT_3D('',#87471,#66837,#66838);
#54854=AXIS2_PLACEMENT_3D('',#87472,#66839,#66840);
#54855=AXIS2_PLACEMENT_3D('',#87473,#66841,#66842);
#54856=AXIS2_PLACEMENT_3D('',#87474,#66843,#66844);
#54857=AXIS2_PLACEMENT_3D('',#87475,#66845,#66846);
#54858=AXIS2_PLACEMENT_3D('',#87476,#66847,#66848);
#54859=AXIS2_PLACEMENT_3D('',#87477,#66849,#66850);
#54860=AXIS2_PLACEMENT_3D('',#87493,#66852,#66853);
#54861=AXIS2_PLACEMENT_3D('',#87501,#66854,#66855);
#54862=AXIS2_PLACEMENT_3D('',#87549,#66857,#66858);
#54863=AXIS2_PLACEMENT_3D('',#87597,#66860,#66861);
#54864=AXIS2_PLACEMENT_3D('',#87651,#66863,#66864);
#54865=AXIS2_PLACEMENT_3D('',#87699,#66866,#66867);
#54866=AXIS2_PLACEMENT_3D('',#87747,#66869,#66870);
#54867=AXIS2_PLACEMENT_3D('',#87795,#66872,#66873);
#54868=AXIS2_PLACEMENT_3D('',#87849,#66875,#66876);
#54869=AXIS2_PLACEMENT_3D('',#87897,#66878,#66879);
#54870=AXIS2_PLACEMENT_3D('',#87945,#66881,#66882);
#54871=AXIS2_PLACEMENT_3D('',#87999,#66884,#66885);
#54872=AXIS2_PLACEMENT_3D('',#88047,#66887,#66888);
#54873=AXIS2_PLACEMENT_3D('',#88095,#66890,#66891);
#54874=AXIS2_PLACEMENT_3D('',#88149,#66893,#66894);
#54875=AXIS2_PLACEMENT_3D('',#88197,#66896,#66897);
#54876=AXIS2_PLACEMENT_3D('',#88202,#66899,#66900);
#54877=AXIS2_PLACEMENT_3D('',#88244,#66901,#66902);
#54878=AXIS2_PLACEMENT_3D('',#88257,#66904,#66905);
#54879=AXIS2_PLACEMENT_3D('',#88264,#66906,#66907);
#54880=AXIS2_PLACEMENT_3D('',#88288,#66909,#66910);
#54881=AXIS2_PLACEMENT_3D('',#88313,#66912,#66913);
#54882=AXIS2_PLACEMENT_3D('',#88338,#66915,#66916);
#54883=AXIS2_PLACEMENT_3D('',#88362,#66918,#66919);
#54884=AXIS2_PLACEMENT_3D('',#88387,#66921,#66922);
#54885=AXIS2_PLACEMENT_3D('',#88412,#66924,#66925);
#54886=AXIS2_PLACEMENT_3D('',#88436,#66927,#66928);
#54887=AXIS2_PLACEMENT_3D('',#88461,#66930,#66931);
#54888=AXIS2_PLACEMENT_3D('',#88486,#66933,#66934);
#54889=AXIS2_PLACEMENT_3D('',#88510,#66936,#66937);
#54890=AXIS2_PLACEMENT_3D('',#88534,#66939,#66940);
#54891=AXIS2_PLACEMENT_3D('',#88559,#66942,#66943);
#54892=AXIS2_PLACEMENT_3D('',#88584,#66945,#66946);
#54893=AXIS2_PLACEMENT_3D('',#88608,#66948,#66949);
#54894=AXIS2_PLACEMENT_3D('',#88701,#66950,#66951);
#54895=AXIS2_PLACEMENT_3D('',#88703,#66952,#66953);
#54896=AXIS2_PLACEMENT_3D('',#89307,#66954,#66955);
#54897=AXIS2_PLACEMENT_3D('',#89309,#66956,#66957);
#54898=AXIS2_PLACEMENT_3D('',#89310,#66958,#66959);
#54899=AXIS2_PLACEMENT_3D('',#89406,#66960,#66961);
#54900=AXIS2_PLACEMENT_3D('',#89407,#66962,#66963);
#54901=AXIS2_PLACEMENT_3D('',#89820,#66964,#66965);
#54902=AXIS2_PLACEMENT_3D('',#89821,#66966,#66967);
#54903=AXIS2_PLACEMENT_3D('',#89823,#66968,#66969);
#54904=AXIS2_PLACEMENT_3D('',#89824,#66970,#66971);
#54905=AXIS2_PLACEMENT_3D('',#89825,#66972,#66973);
#54906=AXIS2_PLACEMENT_3D('',#89826,#66974,#66975);
#54907=AXIS2_PLACEMENT_3D('',#89828,#66976,#66977);
#54908=AXIS2_PLACEMENT_3D('',#89829,#66978,#66979);
#54909=AXIS2_PLACEMENT_3D('',#89838,#66984,#66985);
#54910=AXIS2_PLACEMENT_3D('',#89840,#66986,#66987);
#54911=AXIS2_PLACEMENT_3D('',#89842,#66989,#66990);
#54912=AXIS2_PLACEMENT_3D('',#89846,#66993,#66994);
#54913=AXIS2_PLACEMENT_3D('',#89847,#66995,#66996);
#54914=AXIS2_PLACEMENT_3D('',#89848,#66997,#66998);
#54915=AXIS2_PLACEMENT_3D('',#89857,#67003,#67004);
#54916=AXIS2_PLACEMENT_3D('',#89859,#67005,#67006);
#54917=AXIS2_PLACEMENT_3D('',#89861,#67008,#67009);
#54918=AXIS2_PLACEMENT_3D('',#89865,#67012,#67013);
#54919=AXIS2_PLACEMENT_3D('',#89866,#67014,#67015);
#54920=AXIS2_PLACEMENT_3D('',#89867,#67016,#67017);
#54921=AXIS2_PLACEMENT_3D('',#89876,#67022,#67023);
#54922=AXIS2_PLACEMENT_3D('',#89878,#67024,#67025);
#54923=AXIS2_PLACEMENT_3D('',#89880,#67027,#67028);
#54924=AXIS2_PLACEMENT_3D('',#89884,#67031,#67032);
#54925=AXIS2_PLACEMENT_3D('',#89885,#67033,#67034);
#54926=AXIS2_PLACEMENT_3D('',#89886,#67035,#67036);
#54927=AXIS2_PLACEMENT_3D('',#89895,#67041,#67042);
#54928=AXIS2_PLACEMENT_3D('',#89897,#67043,#67044);
#54929=AXIS2_PLACEMENT_3D('',#89899,#67046,#67047);
#54930=AXIS2_PLACEMENT_3D('',#89903,#67050,#67051);
#54931=AXIS2_PLACEMENT_3D('',#89904,#67052,#67053);
#54932=AXIS2_PLACEMENT_3D('',#89905,#67054,#67055);
#54933=AXIS2_PLACEMENT_3D('',#89914,#67060,#67061);
#54934=AXIS2_PLACEMENT_3D('',#89916,#67062,#67063);
#54935=AXIS2_PLACEMENT_3D('',#89918,#67065,#67066);
#54936=AXIS2_PLACEMENT_3D('',#89922,#67069,#67070);
#54937=AXIS2_PLACEMENT_3D('',#89923,#67071,#67072);
#54938=AXIS2_PLACEMENT_3D('',#89924,#67073,#67074);
#54939=AXIS2_PLACEMENT_3D('',#89933,#67079,#67080);
#54940=AXIS2_PLACEMENT_3D('',#89935,#67081,#67082);
#54941=AXIS2_PLACEMENT_3D('',#89937,#67084,#67085);
#54942=AXIS2_PLACEMENT_3D('',#89941,#67088,#67089);
#54943=AXIS2_PLACEMENT_3D('',#89942,#67090,#67091);
#54944=AXIS2_PLACEMENT_3D('',#89943,#67092,#67093);
#54945=AXIS2_PLACEMENT_3D('',#89952,#67098,#67099);
#54946=AXIS2_PLACEMENT_3D('',#89954,#67100,#67101);
#54947=AXIS2_PLACEMENT_3D('',#89956,#67103,#67104);
#54948=AXIS2_PLACEMENT_3D('',#89960,#67107,#67108);
#54949=AXIS2_PLACEMENT_3D('',#89961,#67109,#67110);
#54950=AXIS2_PLACEMENT_3D('',#89962,#67111,#67112);
#54951=AXIS2_PLACEMENT_3D('',#89971,#67117,#67118);
#54952=AXIS2_PLACEMENT_3D('',#89973,#67119,#67120);
#54953=AXIS2_PLACEMENT_3D('',#89975,#67122,#67123);
#54954=AXIS2_PLACEMENT_3D('',#89979,#67126,#67127);
#54955=AXIS2_PLACEMENT_3D('',#89980,#67128,#67129);
#54956=AXIS2_PLACEMENT_3D('',#89981,#67130,#67131);
#54957=AXIS2_PLACEMENT_3D('',#89990,#67136,#67137);
#54958=AXIS2_PLACEMENT_3D('',#89992,#67138,#67139);
#54959=AXIS2_PLACEMENT_3D('',#89994,#67141,#67142);
#54960=AXIS2_PLACEMENT_3D('',#89998,#67145,#67146);
#54961=AXIS2_PLACEMENT_3D('',#89999,#67147,#67148);
#54962=AXIS2_PLACEMENT_3D('',#90000,#67149,#67150);
#54963=AXIS2_PLACEMENT_3D('',#90009,#67155,#67156);
#54964=AXIS2_PLACEMENT_3D('',#90011,#67157,#67158);
#54965=AXIS2_PLACEMENT_3D('',#90013,#67160,#67161);
#54966=AXIS2_PLACEMENT_3D('',#90017,#67164,#67165);
#54967=AXIS2_PLACEMENT_3D('',#90018,#67166,#67167);
#54968=AXIS2_PLACEMENT_3D('',#90019,#67168,#67169);
#54969=AXIS2_PLACEMENT_3D('',#90028,#67174,#67175);
#54970=AXIS2_PLACEMENT_3D('',#90030,#67176,#67177);
#54971=AXIS2_PLACEMENT_3D('',#90032,#67179,#67180);
#54972=AXIS2_PLACEMENT_3D('',#90036,#67183,#67184);
#54973=AXIS2_PLACEMENT_3D('',#90037,#67185,#67186);
#54974=AXIS2_PLACEMENT_3D('',#90038,#67187,#67188);
#54975=AXIS2_PLACEMENT_3D('',#90047,#67193,#67194);
#54976=AXIS2_PLACEMENT_3D('',#90049,#67195,#67196);
#54977=AXIS2_PLACEMENT_3D('',#90051,#67198,#67199);
#54978=AXIS2_PLACEMENT_3D('',#90055,#67202,#67203);
#54979=AXIS2_PLACEMENT_3D('',#90056,#67204,#67205);
#54980=AXIS2_PLACEMENT_3D('',#90057,#67206,#67207);
#54981=AXIS2_PLACEMENT_3D('',#90066,#67212,#67213);
#54982=AXIS2_PLACEMENT_3D('',#90068,#67214,#67215);
#54983=AXIS2_PLACEMENT_3D('',#90070,#67217,#67218);
#54984=AXIS2_PLACEMENT_3D('',#90074,#67221,#67222);
#54985=AXIS2_PLACEMENT_3D('',#90075,#67223,#67224);
#54986=AXIS2_PLACEMENT_3D('',#90076,#67225,#67226);
#54987=AXIS2_PLACEMENT_3D('',#90085,#67231,#67232);
#54988=AXIS2_PLACEMENT_3D('',#90087,#67233,#67234);
#54989=AXIS2_PLACEMENT_3D('',#90089,#67236,#67237);
#54990=AXIS2_PLACEMENT_3D('',#90093,#67240,#67241);
#54991=AXIS2_PLACEMENT_3D('',#90094,#67242,#67243);
#54992=AXIS2_PLACEMENT_3D('',#90095,#67244,#67245);
#54993=AXIS2_PLACEMENT_3D('',#90104,#67250,#67251);
#54994=AXIS2_PLACEMENT_3D('',#90106,#67252,#67253);
#54995=AXIS2_PLACEMENT_3D('',#90108,#67255,#67256);
#54996=AXIS2_PLACEMENT_3D('',#90112,#67259,#67260);
#54997=AXIS2_PLACEMENT_3D('',#90113,#67261,#67262);
#54998=AXIS2_PLACEMENT_3D('',#90114,#67263,#67264);
#54999=AXIS2_PLACEMENT_3D('',#90123,#67269,#67270);
#55000=AXIS2_PLACEMENT_3D('',#90125,#67271,#67272);
#55001=AXIS2_PLACEMENT_3D('',#90127,#67274,#67275);
#55002=AXIS2_PLACEMENT_3D('',#90131,#67278,#67279);
#55003=AXIS2_PLACEMENT_3D('',#90132,#67280,#67281);
#55004=AXIS2_PLACEMENT_3D('',#90133,#67282,#67283);
#55005=AXIS2_PLACEMENT_3D('',#90142,#67288,#67289);
#55006=AXIS2_PLACEMENT_3D('',#90144,#67290,#67291);
#55007=AXIS2_PLACEMENT_3D('',#90146,#67293,#67294);
#55008=AXIS2_PLACEMENT_3D('',#90150,#67297,#67298);
#55009=AXIS2_PLACEMENT_3D('',#90151,#67299,#67300);
#55010=AXIS2_PLACEMENT_3D('',#90152,#67301,#67302);
#55011=AXIS2_PLACEMENT_3D('',#90161,#67307,#67308);
#55012=AXIS2_PLACEMENT_3D('',#90163,#67309,#67310);
#55013=AXIS2_PLACEMENT_3D('',#90166,#67312,#67313);
#55014=AXIS2_PLACEMENT_3D('',#90167,#67314,#67315);
#55015=AXIS2_PLACEMENT_3D('',#90171,#67318,#67319);
#55016=AXIS2_PLACEMENT_3D('',#90173,#67320,#67321);
#55017=AXIS2_PLACEMENT_3D('',#90174,#67322,#67323);
#55018=AXIS2_PLACEMENT_3D('',#90175,#67324,#67325);
#55019=AXIS2_PLACEMENT_3D('',#90184,#67330,#67331);
#55020=AXIS2_PLACEMENT_3D('',#90186,#67332,#67333);
#55021=AXIS2_PLACEMENT_3D('',#90188,#67335,#67336);
#55022=AXIS2_PLACEMENT_3D('',#90192,#67339,#67340);
#55023=AXIS2_PLACEMENT_3D('',#90193,#67341,#67342);
#55024=AXIS2_PLACEMENT_3D('',#90194,#67343,#67344);
#55025=AXIS2_PLACEMENT_3D('',#90203,#67349,#67350);
#55026=AXIS2_PLACEMENT_3D('',#90205,#67351,#67352);
#55027=AXIS2_PLACEMENT_3D('',#90207,#67354,#67355);
#55028=AXIS2_PLACEMENT_3D('',#90211,#67358,#67359);
#55029=AXIS2_PLACEMENT_3D('',#90212,#67360,#67361);
#55030=AXIS2_PLACEMENT_3D('',#90213,#67362,#67363);
#55031=AXIS2_PLACEMENT_3D('',#90222,#67368,#67369);
#55032=AXIS2_PLACEMENT_3D('',#90224,#67370,#67371);
#55033=AXIS2_PLACEMENT_3D('',#90226,#67373,#67374);
#55034=AXIS2_PLACEMENT_3D('',#90230,#67377,#67378);
#55035=AXIS2_PLACEMENT_3D('',#90231,#67379,#67380);
#55036=AXIS2_PLACEMENT_3D('',#90232,#67381,#67382);
#55037=AXIS2_PLACEMENT_3D('',#90241,#67387,#67388);
#55038=AXIS2_PLACEMENT_3D('',#90243,#67389,#67390);
#55039=AXIS2_PLACEMENT_3D('',#90245,#67392,#67393);
#55040=AXIS2_PLACEMENT_3D('',#90249,#67396,#67397);
#55041=AXIS2_PLACEMENT_3D('',#90250,#67398,#67399);
#55042=AXIS2_PLACEMENT_3D('',#90251,#67400,#67401);
#55043=AXIS2_PLACEMENT_3D('',#90260,#67406,#67407);
#55044=AXIS2_PLACEMENT_3D('',#90262,#67408,#67409);
#55045=AXIS2_PLACEMENT_3D('',#90264,#67411,#67412);
#55046=AXIS2_PLACEMENT_3D('',#90268,#67415,#67416);
#55047=AXIS2_PLACEMENT_3D('',#90269,#67417,#67418);
#55048=AXIS2_PLACEMENT_3D('',#90270,#67419,#67420);
#55049=AXIS2_PLACEMENT_3D('',#90279,#67425,#67426);
#55050=AXIS2_PLACEMENT_3D('',#90281,#67427,#67428);
#55051=AXIS2_PLACEMENT_3D('',#90283,#67430,#67431);
#55052=AXIS2_PLACEMENT_3D('',#90287,#67434,#67435);
#55053=AXIS2_PLACEMENT_3D('',#90288,#67436,#67437);
#55054=AXIS2_PLACEMENT_3D('',#90289,#67438,#67439);
#55055=AXIS2_PLACEMENT_3D('',#90298,#67444,#67445);
#55056=AXIS2_PLACEMENT_3D('',#90300,#67446,#67447);
#55057=AXIS2_PLACEMENT_3D('',#90302,#67449,#67450);
#55058=AXIS2_PLACEMENT_3D('',#90306,#67453,#67454);
#55059=AXIS2_PLACEMENT_3D('',#90307,#67455,#67456);
#55060=AXIS2_PLACEMENT_3D('',#90308,#67457,#67458);
#55061=AXIS2_PLACEMENT_3D('',#90317,#67463,#67464);
#55062=AXIS2_PLACEMENT_3D('',#90319,#67465,#67466);
#55063=AXIS2_PLACEMENT_3D('',#90321,#67468,#67469);
#55064=AXIS2_PLACEMENT_3D('',#90325,#67472,#67473);
#55065=AXIS2_PLACEMENT_3D('',#90326,#67474,#67475);
#55066=AXIS2_PLACEMENT_3D('',#90327,#67476,#67477);
#55067=AXIS2_PLACEMENT_3D('',#90336,#67482,#67483);
#55068=AXIS2_PLACEMENT_3D('',#90338,#67484,#67485);
#55069=AXIS2_PLACEMENT_3D('',#90340,#67487,#67488);
#55070=AXIS2_PLACEMENT_3D('',#90344,#67491,#67492);
#55071=AXIS2_PLACEMENT_3D('',#90345,#67493,#67494);
#55072=AXIS2_PLACEMENT_3D('',#90346,#67495,#67496);
#55073=AXIS2_PLACEMENT_3D('',#90355,#67501,#67502);
#55074=AXIS2_PLACEMENT_3D('',#90357,#67503,#67504);
#55075=AXIS2_PLACEMENT_3D('',#90359,#67506,#67507);
#55076=AXIS2_PLACEMENT_3D('',#90363,#67510,#67511);
#55077=AXIS2_PLACEMENT_3D('',#90364,#67512,#67513);
#55078=AXIS2_PLACEMENT_3D('',#90365,#67514,#67515);
#55079=AXIS2_PLACEMENT_3D('',#90374,#67520,#67521);
#55080=AXIS2_PLACEMENT_3D('',#90376,#67522,#67523);
#55081=AXIS2_PLACEMENT_3D('',#90378,#67525,#67526);
#55082=AXIS2_PLACEMENT_3D('',#90382,#67529,#67530);
#55083=AXIS2_PLACEMENT_3D('',#90383,#67531,#67532);
#55084=AXIS2_PLACEMENT_3D('',#90384,#67533,#67534);
#55085=AXIS2_PLACEMENT_3D('',#90393,#67539,#67540);
#55086=AXIS2_PLACEMENT_3D('',#90395,#67541,#67542);
#55087=AXIS2_PLACEMENT_3D('',#90397,#67544,#67545);
#55088=AXIS2_PLACEMENT_3D('',#90401,#67548,#67549);
#55089=AXIS2_PLACEMENT_3D('',#90402,#67550,#67551);
#55090=AXIS2_PLACEMENT_3D('',#90403,#67552,#67553);
#55091=AXIS2_PLACEMENT_3D('',#90412,#67558,#67559);
#55092=AXIS2_PLACEMENT_3D('',#90414,#67560,#67561);
#55093=AXIS2_PLACEMENT_3D('',#90416,#67563,#67564);
#55094=AXIS2_PLACEMENT_3D('',#90420,#67567,#67568);
#55095=AXIS2_PLACEMENT_3D('',#90421,#67569,#67570);
#55096=AXIS2_PLACEMENT_3D('',#90422,#67571,#67572);
#55097=AXIS2_PLACEMENT_3D('',#90431,#67577,#67578);
#55098=AXIS2_PLACEMENT_3D('',#90433,#67579,#67580);
#55099=AXIS2_PLACEMENT_3D('',#90435,#67582,#67583);
#55100=AXIS2_PLACEMENT_3D('',#90439,#67586,#67587);
#55101=AXIS2_PLACEMENT_3D('',#90440,#67588,#67589);
#55102=AXIS2_PLACEMENT_3D('',#90441,#67590,#67591);
#55103=AXIS2_PLACEMENT_3D('',#90450,#67596,#67597);
#55104=AXIS2_PLACEMENT_3D('',#90452,#67598,#67599);
#55105=AXIS2_PLACEMENT_3D('',#90454,#67601,#67602);
#55106=AXIS2_PLACEMENT_3D('',#90458,#67605,#67606);
#55107=AXIS2_PLACEMENT_3D('',#90459,#67607,#67608);
#55108=AXIS2_PLACEMENT_3D('',#90460,#67609,#67610);
#55109=AXIS2_PLACEMENT_3D('',#90469,#67615,#67616);
#55110=AXIS2_PLACEMENT_3D('',#90471,#67617,#67618);
#55111=AXIS2_PLACEMENT_3D('',#90473,#67620,#67621);
#55112=AXIS2_PLACEMENT_3D('',#90477,#67624,#67625);
#55113=AXIS2_PLACEMENT_3D('',#90478,#67626,#67627);
#55114=AXIS2_PLACEMENT_3D('',#90479,#67628,#67629);
#55115=AXIS2_PLACEMENT_3D('',#90488,#67634,#67635);
#55116=AXIS2_PLACEMENT_3D('',#90490,#67636,#67637);
#55117=AXIS2_PLACEMENT_3D('',#90492,#67639,#67640);
#55118=AXIS2_PLACEMENT_3D('',#90496,#67643,#67644);
#55119=AXIS2_PLACEMENT_3D('',#90497,#67645,#67646);
#55120=AXIS2_PLACEMENT_3D('',#90498,#67647,#67648);
#55121=AXIS2_PLACEMENT_3D('',#90501,#67649,#67650);
#55122=AXIS2_PLACEMENT_3D('',#90505,#67653,#67654);
#55123=AXIS2_PLACEMENT_3D('',#90511,#67658,#67659);
#55124=AXIS2_PLACEMENT_3D('',#90515,#67662,#67663);
#55125=AXIS2_PLACEMENT_3D('',#90516,#67664,#67665);
#55126=AXIS2_PLACEMENT_3D('',#90517,#67666,#67667);
#55127=AXIS2_PLACEMENT_3D('',#90521,#67669,#67670);
#55128=AXIS2_PLACEMENT_3D('',#90522,#67671,#67672);
#55129=AXIS2_PLACEMENT_3D('',#90531,#67677,#67678);
#55130=AXIS2_PLACEMENT_3D('',#90537,#67682,#67683);
#55131=AXIS2_PLACEMENT_3D('',#90543,#67687,#67688);
#55132=AXIS2_PLACEMENT_3D('',#90549,#67692,#67693);
#55133=AXIS2_PLACEMENT_3D('',#90555,#67697,#67698);
#55134=AXIS2_PLACEMENT_3D('',#90558,#67701,#67702);
#55135=AXIS2_PLACEMENT_3D('',#90559,#67703,#67704);
#55136=AXIS2_PLACEMENT_3D('',#90561,#67705,#67706);
#55137=AXIS2_PLACEMENT_3D('',#90562,#67707,#67708);
#55138=AXIS2_PLACEMENT_3D('',#90564,#67710,#67711);
#55139=AXIS2_PLACEMENT_3D('',#90565,#67712,#67713);
#55140=AXIS2_PLACEMENT_3D('',#90566,#67714,#67715);
#55141=AXIS2_PLACEMENT_3D('',#90567,#67716,#67717);
#55142=AXIS2_PLACEMENT_3D('',#90568,#67718,#67719);
#55143=AXIS2_PLACEMENT_3D('',#90569,#67720,#67721);
#55144=AXIS2_PLACEMENT_3D('',#90570,#67722,#67723);
#55145=AXIS2_PLACEMENT_3D('',#90571,#67724,#67725);
#55146=AXIS2_PLACEMENT_3D('',#90572,#67726,#67727);
#55147=AXIS2_PLACEMENT_3D('',#90573,#67728,#67729);
#55148=AXIS2_PLACEMENT_3D('',#90574,#67730,#67731);
#55149=AXIS2_PLACEMENT_3D('',#90575,#67732,#67733);
#55150=AXIS2_PLACEMENT_3D('',#90576,#67734,#67735);
#55151=AXIS2_PLACEMENT_3D('',#90577,#67736,#67737);
#55152=AXIS2_PLACEMENT_3D('',#90578,#67738,#67739);
#55153=AXIS2_PLACEMENT_3D('',#90579,#67740,#67741);
#55154=AXIS2_PLACEMENT_3D('',#90580,#67742,#67743);
#55155=AXIS2_PLACEMENT_3D('',#90581,#67744,#67745);
#55156=AXIS2_PLACEMENT_3D('',#90583,#67747,#67748);
#55157=AXIS2_PLACEMENT_3D('',#90584,#67749,#67750);
#55158=AXIS2_PLACEMENT_3D('',#90585,#67751,#67752);
#55159=AXIS2_PLACEMENT_3D('',#90586,#67753,#67754);
#55160=AXIS2_PLACEMENT_3D('',#90587,#67755,#67756);
#55161=AXIS2_PLACEMENT_3D('',#90588,#67757,#67758);
#55162=AXIS2_PLACEMENT_3D('',#90589,#67759,#67760);
#55163=AXIS2_PLACEMENT_3D('',#90590,#67761,#67762);
#55164=AXIS2_PLACEMENT_3D('',#90591,#67763,#67764);
#55165=AXIS2_PLACEMENT_3D('',#90592,#67765,#67766);
#55166=AXIS2_PLACEMENT_3D('',#90593,#67767,#67768);
#55167=AXIS2_PLACEMENT_3D('',#90594,#67769,#67770);
#55168=AXIS2_PLACEMENT_3D('',#90595,#67771,#67772);
#55169=AXIS2_PLACEMENT_3D('',#90596,#67773,#67774);
#55170=AXIS2_PLACEMENT_3D('',#90597,#67775,#67776);
#55171=AXIS2_PLACEMENT_3D('',#90598,#67777,#67778);
#55172=AXIS2_PLACEMENT_3D('',#90599,#67779,#67780);
#55173=AXIS2_PLACEMENT_3D('',#90600,#67781,#67782);
#55174=AXIS2_PLACEMENT_3D('',#90601,#67783,#67784);
#55175=AXIS2_PLACEMENT_3D('',#90602,#67785,#67786);
#55176=AXIS2_PLACEMENT_3D('',#90604,#67787,#67788);
#55177=AXIS2_PLACEMENT_3D('',#90606,#67790,#67791);
#55178=AXIS2_PLACEMENT_3D('',#90607,#67792,#67793);
#55179=AXIS2_PLACEMENT_3D('',#90608,#67794,#67795);
#55180=AXIS2_PLACEMENT_3D('',#90610,#67796,#67797);
#55181=AXIS2_PLACEMENT_3D('',#90612,#67798,#67799);
#55182=AXIS2_PLACEMENT_3D('',#90614,#67800,#67801);
#55183=AXIS2_PLACEMENT_3D('',#90615,#67802,#67803);
#55184=AXIS2_PLACEMENT_3D('',#90616,#67804,#67805);
#55185=AXIS2_PLACEMENT_3D('',#90619,#67807,#67808);
#55186=AXIS2_PLACEMENT_3D('',#90620,#67809,#67810);
#55187=AXIS2_PLACEMENT_3D('',#90621,#67811,#67812);
#55188=AXIS2_PLACEMENT_3D('',#90623,#67813,#67814);
#55189=AXIS2_PLACEMENT_3D('',#90624,#67815,#67816);
#55190=AXIS2_PLACEMENT_3D('',#90626,#67817,#67818);
#55191=AXIS2_PLACEMENT_3D('',#90628,#67820,#67821);
#55192=AXIS2_PLACEMENT_3D('',#90630,#67823,#67824);
#55193=AXIS2_PLACEMENT_3D('',#90631,#67825,#67826);
#55194=AXIS2_PLACEMENT_3D('',#90647,#67828,#67829);
#55195=AXIS2_PLACEMENT_3D('',#90655,#67830,#67831);
#55196=AXIS2_PLACEMENT_3D('',#90703,#67833,#67834);
#55197=AXIS2_PLACEMENT_3D('',#90751,#67836,#67837);
#55198=AXIS2_PLACEMENT_3D('',#90805,#67839,#67840);
#55199=AXIS2_PLACEMENT_3D('',#90853,#67842,#67843);
#55200=AXIS2_PLACEMENT_3D('',#90901,#67845,#67846);
#55201=AXIS2_PLACEMENT_3D('',#90955,#67848,#67849);
#55202=AXIS2_PLACEMENT_3D('',#91003,#67851,#67852);
#55203=AXIS2_PLACEMENT_3D('',#91051,#67854,#67855);
#55204=AXIS2_PLACEMENT_3D('',#91099,#67857,#67858);
#55205=AXIS2_PLACEMENT_3D('',#91153,#67860,#67861);
#55206=AXIS2_PLACEMENT_3D('',#91201,#67863,#67864);
#55207=AXIS2_PLACEMENT_3D('',#91249,#67866,#67867);
#55208=AXIS2_PLACEMENT_3D('',#91303,#67869,#67870);
#55209=AXIS2_PLACEMENT_3D('',#91351,#67872,#67873);
#55210=AXIS2_PLACEMENT_3D('',#91399,#67875,#67876);
#55211=AXIS2_PLACEMENT_3D('',#91453,#67878,#67879);
#55212=AXIS2_PLACEMENT_3D('',#91501,#67881,#67882);
#55213=AXIS2_PLACEMENT_3D('',#91549,#67884,#67885);
#55214=AXIS2_PLACEMENT_3D('',#91603,#67887,#67888);
#55215=AXIS2_PLACEMENT_3D('',#91651,#67890,#67891);
#55216=AXIS2_PLACEMENT_3D('',#91699,#67893,#67894);
#55217=AXIS2_PLACEMENT_3D('',#91753,#67896,#67897);
#55218=AXIS2_PLACEMENT_3D('',#91765,#67899,#67900);
#55219=AXIS2_PLACEMENT_3D('',#91771,#67901,#67902);
#55220=AXIS2_PLACEMENT_3D('',#91796,#67904,#67905);
#55221=AXIS2_PLACEMENT_3D('',#91821,#67907,#67908);
#55222=AXIS2_PLACEMENT_3D('',#91845,#67910,#67911);
#55223=AXIS2_PLACEMENT_3D('',#91870,#67913,#67914);
#55224=AXIS2_PLACEMENT_3D('',#91895,#67916,#67917);
#55225=AXIS2_PLACEMENT_3D('',#91919,#67919,#67920);
#55226=AXIS2_PLACEMENT_3D('',#91944,#67922,#67923);
#55227=AXIS2_PLACEMENT_3D('',#91969,#67925,#67926);
#55228=AXIS2_PLACEMENT_3D('',#91993,#67928,#67929);
#55229=AXIS2_PLACEMENT_3D('',#92018,#67931,#67932);
#55230=AXIS2_PLACEMENT_3D('',#92043,#67934,#67935);
#55231=AXIS2_PLACEMENT_3D('',#92067,#67937,#67938);
#55232=AXIS2_PLACEMENT_3D('',#92092,#67940,#67941);
#55233=AXIS2_PLACEMENT_3D('',#92117,#67943,#67944);
#55234=AXIS2_PLACEMENT_3D('',#92141,#67946,#67947);
#55235=AXIS2_PLACEMENT_3D('',#92165,#67949,#67950);
#55236=AXIS2_PLACEMENT_3D('',#92190,#67952,#67953);
#55237=AXIS2_PLACEMENT_3D('',#92215,#67955,#67956);
#55238=AXIS2_PLACEMENT_3D('',#92239,#67958,#67959);
#55239=AXIS2_PLACEMENT_3D('',#92264,#67961,#67962);
#55240=AXIS2_PLACEMENT_3D('',#92289,#67964,#67965);
#55241=AXIS2_PLACEMENT_3D('',#92313,#67967,#67968);
#55242=AXIS2_PLACEMENT_3D('',#92413,#67969,#67970);
#55243=AXIS2_PLACEMENT_3D('',#92415,#67971,#67972);
#55244=AXIS2_PLACEMENT_3D('',#93243,#67973,#67974);
#55245=AXIS2_PLACEMENT_3D('',#93245,#67975,#67976);
#55246=AXIS2_PLACEMENT_3D('',#93246,#67977,#67978);
#55247=AXIS2_PLACEMENT_3D('',#93345,#67979,#67980);
#55248=AXIS2_PLACEMENT_3D('',#93346,#67981,#67982);
#55249=AXIS2_PLACEMENT_3D('',#93975,#67983,#67984);
#55250=AXIS2_PLACEMENT_3D('',#93977,#67985,#67986);
#55251=AXIS2_PLACEMENT_3D('',#93978,#67987,#67988);
#55252=AXIS2_PLACEMENT_3D('',#93979,#67989,#67990);
#55253=AXIS2_PLACEMENT_3D('',#93980,#67991,#67992);
#55254=AXIS2_PLACEMENT_3D('',#93981,#67993,#67994);
#55255=AXIS2_PLACEMENT_3D('',#93983,#67995,#67996);
#55256=AXIS2_PLACEMENT_3D('',#93984,#67997,#67998);
#55257=AXIS2_PLACEMENT_3D('',#94008,#68000,#68001);
#55258=AXIS2_PLACEMENT_3D('',#94012,#68002,#68003);
#55259=AXIS2_PLACEMENT_3D('',#94018,#68007,#68008);
#55260=AXIS2_PLACEMENT_3D('',#94022,#68011,#68012);
#55261=AXIS2_PLACEMENT_3D('',#94026,#68015,#68016);
#55262=AXIS2_PLACEMENT_3D('',#94028,#68017,#68018);
#55263=AXIS2_PLACEMENT_3D('',#94030,#68020,#68021);
#55264=AXIS2_PLACEMENT_3D('',#94032,#68022,#68023);
#55265=AXIS2_PLACEMENT_3D('',#94033,#68024,#68025);
#55266=AXIS2_PLACEMENT_3D('',#94035,#68027,#68028);
#55267=AXIS2_PLACEMENT_3D('',#94039,#68031,#68032);
#55268=AXIS2_PLACEMENT_3D('',#94043,#68035,#68036);
#55269=AXIS2_PLACEMENT_3D('',#94045,#68038,#68039);
#55270=AXIS2_PLACEMENT_3D('',#94046,#68040,#68041);
#55271=AXIS2_PLACEMENT_3D('',#94047,#68042,#68043);
#55272=AXIS2_PLACEMENT_3D('',#94048,#68044,#68045);
#55273=AXIS2_PLACEMENT_3D('',#94050,#68046,#68047);
#55274=AXIS2_PLACEMENT_3D('',#94053,#68049,#68050);
#55275=AXIS2_PLACEMENT_3D('',#94054,#68051,#68052);
#55276=AXIS2_PLACEMENT_3D('',#94056,#68053,#68054);
#55277=AXIS2_PLACEMENT_3D('',#94058,#68056,#68057);
#55278=AXIS2_PLACEMENT_3D('',#94060,#68058,#68059);
#55279=AXIS2_PLACEMENT_3D('',#94062,#68061,#68062);
#55280=AXIS2_PLACEMENT_3D('',#94064,#68063,#68064);
#55281=AXIS2_PLACEMENT_3D('',#94065,#68065,#68066);
#55282=AXIS2_PLACEMENT_3D('',#94068,#68068,#68069);
#55283=AXIS2_PLACEMENT_3D('',#94069,#68070,#68071);
#55284=AXIS2_PLACEMENT_3D('',#94072,#68073,#68074);
#55285=AXIS2_PLACEMENT_3D('',#94073,#68075,#68076);
#55286=AXIS2_PLACEMENT_3D('',#94076,#68078,#68079);
#55287=AXIS2_PLACEMENT_3D('',#94077,#68080,#68081);
#55288=AXIS2_PLACEMENT_3D('',#94078,#68082,#68083);
#55289=AXIS2_PLACEMENT_3D('',#94079,#68084,#68085);
#55290=AXIS2_PLACEMENT_3D('',#94084,#68087,#68088);
#55291=AXIS2_PLACEMENT_3D('',#94086,#68089,#68090);
#55292=AXIS2_PLACEMENT_3D('',#94087,#68091,#68092);
#55293=AXIS2_PLACEMENT_3D('',#94088,#68093,#68094);
#55294=AXIS2_PLACEMENT_3D('',#94101,#68096,#68097);
#55295=AXIS2_PLACEMENT_3D('',#94112,#68099,#68100);
#55296=AXIS2_PLACEMENT_3D('',#94113,#68101,#68102);
#55297=AXIS2_PLACEMENT_3D('',#94120,#68103,#68104);
#55298=AXIS2_PLACEMENT_3D('',#94135,#68107,#68108);
#55299=AXIS2_PLACEMENT_3D('',#94136,#68109,#68110);
#55300=AXIS2_PLACEMENT_3D('',#94137,#68111,#68112);
#55301=AXIS2_PLACEMENT_3D('',#94138,#68113,#68114);
#55302=AXIS2_PLACEMENT_3D('',#94139,#68115,#68116);
#55303=AXIS2_PLACEMENT_3D('',#94140,#68117,#68118);
#55304=AXIS2_PLACEMENT_3D('',#94141,#68119,#68120);
#55305=AXIS2_PLACEMENT_3D('',#94142,#68121,#68122);
#55306=AXIS2_PLACEMENT_3D('',#94143,#68123,#68124);
#55307=AXIS2_PLACEMENT_3D('',#94144,#68125,#68126);
#55308=AXIS2_PLACEMENT_3D('',#94145,#68127,#68128);
#55309=AXIS2_PLACEMENT_3D('',#94146,#68129,#68130);
#55310=AXIS2_PLACEMENT_3D('',#94147,#68131,#68132);
#55311=AXIS2_PLACEMENT_3D('',#94148,#68133,#68134);
#55312=AXIS2_PLACEMENT_3D('',#94149,#68135,#68136);
#55313=AXIS2_PLACEMENT_3D('',#94150,#68137,#68138);
#55314=AXIS2_PLACEMENT_3D('',#94151,#68139,#68140);
#55315=AXIS2_PLACEMENT_3D('',#94152,#68141,#68142);
#55316=AXIS2_PLACEMENT_3D('',#94154,#68143,#68144);
#55317=AXIS2_PLACEMENT_3D('',#94157,#68146,#68147);
#55318=AXIS2_PLACEMENT_3D('',#94158,#68148,#68149);
#55319=AXIS2_PLACEMENT_3D('',#94161,#68151,#68152);
#55320=AXIS2_PLACEMENT_3D('',#94162,#68153,#68154);
#55321=AXIS2_PLACEMENT_3D('',#94165,#68156,#68157);
#55322=AXIS2_PLACEMENT_3D('',#94166,#68158,#68159);
#55323=AXIS2_PLACEMENT_3D('',#94168,#68160,#68161);
#55324=AXIS2_PLACEMENT_3D('',#94194,#68163,#68164);
#55325=AXIS2_PLACEMENT_3D('',#94202,#68167,#68168);
#55326=AXIS2_PLACEMENT_3D('',#94208,#68170,#68171);
#55327=AXIS2_PLACEMENT_3D('',#94214,#68173,#68174);
#55328=AXIS2_PLACEMENT_3D('',#94225,#68176,#68177);
#55329=AXIS2_PLACEMENT_3D('',#94229,#68178,#68179);
#55330=AXIS2_PLACEMENT_3D('',#94231,#68181,#68182);
#55331=AXIS2_PLACEMENT_3D('',#94233,#68184,#68185);
#55332=AXIS2_PLACEMENT_3D('',#94234,#68186,#68187);
#55333=AXIS2_PLACEMENT_3D('',#94235,#68188,#68189);
#55334=AXIS2_PLACEMENT_3D('',#94236,#68190,#68191);
#55335=AXIS2_PLACEMENT_3D('',#94237,#68192,#68193);
#55336=AXIS2_PLACEMENT_3D('',#94238,#68194,#68195);
#55337=AXIS2_PLACEMENT_3D('',#94239,#68196,#68197);
#55338=AXIS2_PLACEMENT_3D('',#94240,#68198,#68199);
#55339=AXIS2_PLACEMENT_3D('',#94241,#68200,#68201);
#55340=AXIS2_PLACEMENT_3D('',#94242,#68202,#68203);
#55341=AXIS2_PLACEMENT_3D('',#94243,#68204,#68205);
#55342=AXIS2_PLACEMENT_3D('',#94244,#68206,#68207);
#55343=AXIS2_PLACEMENT_3D('',#94245,#68208,#68209);
#55344=AXIS2_PLACEMENT_3D('',#94246,#68210,#68211);
#55345=AXIS2_PLACEMENT_3D('',#94247,#68212,#68213);
#55346=AXIS2_PLACEMENT_3D('',#94248,#68214,#68215);
#55347=AXIS2_PLACEMENT_3D('',#94249,#68216,#68217);
#55348=AXIS2_PLACEMENT_3D('',#94250,#68218,#68219);
#55349=AXIS2_PLACEMENT_3D('',#94251,#68220,#68221);
#55350=AXIS2_PLACEMENT_3D('',#94252,#68222,#68223);
#55351=AXIS2_PLACEMENT_3D('',#94253,#68224,#68225);
#55352=AXIS2_PLACEMENT_3D('',#94254,#68226,#68227);
#55353=AXIS2_PLACEMENT_3D('',#94255,#68228,#68229);
#55354=AXIS2_PLACEMENT_3D('',#94256,#68230,#68231);
#55355=AXIS2_PLACEMENT_3D('',#94257,#68232,#68233);
#55356=AXIS2_PLACEMENT_3D('',#94258,#68234,#68235);
#55357=AXIS2_PLACEMENT_3D('',#94259,#68236,#68237);
#55358=AXIS2_PLACEMENT_3D('',#94260,#68238,#68239);
#55359=AXIS2_PLACEMENT_3D('',#94261,#68240,#68241);
#55360=AXIS2_PLACEMENT_3D('',#94262,#68242,#68243);
#55361=AXIS2_PLACEMENT_3D('',#94263,#68244,#68245);
#55362=AXIS2_PLACEMENT_3D('',#94264,#68246,#68247);
#55363=AXIS2_PLACEMENT_3D('',#94265,#68248,#68249);
#55364=AXIS2_PLACEMENT_3D('',#94266,#68250,#68251);
#55365=AXIS2_PLACEMENT_3D('',#94267,#68252,#68253);
#55366=AXIS2_PLACEMENT_3D('',#94268,#68254,#68255);
#55367=AXIS2_PLACEMENT_3D('',#94269,#68256,#68257);
#55368=DIRECTION('axis',(0.,0.,1.));
#55369=DIRECTION('refdir',(1.,0.,0.));
#55370=DIRECTION('axis',(0.,0.,1.));
#55371=DIRECTION('refdir',(1.,0.,0.));
#55372=DIRECTION('center_axis',(1.,0.,0.));
#55373=DIRECTION('ref_axis',(0.,1.,0.));
#55374=DIRECTION('center_axis',(-1.,0.,0.));
#55375=DIRECTION('ref_axis',(0.,1.,0.));
#55376=DIRECTION('center_axis',(1.,0.,0.));
#55377=DIRECTION('ref_axis',(0.,1.,0.));
#55378=DIRECTION('center_axis',(-1.,0.,0.));
#55379=DIRECTION('ref_axis',(0.,1.,0.));
#55380=DIRECTION('center_axis',(1.,0.,0.));
#55381=DIRECTION('ref_axis',(0.,1.,0.));
#55382=DIRECTION('center_axis',(-1.,0.,0.));
#55383=DIRECTION('ref_axis',(0.,1.,0.));
#55384=DIRECTION('center_axis',(1.,0.,0.));
#55385=DIRECTION('ref_axis',(0.,1.,0.));
#55386=DIRECTION('center_axis',(-1.,0.,0.));
#55387=DIRECTION('ref_axis',(0.,1.,0.));
#55388=DIRECTION('center_axis',(1.,0.,0.));
#55389=DIRECTION('ref_axis',(0.,1.,0.));
#55390=DIRECTION('center_axis',(-1.,0.,0.));
#55391=DIRECTION('ref_axis',(0.,1.,0.));
#55392=DIRECTION('center_axis',(1.,0.,0.));
#55393=DIRECTION('ref_axis',(0.,1.,0.));
#55394=DIRECTION('center_axis',(-1.,0.,0.));
#55395=DIRECTION('ref_axis',(0.,1.,0.));
#55396=DIRECTION('center_axis',(1.,0.,0.));
#55397=DIRECTION('ref_axis',(0.,1.,0.));
#55398=DIRECTION('center_axis',(-1.,0.,0.));
#55399=DIRECTION('ref_axis',(0.,1.,0.));
#55400=DIRECTION('center_axis',(1.,0.,0.));
#55401=DIRECTION('ref_axis',(0.,1.,0.));
#55402=DIRECTION('center_axis',(-1.,0.,0.));
#55403=DIRECTION('ref_axis',(0.,1.,0.));
#55404=DIRECTION('center_axis',(1.,0.,0.));
#55405=DIRECTION('ref_axis',(0.,1.,0.));
#55406=DIRECTION('center_axis',(-1.,0.,0.));
#55407=DIRECTION('ref_axis',(0.,1.,0.));
#55408=DIRECTION('center_axis',(1.,0.,0.));
#55409=DIRECTION('ref_axis',(0.,1.,0.));
#55410=DIRECTION('center_axis',(-1.,0.,0.));
#55411=DIRECTION('ref_axis',(0.,1.,0.));
#55412=DIRECTION('center_axis',(1.,0.,0.));
#55413=DIRECTION('ref_axis',(0.,1.,0.));
#55414=DIRECTION('center_axis',(-1.,0.,0.));
#55415=DIRECTION('ref_axis',(0.,1.,0.));
#55416=DIRECTION('center_axis',(1.,0.,0.));
#55417=DIRECTION('ref_axis',(0.,1.,0.));
#55418=DIRECTION('center_axis',(-1.,0.,0.));
#55419=DIRECTION('ref_axis',(0.,1.,0.));
#55420=DIRECTION('center_axis',(1.,0.,0.));
#55421=DIRECTION('ref_axis',(0.,1.,0.));
#55422=DIRECTION('center_axis',(-1.,0.,0.));
#55423=DIRECTION('ref_axis',(0.,1.,0.));
#55424=DIRECTION('center_axis',(1.,0.,0.));
#55425=DIRECTION('ref_axis',(0.,1.,0.));
#55426=DIRECTION('center_axis',(-1.,0.,0.));
#55427=DIRECTION('ref_axis',(0.,1.,0.));
#55428=DIRECTION('center_axis',(1.,0.,0.));
#55429=DIRECTION('ref_axis',(0.,1.,0.));
#55430=DIRECTION('center_axis',(-1.,0.,0.));
#55431=DIRECTION('ref_axis',(0.,1.,0.));
#55432=DIRECTION('center_axis',(1.,0.,0.));
#55433=DIRECTION('ref_axis',(0.,1.,0.));
#55434=DIRECTION('center_axis',(-1.,0.,0.));
#55435=DIRECTION('ref_axis',(0.,1.,0.));
#55436=DIRECTION('center_axis',(1.,0.,0.));
#55437=DIRECTION('ref_axis',(0.,1.,0.));
#55438=DIRECTION('center_axis',(-1.,0.,0.));
#55439=DIRECTION('ref_axis',(0.,1.,0.));
#55440=DIRECTION('center_axis',(1.,0.,0.));
#55441=DIRECTION('ref_axis',(0.,-1.,1.22464679914735E-16));
#55442=DIRECTION('center_axis',(-1.,0.,0.));
#55443=DIRECTION('ref_axis',(0.,1.,0.));
#55444=DIRECTION('center_axis',(1.,0.,0.));
#55445=DIRECTION('ref_axis',(0.,1.,0.));
#55446=DIRECTION('center_axis',(-1.,0.,0.));
#55447=DIRECTION('ref_axis',(0.,1.,0.));
#55448=DIRECTION('center_axis',(1.,0.,0.));
#55449=DIRECTION('ref_axis',(0.,1.,0.));
#55450=DIRECTION('center_axis',(-1.,0.,0.));
#55451=DIRECTION('ref_axis',(0.,1.,0.));
#55452=DIRECTION('center_axis',(1.,0.,0.));
#55453=DIRECTION('ref_axis',(0.,1.,0.));
#55454=DIRECTION('center_axis',(-1.,0.,0.));
#55455=DIRECTION('ref_axis',(0.,1.,0.));
#55456=DIRECTION('center_axis',(1.,0.,0.));
#55457=DIRECTION('ref_axis',(0.,1.,0.));
#55458=DIRECTION('center_axis',(-1.,0.,0.));
#55459=DIRECTION('ref_axis',(0.,1.,0.));
#55460=DIRECTION('center_axis',(1.,0.,0.));
#55461=DIRECTION('ref_axis',(0.,1.,0.));
#55462=DIRECTION('center_axis',(-1.,0.,0.));
#55463=DIRECTION('ref_axis',(0.,1.,0.));
#55464=DIRECTION('center_axis',(1.,0.,0.));
#55465=DIRECTION('ref_axis',(0.,1.,0.));
#55466=DIRECTION('center_axis',(-1.,0.,0.));
#55467=DIRECTION('ref_axis',(0.,1.,0.));
#55468=DIRECTION('center_axis',(1.,0.,0.));
#55469=DIRECTION('ref_axis',(0.,1.,0.));
#55470=DIRECTION('center_axis',(-1.,0.,0.));
#55471=DIRECTION('ref_axis',(0.,1.,0.));
#55472=DIRECTION('center_axis',(1.,0.,0.));
#55473=DIRECTION('ref_axis',(0.,1.,0.));
#55474=DIRECTION('center_axis',(-1.,0.,0.));
#55475=DIRECTION('ref_axis',(0.,1.,0.));
#55476=DIRECTION('center_axis',(1.,0.,0.));
#55477=DIRECTION('ref_axis',(0.,1.,0.));
#55478=DIRECTION('center_axis',(-1.,0.,0.));
#55479=DIRECTION('ref_axis',(0.,1.,0.));
#55480=DIRECTION('center_axis',(1.,0.,0.));
#55481=DIRECTION('ref_axis',(0.,1.,0.));
#55482=DIRECTION('center_axis',(-1.,0.,0.));
#55483=DIRECTION('ref_axis',(0.,1.,0.));
#55484=DIRECTION('center_axis',(1.,0.,0.));
#55485=DIRECTION('ref_axis',(0.,1.,0.));
#55486=DIRECTION('center_axis',(-1.,0.,0.));
#55487=DIRECTION('ref_axis',(0.,1.,0.));
#55488=DIRECTION('center_axis',(1.,0.,0.));
#55489=DIRECTION('ref_axis',(0.,1.,0.));
#55490=DIRECTION('center_axis',(-1.,0.,0.));
#55491=DIRECTION('ref_axis',(0.,1.,0.));
#55492=DIRECTION('center_axis',(1.,0.,0.));
#55493=DIRECTION('ref_axis',(0.,1.,0.));
#55494=DIRECTION('center_axis',(-1.,0.,0.));
#55495=DIRECTION('ref_axis',(0.,1.,0.));
#55496=DIRECTION('center_axis',(1.,0.,0.));
#55497=DIRECTION('ref_axis',(0.,1.,0.));
#55498=DIRECTION('center_axis',(-1.,0.,0.));
#55499=DIRECTION('ref_axis',(0.,1.,0.));
#55500=DIRECTION('center_axis',(1.,0.,0.));
#55501=DIRECTION('ref_axis',(0.,1.,0.));
#55502=DIRECTION('center_axis',(-1.,0.,0.));
#55503=DIRECTION('ref_axis',(0.,1.,0.));
#55504=DIRECTION('center_axis',(1.,0.,0.));
#55505=DIRECTION('ref_axis',(0.,1.,0.));
#55506=DIRECTION('center_axis',(-1.,0.,0.));
#55507=DIRECTION('ref_axis',(0.,1.,0.));
#55508=DIRECTION('center_axis',(1.,0.,0.));
#55509=DIRECTION('ref_axis',(0.,1.,0.));
#55510=DIRECTION('center_axis',(-1.,0.,0.));
#55511=DIRECTION('ref_axis',(0.,1.,0.));
#55512=DIRECTION('center_axis',(1.,0.,0.));
#55513=DIRECTION('ref_axis',(0.,1.,0.));
#55514=DIRECTION('center_axis',(-1.,0.,0.));
#55515=DIRECTION('ref_axis',(0.,1.,0.));
#55516=DIRECTION('center_axis',(0.,1.,0.));
#55517=DIRECTION('ref_axis',(1.,0.,0.));
#55518=DIRECTION('',(0.755033118392644,0.,-0.655686655446243));
#55519=DIRECTION('',(1.,0.,0.));
#55520=DIRECTION('',(0.,0.,1.));
#55521=DIRECTION('',(0.998052578482888,0.,0.0623782861551806));
#55522=DIRECTION('',(0.957826285221151,0.,-0.287347885566345));
#55523=DIRECTION('',(0.86824314212446,0.,-0.496138938356832));
#55524=DIRECTION('',(0.948683298050513,0.,-0.31622776601684));
#55525=DIRECTION('',(1.,0.,0.));
#55526=DIRECTION('',(0.948683298050514,0.,0.316227766016839));
#55527=DIRECTION('',(0.868243142124459,0.,0.496138938356833));
#55528=DIRECTION('',(0.957826285221151,0.,0.287347885566346));
#55529=DIRECTION('',(0.998052578482888,0.,-0.0623782861551805));
#55530=DIRECTION('',(0.,0.,-1.));
#55531=DIRECTION('',(1.,0.,0.));
#55532=DIRECTION('',(0.755033118392644,0.,0.655686655446243));
#55533=DIRECTION('',(-0.755033118392644,0.,0.655686655446243));
#55534=DIRECTION('',(-1.,0.,0.));
#55535=DIRECTION('',(0.,0.,-1.));
#55536=DIRECTION('',(-0.998052578482888,0.,-0.0623782861551805));
#55537=DIRECTION('',(-0.957826285221151,0.,0.287347885566346));
#55538=DIRECTION('',(-0.868243142124459,0.,0.496138938356833));
#55539=DIRECTION('',(-0.948683298050514,0.,0.316227766016839));
#55540=DIRECTION('',(-1.,0.,0.));
#55541=DIRECTION('',(-0.948683298050513,0.,-0.31622776601684));
#55542=DIRECTION('',(-0.86824314212446,0.,-0.496138938356832));
#55543=DIRECTION('',(-0.957826285221151,0.,-0.287347885566345));
#55544=DIRECTION('',(-0.998052578482888,0.,0.0623782861551806));
#55545=DIRECTION('',(0.,0.,1.));
#55546=DIRECTION('',(-1.,0.,0.));
#55547=DIRECTION('',(-0.755033118392644,0.,-0.655686655446243));
#55548=DIRECTION('center_axis',(0.649305557988371,-0.139173100960065,0.747685187986608));
#55549=DIRECTION('ref_axis',(0.755033118392643,0.,-0.655686655446243));
#55550=DIRECTION('',(0.,0.983113759331517,0.182995454077559));
#55551=DIRECTION('',(-0.755033118392644,0.,0.655686655446243));
#55552=DIRECTION('center_axis',(-0.649305557988371,0.139173100960065,-0.747685187986608));
#55553=DIRECTION('ref_axis',(0.760527640763576,0.118819965419165,-0.638341228068795));
#55554=DIRECTION('',(0.0519254248777275,0.98893216263388,0.138985351600607));
#55555=DIRECTION('center_axis',(0.,0.984807753012208,0.17364817766693));
#55556=DIRECTION('ref_axis',(1.,0.,0.));
#55557=DIRECTION('',(0.755033118392643,0.113858792838765,-0.645725301830105));
#55558=DIRECTION('',(1.,0.,0.));
#55559=DIRECTION('',(0.,-0.17364817766693,0.984807753012208));
#55560=DIRECTION('',(0.998052578482888,-0.0108318757168334,0.0614306198252359));
#55561=DIRECTION('',(0.957826285221151,0.0498974366850415,-0.282982425517402));
#55562=DIRECTION('',(0.86824314212446,0.0861536225152694,-0.488601473065054));
#55563=DIRECTION('',(0.948683298050513,0.0549123752965087,-0.311423555691114));
#55564=DIRECTION('',(1.,0.,0.));
#55565=DIRECTION('',(0.948683298050514,-0.0549123752965085,0.311423555691113));
#55566=DIRECTION('',(0.868243142124459,-0.0861536225152696,0.488601473065055));
#55567=DIRECTION('',(0.957826285221151,-0.0498974366850416,0.282982425517402));
#55568=DIRECTION('',(0.998052578482888,0.0108318757168334,-0.0614306198252359));
#55569=DIRECTION('',(0.,0.17364817766693,-0.984807753012208));
#55570=DIRECTION('',(1.,0.,0.));
#55571=DIRECTION('',(0.755033118392644,-0.113858792838765,0.645725301830105));
#55572=DIRECTION('',(-0.755033118392644,-0.113858792838765,0.645725301830105));
#55573=DIRECTION('',(-1.,0.,0.));
#55574=DIRECTION('',(0.,0.17364817766693,-0.984807753012208));
#55575=DIRECTION('',(-0.998052578482888,0.0108318757168334,-0.0614306198252359));
#55576=DIRECTION('',(-0.957826285221151,-0.0498974366850416,0.282982425517402));
#55577=DIRECTION('',(-0.868243142124459,-0.0861536225152696,0.488601473065055));
#55578=DIRECTION('',(-0.948683298050514,-0.0549123752965085,0.311423555691113));
#55579=DIRECTION('',(-1.,0.,0.));
#55580=DIRECTION('',(-0.948683298050513,0.0549123752965087,-0.311423555691114));
#55581=DIRECTION('',(-0.86824314212446,0.0861536225152694,-0.488601473065054));
#55582=DIRECTION('',(-0.957826285221151,0.0498974366850415,-0.282982425517402));
#55583=DIRECTION('',(-0.998052578482888,-0.0108318757168334,0.0614306198252359));
#55584=DIRECTION('',(0.,-0.17364817766693,0.984807753012208));
#55585=DIRECTION('',(-1.,0.,0.));
#55586=DIRECTION('',(-0.755033118392643,0.113858792838765,-0.645725301830105));
#55587=DIRECTION('center_axis',(0.649305557988371,-0.266892919198654,0.712159014579631));
#55588=DIRECTION('ref_axis',(0.755033118392643,0.113858792838765,-0.645725301830105));
#55589=DIRECTION('',(0.,0.936401225160756,0.350931254688773));
#55590=DIRECTION('',(-0.755033118392643,-0.113858792838765,0.645725301830105));
#55591=DIRECTION('center_axis',(-0.649305557988371,0.266892919198654,-0.712159014579631));
#55592=DIRECTION('ref_axis',(0.760527640763576,0.227861614141253,-0.608010520003998));
#55593=DIRECTION('',(0.0519254248777275,0.949773507937132,0.308600119688995));
#55594=DIRECTION('center_axis',(0.,0.939692620785908,0.342020143325669));
#55595=DIRECTION('ref_axis',(1.,0.,0.));
#55596=DIRECTION('',(0.755033118392644,0.224258043872452,-0.616143911670627));
#55597=DIRECTION('',(1.,0.,0.));
#55598=DIRECTION('',(0.,-0.342020143325669,0.939692620785908));
#55599=DIRECTION('',(0.998052578482888,-0.0213346303712044,0.058616415197295));
#55600=DIRECTION('',(0.957826285221151,0.0982787650057293,-0.270018687665128));
#55601=DIRECTION('',(0.86824314212446,0.169689510806249,-0.46621809925847));
#55602=DIRECTION('',(0.948683298050513,0.108156265856636,-0.297156898213637));
#55603=DIRECTION('',(1.,0.,0.));
#55604=DIRECTION('',(0.948683298050514,-0.108156265856635,0.297156898213636));
#55605=DIRECTION('',(0.868243142124459,-0.169689510806249,0.466218099258471));
#55606=DIRECTION('',(0.957826285221151,-0.0982787650057295,0.270018687665129));
#55607=DIRECTION('',(0.998052578482888,0.0213346303712044,-0.0586164151972949));
#55608=DIRECTION('',(0.,0.342020143325669,-0.939692620785908));
#55609=DIRECTION('',(1.,0.,0.));
#55610=DIRECTION('',(0.755033118392644,-0.224258043872452,0.616143911670627));
#55611=DIRECTION('',(-0.755033118392644,-0.224258043872452,0.616143911670627));
#55612=DIRECTION('',(-1.,0.,0.));
#55613=DIRECTION('',(0.,0.342020143325669,-0.939692620785908));
#55614=DIRECTION('',(-0.998052578482888,0.0213346303712044,-0.0586164151972949));
#55615=DIRECTION('',(-0.957826285221151,-0.0982787650057295,0.270018687665129));
#55616=DIRECTION('',(-0.868243142124459,-0.169689510806249,0.466218099258471));
#55617=DIRECTION('',(-0.948683298050514,-0.108156265856635,0.297156898213636));
#55618=DIRECTION('',(-1.,0.,0.));
#55619=DIRECTION('',(-0.948683298050513,0.108156265856636,-0.297156898213637));
#55620=DIRECTION('',(-0.86824314212446,0.169689510806249,-0.46621809925847));
#55621=DIRECTION('',(-0.957826285221151,0.0982787650057293,-0.270018687665128));
#55622=DIRECTION('',(-0.998052578482888,-0.0213346303712044,0.058616415197295));
#55623=DIRECTION('',(0.,-0.342020143325669,0.939692620785908));
#55624=DIRECTION('',(-1.,0.,0.));
#55625=DIRECTION('',(-0.755033118392644,0.224258043872452,-0.616143911670627));
#55626=DIRECTION('center_axis',(0.649305557988371,-0.386503331141725,0.654994249884502));
#55627=DIRECTION('ref_axis',(0.755033118392643,0.224258043872452,-0.616143911670627));
#55628=DIRECTION('',(0.,0.861236613605368,0.508204186706051));
#55629=DIRECTION('',(-0.755033118392644,-0.224258043872452,0.616143911670627));
#55630=DIRECTION('center_axis',(-0.649305557988371,0.386503331141725,-0.654994249884502));
#55631=DIRECTION('ref_axis',(0.760527640763576,0.329979803021199,-0.559205719957048));
#55632=DIRECTION('',(0.0519254248777275,0.881756465810299,0.468838229299828));
#55633=DIRECTION('center_axis',(0.,0.866025403784439,0.5));
#55634=DIRECTION('ref_axis',(1.,0.,0.));
#55635=DIRECTION('',(0.755033118392644,0.327843327723122,-0.567841300538901));
#55636=DIRECTION('',(1.,0.,0.));
#55637=DIRECTION('',(0.,-0.5,0.866025403784439));
#55638=DIRECTION('',(0.998052578482888,-0.0311891430775903,0.0540211804549215));
#55639=DIRECTION('',(0.957826285221151,0.143673942783173,-0.248850568624199));
#55640=DIRECTION('',(0.86824314212446,0.248069469178416,-0.429668924423658));
#55641=DIRECTION('',(0.948683298050513,0.15811388300842,-0.273861278752585));
#55642=DIRECTION('',(1.,0.,0.));
#55643=DIRECTION('',(0.948683298050514,-0.158113883008419,0.273861278752584));
#55644=DIRECTION('',(0.868243142124459,-0.248069469178417,0.429668924423659));
#55645=DIRECTION('',(0.957826285221151,-0.143673942783173,0.248850568624199));
#55646=DIRECTION('',(0.998052578482888,0.0311891430775903,-0.0540211804549215));
#55647=DIRECTION('',(0.,0.5,-0.866025403784439));
#55648=DIRECTION('',(1.,0.,0.));
#55649=DIRECTION('',(0.755033118392644,-0.327843327723121,0.567841300538901));
#55650=DIRECTION('',(-0.755033118392644,-0.327843327723121,0.567841300538901));
#55651=DIRECTION('',(-1.,0.,0.));
#55652=DIRECTION('',(0.,0.5,-0.866025403784439));
#55653=DIRECTION('',(-0.998052578482888,0.0311891430775903,-0.0540211804549215));
#55654=DIRECTION('',(-0.957826285221151,-0.143673942783173,0.248850568624199));
#55655=DIRECTION('',(-0.868243142124459,-0.248069469178417,0.429668924423659));
#55656=DIRECTION('',(-0.948683298050514,-0.158113883008419,0.273861278752584));
#55657=DIRECTION('',(-1.,0.,0.));
#55658=DIRECTION('',(-0.948683298050513,0.15811388300842,-0.273861278752585));
#55659=DIRECTION('',(-0.86824314212446,0.248069469178416,-0.429668924423658));
#55660=DIRECTION('',(-0.957826285221151,0.143673942783173,-0.248850568624199));
#55661=DIRECTION('',(-0.998052578482888,-0.0311891430775903,0.0540211804549215));
#55662=DIRECTION('',(0.,-0.5,0.866025403784439));
#55663=DIRECTION('',(-1.,0.,0.));
#55664=DIRECTION('',(-0.755033118392644,0.327843327723122,-0.567841300538901));
#55665=DIRECTION('center_axis',(0.649305557988371,-0.494370034948177,0.577927816349714));
#55666=DIRECTION('ref_axis',(0.755033118392643,0.327843327723122,-0.567841300538901));
#55667=DIRECTION('',(0.,0.759903763352335,0.650035591673993));
#55668=DIRECTION('',(-0.755033118392644,-0.327843327723122,0.567841300538901));
#55669=DIRECTION('center_axis',(-0.649305557988371,0.494370034948177,-0.577927816349714));
#55670=DIRECTION('ref_axis',(0.760527640763576,0.422071722564183,-0.493409737080951));
#55671=DIRECTION('',(0.0519254248777275,0.786947699660121,0.614830926556978));
#55672=DIRECTION('center_axis',(0.,0.766044443118978,0.642787609686539));
#55673=DIRECTION('ref_axis',(1.,0.,0.));
#55674=DIRECTION('',(0.755033118392644,0.421467257957652,-0.502285118831863));
#55675=DIRECTION('',(1.,0.,0.));
#55676=DIRECTION('',(0.,-0.642787609686539,0.766044443118978));
#55677=DIRECTION('',(0.998052578482888,-0.0400959894540315,0.0477845394804616));
#55678=DIRECTION('',(0.957826285221151,0.184703660511672,-0.220121250980087));
#55679=DIRECTION('',(0.86824314212446,0.318911962258805,-0.3800644767432));
#55680=DIRECTION('',(0.948683298050513,0.203267289834479,-0.242244522917128));
#55681=DIRECTION('',(1.,0.,0.));
#55682=DIRECTION('',(0.948683298050514,-0.203267289834478,0.242244522917128));
#55683=DIRECTION('',(0.868243142124459,-0.318911962258806,0.380064476743201));
#55684=DIRECTION('',(0.957826285221151,-0.184703660511673,0.220121250980087));
#55685=DIRECTION('',(0.998052578482888,0.0400959894540314,-0.0477845394804615));
#55686=DIRECTION('',(0.,0.642787609686539,-0.766044443118978));
#55687=DIRECTION('',(1.,0.,0.));
#55688=DIRECTION('',(0.755033118392644,-0.421467257957652,0.502285118831862));
#55689=DIRECTION('',(-0.755033118392644,-0.421467257957652,0.502285118831862));
#55690=DIRECTION('',(-1.,0.,0.));
#55691=DIRECTION('',(0.,0.642787609686539,-0.766044443118978));
#55692=DIRECTION('',(-0.998052578482888,0.0400959894540314,-0.0477845394804615));
#55693=DIRECTION('',(-0.957826285221151,-0.184703660511673,0.220121250980087));
#55694=DIRECTION('',(-0.868243142124459,-0.318911962258806,0.380064476743201));
#55695=DIRECTION('',(-0.948683298050514,-0.203267289834478,0.242244522917128));
#55696=DIRECTION('',(-1.,0.,0.));
#55697=DIRECTION('',(-0.948683298050513,0.203267289834479,-0.242244522917128));
#55698=DIRECTION('',(-0.86824314212446,0.318911962258805,-0.3800644767432));
#55699=DIRECTION('',(-0.957826285221151,0.184703660511672,-0.220121250980087));
#55700=DIRECTION('',(-0.998052578482888,-0.0400959894540315,0.0477845394804616));
#55701=DIRECTION('',(0.,-0.642787609686539,0.766044443118978));
#55702=DIRECTION('',(-1.,0.,0.));
#55703=DIRECTION('',(-0.755033118392644,0.421467257957652,-0.502285118831863));
#55704=DIRECTION('center_axis',(0.649305557988371,-0.587215555406037,0.483301338560726));
#55705=DIRECTION('ref_axis',(0.755033118392643,0.421467257957652,-0.502285118831863));
#55706=DIRECTION('',(0.,0.6354816217797,0.772115994122802));
#55707=DIRECTION('',(-0.755033118392644,-0.421467257957652,0.502285118831863));
#55708=DIRECTION('center_axis',(-0.649305557988371,0.587215555406037,-0.483301338560726));
#55709=DIRECTION('ref_axis',(0.760527640763576,0.501339206395651,-0.412621749021023));
#55710=DIRECTION('',(0.0519254248777275,0.66822792587052,0.742142297230154));
#55711=DIRECTION('center_axis',(0.,0.642787609686539,0.766044443118978));
#55712=DIRECTION('ref_axis',(1.,0.,0.));
#55713=DIRECTION('',(0.755033118392644,0.502285118831863,-0.421467257957652));
#55714=DIRECTION('',(1.,0.,0.));
#55715=DIRECTION('',(0.,-0.766044443118978,0.642787609686539));
#55716=DIRECTION('',(0.998052578482888,-0.0477845394804615,0.0400959894540315));
#55717=DIRECTION('',(0.957826285221151,0.220121250980087,-0.184703660511672));
#55718=DIRECTION('',(0.86824314212446,0.3800644767432,-0.318911962258805));
#55719=DIRECTION('',(0.948683298050513,0.242244522917128,-0.203267289834479));
#55720=DIRECTION('',(1.,0.,0.));
#55721=DIRECTION('',(0.948683298050513,-0.242244522917128,0.203267289834478));
#55722=DIRECTION('',(0.868243142124459,-0.380064476743201,0.318911962258806));
#55723=DIRECTION('',(0.957826285221151,-0.220121250980087,0.184703660511673));
#55724=DIRECTION('',(0.998052578482888,0.0477845394804615,-0.0400959894540314));
#55725=DIRECTION('',(0.,0.766044443118978,-0.642787609686539));
#55726=DIRECTION('',(1.,0.,0.));
#55727=DIRECTION('',(0.755033118392644,-0.502285118831862,0.421467257957652));
#55728=DIRECTION('',(-0.755033118392644,-0.502285118831862,0.421467257957652));
#55729=DIRECTION('',(-1.,0.,0.));
#55730=DIRECTION('',(0.,0.766044443118978,-0.642787609686539));
#55731=DIRECTION('',(-0.998052578482888,0.0477845394804615,-0.0400959894540314));
#55732=DIRECTION('',(-0.957826285221151,-0.220121250980087,0.184703660511673));
#55733=DIRECTION('',(-0.868243142124459,-0.380064476743201,0.318911962258806));
#55734=DIRECTION('',(-0.948683298050513,-0.242244522917128,0.203267289834478));
#55735=DIRECTION('',(-1.,0.,0.));
#55736=DIRECTION('',(-0.948683298050513,0.242244522917128,-0.203267289834479));
#55737=DIRECTION('',(-0.86824314212446,0.3800644767432,-0.318911962258805));
#55738=DIRECTION('',(-0.957826285221151,0.220121250980087,-0.184703660511672));
#55739=DIRECTION('',(-0.998052578482888,-0.0477845394804615,0.0400959894540315));
#55740=DIRECTION('',(0.,-0.766044443118978,0.642787609686539));
#55741=DIRECTION('',(-1.,0.,0.));
#55742=DIRECTION('',(-0.755033118392644,0.502285118831863,-0.421467257957652));
#55743=DIRECTION('center_axis',(0.649305557988371,-0.662218828358294,0.373989994161848));
#55744=DIRECTION('ref_axis',(0.755033118392643,0.502285118831863,-0.421467257957652));
#55745=DIRECTION('',(0.,0.491750692698505,0.870736042799734));
#55746=DIRECTION('',(-0.755033118392644,-0.502285118831863,0.421467257957652));
#55747=DIRECTION('center_axis',(-0.649305557988371,0.662218828358294,-0.373989994161848));
#55748=DIRECTION('ref_axis',(0.760527640763576,0.565373752130667,-0.319296457913771));
#55749=DIRECTION('',(0.0519254248777275,0.52920438469299,0.846904049744115));
#55750=DIRECTION('center_axis',(0.,0.5,0.866025403784439));
#55751=DIRECTION('ref_axis',(1.,0.,0.));
#55752=DIRECTION('',(0.755033118392644,0.567841300538901,-0.327843327723122));
#55753=DIRECTION('',(1.,0.,0.));
#55754=DIRECTION('',(0.,-0.866025403784439,0.5));
#55755=DIRECTION('',(0.998052578482888,-0.0540211804549215,0.0311891430775903));
#55756=DIRECTION('',(0.957826285221151,0.248850568624199,-0.143673942783173));
#55757=DIRECTION('',(0.86824314212446,0.429668924423658,-0.248069469178416));
#55758=DIRECTION('',(0.948683298050513,0.273861278752585,-0.15811388300842));
#55759=DIRECTION('',(1.,0.,0.));
#55760=DIRECTION('',(0.948683298050514,-0.273861278752584,0.158113883008419));
#55761=DIRECTION('',(0.868243142124459,-0.429668924423659,0.248069469178417));
#55762=DIRECTION('',(0.957826285221151,-0.248850568624199,0.143673942783173));
#55763=DIRECTION('',(0.998052578482888,0.0540211804549215,-0.0311891430775903));
#55764=DIRECTION('',(0.,0.866025403784439,-0.5));
#55765=DIRECTION('',(1.,0.,0.));
#55766=DIRECTION('',(0.755033118392644,-0.567841300538901,0.327843327723122));
#55767=DIRECTION('',(-0.755033118392644,-0.567841300538901,0.327843327723122));
#55768=DIRECTION('',(-1.,0.,0.));
#55769=DIRECTION('',(0.,0.866025403784439,-0.5));
#55770=DIRECTION('',(-0.998052578482888,0.0540211804549215,-0.0311891430775903));
#55771=DIRECTION('',(-0.957826285221151,-0.248850568624199,0.143673942783173));
#55772=DIRECTION('',(-0.868243142124459,-0.429668924423659,0.248069469178417));
#55773=DIRECTION('',(-0.948683298050514,-0.273861278752584,0.158113883008419));
#55774=DIRECTION('',(-1.,0.,0.));
#55775=DIRECTION('',(-0.948683298050513,0.273861278752585,-0.15811388300842));
#55776=DIRECTION('',(-0.86824314212446,0.429668924423658,-0.248069469178416));
#55777=DIRECTION('',(-0.957826285221151,0.248850568624199,-0.143673942783173));
#55778=DIRECTION('',(-0.998052578482888,-0.0540211804549215,0.0311891430775903));
#55779=DIRECTION('',(0.,-0.866025403784439,0.5));
#55780=DIRECTION('',(-1.,0.,0.));
#55781=DIRECTION('',(-0.755033118392644,0.567841300538901,-0.327843327723122));
#55782=DIRECTION('center_axis',(0.649305557988371,-0.717100917309779,0.253315153038431));
#55783=DIRECTION('ref_axis',(0.755033118392643,0.567841300538901,-0.327843327723122));
#55784=DIRECTION('',(0.,0.333078167657524,0.942899217429894));
#55785=DIRECTION('',(-0.755033118392644,-0.567841300538901,0.327843327723122));
#55786=DIRECTION('center_axis',(-0.649305557988371,0.717100917309779,-0.253315153038431));
#55787=DIRECTION('ref_axis',(0.760527640763576,0.612229702500115,-0.216269505504613));
#55788=DIRECTION('',(0.0519254248777275,0.374101236076903,0.925933051260728));
#55789=DIRECTION('center_axis',(0.,0.342020143325669,0.939692620785908));
#55790=DIRECTION('ref_axis',(1.,0.,0.));
#55791=DIRECTION('',(0.755033118392644,0.616143911670627,-0.224258043872453));
#55792=DIRECTION('',(1.,0.,0.));
#55793=DIRECTION('',(0.,-0.939692620785908,0.342020143325669));
#55794=DIRECTION('',(0.998052578482888,-0.058616415197295,0.0213346303712044));
#55795=DIRECTION('',(0.957826285221151,0.270018687665128,-0.0982787650057293));
#55796=DIRECTION('',(0.86824314212446,0.46621809925847,-0.169689510806249));
#55797=DIRECTION('',(0.948683298050513,0.297156898213637,-0.108156265856636));
#55798=DIRECTION('',(1.,0.,0.));
#55799=DIRECTION('',(0.948683298050514,-0.297156898213636,0.108156265856635));
#55800=DIRECTION('',(0.868243142124459,-0.466218099258471,0.169689510806249));
#55801=DIRECTION('',(0.957826285221151,-0.270018687665129,0.0982787650057295));
#55802=DIRECTION('',(0.998052578482888,0.0586164151972949,-0.0213346303712044));
#55803=DIRECTION('',(0.,0.939692620785908,-0.342020143325669));
#55804=DIRECTION('',(1.,0.,0.));
#55805=DIRECTION('',(0.755033118392644,-0.616143911670627,0.224258043872453));
#55806=DIRECTION('',(-0.755033118392644,-0.616143911670627,0.224258043872453));
#55807=DIRECTION('',(-1.,0.,0.));
#55808=DIRECTION('',(0.,0.939692620785908,-0.342020143325669));
#55809=DIRECTION('',(-0.998052578482888,0.0586164151972949,-0.0213346303712044));
#55810=DIRECTION('',(-0.957826285221151,-0.270018687665129,0.0982787650057295));
#55811=DIRECTION('',(-0.868243142124459,-0.466218099258471,0.169689510806249));
#55812=DIRECTION('',(-0.948683298050514,-0.297156898213636,0.108156265856635));
#55813=DIRECTION('',(-1.,0.,0.));
#55814=DIRECTION('',(-0.948683298050513,0.297156898213637,-0.108156265856636));
#55815=DIRECTION('',(-0.86824314212446,0.46621809925847,-0.169689510806249));
#55816=DIRECTION('',(-0.957826285221151,0.270018687665128,-0.0982787650057293));
#55817=DIRECTION('',(-0.998052578482888,-0.058616415197295,0.0213346303712044));
#55818=DIRECTION('',(0.,-0.939692620785908,0.342020143325669));
#55819=DIRECTION('',(-1.,0.,0.));
#55820=DIRECTION('',(-0.755033118392644,0.616143911670627,-0.224258043872453));
#55821=DIRECTION('center_axis',(0.649305557988371,-0.75019425775938,0.124943459173594));
#55822=DIRECTION('ref_axis',(0.755033118392643,0.616143911670627,-0.224258043872453));
#55823=DIRECTION('',(0.,0.164285231037954,0.986412876468473));
#55824=DIRECTION('',(-0.755033118392644,-0.616143911670627,0.224258043872453));
#55825=DIRECTION('center_axis',(-0.649305557988371,0.75019425775938,-0.124943459173594));
#55826=DIRECTION('ref_axis',(0.760527640763576,0.640483363162275,-0.106671313608347));
#55827=DIRECTION('',(0.0519254248777275,0.207631210706978,0.976828045559515));
#55828=DIRECTION('center_axis',(0.,0.17364817766693,0.984807753012208));
#55829=DIRECTION('ref_axis',(1.,0.,0.));
#55830=DIRECTION('',(0.755033118392643,0.645725301830105,-0.113858792838765));
#55831=DIRECTION('',(1.,0.,0.));
#55832=DIRECTION('',(0.,-0.984807753012208,0.17364817766693));
#55833=DIRECTION('',(0.998052578482888,-0.0614306198252359,0.0108318757168334));
#55834=DIRECTION('',(0.957826285221151,0.282982425517402,-0.0498974366850415));
#55835=DIRECTION('',(0.86824314212446,0.488601473065054,-0.0861536225152694));
#55836=DIRECTION('',(0.948683298050513,0.311423555691114,-0.0549123752965087));
#55837=DIRECTION('',(1.,0.,0.));
#55838=DIRECTION('',(0.948683298050514,-0.311423555691113,0.0549123752965085));
#55839=DIRECTION('',(0.868243142124459,-0.488601473065055,0.0861536225152696));
#55840=DIRECTION('',(0.957826285221151,-0.282982425517402,0.0498974366850416));
#55841=DIRECTION('',(0.998052578482888,0.0614306198252359,-0.0108318757168334));
#55842=DIRECTION('',(0.,0.984807753012208,-0.17364817766693));
#55843=DIRECTION('',(1.,0.,0.));
#55844=DIRECTION('',(0.755033118392644,-0.645725301830105,0.113858792838765));
#55845=DIRECTION('',(-0.755033118392644,-0.645725301830105,0.113858792838765));
#55846=DIRECTION('',(-1.,0.,0.));
#55847=DIRECTION('',(0.,0.984807753012208,-0.17364817766693));
#55848=DIRECTION('',(-0.998052578482888,0.0614306198252359,-0.0108318757168334));
#55849=DIRECTION('',(-0.957826285221151,-0.282982425517402,0.0498974366850416));
#55850=DIRECTION('',(-0.868243142124459,-0.488601473065055,0.0861536225152696));
#55851=DIRECTION('',(-0.948683298050514,-0.311423555691113,0.0549123752965085));
#55852=DIRECTION('',(-1.,0.,0.));
#55853=DIRECTION('',(-0.948683298050513,0.311423555691114,-0.0549123752965087));
#55854=DIRECTION('',(-0.86824314212446,0.488601473065054,-0.0861536225152694));
#55855=DIRECTION('',(-0.957826285221151,0.282982425517402,-0.0498974366850415));
#55856=DIRECTION('',(-0.998052578482888,-0.0614306198252359,0.0108318757168334));
#55857=DIRECTION('',(0.,-0.984807753012208,0.17364817766693));
#55858=DIRECTION('',(-1.,0.,0.));
#55859=DIRECTION('',(-0.755033118392643,0.645725301830105,-0.113858792838765));
#55860=DIRECTION('center_axis',(0.649305557988371,-0.760493325303573,-0.00722457847379221));
#55861=DIRECTION('ref_axis',(0.755033118392643,0.645725301830105,-0.113858792838765));
#55862=DIRECTION('',(0.,-0.00949942919436652,0.999954879404557));
#55863=DIRECTION('',(-0.755033118392643,-0.645725301830105,0.113858792838765));
#55864=DIRECTION('center_axis',(-0.649305557988371,0.760493325303573,0.00722457847379221));
#55865=DIRECTION('ref_axis',(0.760527640763576,0.64927626093497,0.00616803217361917));
#55866=DIRECTION('',(0.0519254248777275,0.0348524160661845,0.998042613992818));
#55867=DIRECTION('center_axis',(0.,6.12323399573677E-17,1.));
#55868=DIRECTION('ref_axis',(1.,0.,0.));
#55869=DIRECTION('',(0.755033118392644,0.655686655446243,-4.01492281917938E-17));
#55870=DIRECTION('',(1.,0.,0.));
#55871=DIRECTION('',(0.,-1.,6.12323399573677E-17));
#55872=DIRECTION('',(0.998052578482888,-0.0623782861551806,3.81956842381198E-18));
#55873=DIRECTION('',(0.957826285221151,0.287347885566345,-1.75949834150292E-17));
#55874=DIRECTION('',(0.86824314212446,0.496138938356832,-3.0379748139553E-17));
#55875=DIRECTION('',(0.948683298050513,0.31622776601684,-1.9363366072702E-17));
#55876=DIRECTION('',(1.,0.,0.));
#55877=DIRECTION('',(0.948683298050514,-0.316227766016839,1.9363366072702E-17));
#55878=DIRECTION('',(0.868243142124459,-0.496138938356833,3.03797481395531E-17));
#55879=DIRECTION('',(0.957826285221151,-0.287347885566346,1.75949834150293E-17));
#55880=DIRECTION('',(0.998052578482888,0.0623782861551805,-3.81956842381197E-18));
#55881=DIRECTION('',(0.,1.,-6.12323399573677E-17));
#55882=DIRECTION('',(1.,0.,0.));
#55883=DIRECTION('',(0.755033118392644,-0.655686655446243,4.01492281917938E-17));
#55884=DIRECTION('',(-0.755033118392644,-0.655686655446243,4.01492281917938E-17));
#55885=DIRECTION('',(-1.,0.,0.));
#55886=DIRECTION('',(0.,1.,-6.12323399573677E-17));
#55887=DIRECTION('',(-0.998052578482888,0.0623782861551805,-3.81956842381197E-18));
#55888=DIRECTION('',(-0.957826285221151,-0.287347885566346,1.75949834150293E-17));
#55889=DIRECTION('',(-0.868243142124459,-0.496138938356833,3.03797481395531E-17));
#55890=DIRECTION('',(-0.948683298050514,-0.316227766016839,1.9363366072702E-17));
#55891=DIRECTION('',(-1.,0.,0.));
#55892=DIRECTION('',(-0.948683298050513,0.31622776601684,-1.9363366072702E-17));
#55893=DIRECTION('',(-0.86824314212446,0.496138938356832,-3.0379748139553E-17));
#55894=DIRECTION('',(-0.957826285221151,0.287347885566345,-1.75949834150292E-17));
#55895=DIRECTION('',(-0.998052578482888,-0.0623782861551806,3.81956842381198E-18));
#55896=DIRECTION('',(0.,-1.,6.12323399573677E-17));
#55897=DIRECTION('',(-1.,0.,0.));
#55898=DIRECTION('',(-0.755033118392644,0.655686655446243,-4.01492281917938E-17));
#55899=DIRECTION('center_axis',(0.649305557988371,-0.747685187986608,-0.139173100960065));
#55900=DIRECTION('ref_axis',(0.755033118392643,0.655686655446243,-4.01492281917938E-17));
#55901=DIRECTION('',(0.,-0.182995454077559,0.983113759331517));
#55902=DIRECTION('',(-0.755033118392644,-0.655686655446243,4.01492281917938E-17));
#55903=DIRECTION('center_axis',(-0.649305557988371,0.747685187986608,0.139173100960065));
#55904=DIRECTION('ref_axis',(0.760527640763576,0.638341228068795,0.118819965419165));
#55905=DIRECTION('',(0.0519254248777275,-0.138985351600607,0.98893216263388));
#55906=DIRECTION('center_axis',(0.,-0.17364817766693,0.984807753012208));
#55907=DIRECTION('ref_axis',(1.,0.,0.));
#55908=DIRECTION('',(0.755033118392643,0.645725301830105,0.113858792838765));
#55909=DIRECTION('',(1.,0.,0.));
#55910=DIRECTION('',(0.,-0.984807753012208,-0.17364817766693));
#55911=DIRECTION('',(0.998052578482888,-0.0614306198252359,-0.0108318757168334));
#55912=DIRECTION('',(0.957826285221151,0.282982425517402,0.0498974366850415));
#55913=DIRECTION('',(0.86824314212446,0.488601473065054,0.0861536225152694));
#55914=DIRECTION('',(0.948683298050513,0.311423555691114,0.0549123752965087));
#55915=DIRECTION('',(1.,0.,0.));
#55916=DIRECTION('',(0.948683298050514,-0.311423555691113,-0.0549123752965085));
#55917=DIRECTION('',(0.868243142124459,-0.488601473065055,-0.0861536225152696));
#55918=DIRECTION('',(0.957826285221151,-0.282982425517402,-0.0498974366850416));
#55919=DIRECTION('',(0.998052578482888,0.0614306198252359,0.0108318757168334));
#55920=DIRECTION('',(0.,0.984807753012208,0.17364817766693));
#55921=DIRECTION('',(1.,0.,0.));
#55922=DIRECTION('',(0.755033118392644,-0.645725301830105,-0.113858792838765));
#55923=DIRECTION('',(-0.755033118392644,-0.645725301830105,-0.113858792838765));
#55924=DIRECTION('',(-1.,0.,0.));
#55925=DIRECTION('',(0.,0.984807753012208,0.17364817766693));
#55926=DIRECTION('',(-0.998052578482888,0.0614306198252359,0.0108318757168334));
#55927=DIRECTION('',(-0.957826285221151,-0.282982425517402,-0.0498974366850416));
#55928=DIRECTION('',(-0.868243142124459,-0.488601473065055,-0.0861536225152696));
#55929=DIRECTION('',(-0.948683298050514,-0.311423555691113,-0.0549123752965085));
#55930=DIRECTION('',(-1.,0.,0.));
#55931=DIRECTION('',(-0.948683298050513,0.311423555691114,0.0549123752965087));
#55932=DIRECTION('',(-0.86824314212446,0.488601473065054,0.0861536225152694));
#55933=DIRECTION('',(-0.957826285221151,0.282982425517402,0.0498974366850415));
#55934=DIRECTION('',(-0.998052578482888,-0.0614306198252359,-0.0108318757168334));
#55935=DIRECTION('',(0.,-0.984807753012208,-0.17364817766693));
#55936=DIRECTION('',(-1.,0.,0.));
#55937=DIRECTION('',(-0.755033118392643,0.645725301830105,0.113858792838765));
#55938=DIRECTION('center_axis',(0.649305557988371,-0.712159014579631,-0.266892919198654));
#55939=DIRECTION('ref_axis',(0.755033118392643,0.645725301830105,0.113858792838765));
#55940=DIRECTION('',(0.,-0.350931254688773,0.936401225160756));
#55941=DIRECTION('',(-0.755033118392643,-0.645725301830105,-0.113858792838765));
#55942=DIRECTION('center_axis',(-0.649305557988371,0.712159014579631,0.266892919198654));
#55943=DIRECTION('ref_axis',(0.760527640763576,0.608010520003998,0.227861614141253));
#55944=DIRECTION('',(0.0519254248777275,-0.308600119688995,0.949773507937132));
#55945=DIRECTION('center_axis',(0.,-0.342020143325669,0.939692620785908));
#55946=DIRECTION('ref_axis',(1.,0.,0.));
#55947=DIRECTION('',(0.755033118392644,0.616143911670627,0.224258043872452));
#55948=DIRECTION('',(1.,0.,0.));
#55949=DIRECTION('',(0.,-0.939692620785908,-0.342020143325669));
#55950=DIRECTION('',(0.998052578482888,-0.058616415197295,-0.0213346303712044));
#55951=DIRECTION('',(0.957826285221151,0.270018687665128,0.0982787650057293));
#55952=DIRECTION('',(0.86824314212446,0.46621809925847,0.169689510806249));
#55953=DIRECTION('',(0.948683298050513,0.297156898213637,0.108156265856636));
#55954=DIRECTION('',(1.,0.,0.));
#55955=DIRECTION('',(0.948683298050514,-0.297156898213636,-0.108156265856635));
#55956=DIRECTION('',(0.868243142124459,-0.466218099258471,-0.169689510806249));
#55957=DIRECTION('',(0.957826285221151,-0.270018687665129,-0.0982787650057295));
#55958=DIRECTION('',(0.998052578482888,0.0586164151972949,0.0213346303712044));
#55959=DIRECTION('',(0.,0.939692620785908,0.342020143325669));
#55960=DIRECTION('',(1.,0.,0.));
#55961=DIRECTION('',(0.755033118392644,-0.616143911670627,-0.224258043872452));
#55962=DIRECTION('',(-0.755033118392644,-0.616143911670627,-0.224258043872452));
#55963=DIRECTION('',(-1.,0.,0.));
#55964=DIRECTION('',(0.,0.939692620785908,0.342020143325669));
#55965=DIRECTION('',(-0.998052578482888,0.0586164151972949,0.0213346303712044));
#55966=DIRECTION('',(-0.957826285221151,-0.270018687665129,-0.0982787650057295));
#55967=DIRECTION('',(-0.868243142124459,-0.466218099258471,-0.169689510806249));
#55968=DIRECTION('',(-0.948683298050514,-0.297156898213636,-0.108156265856635));
#55969=DIRECTION('',(-1.,0.,0.));
#55970=DIRECTION('',(-0.948683298050513,0.297156898213637,0.108156265856636));
#55971=DIRECTION('',(-0.86824314212446,0.46621809925847,0.169689510806249));
#55972=DIRECTION('',(-0.957826285221151,0.270018687665128,0.0982787650057293));
#55973=DIRECTION('',(-0.998052578482888,-0.058616415197295,-0.0213346303712044));
#55974=DIRECTION('',(0.,-0.939692620785908,-0.342020143325669));
#55975=DIRECTION('',(-1.,0.,0.));
#55976=DIRECTION('',(-0.755033118392644,0.616143911670627,0.224258043872452));
#55977=DIRECTION('center_axis',(0.649305557988371,-0.654994249884502,-0.386503331141725));
#55978=DIRECTION('ref_axis',(0.755033118392643,0.616143911670627,0.224258043872452));
#55979=DIRECTION('',(0.,-0.508204186706051,0.861236613605368));
#55980=DIRECTION('',(-0.755033118392644,-0.616143911670627,-0.224258043872452));
#55981=DIRECTION('center_axis',(-0.649305557988371,0.654994249884502,0.386503331141725));
#55982=DIRECTION('ref_axis',(0.760527640763576,0.559205719957048,0.329979803021199));
#55983=DIRECTION('',(0.0519254248777275,-0.468838229299828,0.881756465810299));
#55984=DIRECTION('center_axis',(0.,-0.5,0.866025403784439));
#55985=DIRECTION('ref_axis',(1.,0.,0.));
#55986=DIRECTION('',(0.755033118392644,0.567841300538901,0.327843327723121));
#55987=DIRECTION('',(1.,0.,0.));
#55988=DIRECTION('',(0.,-0.866025403784439,-0.5));
#55989=DIRECTION('',(0.998052578482888,-0.0540211804549215,-0.0311891430775903));
#55990=DIRECTION('',(0.957826285221151,0.248850568624199,0.143673942783173));
#55991=DIRECTION('',(0.86824314212446,0.429668924423658,0.248069469178416));
#55992=DIRECTION('',(0.948683298050513,0.273861278752585,0.15811388300842));
#55993=DIRECTION('',(1.,0.,0.));
#55994=DIRECTION('',(0.948683298050513,-0.273861278752584,-0.158113883008419));
#55995=DIRECTION('',(0.868243142124459,-0.429668924423659,-0.248069469178417));
#55996=DIRECTION('',(0.957826285221151,-0.248850568624199,-0.143673942783173));
#55997=DIRECTION('',(0.998052578482888,0.0540211804549215,0.0311891430775902));
#55998=DIRECTION('',(0.,0.866025403784439,0.5));
#55999=DIRECTION('',(1.,0.,0.));
#56000=DIRECTION('',(0.755033118392644,-0.567841300538901,-0.327843327723121));
#56001=DIRECTION('',(-0.755033118392644,-0.567841300538901,-0.327843327723121));
#56002=DIRECTION('',(-1.,0.,0.));
#56003=DIRECTION('',(0.,0.866025403784439,0.5));
#56004=DIRECTION('',(-0.998052578482888,0.0540211804549215,0.0311891430775902));
#56005=DIRECTION('',(-0.957826285221151,-0.248850568624199,-0.143673942783173));
#56006=DIRECTION('',(-0.868243142124459,-0.429668924423659,-0.248069469178417));
#56007=DIRECTION('',(-0.948683298050513,-0.273861278752584,-0.158113883008419));
#56008=DIRECTION('',(-1.,0.,0.));
#56009=DIRECTION('',(-0.948683298050513,0.273861278752585,0.15811388300842));
#56010=DIRECTION('',(-0.86824314212446,0.429668924423658,0.248069469178416));
#56011=DIRECTION('',(-0.957826285221151,0.248850568624199,0.143673942783173));
#56012=DIRECTION('',(-0.998052578482888,-0.0540211804549215,-0.0311891430775903));
#56013=DIRECTION('',(0.,-0.866025403784439,-0.5));
#56014=DIRECTION('',(-1.,0.,0.));
#56015=DIRECTION('',(-0.755033118392644,0.567841300538901,0.327843327723121));
#56016=DIRECTION('center_axis',(0.649305557988371,-0.577927816349714,-0.494370034948177));
#56017=DIRECTION('ref_axis',(0.755033118392643,0.567841300538901,0.327843327723121));
#56018=DIRECTION('',(0.,-0.650035591673993,0.759903763352335));
#56019=DIRECTION('',(-0.755033118392644,-0.567841300538901,-0.327843327723121));
#56020=DIRECTION('center_axis',(-0.649305557988371,0.577927816349714,0.494370034948177));
#56021=DIRECTION('ref_axis',(0.760527640763576,0.493409737080951,0.422071722564183));
#56022=DIRECTION('',(0.0519254248777275,-0.614830926556978,0.786947699660121));
#56023=DIRECTION('center_axis',(0.,-0.642787609686539,0.766044443118978));
#56024=DIRECTION('ref_axis',(1.,0.,0.));
#56025=DIRECTION('',(0.755033118392644,0.502285118831863,0.421467257957652));
#56026=DIRECTION('',(1.,0.,0.));
#56027=DIRECTION('',(0.,-0.766044443118978,-0.642787609686539));
#56028=DIRECTION('',(0.998052578482888,-0.0477845394804615,-0.0400959894540315));
#56029=DIRECTION('',(0.957826285221151,0.220121250980087,0.184703660511672));
#56030=DIRECTION('',(0.86824314212446,0.3800644767432,0.318911962258805));
#56031=DIRECTION('',(0.948683298050513,0.242244522917128,0.203267289834479));
#56032=DIRECTION('',(1.,0.,0.));
#56033=DIRECTION('',(0.948683298050513,-0.242244522917128,-0.203267289834478));
#56034=DIRECTION('',(0.868243142124459,-0.380064476743201,-0.318911962258806));
#56035=DIRECTION('',(0.957826285221151,-0.220121250980087,-0.184703660511673));
#56036=DIRECTION('',(0.998052578482888,0.0477845394804615,0.0400959894540314));
#56037=DIRECTION('',(0.,0.766044443118978,0.642787609686539));
#56038=DIRECTION('',(1.,0.,0.));
#56039=DIRECTION('',(0.755033118392644,-0.502285118831862,-0.421467257957652));
#56040=DIRECTION('',(-0.755033118392644,-0.502285118831862,-0.421467257957652));
#56041=DIRECTION('',(-1.,0.,0.));
#56042=DIRECTION('',(0.,0.766044443118978,0.642787609686539));
#56043=DIRECTION('',(-0.998052578482888,0.0477845394804615,0.0400959894540314));
#56044=DIRECTION('',(-0.957826285221151,-0.220121250980087,-0.184703660511673));
#56045=DIRECTION('',(-0.868243142124459,-0.380064476743201,-0.318911962258806));
#56046=DIRECTION('',(-0.948683298050513,-0.242244522917128,-0.203267289834478));
#56047=DIRECTION('',(-1.,0.,0.));
#56048=DIRECTION('',(-0.948683298050513,0.242244522917128,0.203267289834479));
#56049=DIRECTION('',(-0.86824314212446,0.3800644767432,0.318911962258805));
#56050=DIRECTION('',(-0.957826285221151,0.220121250980087,0.184703660511672));
#56051=DIRECTION('',(-0.998052578482888,-0.0477845394804615,-0.0400959894540315));
#56052=DIRECTION('',(0.,-0.766044443118978,-0.642787609686539));
#56053=DIRECTION('',(-1.,0.,0.));
#56054=DIRECTION('',(-0.755033118392644,0.502285118831863,0.421467257957652));
#56055=DIRECTION('center_axis',(0.649305557988371,-0.483301338560726,-0.587215555406037));
#56056=DIRECTION('ref_axis',(0.755033118392643,0.502285118831863,0.421467257957652));
#56057=DIRECTION('',(0.,-0.772115994122802,0.6354816217797));
#56058=DIRECTION('',(-0.755033118392644,-0.502285118831863,-0.421467257957652));
#56059=DIRECTION('center_axis',(-0.649305557988371,0.483301338560726,0.587215555406037));
#56060=DIRECTION('ref_axis',(0.760527640763576,0.412621749021023,0.501339206395652));
#56061=DIRECTION('',(0.0519254248777275,-0.742142297230154,0.66822792587052));
#56062=DIRECTION('center_axis',(0.,-0.766044443118978,0.642787609686539));
#56063=DIRECTION('ref_axis',(1.,0.,0.));
#56064=DIRECTION('',(0.755033118392644,0.421467257957652,0.502285118831862));
#56065=DIRECTION('',(1.,0.,0.));
#56066=DIRECTION('',(0.,-0.642787609686539,-0.766044443118978));
#56067=DIRECTION('',(0.998052578482888,-0.0400959894540315,-0.0477845394804615));
#56068=DIRECTION('',(0.957826285221151,0.184703660511672,0.220121250980087));
#56069=DIRECTION('',(0.86824314212446,0.318911962258805,0.3800644767432));
#56070=DIRECTION('',(0.948683298050513,0.203267289834479,0.242244522917128));
#56071=DIRECTION('',(1.,0.,0.));
#56072=DIRECTION('',(0.948683298050514,-0.203267289834478,-0.242244522917128));
#56073=DIRECTION('',(0.868243142124459,-0.318911962258806,-0.380064476743201));
#56074=DIRECTION('',(0.957826285221151,-0.184703660511673,-0.220121250980087));
#56075=DIRECTION('',(0.998052578482888,0.0400959894540314,0.0477845394804615));
#56076=DIRECTION('',(0.,0.642787609686539,0.766044443118978));
#56077=DIRECTION('',(1.,0.,0.));
#56078=DIRECTION('',(0.755033118392644,-0.421467257957652,-0.502285118831862));
#56079=DIRECTION('',(-0.755033118392644,-0.421467257957652,-0.502285118831862));
#56080=DIRECTION('',(-1.,0.,0.));
#56081=DIRECTION('',(0.,0.642787609686539,0.766044443118978));
#56082=DIRECTION('',(-0.998052578482888,0.0400959894540314,0.0477845394804615));
#56083=DIRECTION('',(-0.957826285221151,-0.184703660511673,-0.220121250980087));
#56084=DIRECTION('',(-0.868243142124459,-0.318911962258806,-0.380064476743201));
#56085=DIRECTION('',(-0.948683298050514,-0.203267289834478,-0.242244522917128));
#56086=DIRECTION('',(-1.,0.,0.));
#56087=DIRECTION('',(-0.948683298050513,0.203267289834479,0.242244522917128));
#56088=DIRECTION('',(-0.86824314212446,0.318911962258805,0.3800644767432));
#56089=DIRECTION('',(-0.957826285221151,0.184703660511672,0.220121250980087));
#56090=DIRECTION('',(-0.998052578482888,-0.0400959894540315,-0.0477845394804615));
#56091=DIRECTION('',(0.,-0.642787609686539,-0.766044443118978));
#56092=DIRECTION('',(-1.,0.,0.));
#56093=DIRECTION('',(-0.755033118392644,0.421467257957652,0.502285118831862));
#56094=DIRECTION('center_axis',(0.649305557988371,-0.373989994161848,-0.662218828358294));
#56095=DIRECTION('ref_axis',(0.755033118392644,0.421467257957652,0.502285118831862));
#56096=DIRECTION('',(0.,-0.870736042799734,0.491750692698505));
#56097=DIRECTION('',(-0.755033118392644,-0.421467257957652,-0.502285118831862));
#56098=DIRECTION('center_axis',(-0.649305557988371,0.373989994161848,0.662218828358294));
#56099=DIRECTION('ref_axis',(0.760527640763576,0.319296457913771,0.565373752130667));
#56100=DIRECTION('',(0.0519254248777275,-0.846904049744115,0.52920438469299));
#56101=DIRECTION('center_axis',(0.,-0.866025403784439,0.5));
#56102=DIRECTION('ref_axis',(1.,0.,0.));
#56103=DIRECTION('',(0.755033118392644,0.327843327723122,0.567841300538901));
#56104=DIRECTION('',(1.,0.,0.));
#56105=DIRECTION('',(0.,-0.5,-0.866025403784439));
#56106=DIRECTION('',(0.998052578482888,-0.0311891430775903,-0.0540211804549215));
#56107=DIRECTION('',(0.957826285221151,0.143673942783173,0.248850568624199));
#56108=DIRECTION('',(0.86824314212446,0.248069469178416,0.429668924423658));
#56109=DIRECTION('',(0.948683298050513,0.15811388300842,0.273861278752585));
#56110=DIRECTION('',(1.,0.,0.));
#56111=DIRECTION('',(0.948683298050514,-0.158113883008419,-0.273861278752584));
#56112=DIRECTION('',(0.868243142124459,-0.248069469178417,-0.429668924423659));
#56113=DIRECTION('',(0.957826285221151,-0.143673942783173,-0.248850568624199));
#56114=DIRECTION('',(0.998052578482888,0.0311891430775903,0.0540211804549215));
#56115=DIRECTION('',(0.,0.5,0.866025403784439));
#56116=DIRECTION('',(1.,0.,0.));
#56117=DIRECTION('',(0.755033118392644,-0.327843327723121,-0.567841300538901));
#56118=DIRECTION('',(-0.755033118392644,-0.327843327723121,-0.567841300538901));
#56119=DIRECTION('',(-1.,0.,0.));
#56120=DIRECTION('',(0.,0.5,0.866025403784439));
#56121=DIRECTION('',(-0.998052578482888,0.0311891430775903,0.0540211804549215));
#56122=DIRECTION('',(-0.957826285221151,-0.143673942783173,-0.248850568624199));
#56123=DIRECTION('',(-0.868243142124459,-0.248069469178417,-0.429668924423659));
#56124=DIRECTION('',(-0.948683298050514,-0.158113883008419,-0.273861278752584));
#56125=DIRECTION('',(-1.,0.,0.));
#56126=DIRECTION('',(-0.948683298050513,0.15811388300842,0.273861278752585));
#56127=DIRECTION('',(-0.86824314212446,0.248069469178416,0.429668924423658));
#56128=DIRECTION('',(-0.957826285221151,0.143673942783173,0.248850568624199));
#56129=DIRECTION('',(-0.998052578482888,-0.0311891430775903,-0.0540211804549215));
#56130=DIRECTION('',(0.,-0.5,-0.866025403784439));
#56131=DIRECTION('',(-1.,0.,0.));
#56132=DIRECTION('',(-0.755033118392644,0.327843327723122,0.567841300538901));
#56133=DIRECTION('center_axis',(0.649305557988371,-0.253315153038431,-0.717100917309779));
#56134=DIRECTION('ref_axis',(0.755033118392643,0.327843327723122,0.567841300538901));
#56135=DIRECTION('',(0.,-0.942899217429894,0.333078167657524));
#56136=DIRECTION('',(-0.755033118392644,-0.327843327723122,-0.567841300538901));
#56137=DIRECTION('center_axis',(-0.649305557988371,0.253315153038431,0.717100917309779));
#56138=DIRECTION('ref_axis',(0.760527640763576,0.216269505504613,0.612229702500115));
#56139=DIRECTION('',(0.0519254248777275,-0.925933051260728,0.374101236076902));
#56140=DIRECTION('center_axis',(0.,-0.939692620785908,0.342020143325669));
#56141=DIRECTION('ref_axis',(1.,0.,0.));
#56142=DIRECTION('',(0.755033118392643,0.224258043872453,0.616143911670627));
#56143=DIRECTION('',(1.,0.,0.));
#56144=DIRECTION('',(0.,-0.342020143325669,-0.939692620785908));
#56145=DIRECTION('',(0.998052578482888,-0.0213346303712044,-0.058616415197295));
#56146=DIRECTION('',(0.957826285221151,0.0982787650057294,0.270018687665128));
#56147=DIRECTION('',(0.86824314212446,0.169689510806249,0.46621809925847));
#56148=DIRECTION('',(0.948683298050513,0.108156265856636,0.297156898213637));
#56149=DIRECTION('',(1.,0.,0.));
#56150=DIRECTION('',(0.948683298050514,-0.108156265856635,-0.297156898213636));
#56151=DIRECTION('',(0.868243142124459,-0.169689510806249,-0.466218099258471));
#56152=DIRECTION('',(0.957826285221151,-0.0982787650057295,-0.270018687665129));
#56153=DIRECTION('',(0.998052578482888,0.0213346303712044,0.0586164151972949));
#56154=DIRECTION('',(0.,0.342020143325669,0.939692620785908));
#56155=DIRECTION('',(1.,0.,0.));
#56156=DIRECTION('',(0.755033118392644,-0.224258043872452,-0.616143911670627));
#56157=DIRECTION('',(-0.755033118392644,-0.224258043872452,-0.616143911670627));
#56158=DIRECTION('',(-1.,0.,0.));
#56159=DIRECTION('',(0.,0.342020143325669,0.939692620785908));
#56160=DIRECTION('',(-0.998052578482888,0.0213346303712044,0.0586164151972949));
#56161=DIRECTION('',(-0.957826285221151,-0.0982787650057295,-0.270018687665129));
#56162=DIRECTION('',(-0.868243142124459,-0.169689510806249,-0.466218099258471));
#56163=DIRECTION('',(-0.948683298050514,-0.108156265856635,-0.297156898213636));
#56164=DIRECTION('',(-1.,0.,0.));
#56165=DIRECTION('',(-0.948683298050513,0.108156265856636,0.297156898213637));
#56166=DIRECTION('',(-0.86824314212446,0.169689510806249,0.46621809925847));
#56167=DIRECTION('',(-0.957826285221151,0.0982787650057294,0.270018687665128));
#56168=DIRECTION('',(-0.998052578482888,-0.0213346303712044,-0.058616415197295));
#56169=DIRECTION('',(0.,-0.342020143325669,-0.939692620785908));
#56170=DIRECTION('',(-1.,0.,0.));
#56171=DIRECTION('',(-0.755033118392643,0.224258043872453,0.616143911670627));
#56172=DIRECTION('center_axis',(0.649305557988371,-0.124943459173594,-0.75019425775938));
#56173=DIRECTION('ref_axis',(0.755033118392643,0.224258043872453,0.616143911670627));
#56174=DIRECTION('',(0.,-0.986412876468473,0.164285231037954));
#56175=DIRECTION('',(-0.755033118392643,-0.224258043872453,-0.616143911670627));
#56176=DIRECTION('center_axis',(-0.649305557988371,0.124943459173594,0.75019425775938));
#56177=DIRECTION('ref_axis',(0.760527640763576,0.106671313608347,0.640483363162275));
#56178=DIRECTION('',(0.0519254248777275,-0.976828045559515,0.207631210706978));
#56179=DIRECTION('center_axis',(0.,-0.984807753012208,0.173648177666931));
#56180=DIRECTION('ref_axis',(1.,0.,0.));
#56181=DIRECTION('',(0.755033118392644,0.113858792838765,0.645725301830105));
#56182=DIRECTION('',(1.,0.,0.));
#56183=DIRECTION('',(0.,-0.173648177666931,-0.984807753012208));
#56184=DIRECTION('',(0.998052578482888,-0.0108318757168334,-0.0614306198252359));
#56185=DIRECTION('',(0.957826285221151,0.0498974366850416,0.282982425517402));
#56186=DIRECTION('',(0.86824314212446,0.0861536225152695,0.488601473065054));
#56187=DIRECTION('',(0.948683298050513,0.0549123752965088,0.311423555691114));
#56188=DIRECTION('',(1.,0.,0.));
#56189=DIRECTION('',(0.948683298050514,-0.0549123752965086,-0.311423555691113));
#56190=DIRECTION('',(0.868243142124459,-0.0861536225152698,-0.488601473065055));
#56191=DIRECTION('',(0.957826285221151,-0.0498974366850417,-0.282982425517402));
#56192=DIRECTION('',(0.998052578482888,0.0108318757168334,0.0614306198252358));
#56193=DIRECTION('',(0.,0.173648177666931,0.984807753012208));
#56194=DIRECTION('',(1.,0.,0.));
#56195=DIRECTION('',(0.755033118392644,-0.113858792838765,-0.645725301830104));
#56196=DIRECTION('',(-0.755033118392644,-0.113858792838765,-0.645725301830104));
#56197=DIRECTION('',(-1.,0.,0.));
#56198=DIRECTION('',(0.,0.173648177666931,0.984807753012208));
#56199=DIRECTION('',(-0.998052578482888,0.0108318757168334,0.0614306198252358));
#56200=DIRECTION('',(-0.957826285221151,-0.0498974366850417,-0.282982425517402));
#56201=DIRECTION('',(-0.868243142124459,-0.0861536225152698,-0.488601473065055));
#56202=DIRECTION('',(-0.948683298050514,-0.0549123752965086,-0.311423555691113));
#56203=DIRECTION('',(-1.,0.,0.));
#56204=DIRECTION('',(-0.948683298050513,0.0549123752965088,0.311423555691114));
#56205=DIRECTION('',(-0.86824314212446,0.0861536225152695,0.488601473065054));
#56206=DIRECTION('',(-0.957826285221151,0.0498974366850416,0.282982425517402));
#56207=DIRECTION('',(-0.998052578482888,-0.0108318757168334,-0.0614306198252359));
#56208=DIRECTION('',(0.,-0.173648177666931,-0.984807753012208));
#56209=DIRECTION('',(-1.,0.,0.));
#56210=DIRECTION('',(-0.755033118392644,0.113858792838765,0.645725301830105));
#56211=DIRECTION('center_axis',(0.649305557988371,0.00722457847379199,-0.760493325303573));
#56212=DIRECTION('ref_axis',(0.755033118392643,0.113858792838765,0.645725301830105));
#56213=DIRECTION('',(0.,-0.999954879404557,-0.00949942919436624));
#56214=DIRECTION('',(-0.755033118392644,-0.113858792838765,-0.645725301830105));
#56215=DIRECTION('center_axis',(-0.649305557988371,-0.00722457847379199,
0.760493325303573));
#56216=DIRECTION('ref_axis',(-0.760527640763576,0.00616803217361895,-0.64927626093497));
#56217=DIRECTION('',(0.0519254248777275,-0.998042613992818,0.0348524160661848));
#56218=DIRECTION('center_axis',(0.,-1.,1.22464679914735E-16));
#56219=DIRECTION('ref_axis',(1.,0.,0.));
#56220=DIRECTION('',(0.755033118392644,8.02984563835875E-17,0.655686655446243));
#56221=DIRECTION('',(1.,0.,0.));
#56222=DIRECTION('',(0.,-1.22464679914735E-16,-1.));
#56223=DIRECTION('',(0.998052578482888,-7.63913684762395E-18,-0.0623782861551806));
#56224=DIRECTION('',(0.957826285221151,3.51899668300585E-17,0.287347885566345));
#56225=DIRECTION('',(0.86824314212446,6.0759496279106E-17,0.496138938356832));
#56226=DIRECTION('',(0.948683298050513,3.87267321454041E-17,0.31622776601684));
#56227=DIRECTION('',(1.,0.,0.));
#56228=DIRECTION('',(0.948683298050514,-3.8726732145404E-17,-0.316227766016839));
#56229=DIRECTION('',(0.868243142124459,-6.07594962791062E-17,-0.496138938356833));
#56230=DIRECTION('',(0.957826285221151,-3.51899668300585E-17,-0.287347885566346));
#56231=DIRECTION('',(0.998052578482888,7.63913684762395E-18,0.0623782861551805));
#56232=DIRECTION('',(0.,1.22464679914735E-16,1.));
#56233=DIRECTION('',(1.,0.,0.));
#56234=DIRECTION('',(0.755033118392644,-8.02984563835875E-17,-0.655686655446243));
#56235=DIRECTION('',(-0.755033118392644,-8.02984563835875E-17,-0.655686655446243));
#56236=DIRECTION('',(-1.,0.,0.));
#56237=DIRECTION('',(0.,1.22464679914735E-16,1.));
#56238=DIRECTION('',(-0.998052578482888,7.63913684762395E-18,0.0623782861551805));
#56239=DIRECTION('',(-0.957826285221151,-3.51899668300585E-17,-0.287347885566346));
#56240=DIRECTION('',(-0.868243142124459,-6.07594962791062E-17,-0.496138938356833));
#56241=DIRECTION('',(-0.948683298050514,-3.8726732145404E-17,-0.316227766016839));
#56242=DIRECTION('',(-1.,0.,0.));
#56243=DIRECTION('',(-0.948683298050513,3.87267321454041E-17,0.31622776601684));
#56244=DIRECTION('',(-0.86824314212446,6.0759496279106E-17,0.496138938356832));
#56245=DIRECTION('',(-0.957826285221151,3.51899668300585E-17,0.287347885566345));
#56246=DIRECTION('',(-0.998052578482888,-7.63913684762395E-18,-0.0623782861551806));
#56247=DIRECTION('',(0.,-1.22464679914735E-16,-1.));
#56248=DIRECTION('',(-1.,0.,0.));
#56249=DIRECTION('',(-0.755033118392644,8.02984563835875E-17,0.655686655446243));
#56250=DIRECTION('center_axis',(0.649305557988371,0.139173100960065,-0.747685187986608));
#56251=DIRECTION('ref_axis',(0.755033118392643,8.02984563835875E-17,0.655686655446243));
#56252=DIRECTION('',(0.,-0.983113759331517,-0.182995454077559));
#56253=DIRECTION('',(-0.755033118392644,-8.02984563835875E-17,-0.655686655446243));
#56254=DIRECTION('center_axis',(-0.649305557988371,-0.139173100960065,0.747685187986608));
#56255=DIRECTION('ref_axis',(-0.760527640763576,0.118819965419165,-0.638341228068795));
#56256=DIRECTION('',(0.0519254248777275,-0.98893216263388,-0.138985351600607));
#56257=DIRECTION('center_axis',(0.,-0.984807753012208,-0.17364817766693));
#56258=DIRECTION('ref_axis',(1.,0.,0.));
#56259=DIRECTION('',(0.755033118392643,-0.113858792838764,0.645725301830105));
#56260=DIRECTION('',(1.,0.,0.));
#56261=DIRECTION('',(0.,0.17364817766693,-0.984807753012208));
#56262=DIRECTION('',(0.998052578482888,0.0108318757168334,-0.0614306198252359));
#56263=DIRECTION('',(0.957826285221151,-0.0498974366850414,0.282982425517402));
#56264=DIRECTION('',(0.86824314212446,-0.0861536225152693,0.488601473065054));
#56265=DIRECTION('',(0.948683298050513,-0.0549123752965086,0.311423555691114));
#56266=DIRECTION('',(1.,0.,0.));
#56267=DIRECTION('',(0.948683298050514,0.0549123752965084,-0.311423555691113));
#56268=DIRECTION('',(0.868243142124459,0.0861536225152694,-0.488601473065055));
#56269=DIRECTION('',(0.957826285221151,0.0498974366850415,-0.282982425517402));
#56270=DIRECTION('',(0.998052578482888,-0.0108318757168334,0.0614306198252359));
#56271=DIRECTION('',(0.,-0.17364817766693,0.984807753012208));
#56272=DIRECTION('',(1.,0.,0.));
#56273=DIRECTION('',(0.755033118392644,0.113858792838764,-0.645725301830105));
#56274=DIRECTION('',(-0.755033118392644,0.113858792838764,-0.645725301830105));
#56275=DIRECTION('',(-1.,0.,0.));
#56276=DIRECTION('',(0.,-0.17364817766693,0.984807753012208));
#56277=DIRECTION('',(-0.998052578482888,-0.0108318757168334,0.0614306198252359));
#56278=DIRECTION('',(-0.957826285221151,0.0498974366850415,-0.282982425517402));
#56279=DIRECTION('',(-0.868243142124459,0.0861536225152694,-0.488601473065055));
#56280=DIRECTION('',(-0.948683298050514,0.0549123752965084,-0.311423555691113));
#56281=DIRECTION('',(-1.,0.,0.));
#56282=DIRECTION('',(-0.948683298050513,-0.0549123752965086,0.311423555691114));
#56283=DIRECTION('',(-0.86824314212446,-0.0861536225152693,0.488601473065054));
#56284=DIRECTION('',(-0.957826285221151,-0.0498974366850414,0.282982425517402));
#56285=DIRECTION('',(-0.998052578482888,0.0108318757168334,-0.0614306198252359));
#56286=DIRECTION('',(0.,0.17364817766693,-0.984807753012208));
#56287=DIRECTION('',(-1.,0.,0.));
#56288=DIRECTION('',(-0.755033118392643,-0.113858792838764,0.645725301830105));
#56289=DIRECTION('center_axis',(0.649305557988371,0.266892919198654,-0.712159014579631));
#56290=DIRECTION('ref_axis',(0.755033118392643,-0.113858792838764,0.645725301830105));
#56291=DIRECTION('',(0.,-0.936401225160756,-0.350931254688773));
#56292=DIRECTION('',(-0.755033118392643,0.113858792838764,-0.645725301830105));
#56293=DIRECTION('center_axis',(-0.649305557988371,-0.266892919198654,0.712159014579631));
#56294=DIRECTION('ref_axis',(-0.760527640763576,0.227861614141253,-0.608010520003998));
#56295=DIRECTION('',(0.0519254248777275,-0.949773507937132,-0.308600119688995));
#56296=DIRECTION('center_axis',(0.,-0.939692620785908,-0.342020143325669));
#56297=DIRECTION('ref_axis',(1.,0.,0.));
#56298=DIRECTION('',(0.755033118392644,-0.224258043872452,0.616143911670627));
#56299=DIRECTION('',(1.,0.,0.));
#56300=DIRECTION('',(0.,0.342020143325669,-0.939692620785909));
#56301=DIRECTION('',(0.998052578482888,0.0213346303712044,-0.058616415197295));
#56302=DIRECTION('',(0.957826285221151,-0.0982787650057293,0.270018687665128));
#56303=DIRECTION('',(0.86824314212446,-0.169689510806249,0.46621809925847));
#56304=DIRECTION('',(0.948683298050513,-0.108156265856636,0.297156898213637));
#56305=DIRECTION('',(1.,0.,0.));
#56306=DIRECTION('',(0.948683298050514,0.108156265856635,-0.297156898213636));
#56307=DIRECTION('',(0.868243142124459,0.169689510806249,-0.466218099258471));
#56308=DIRECTION('',(0.957826285221151,0.0982787650057294,-0.270018687665129));
#56309=DIRECTION('',(0.998052578482888,-0.0213346303712044,0.0586164151972949));
#56310=DIRECTION('',(0.,-0.342020143325669,0.939692620785909));
#56311=DIRECTION('',(1.,0.,0.));
#56312=DIRECTION('',(0.755033118392644,0.224258043872452,-0.616143911670627));
#56313=DIRECTION('',(-0.755033118392644,0.224258043872452,-0.616143911670627));
#56314=DIRECTION('',(-1.,0.,0.));
#56315=DIRECTION('',(0.,-0.342020143325669,0.939692620785909));
#56316=DIRECTION('',(-0.998052578482888,-0.0213346303712044,0.0586164151972949));
#56317=DIRECTION('',(-0.957826285221151,0.0982787650057294,-0.270018687665129));
#56318=DIRECTION('',(-0.868243142124459,0.169689510806249,-0.466218099258471));
#56319=DIRECTION('',(-0.948683298050514,0.108156265856635,-0.297156898213636));
#56320=DIRECTION('',(-1.,0.,0.));
#56321=DIRECTION('',(-0.948683298050513,-0.108156265856636,0.297156898213637));
#56322=DIRECTION('',(-0.86824314212446,-0.169689510806249,0.46621809925847));
#56323=DIRECTION('',(-0.957826285221151,-0.0982787650057293,0.270018687665128));
#56324=DIRECTION('',(-0.998052578482888,0.0213346303712044,-0.058616415197295));
#56325=DIRECTION('',(0.,0.342020143325669,-0.939692620785909));
#56326=DIRECTION('',(-1.,0.,0.));
#56327=DIRECTION('',(-0.755033118392644,-0.224258043872452,0.616143911670627));
#56328=DIRECTION('center_axis',(0.649305557988371,0.386503331141725,-0.654994249884502));
#56329=DIRECTION('ref_axis',(0.755033118392643,-0.224258043872452,0.616143911670627));
#56330=DIRECTION('',(0.,-0.861236613605368,-0.508204186706051));
#56331=DIRECTION('',(-0.755033118392644,0.224258043872452,-0.616143911670627));
#56332=DIRECTION('center_axis',(-0.649305557988371,-0.386503331141725,0.654994249884502));
#56333=DIRECTION('ref_axis',(-0.760527640763576,0.329979803021199,-0.559205719957048));
#56334=DIRECTION('',(0.0519254248777275,-0.881756465810299,-0.468838229299828));
#56335=DIRECTION('center_axis',(0.,-0.866025403784439,-0.5));
#56336=DIRECTION('ref_axis',(1.,0.,0.));
#56337=DIRECTION('',(0.755033118392644,-0.327843327723121,0.567841300538901));
#56338=DIRECTION('',(1.,0.,0.));
#56339=DIRECTION('',(0.,0.5,-0.866025403784439));
#56340=DIRECTION('',(0.998052578482888,0.0311891430775903,-0.0540211804549215));
#56341=DIRECTION('',(0.957826285221151,-0.143673942783173,0.248850568624199));
#56342=DIRECTION('',(0.86824314212446,-0.248069469178416,0.429668924423658));
#56343=DIRECTION('',(0.948683298050513,-0.15811388300842,0.273861278752585));
#56344=DIRECTION('',(1.,0.,0.));
#56345=DIRECTION('',(0.948683298050513,0.158113883008419,-0.273861278752584));
#56346=DIRECTION('',(0.868243142124459,0.248069469178416,-0.429668924423659));
#56347=DIRECTION('',(0.957826285221151,0.143673942783173,-0.248850568624199));
#56348=DIRECTION('',(0.998052578482888,-0.0311891430775902,0.0540211804549215));
#56349=DIRECTION('',(0.,-0.5,0.866025403784439));
#56350=DIRECTION('',(1.,0.,0.));
#56351=DIRECTION('',(0.755033118392644,0.327843327723121,-0.567841300538901));
#56352=DIRECTION('',(-0.755033118392644,0.327843327723121,-0.567841300538901));
#56353=DIRECTION('',(-1.,0.,0.));
#56354=DIRECTION('',(0.,-0.5,0.866025403784439));
#56355=DIRECTION('',(-0.998052578482888,-0.0311891430775902,0.0540211804549215));
#56356=DIRECTION('',(-0.957826285221151,0.143673942783173,-0.248850568624199));
#56357=DIRECTION('',(-0.868243142124459,0.248069469178416,-0.429668924423659));
#56358=DIRECTION('',(-0.948683298050513,0.158113883008419,-0.273861278752584));
#56359=DIRECTION('',(-1.,0.,0.));
#56360=DIRECTION('',(-0.948683298050513,-0.15811388300842,0.273861278752585));
#56361=DIRECTION('',(-0.86824314212446,-0.248069469178416,0.429668924423658));
#56362=DIRECTION('',(-0.957826285221151,-0.143673942783173,0.248850568624199));
#56363=DIRECTION('',(-0.998052578482888,0.0311891430775903,-0.0540211804549215));
#56364=DIRECTION('',(0.,0.5,-0.866025403784439));
#56365=DIRECTION('',(-1.,0.,0.));
#56366=DIRECTION('',(-0.755033118392644,-0.327843327723121,0.567841300538901));
#56367=DIRECTION('center_axis',(0.649305557988371,0.494370034948177,-0.577927816349714));
#56368=DIRECTION('ref_axis',(0.755033118392643,-0.327843327723121,0.567841300538901));
#56369=DIRECTION('',(0.,-0.759903763352335,-0.650035591673993));
#56370=DIRECTION('',(-0.755033118392644,0.327843327723121,-0.567841300538901));
#56371=DIRECTION('center_axis',(-0.649305557988371,-0.494370034948177,0.577927816349714));
#56372=DIRECTION('ref_axis',(-0.760527640763576,0.422071722564183,-0.493409737080951));
#56373=DIRECTION('',(0.0519254248777275,-0.786947699660121,-0.614830926556978));
#56374=DIRECTION('center_axis',(0.,-0.766044443118978,-0.642787609686539));
#56375=DIRECTION('ref_axis',(1.,0.,0.));
#56376=DIRECTION('',(0.755033118392644,-0.421467257957652,0.502285118831863));
#56377=DIRECTION('',(1.,0.,0.));
#56378=DIRECTION('',(0.,0.642787609686539,-0.766044443118978));
#56379=DIRECTION('',(0.998052578482888,0.0400959894540315,-0.0477845394804616));
#56380=DIRECTION('',(0.957826285221151,-0.184703660511672,0.220121250980087));
#56381=DIRECTION('',(0.86824314212446,-0.318911962258805,0.3800644767432));
#56382=DIRECTION('',(0.948683298050513,-0.203267289834479,0.242244522917128));
#56383=DIRECTION('',(1.,0.,0.));
#56384=DIRECTION('',(0.948683298050514,0.203267289834478,-0.242244522917128));
#56385=DIRECTION('',(0.868243142124459,0.318911962258806,-0.380064476743201));
#56386=DIRECTION('',(0.957826285221151,0.184703660511673,-0.220121250980087));
#56387=DIRECTION('',(0.998052578482888,-0.0400959894540314,0.0477845394804615));
#56388=DIRECTION('',(0.,-0.642787609686539,0.766044443118978));
#56389=DIRECTION('',(1.,0.,0.));
#56390=DIRECTION('',(0.755033118392644,0.421467257957652,-0.502285118831862));
#56391=DIRECTION('',(-0.755033118392644,0.421467257957652,-0.502285118831862));
#56392=DIRECTION('',(-1.,0.,0.));
#56393=DIRECTION('',(0.,-0.642787609686539,0.766044443118978));
#56394=DIRECTION('',(-0.998052578482888,-0.0400959894540314,0.0477845394804615));
#56395=DIRECTION('',(-0.957826285221151,0.184703660511673,-0.220121250980087));
#56396=DIRECTION('',(-0.868243142124459,0.318911962258806,-0.380064476743201));
#56397=DIRECTION('',(-0.948683298050514,0.203267289834478,-0.242244522917128));
#56398=DIRECTION('',(-1.,0.,0.));
#56399=DIRECTION('',(-0.948683298050513,-0.203267289834479,0.242244522917128));
#56400=DIRECTION('',(-0.86824314212446,-0.318911962258805,0.3800644767432));
#56401=DIRECTION('',(-0.957826285221151,-0.184703660511672,0.220121250980087));
#56402=DIRECTION('',(-0.998052578482888,0.0400959894540315,-0.0477845394804616));
#56403=DIRECTION('',(0.,0.642787609686539,-0.766044443118978));
#56404=DIRECTION('',(-1.,0.,0.));
#56405=DIRECTION('',(-0.755033118392644,-0.421467257957652,0.502285118831863));
#56406=DIRECTION('center_axis',(0.649305557988371,0.587215555406037,-0.483301338560726));
#56407=DIRECTION('ref_axis',(0.755033118392643,-0.421467257957652,0.502285118831863));
#56408=DIRECTION('',(0.,-0.6354816217797,-0.772115994122802));
#56409=DIRECTION('',(-0.755033118392644,0.421467257957652,-0.502285118831863));
#56410=DIRECTION('center_axis',(-0.649305557988371,-0.587215555406037,0.483301338560726));
#56411=DIRECTION('ref_axis',(-0.760527640763576,0.501339206395651,-0.412621749021023));
#56412=DIRECTION('',(0.0519254248777275,-0.66822792587052,-0.742142297230154));
#56413=DIRECTION('center_axis',(0.,-0.642787609686539,-0.766044443118978));
#56414=DIRECTION('ref_axis',(1.,0.,0.));
#56415=DIRECTION('',(0.755033118392644,-0.502285118831862,0.421467257957652));
#56416=DIRECTION('',(1.,0.,0.));
#56417=DIRECTION('',(0.,0.766044443118978,-0.642787609686539));
#56418=DIRECTION('',(0.998052578482888,0.0477845394804615,-0.0400959894540315));
#56419=DIRECTION('',(0.957826285221151,-0.220121250980087,0.184703660511672));
#56420=DIRECTION('',(0.86824314212446,-0.3800644767432,0.318911962258805));
#56421=DIRECTION('',(0.948683298050513,-0.242244522917128,0.203267289834479));
#56422=DIRECTION('',(1.,0.,0.));
#56423=DIRECTION('',(0.948683298050514,0.242244522917128,-0.203267289834478));
#56424=DIRECTION('',(0.86824314212446,0.380064476743201,-0.318911962258806));
#56425=DIRECTION('',(0.957826285221151,0.220121250980087,-0.184703660511673));
#56426=DIRECTION('',(0.998052578482888,-0.0477845394804615,0.0400959894540314));
#56427=DIRECTION('',(0.,-0.766044443118978,0.642787609686539));
#56428=DIRECTION('',(1.,0.,0.));
#56429=DIRECTION('',(0.755033118392644,0.502285118831862,-0.421467257957652));
#56430=DIRECTION('',(-0.755033118392644,0.502285118831862,-0.421467257957652));
#56431=DIRECTION('',(-1.,0.,0.));
#56432=DIRECTION('',(0.,-0.766044443118978,0.642787609686539));
#56433=DIRECTION('',(-0.998052578482888,-0.0477845394804615,0.0400959894540314));
#56434=DIRECTION('',(-0.957826285221151,0.220121250980087,-0.184703660511673));
#56435=DIRECTION('',(-0.86824314212446,0.380064476743201,-0.318911962258806));
#56436=DIRECTION('',(-0.948683298050514,0.242244522917128,-0.203267289834478));
#56437=DIRECTION('',(-1.,0.,0.));
#56438=DIRECTION('',(-0.948683298050513,-0.242244522917128,0.203267289834479));
#56439=DIRECTION('',(-0.86824314212446,-0.3800644767432,0.318911962258805));
#56440=DIRECTION('',(-0.957826285221151,-0.220121250980087,0.184703660511672));
#56441=DIRECTION('',(-0.998052578482888,0.0477845394804615,-0.0400959894540315));
#56442=DIRECTION('',(0.,0.766044443118978,-0.642787609686539));
#56443=DIRECTION('',(-1.,0.,0.));
#56444=DIRECTION('',(-0.755033118392644,-0.502285118831862,0.421467257957652));
#56445=DIRECTION('center_axis',(0.649305557988371,0.662218828358294,-0.373989994161848));
#56446=DIRECTION('ref_axis',(0.755033118392643,-0.502285118831862,0.421467257957652));
#56447=DIRECTION('',(0.,-0.491750692698505,-0.870736042799734));
#56448=DIRECTION('',(-0.755033118392644,0.502285118831862,-0.421467257957652));
#56449=DIRECTION('center_axis',(-0.649305557988371,-0.662218828358294,0.373989994161848));
#56450=DIRECTION('ref_axis',(-0.760527640763576,0.565373752130667,-0.319296457913771));
#56451=DIRECTION('',(0.0519254248777275,-0.52920438469299,-0.846904049744115));
#56452=DIRECTION('center_axis',(0.,-0.5,-0.866025403784438));
#56453=DIRECTION('ref_axis',(1.,0.,0.));
#56454=DIRECTION('',(0.755033118392644,-0.567841300538901,0.327843327723122));
#56455=DIRECTION('',(1.,0.,0.));
#56456=DIRECTION('',(0.,0.866025403784438,-0.5));
#56457=DIRECTION('',(0.998052578482888,0.0540211804549215,-0.0311891430775903));
#56458=DIRECTION('',(0.957826285221151,-0.248850568624199,0.143673942783173));
#56459=DIRECTION('',(0.86824314212446,-0.429668924423658,0.248069469178416));
#56460=DIRECTION('',(0.948683298050513,-0.273861278752584,0.15811388300842));
#56461=DIRECTION('',(1.,0.,0.));
#56462=DIRECTION('',(0.948683298050514,0.273861278752584,-0.158113883008419));
#56463=DIRECTION('',(0.86824314212446,0.429668924423659,-0.248069469178417));
#56464=DIRECTION('',(0.957826285221151,0.248850568624199,-0.143673942783173));
#56465=DIRECTION('',(0.998052578482888,-0.0540211804549214,0.0311891430775903));
#56466=DIRECTION('',(0.,-0.866025403784438,0.5));
#56467=DIRECTION('',(1.,0.,0.));
#56468=DIRECTION('',(0.755033118392644,0.567841300538901,-0.327843327723122));
#56469=DIRECTION('',(-0.755033118392644,0.567841300538901,-0.327843327723122));
#56470=DIRECTION('',(-1.,0.,0.));
#56471=DIRECTION('',(0.,-0.866025403784438,0.5));
#56472=DIRECTION('',(-0.998052578482888,-0.0540211804549214,0.0311891430775903));
#56473=DIRECTION('',(-0.957826285221151,0.248850568624199,-0.143673942783173));
#56474=DIRECTION('',(-0.86824314212446,0.429668924423659,-0.248069469178417));
#56475=DIRECTION('',(-0.948683298050514,0.273861278752584,-0.158113883008419));
#56476=DIRECTION('',(-1.,0.,0.));
#56477=DIRECTION('',(-0.948683298050513,-0.273861278752584,0.15811388300842));
#56478=DIRECTION('',(-0.86824314212446,-0.429668924423658,0.248069469178416));
#56479=DIRECTION('',(-0.957826285221151,-0.248850568624199,0.143673942783173));
#56480=DIRECTION('',(-0.998052578482888,0.0540211804549215,-0.0311891430775903));
#56481=DIRECTION('',(0.,0.866025403784438,-0.5));
#56482=DIRECTION('',(-1.,0.,0.));
#56483=DIRECTION('',(-0.755033118392644,-0.567841300538901,0.327843327723122));
#56484=DIRECTION('center_axis',(0.649305557988371,0.717100917309779,-0.253315153038432));
#56485=DIRECTION('ref_axis',(0.755033118392643,-0.567841300538901,0.327843327723122));
#56486=DIRECTION('',(0.,-0.333078167657524,-0.942899217429894));
#56487=DIRECTION('',(-0.755033118392644,0.567841300538901,-0.327843327723122));
#56488=DIRECTION('center_axis',(-0.649305557988371,-0.717100917309779,0.253315153038432));
#56489=DIRECTION('ref_axis',(-0.760527640763576,0.612229702500115,-0.216269505504613));
#56490=DIRECTION('',(0.0519254248777275,-0.374101236076903,-0.925933051260727));
#56491=DIRECTION('center_axis',(0.,-0.342020143325669,-0.939692620785908));
#56492=DIRECTION('ref_axis',(1.,0.,0.));
#56493=DIRECTION('',(0.755033118392644,-0.616143911670627,0.224258043872453));
#56494=DIRECTION('',(1.,0.,0.));
#56495=DIRECTION('',(0.,0.939692620785908,-0.342020143325669));
#56496=DIRECTION('',(0.998052578482888,0.0586164151972949,-0.0213346303712045));
#56497=DIRECTION('',(0.957826285221151,-0.270018687665128,0.0982787650057295));
#56498=DIRECTION('',(0.86824314212446,-0.46621809925847,0.169689510806249));
#56499=DIRECTION('',(0.948683298050513,-0.297156898213637,0.108156265856636));
#56500=DIRECTION('',(1.,0.,0.));
#56501=DIRECTION('',(0.948683298050514,0.297156898213636,-0.108156265856635));
#56502=DIRECTION('',(0.868243142124459,0.466218099258471,-0.16968951080625));
#56503=DIRECTION('',(0.957826285221151,0.270018687665129,-0.0982787650057297));
#56504=DIRECTION('',(0.998052578482888,-0.0586164151972949,0.0213346303712045));
#56505=DIRECTION('',(0.,-0.939692620785908,0.342020143325669));
#56506=DIRECTION('',(1.,0.,0.));
#56507=DIRECTION('',(0.755033118392644,0.616143911670627,-0.224258043872453));
#56508=DIRECTION('',(-0.755033118392644,0.616143911670627,-0.224258043872453));
#56509=DIRECTION('',(-1.,0.,0.));
#56510=DIRECTION('',(0.,-0.939692620785908,0.342020143325669));
#56511=DIRECTION('',(-0.998052578482888,-0.0586164151972949,0.0213346303712045));
#56512=DIRECTION('',(-0.957826285221151,0.270018687665129,-0.0982787650057297));
#56513=DIRECTION('',(-0.868243142124459,0.466218099258471,-0.16968951080625));
#56514=DIRECTION('',(-0.948683298050514,0.297156898213636,-0.108156265856635));
#56515=DIRECTION('',(-1.,0.,0.));
#56516=DIRECTION('',(-0.948683298050513,-0.297156898213637,0.108156265856636));
#56517=DIRECTION('',(-0.86824314212446,-0.46621809925847,0.169689510806249));
#56518=DIRECTION('',(-0.957826285221151,-0.270018687665128,0.0982787650057295));
#56519=DIRECTION('',(-0.998052578482888,0.0586164151972949,-0.0213346303712045));
#56520=DIRECTION('',(0.,0.939692620785908,-0.342020143325669));
#56521=DIRECTION('',(-1.,0.,0.));
#56522=DIRECTION('',(-0.755033118392644,-0.616143911670627,0.224258043872453));
#56523=DIRECTION('center_axis',(0.649305557988371,0.75019425775938,-0.124943459173594));
#56524=DIRECTION('ref_axis',(0.755033118392643,-0.616143911670627,0.224258043872453));
#56525=DIRECTION('',(0.,-0.164285231037954,-0.986412876468473));
#56526=DIRECTION('',(-0.755033118392644,0.616143911670627,-0.224258043872453));
#56527=DIRECTION('center_axis',(-0.649305557988371,-0.75019425775938,0.124943459173594));
#56528=DIRECTION('ref_axis',(-0.760527640763576,0.640483363162275,-0.106671313608347));
#56529=DIRECTION('',(0.0519254248777275,-0.207631210706979,-0.976828045559515));
#56530=DIRECTION('center_axis',(0.,-0.17364817766693,-0.984807753012208));
#56531=DIRECTION('ref_axis',(1.,0.,0.));
#56532=DIRECTION('',(0.755033118392643,-0.645725301830105,0.113858792838765));
#56533=DIRECTION('',(1.,0.,0.));
#56534=DIRECTION('',(0.,0.984807753012208,-0.17364817766693));
#56535=DIRECTION('',(0.998052578482888,0.0614306198252359,-0.0108318757168334));
#56536=DIRECTION('',(0.957826285221151,-0.282982425517402,0.0498974366850415));
#56537=DIRECTION('',(0.86824314212446,-0.488601473065054,0.0861536225152694));
#56538=DIRECTION('',(0.948683298050513,-0.311423555691114,0.0549123752965087));
#56539=DIRECTION('',(1.,0.,0.));
#56540=DIRECTION('',(0.948683298050514,0.311423555691113,-0.0549123752965085));
#56541=DIRECTION('',(0.868243142124459,0.488601473065055,-0.0861536225152696));
#56542=DIRECTION('',(0.957826285221151,0.282982425517402,-0.0498974366850416));
#56543=DIRECTION('',(0.998052578482888,-0.0614306198252359,0.0108318757168334));
#56544=DIRECTION('',(0.,-0.984807753012208,0.17364817766693));
#56545=DIRECTION('',(1.,0.,0.));
#56546=DIRECTION('',(0.755033118392644,0.645725301830105,-0.113858792838765));
#56547=DIRECTION('',(-0.755033118392644,0.645725301830105,-0.113858792838765));
#56548=DIRECTION('',(-1.,0.,0.));
#56549=DIRECTION('',(0.,-0.984807753012208,0.17364817766693));
#56550=DIRECTION('',(-0.998052578482888,-0.0614306198252359,0.0108318757168334));
#56551=DIRECTION('',(-0.957826285221151,0.282982425517402,-0.0498974366850416));
#56552=DIRECTION('',(-0.868243142124459,0.488601473065055,-0.0861536225152696));
#56553=DIRECTION('',(-0.948683298050514,0.311423555691113,-0.0549123752965085));
#56554=DIRECTION('',(-1.,0.,0.));
#56555=DIRECTION('',(-0.948683298050513,-0.311423555691114,0.0549123752965087));
#56556=DIRECTION('',(-0.86824314212446,-0.488601473065054,0.0861536225152694));
#56557=DIRECTION('',(-0.957826285221151,-0.282982425517402,0.0498974366850415));
#56558=DIRECTION('',(-0.998052578482888,0.0614306198252359,-0.0108318757168334));
#56559=DIRECTION('',(0.,0.984807753012208,-0.17364817766693));
#56560=DIRECTION('',(-1.,0.,0.));
#56561=DIRECTION('',(-0.755033118392643,-0.645725301830105,0.113858792838765));
#56562=DIRECTION('center_axis',(0.649305557988371,0.760493325303573,0.00722457847379226));
#56563=DIRECTION('ref_axis',(0.755033118392643,-0.645725301830105,0.113858792838765));
#56564=DIRECTION('',(0.,0.0094994291943666,-0.999954879404557));
#56565=DIRECTION('',(-0.755033118392643,0.645725301830105,-0.113858792838765));
#56566=DIRECTION('center_axis',(-0.649305557988371,-0.760493325303573,-0.00722457847379226));
#56567=DIRECTION('ref_axis',(-0.760527640763576,0.64927626093497,0.00616803217361923));
#56568=DIRECTION('',(0.0519254248777275,-0.0348524160661844,-0.998042613992818));
#56569=DIRECTION('center_axis',(0.,-1.83697019872103E-16,-1.));
#56570=DIRECTION('ref_axis',(1.,0.,0.));
#56571=DIRECTION('',(0.755033118392644,-0.655686655446243,1.20447684575381E-16));
#56572=DIRECTION('',(1.,0.,0.));
#56573=DIRECTION('',(0.,1.,-1.83697019872103E-16));
#56574=DIRECTION('',(0.998052578482888,0.0623782861551806,-1.14587052714359E-17));
#56575=DIRECTION('',(0.957826285221151,-0.287347885566345,5.27849502450877E-17));
#56576=DIRECTION('',(0.86824314212446,-0.496138938356832,9.11392444186591E-17));
#56577=DIRECTION('',(0.948683298050513,-0.31622776601684,5.80900982181061E-17));
#56578=DIRECTION('',(1.,0.,0.));
#56579=DIRECTION('',(0.948683298050514,0.316227766016839,-5.80900982181059E-17));
#56580=DIRECTION('',(0.868243142124459,0.496138938356833,-9.11392444186592E-17));
#56581=DIRECTION('',(0.957826285221151,0.287347885566346,-5.27849502450878E-17));
#56582=DIRECTION('',(0.998052578482888,-0.0623782861551805,1.14587052714359E-17));
#56583=DIRECTION('',(0.,-1.,1.83697019872103E-16));
#56584=DIRECTION('',(1.,0.,0.));
#56585=DIRECTION('',(0.755033118392644,0.655686655446243,-1.20447684575381E-16));
#56586=DIRECTION('',(-0.755033118392644,0.655686655446243,-1.20447684575381E-16));
#56587=DIRECTION('',(-1.,0.,0.));
#56588=DIRECTION('',(0.,-1.,1.83697019872103E-16));
#56589=DIRECTION('',(-0.998052578482888,-0.0623782861551805,1.14587052714359E-17));
#56590=DIRECTION('',(-0.957826285221151,0.287347885566346,-5.27849502450878E-17));
#56591=DIRECTION('',(-0.868243142124459,0.496138938356833,-9.11392444186592E-17));
#56592=DIRECTION('',(-0.948683298050514,0.316227766016839,-5.80900982181059E-17));
#56593=DIRECTION('',(-1.,0.,0.));
#56594=DIRECTION('',(-0.948683298050513,-0.31622776601684,5.80900982181061E-17));
#56595=DIRECTION('',(-0.86824314212446,-0.496138938356832,9.11392444186591E-17));
#56596=DIRECTION('',(-0.957826285221151,-0.287347885566345,5.27849502450877E-17));
#56597=DIRECTION('',(-0.998052578482888,0.0623782861551806,-1.14587052714359E-17));
#56598=DIRECTION('',(0.,1.,-1.83697019872103E-16));
#56599=DIRECTION('',(-1.,0.,0.));
#56600=DIRECTION('',(-0.755033118392644,-0.655686655446243,1.20447684575381E-16));
#56601=DIRECTION('center_axis',(0.649305557988371,0.747685187986609,0.139173100960065));
#56602=DIRECTION('ref_axis',(0.755033118392643,-0.655686655446243,1.20447684575381E-16));
#56603=DIRECTION('',(0.,0.182995454077559,-0.983113759331517));
#56604=DIRECTION('',(-0.755033118392644,0.655686655446243,-1.20447684575381E-16));
#56605=DIRECTION('center_axis',(-0.649305557988371,-0.747685187986609,-0.139173100960065));
#56606=DIRECTION('ref_axis',(-0.760527640763576,0.638341228068795,0.118819965419165));
#56607=DIRECTION('',(0.0519254248777275,0.138985351600607,-0.98893216263388));
#56608=DIRECTION('center_axis',(0.,0.17364817766693,-0.984807753012208));
#56609=DIRECTION('ref_axis',(1.,0.,0.));
#56610=DIRECTION('',(0.755033118392643,-0.645725301830105,-0.113858792838764));
#56611=DIRECTION('',(1.,0.,0.));
#56612=DIRECTION('',(0.,0.984807753012208,0.17364817766693));
#56613=DIRECTION('',(0.998052578482888,0.0614306198252359,0.0108318757168334));
#56614=DIRECTION('',(0.957826285221151,-0.282982425517402,-0.0498974366850414));
#56615=DIRECTION('',(0.86824314212446,-0.488601473065054,-0.0861536225152692));
#56616=DIRECTION('',(0.948683298050513,-0.311423555691114,-0.0549123752965085));
#56617=DIRECTION('',(1.,0.,0.));
#56618=DIRECTION('',(0.948683298050514,0.311423555691113,0.0549123752965084));
#56619=DIRECTION('',(0.86824314212446,0.488601473065055,0.0861536225152694));
#56620=DIRECTION('',(0.957826285221151,0.282982425517402,0.0498974366850415));
#56621=DIRECTION('',(0.998052578482888,-0.0614306198252359,-0.0108318757168334));
#56622=DIRECTION('',(0.,-0.984807753012208,-0.17364817766693));
#56623=DIRECTION('',(1.,0.,0.));
#56624=DIRECTION('',(0.755033118392644,0.645725301830105,0.113858792838764));
#56625=DIRECTION('',(-0.755033118392644,0.645725301830105,0.113858792838764));
#56626=DIRECTION('',(-1.,0.,0.));
#56627=DIRECTION('',(0.,-0.984807753012208,-0.17364817766693));
#56628=DIRECTION('',(-0.998052578482888,-0.0614306198252359,-0.0108318757168334));
#56629=DIRECTION('',(-0.957826285221151,0.282982425517402,0.0498974366850415));
#56630=DIRECTION('',(-0.86824314212446,0.488601473065055,0.0861536225152694));
#56631=DIRECTION('',(-0.948683298050514,0.311423555691113,0.0549123752965084));
#56632=DIRECTION('',(-1.,0.,0.));
#56633=DIRECTION('',(-0.948683298050513,-0.311423555691114,-0.0549123752965085));
#56634=DIRECTION('',(-0.86824314212446,-0.488601473065054,-0.0861536225152692));
#56635=DIRECTION('',(-0.957826285221151,-0.282982425517402,-0.0498974366850414));
#56636=DIRECTION('',(-0.998052578482888,0.0614306198252359,0.0108318757168334));
#56637=DIRECTION('',(0.,0.984807753012208,0.17364817766693));
#56638=DIRECTION('',(-1.,0.,0.));
#56639=DIRECTION('',(-0.755033118392643,-0.645725301830105,-0.113858792838764));
#56640=DIRECTION('center_axis',(0.649305557988371,0.712159014579631,0.266892919198654));
#56641=DIRECTION('ref_axis',(0.755033118392643,-0.645725301830105,-0.113858792838764));
#56642=DIRECTION('',(0.,0.350931254688772,-0.936401225160756));
#56643=DIRECTION('',(-0.755033118392643,0.645725301830105,0.113858792838764));
#56644=DIRECTION('center_axis',(-0.649305557988371,-0.712159014579631,-0.266892919198654));
#56645=DIRECTION('ref_axis',(-0.760527640763576,0.608010520003999,0.227861614141252));
#56646=DIRECTION('',(0.0519254248777275,0.308600119688995,-0.949773507937132));
#56647=DIRECTION('center_axis',(0.,0.342020143325668,-0.939692620785909));
#56648=DIRECTION('ref_axis',(1.,0.,0.));
#56649=DIRECTION('',(0.755033118392643,-0.616143911670627,-0.224258043872452));
#56650=DIRECTION('',(1.,0.,0.));
#56651=DIRECTION('',(0.,0.939692620785909,0.342020143325668));
#56652=DIRECTION('',(0.998052578482888,0.058616415197295,0.0213346303712044));
#56653=DIRECTION('',(0.957826285221151,-0.270018687665128,-0.0982787650057291));
#56654=DIRECTION('',(0.86824314212446,-0.46621809925847,-0.169689510806249));
#56655=DIRECTION('',(0.948683298050513,-0.297156898213637,-0.108156265856635));
#56656=DIRECTION('',(1.,0.,0.));
#56657=DIRECTION('',(0.948683298050514,0.297156898213636,0.108156265856635));
#56658=DIRECTION('',(0.868243142124459,0.466218099258471,0.169689510806249));
#56659=DIRECTION('',(0.957826285221151,0.270018687665129,0.0982787650057293));
#56660=DIRECTION('',(0.998052578482888,-0.0586164151972949,-0.0213346303712044));
#56661=DIRECTION('',(0.,-0.939692620785909,-0.342020143325668));
#56662=DIRECTION('',(1.,0.,0.));
#56663=DIRECTION('',(0.755033118392644,0.616143911670627,0.224258043872452));
#56664=DIRECTION('',(-0.755033118392644,0.616143911670627,0.224258043872452));
#56665=DIRECTION('',(-1.,0.,0.));
#56666=DIRECTION('',(0.,-0.939692620785909,-0.342020143325668));
#56667=DIRECTION('',(-0.998052578482888,-0.0586164151972949,-0.0213346303712044));
#56668=DIRECTION('',(-0.957826285221151,0.270018687665129,0.0982787650057293));
#56669=DIRECTION('',(-0.868243142124459,0.466218099258471,0.169689510806249));
#56670=DIRECTION('',(-0.948683298050514,0.297156898213636,0.108156265856635));
#56671=DIRECTION('',(-1.,0.,0.));
#56672=DIRECTION('',(-0.948683298050513,-0.297156898213637,-0.108156265856635));
#56673=DIRECTION('',(-0.86824314212446,-0.46621809925847,-0.169689510806249));
#56674=DIRECTION('',(-0.957826285221151,-0.270018687665128,-0.0982787650057291));
#56675=DIRECTION('',(-0.998052578482888,0.058616415197295,0.0213346303712044));
#56676=DIRECTION('',(0.,0.939692620785909,0.342020143325668));
#56677=DIRECTION('',(-1.,0.,0.));
#56678=DIRECTION('',(-0.755033118392643,-0.616143911670627,-0.224258043872452));
#56679=DIRECTION('center_axis',(0.649305557988371,0.654994249884502,0.386503331141725));
#56680=DIRECTION('ref_axis',(0.755033118392643,-0.616143911670627,-0.224258043872452));
#56681=DIRECTION('',(0.,0.508204186706051,-0.861236613605368));
#56682=DIRECTION('',(-0.755033118392643,0.616143911670627,0.224258043872452));
#56683=DIRECTION('center_axis',(-0.649305557988371,-0.654994249884502,-0.386503331141725));
#56684=DIRECTION('ref_axis',(-0.760527640763576,0.559205719957048,0.329979803021198));
#56685=DIRECTION('',(0.0519254248777275,0.468838229299828,-0.881756465810299));
#56686=DIRECTION('center_axis',(0.,0.5,-0.866025403784439));
#56687=DIRECTION('ref_axis',(1.,0.,0.));
#56688=DIRECTION('',(0.755033118392644,-0.567841300538901,-0.327843327723122));
#56689=DIRECTION('',(1.,0.,0.));
#56690=DIRECTION('',(0.,0.866025403784439,0.5));
#56691=DIRECTION('',(0.998052578482888,0.0540211804549215,0.0311891430775903));
#56692=DIRECTION('',(0.957826285221151,-0.248850568624199,-0.143673942783173));
#56693=DIRECTION('',(0.86824314212446,-0.429668924423658,-0.248069469178416));
#56694=DIRECTION('',(0.948683298050513,-0.273861278752585,-0.15811388300842));
#56695=DIRECTION('',(1.,0.,0.));
#56696=DIRECTION('',(0.948683298050514,0.273861278752584,0.158113883008419));
#56697=DIRECTION('',(0.868243142124459,0.429668924423659,0.248069469178417));
#56698=DIRECTION('',(0.957826285221151,0.248850568624199,0.143673942783173));
#56699=DIRECTION('',(0.998052578482888,-0.0540211804549215,-0.0311891430775903));
#56700=DIRECTION('',(0.,-0.866025403784439,-0.5));
#56701=DIRECTION('',(1.,0.,0.));
#56702=DIRECTION('',(0.755033118392644,0.567841300538901,0.327843327723122));
#56703=DIRECTION('',(-0.755033118392644,0.567841300538901,0.327843327723122));
#56704=DIRECTION('',(-1.,0.,0.));
#56705=DIRECTION('',(0.,-0.866025403784439,-0.5));
#56706=DIRECTION('',(-0.998052578482888,-0.0540211804549215,-0.0311891430775903));
#56707=DIRECTION('',(-0.957826285221151,0.248850568624199,0.143673942783173));
#56708=DIRECTION('',(-0.868243142124459,0.429668924423659,0.248069469178417));
#56709=DIRECTION('',(-0.948683298050514,0.273861278752584,0.158113883008419));
#56710=DIRECTION('',(-1.,0.,0.));
#56711=DIRECTION('',(-0.948683298050513,-0.273861278752585,-0.15811388300842));
#56712=DIRECTION('',(-0.86824314212446,-0.429668924423658,-0.248069469178416));
#56713=DIRECTION('',(-0.957826285221151,-0.248850568624199,-0.143673942783173));
#56714=DIRECTION('',(-0.998052578482888,0.0540211804549215,0.0311891430775903));
#56715=DIRECTION('',(0.,0.866025403784439,0.5));
#56716=DIRECTION('',(-1.,0.,0.));
#56717=DIRECTION('',(-0.755033118392644,-0.567841300538901,-0.327843327723122));
#56718=DIRECTION('center_axis',(0.649305557988371,0.577927816349714,0.494370034948177));
#56719=DIRECTION('ref_axis',(0.755033118392643,-0.567841300538901,-0.327843327723122));
#56720=DIRECTION('',(0.,0.650035591673993,-0.759903763352335));
#56721=DIRECTION('',(-0.755033118392644,0.567841300538901,0.327843327723122));
#56722=DIRECTION('center_axis',(-0.649305557988371,-0.577927816349714,-0.494370034948177));
#56723=DIRECTION('ref_axis',(-0.760527640763576,0.493409737080951,0.422071722564183));
#56724=DIRECTION('',(0.0519254248777275,0.614830926556978,-0.786947699660121));
#56725=DIRECTION('center_axis',(0.,0.642787609686539,-0.766044443118978));
#56726=DIRECTION('ref_axis',(1.,0.,0.));
#56727=DIRECTION('',(0.755033118392644,-0.502285118831863,-0.421467257957652));
#56728=DIRECTION('',(1.,0.,0.));
#56729=DIRECTION('',(0.,0.766044443118978,0.642787609686539));
#56730=DIRECTION('',(0.998052578482888,0.0477845394804616,0.0400959894540314));
#56731=DIRECTION('',(0.957826285221151,-0.220121250980087,-0.184703660511672));
#56732=DIRECTION('',(0.86824314212446,-0.3800644767432,-0.318911962258805));
#56733=DIRECTION('',(0.948683298050513,-0.242244522917128,-0.203267289834479));
#56734=DIRECTION('',(1.,0.,0.));
#56735=DIRECTION('',(0.948683298050514,0.242244522917128,0.203267289834478));
#56736=DIRECTION('',(0.868243142124459,0.380064476743201,0.318911962258806));
#56737=DIRECTION('',(0.957826285221151,0.220121250980087,0.184703660511673));
#56738=DIRECTION('',(0.998052578482888,-0.0477845394804615,-0.0400959894540314));
#56739=DIRECTION('',(0.,-0.766044443118978,-0.642787609686539));
#56740=DIRECTION('',(1.,0.,0.));
#56741=DIRECTION('',(0.755033118392644,0.502285118831863,0.421467257957652));
#56742=DIRECTION('',(-0.755033118392644,0.502285118831863,0.421467257957652));
#56743=DIRECTION('',(-1.,0.,0.));
#56744=DIRECTION('',(0.,-0.766044443118978,-0.642787609686539));
#56745=DIRECTION('',(-0.998052578482888,-0.0477845394804615,-0.0400959894540314));
#56746=DIRECTION('',(-0.957826285221151,0.220121250980087,0.184703660511673));
#56747=DIRECTION('',(-0.868243142124459,0.380064476743201,0.318911962258806));
#56748=DIRECTION('',(-0.948683298050514,0.242244522917128,0.203267289834478));
#56749=DIRECTION('',(-1.,0.,0.));
#56750=DIRECTION('',(-0.948683298050513,-0.242244522917128,-0.203267289834479));
#56751=DIRECTION('',(-0.86824314212446,-0.3800644767432,-0.318911962258805));
#56752=DIRECTION('',(-0.957826285221151,-0.220121250980087,-0.184703660511672));
#56753=DIRECTION('',(-0.998052578482888,0.0477845394804616,0.0400959894540314));
#56754=DIRECTION('',(0.,0.766044443118978,0.642787609686539));
#56755=DIRECTION('',(-1.,0.,0.));
#56756=DIRECTION('',(-0.755033118392644,-0.502285118831863,-0.421467257957652));
#56757=DIRECTION('center_axis',(0.649305557988371,0.483301338560726,0.587215555406037));
#56758=DIRECTION('ref_axis',(0.755033118392643,-0.502285118831863,-0.421467257957652));
#56759=DIRECTION('',(0.,0.772115994122802,-0.6354816217797));
#56760=DIRECTION('',(-0.755033118392644,0.502285118831863,0.421467257957652));
#56761=DIRECTION('center_axis',(-0.649305557988371,-0.483301338560726,-0.587215555406037));
#56762=DIRECTION('ref_axis',(-0.760527640763576,0.412621749021023,0.501339206395651));
#56763=DIRECTION('',(0.0519254248777275,0.742142297230154,-0.66822792587052));
#56764=DIRECTION('center_axis',(0.,0.766044443118978,-0.64278760968654));
#56765=DIRECTION('ref_axis',(1.,0.,0.));
#56766=DIRECTION('',(0.755033118392644,-0.421467257957652,-0.502285118831862));
#56767=DIRECTION('',(1.,0.,0.));
#56768=DIRECTION('',(0.,0.64278760968654,0.766044443118978));
#56769=DIRECTION('',(0.998052578482888,0.0400959894540315,0.0477845394804615));
#56770=DIRECTION('',(0.957826285221151,-0.184703660511672,-0.220121250980087));
#56771=DIRECTION('',(0.86824314212446,-0.318911962258806,-0.3800644767432));
#56772=DIRECTION('',(0.948683298050513,-0.203267289834479,-0.242244522917128));
#56773=DIRECTION('',(1.,0.,0.));
#56774=DIRECTION('',(0.948683298050514,0.203267289834478,0.242244522917128));
#56775=DIRECTION('',(0.86824314212446,0.318911962258806,0.380064476743201));
#56776=DIRECTION('',(0.957826285221151,0.184703660511673,0.220121250980087));
#56777=DIRECTION('',(0.998052578482888,-0.0400959894540314,-0.0477845394804615));
#56778=DIRECTION('',(0.,-0.64278760968654,-0.766044443118978));
#56779=DIRECTION('',(1.,0.,0.));
#56780=DIRECTION('',(0.755033118392644,0.421467257957652,0.502285118831862));
#56781=DIRECTION('',(-0.755033118392644,0.421467257957652,0.502285118831862));
#56782=DIRECTION('',(-1.,0.,0.));
#56783=DIRECTION('',(0.,-0.64278760968654,-0.766044443118978));
#56784=DIRECTION('',(-0.998052578482888,-0.0400959894540314,-0.0477845394804615));
#56785=DIRECTION('',(-0.957826285221151,0.184703660511673,0.220121250980087));
#56786=DIRECTION('',(-0.86824314212446,0.318911962258806,0.380064476743201));
#56787=DIRECTION('',(-0.948683298050514,0.203267289834478,0.242244522917128));
#56788=DIRECTION('',(-1.,0.,0.));
#56789=DIRECTION('',(-0.948683298050513,-0.203267289834479,-0.242244522917128));
#56790=DIRECTION('',(-0.86824314212446,-0.318911962258806,-0.3800644767432));
#56791=DIRECTION('',(-0.957826285221151,-0.184703660511672,-0.220121250980087));
#56792=DIRECTION('',(-0.998052578482888,0.0400959894540315,0.0477845394804615));
#56793=DIRECTION('',(0.,0.64278760968654,0.766044443118978));
#56794=DIRECTION('',(-1.,0.,0.));
#56795=DIRECTION('',(-0.755033118392644,-0.421467257957652,-0.502285118831862));
#56796=DIRECTION('center_axis',(0.649305557988371,0.373989994161849,0.662218828358293));
#56797=DIRECTION('ref_axis',(0.755033118392644,-0.421467257957652,-0.502285118831862));
#56798=DIRECTION('',(0.,0.870736042799734,-0.491750692698506));
#56799=DIRECTION('',(-0.755033118392644,0.421467257957652,0.502285118831862));
#56800=DIRECTION('center_axis',(-0.649305557988371,-0.373989994161849,-0.662218828358293));
#56801=DIRECTION('ref_axis',(-0.760527640763576,0.319296457913771,0.565373752130667));
#56802=DIRECTION('',(0.0519254248777275,0.846904049744114,-0.52920438469299));
#56803=DIRECTION('center_axis',(0.,0.866025403784438,-0.5));
#56804=DIRECTION('ref_axis',(1.,0.,0.));
#56805=DIRECTION('',(0.755033118392644,-0.327843327723122,-0.567841300538901));
#56806=DIRECTION('',(1.,0.,0.));
#56807=DIRECTION('',(0.,0.5,0.866025403784438));
#56808=DIRECTION('',(0.998052578482888,0.0311891430775903,0.0540211804549215));
#56809=DIRECTION('',(0.957826285221151,-0.143673942783173,-0.248850568624199));
#56810=DIRECTION('',(0.86824314212446,-0.248069469178416,-0.429668924423658));
#56811=DIRECTION('',(0.948683298050513,-0.15811388300842,-0.273861278752584));
#56812=DIRECTION('',(1.,0.,0.));
#56813=DIRECTION('',(0.948683298050514,0.158113883008419,0.273861278752584));
#56814=DIRECTION('',(0.86824314212446,0.248069469178417,0.429668924423659));
#56815=DIRECTION('',(0.957826285221151,0.143673942783173,0.248850568624199));
#56816=DIRECTION('',(0.998052578482888,-0.0311891430775903,-0.0540211804549214));
#56817=DIRECTION('',(0.,-0.5,-0.866025403784438));
#56818=DIRECTION('',(1.,0.,0.));
#56819=DIRECTION('',(0.755033118392644,0.327843327723122,0.567841300538901));
#56820=DIRECTION('',(-0.755033118392644,0.327843327723122,0.567841300538901));
#56821=DIRECTION('',(-1.,0.,0.));
#56822=DIRECTION('',(0.,-0.5,-0.866025403784438));
#56823=DIRECTION('',(-0.998052578482888,-0.0311891430775903,-0.0540211804549214));
#56824=DIRECTION('',(-0.957826285221151,0.143673942783173,0.248850568624199));
#56825=DIRECTION('',(-0.86824314212446,0.248069469178417,0.429668924423659));
#56826=DIRECTION('',(-0.948683298050514,0.158113883008419,0.273861278752584));
#56827=DIRECTION('',(-1.,0.,0.));
#56828=DIRECTION('',(-0.948683298050513,-0.15811388300842,-0.273861278752584));
#56829=DIRECTION('',(-0.86824314212446,-0.248069469178416,-0.429668924423658));
#56830=DIRECTION('',(-0.957826285221151,-0.143673942783173,-0.248850568624199));
#56831=DIRECTION('',(-0.998052578482888,0.0311891430775903,0.0540211804549215));
#56832=DIRECTION('',(0.,0.5,0.866025403784438));
#56833=DIRECTION('',(-1.,0.,0.));
#56834=DIRECTION('',(-0.755033118392644,-0.327843327723122,-0.567841300538901));
#56835=DIRECTION('center_axis',(0.649305557988371,0.253315153038432,0.717100917309779));
#56836=DIRECTION('ref_axis',(0.755033118392643,-0.327843327723122,-0.567841300538901));
#56837=DIRECTION('',(0.,0.942899217429894,-0.333078167657524));
#56838=DIRECTION('',(-0.755033118392644,0.327843327723122,0.567841300538901));
#56839=DIRECTION('center_axis',(-0.649305557988371,-0.253315153038432,-0.717100917309779));
#56840=DIRECTION('ref_axis',(-0.760527640763576,0.216269505504613,0.612229702500115));
#56841=DIRECTION('',(0.0519254248777275,0.925933051260727,-0.374101236076903));
#56842=DIRECTION('center_axis',(0.,0.939692620785908,-0.342020143325669));
#56843=DIRECTION('ref_axis',(1.,0.,0.));
#56844=DIRECTION('',(0.755033118392644,-0.224258043872453,-0.616143911670627));
#56845=DIRECTION('',(1.,0.,0.));
#56846=DIRECTION('',(0.,0.342020143325669,0.939692620785908));
#56847=DIRECTION('',(0.998052578482888,0.0213346303712045,0.0586164151972949));
#56848=DIRECTION('',(0.957826285221151,-0.0982787650057295,-0.270018687665128));
#56849=DIRECTION('',(0.86824314212446,-0.169689510806249,-0.46621809925847));
#56850=DIRECTION('',(0.948683298050513,-0.108156265856636,-0.297156898213637));
#56851=DIRECTION('',(1.,0.,0.));
#56852=DIRECTION('',(0.948683298050514,0.108156265856635,0.297156898213636));
#56853=DIRECTION('',(0.868243142124459,0.16968951080625,0.466218099258471));
#56854=DIRECTION('',(0.957826285221151,0.0982787650057297,0.270018687665129));
#56855=DIRECTION('',(0.998052578482888,-0.0213346303712045,-0.0586164151972949));
#56856=DIRECTION('',(0.,-0.342020143325669,-0.939692620785908));
#56857=DIRECTION('',(1.,0.,0.));
#56858=DIRECTION('',(0.755033118392644,0.224258043872453,0.616143911670627));
#56859=DIRECTION('',(-0.755033118392644,0.224258043872453,0.616143911670627));
#56860=DIRECTION('',(-1.,0.,0.));
#56861=DIRECTION('',(0.,-0.342020143325669,-0.939692620785908));
#56862=DIRECTION('',(-0.998052578482888,-0.0213346303712045,-0.0586164151972949));
#56863=DIRECTION('',(-0.957826285221151,0.0982787650057297,0.270018687665129));
#56864=DIRECTION('',(-0.868243142124459,0.16968951080625,0.466218099258471));
#56865=DIRECTION('',(-0.948683298050514,0.108156265856635,0.297156898213636));
#56866=DIRECTION('',(-1.,0.,0.));
#56867=DIRECTION('',(-0.948683298050513,-0.108156265856636,-0.297156898213637));
#56868=DIRECTION('',(-0.86824314212446,-0.169689510806249,-0.46621809925847));
#56869=DIRECTION('',(-0.957826285221151,-0.0982787650057295,-0.270018687665128));
#56870=DIRECTION('',(-0.998052578482888,0.0213346303712045,0.0586164151972949));
#56871=DIRECTION('',(0.,0.342020143325669,0.939692620785908));
#56872=DIRECTION('',(-1.,0.,0.));
#56873=DIRECTION('',(-0.755033118392644,-0.224258043872453,-0.616143911670627));
#56874=DIRECTION('center_axis',(0.649305557988371,0.124943459173594,0.75019425775938));
#56875=DIRECTION('ref_axis',(0.755033118392643,-0.224258043872453,-0.616143911670627));
#56876=DIRECTION('',(0.,0.986412876468473,-0.164285231037954));
#56877=DIRECTION('',(-0.755033118392644,0.224258043872453,0.616143911670627));
#56878=DIRECTION('center_axis',(-0.649305557988371,-0.124943459173594,-0.75019425775938));
#56879=DIRECTION('ref_axis',(-0.760527640763576,0.106671313608347,0.640483363162275));
#56880=DIRECTION('',(0.0519254248777275,0.976828045559515,-0.207631210706979));
#56881=DIRECTION('center_axis',(0.,0.984807753012208,-0.17364817766693));
#56882=DIRECTION('ref_axis',(1.,0.,0.));
#56883=DIRECTION('',(0.755033118392643,-0.113858792838765,-0.645725301830105));
#56884=DIRECTION('',(1.,0.,0.));
#56885=DIRECTION('',(0.,0.17364817766693,0.984807753012208));
#56886=DIRECTION('',(0.998052578482888,0.0108318757168334,0.0614306198252359));
#56887=DIRECTION('',(0.957826285221151,-0.0498974366850415,-0.282982425517402));
#56888=DIRECTION('',(0.86824314212446,-0.0861536225152694,-0.488601473065054));
#56889=DIRECTION('',(0.948683298050513,-0.0549123752965087,-0.311423555691114));
#56890=DIRECTION('',(1.,0.,0.));
#56891=DIRECTION('',(0.948683298050514,0.0549123752965085,0.311423555691113));
#56892=DIRECTION('',(0.868243142124459,0.0861536225152696,0.488601473065055));
#56893=DIRECTION('',(0.957826285221151,0.0498974366850416,0.282982425517402));
#56894=DIRECTION('',(0.998052578482888,-0.0108318757168334,-0.0614306198252359));
#56895=DIRECTION('',(0.,-0.17364817766693,-0.984807753012208));
#56896=DIRECTION('',(1.,0.,0.));
#56897=DIRECTION('',(0.755033118392644,0.113858792838765,0.645725301830104));
#56898=DIRECTION('',(-0.755033118392644,0.113858792838765,0.645725301830104));
#56899=DIRECTION('',(-1.,0.,0.));
#56900=DIRECTION('',(0.,-0.17364817766693,-0.984807753012208));
#56901=DIRECTION('',(-0.998052578482888,-0.0108318757168334,-0.0614306198252359));
#56902=DIRECTION('',(-0.957826285221151,0.0498974366850416,0.282982425517402));
#56903=DIRECTION('',(-0.868243142124459,0.0861536225152696,0.488601473065055));
#56904=DIRECTION('',(-0.948683298050514,0.0549123752965085,0.311423555691113));
#56905=DIRECTION('',(-1.,0.,0.));
#56906=DIRECTION('',(-0.948683298050513,-0.0549123752965087,-0.311423555691114));
#56907=DIRECTION('',(-0.86824314212446,-0.0861536225152694,-0.488601473065054));
#56908=DIRECTION('',(-0.957826285221151,-0.0498974366850415,-0.282982425517402));
#56909=DIRECTION('',(-0.998052578482888,0.0108318757168334,0.0614306198252359));
#56910=DIRECTION('',(0.,0.17364817766693,0.984807753012208));
#56911=DIRECTION('',(-1.,0.,0.));
#56912=DIRECTION('',(-0.755033118392643,-0.113858792838765,-0.645725301830105));
#56913=DIRECTION('center_axis',(0.649305557988371,-0.00722457847379224,
0.760493325303573));
#56914=DIRECTION('ref_axis',(0.755033118392643,-0.113858792838765,-0.645725301830105));
#56915=DIRECTION('',(0.,0.999954879404557,0.00949942919436656));
#56916=DIRECTION('',(-0.755033118392643,0.113858792838765,0.645725301830105));
#56917=DIRECTION('center_axis',(-0.649305557988371,0.00722457847379224,
-0.760493325303573));
#56918=DIRECTION('ref_axis',(0.760527640763576,0.00616803217361924,-0.64927626093497));
#56919=DIRECTION('',(0.0519254248777275,0.998042613992818,-0.0348524160661844));
#56920=DIRECTION('center_axis',(-1.,0.,0.));
#56921=DIRECTION('ref_axis',(0.,1.,0.));
#56922=DIRECTION('center_axis',(1.,0.,0.));
#56923=DIRECTION('ref_axis',(0.,1.,0.));
#56924=DIRECTION('center_axis',(-1.,0.,0.));
#56925=DIRECTION('ref_axis',(0.,1.,0.));
#56926=DIRECTION('center_axis',(1.,0.,0.));
#56927=DIRECTION('ref_axis',(0.,1.,0.));
#56928=DIRECTION('center_axis',(-1.,0.,0.));
#56929=DIRECTION('ref_axis',(0.,1.,0.));
#56930=DIRECTION('center_axis',(1.,0.,0.));
#56931=DIRECTION('ref_axis',(0.,1.,0.));
#56932=DIRECTION('center_axis',(-1.,0.,0.));
#56933=DIRECTION('ref_axis',(0.,1.,0.));
#56934=DIRECTION('center_axis',(1.,0.,0.));
#56935=DIRECTION('ref_axis',(0.,1.,0.));
#56936=DIRECTION('center_axis',(-1.,0.,0.));
#56937=DIRECTION('ref_axis',(0.,1.,0.));
#56938=DIRECTION('center_axis',(1.,0.,0.));
#56939=DIRECTION('ref_axis',(0.,1.,0.));
#56940=DIRECTION('center_axis',(-1.,0.,0.));
#56941=DIRECTION('ref_axis',(0.,1.,0.));
#56942=DIRECTION('center_axis',(1.,0.,0.));
#56943=DIRECTION('ref_axis',(0.,1.,0.));
#56944=DIRECTION('center_axis',(-1.,0.,0.));
#56945=DIRECTION('ref_axis',(0.,1.,0.));
#56946=DIRECTION('center_axis',(1.,0.,0.));
#56947=DIRECTION('ref_axis',(0.,1.,0.));
#56948=DIRECTION('center_axis',(-1.,0.,0.));
#56949=DIRECTION('ref_axis',(0.,1.,0.));
#56950=DIRECTION('center_axis',(1.,0.,0.));
#56951=DIRECTION('ref_axis',(0.,1.,0.));
#56952=DIRECTION('center_axis',(-1.,0.,0.));
#56953=DIRECTION('ref_axis',(0.,1.,0.));
#56954=DIRECTION('center_axis',(1.,0.,0.));
#56955=DIRECTION('ref_axis',(0.,1.,0.));
#56956=DIRECTION('center_axis',(-1.,0.,0.));
#56957=DIRECTION('ref_axis',(0.,1.,0.));
#56958=DIRECTION('center_axis',(1.,0.,0.));
#56959=DIRECTION('ref_axis',(0.,1.,0.));
#56960=DIRECTION('center_axis',(-1.,0.,0.));
#56961=DIRECTION('ref_axis',(0.,1.,0.));
#56962=DIRECTION('center_axis',(1.,0.,0.));
#56963=DIRECTION('ref_axis',(0.,1.,0.));
#56964=DIRECTION('center_axis',(-1.,0.,0.));
#56965=DIRECTION('ref_axis',(0.,1.,0.));
#56966=DIRECTION('center_axis',(1.,0.,0.));
#56967=DIRECTION('ref_axis',(0.,1.,0.));
#56968=DIRECTION('center_axis',(-1.,0.,0.));
#56969=DIRECTION('ref_axis',(0.,1.,0.));
#56970=DIRECTION('center_axis',(1.,0.,0.));
#56971=DIRECTION('ref_axis',(0.,1.,0.));
#56972=DIRECTION('center_axis',(-1.,0.,0.));
#56973=DIRECTION('ref_axis',(0.,1.,0.));
#56974=DIRECTION('center_axis',(1.,0.,0.));
#56975=DIRECTION('ref_axis',(0.,1.,0.));
#56976=DIRECTION('center_axis',(-1.,0.,0.));
#56977=DIRECTION('ref_axis',(0.,1.,0.));
#56978=DIRECTION('center_axis',(1.,0.,0.));
#56979=DIRECTION('ref_axis',(0.,1.,0.));
#56980=DIRECTION('center_axis',(-1.,0.,0.));
#56981=DIRECTION('ref_axis',(0.,1.,0.));
#56982=DIRECTION('center_axis',(1.,0.,0.));
#56983=DIRECTION('ref_axis',(0.,1.,0.));
#56984=DIRECTION('center_axis',(-1.,0.,0.));
#56985=DIRECTION('ref_axis',(0.,1.,0.));
#56986=DIRECTION('center_axis',(1.,0.,0.));
#56987=DIRECTION('ref_axis',(0.,1.,0.));
#56988=DIRECTION('center_axis',(-1.,0.,0.));
#56989=DIRECTION('ref_axis',(0.,-1.,5.66553889764798E-16));
#56990=DIRECTION('center_axis',(1.,0.,0.));
#56991=DIRECTION('ref_axis',(0.,1.,0.));
#56992=DIRECTION('center_axis',(-1.,0.,0.));
#56993=DIRECTION('ref_axis',(0.,1.,0.));
#56994=DIRECTION('center_axis',(1.,0.,0.));
#56995=DIRECTION('ref_axis',(0.,1.,0.));
#56996=DIRECTION('center_axis',(-1.,0.,0.));
#56997=DIRECTION('ref_axis',(0.,1.,0.));
#56998=DIRECTION('center_axis',(1.,0.,0.));
#56999=DIRECTION('ref_axis',(0.,1.,0.));
#57000=DIRECTION('center_axis',(-1.,0.,0.));
#57001=DIRECTION('ref_axis',(0.,1.,0.));
#57002=DIRECTION('center_axis',(1.,0.,0.));
#57003=DIRECTION('ref_axis',(0.,1.,0.));
#57004=DIRECTION('center_axis',(-1.,0.,0.));
#57005=DIRECTION('ref_axis',(0.,1.,0.));
#57006=DIRECTION('center_axis',(1.,0.,0.));
#57007=DIRECTION('ref_axis',(0.,1.,0.));
#57008=DIRECTION('center_axis',(-1.,0.,0.));
#57009=DIRECTION('ref_axis',(0.,1.,0.));
#57010=DIRECTION('center_axis',(1.,0.,0.));
#57011=DIRECTION('ref_axis',(0.,1.,0.));
#57012=DIRECTION('center_axis',(-1.,0.,0.));
#57013=DIRECTION('ref_axis',(0.,1.,0.));
#57014=DIRECTION('center_axis',(1.,0.,0.));
#57015=DIRECTION('ref_axis',(0.,1.,0.));
#57016=DIRECTION('center_axis',(-1.,0.,0.));
#57017=DIRECTION('ref_axis',(0.,1.,0.));
#57018=DIRECTION('center_axis',(1.,0.,0.));
#57019=DIRECTION('ref_axis',(0.,1.,0.));
#57020=DIRECTION('center_axis',(-1.,0.,0.));
#57021=DIRECTION('ref_axis',(0.,1.,0.));
#57022=DIRECTION('center_axis',(1.,0.,0.));
#57023=DIRECTION('ref_axis',(0.,1.,0.));
#57024=DIRECTION('center_axis',(-1.,0.,0.));
#57025=DIRECTION('ref_axis',(0.,1.,0.));
#57026=DIRECTION('center_axis',(1.,0.,0.));
#57027=DIRECTION('ref_axis',(0.,1.,0.));
#57028=DIRECTION('center_axis',(-1.,0.,0.));
#57029=DIRECTION('ref_axis',(0.,1.,0.));
#57030=DIRECTION('center_axis',(1.,0.,0.));
#57031=DIRECTION('ref_axis',(0.,1.,0.));
#57032=DIRECTION('center_axis',(-1.,0.,0.));
#57033=DIRECTION('ref_axis',(0.,1.,0.));
#57034=DIRECTION('center_axis',(1.,0.,0.));
#57035=DIRECTION('ref_axis',(0.,1.,0.));
#57036=DIRECTION('center_axis',(-1.,0.,0.));
#57037=DIRECTION('ref_axis',(0.,1.,0.));
#57038=DIRECTION('center_axis',(1.,0.,0.));
#57039=DIRECTION('ref_axis',(0.,1.,0.));
#57040=DIRECTION('center_axis',(-1.,0.,0.));
#57041=DIRECTION('ref_axis',(0.,1.,0.));
#57042=DIRECTION('center_axis',(1.,0.,0.));
#57043=DIRECTION('ref_axis',(0.,1.,0.));
#57044=DIRECTION('center_axis',(-1.,0.,0.));
#57045=DIRECTION('ref_axis',(0.,1.,0.));
#57046=DIRECTION('center_axis',(1.,0.,0.));
#57047=DIRECTION('ref_axis',(0.,1.,0.));
#57048=DIRECTION('center_axis',(-1.,0.,0.));
#57049=DIRECTION('ref_axis',(0.,1.,0.));
#57050=DIRECTION('center_axis',(1.,0.,0.));
#57051=DIRECTION('ref_axis',(0.,1.,0.));
#57052=DIRECTION('center_axis',(-1.,0.,0.));
#57053=DIRECTION('ref_axis',(0.,1.,0.));
#57054=DIRECTION('center_axis',(1.,0.,0.));
#57055=DIRECTION('ref_axis',(0.,1.,0.));
#57056=DIRECTION('center_axis',(-1.,0.,0.));
#57057=DIRECTION('ref_axis',(0.,1.,0.));
#57058=DIRECTION('center_axis',(1.,0.,0.));
#57059=DIRECTION('ref_axis',(0.,1.,0.));
#57060=DIRECTION('center_axis',(-1.,0.,0.));
#57061=DIRECTION('ref_axis',(0.,1.,0.));
#57062=DIRECTION('center_axis',(1.,0.,0.));
#57063=DIRECTION('ref_axis',(0.,1.,0.));
#57064=DIRECTION('center_axis',(-0.649305557988371,-0.139173100960066,-0.747685187986609));
#57065=DIRECTION('ref_axis',(-0.755033118392644,0.,0.655686655446243));
#57066=DIRECTION('',(0.,0.983113759331517,-0.182995454077559));
#57067=DIRECTION('',(0.755033118392644,0.,-0.655686655446243));
#57068=DIRECTION('center_axis',(0.649305557988371,0.139173100960066,0.747685187986609));
#57069=DIRECTION('ref_axis',(-0.760527640763576,0.118819965419165,0.638341228068795));
#57070=DIRECTION('',(-0.0519254248777281,0.98893216263388,-0.138985351600607));
#57071=DIRECTION('center_axis',(-0.649305557988371,-0.00722457847379249,
-0.760493325303573));
#57072=DIRECTION('ref_axis',(-0.755033118392644,-0.113858792838765,0.645725301830105));
#57073=DIRECTION('',(0.,0.999954879404557,-0.00949942919436689));
#57074=DIRECTION('',(0.755033118392644,0.113858792838765,-0.645725301830105));
#57075=DIRECTION('center_axis',(0.649305557988371,0.00722457847379249,0.760493325303573));
#57076=DIRECTION('ref_axis',(-0.760527640763576,0.00616803217361938,0.649276260934969));
#57077=DIRECTION('',(-0.0519254248777281,0.998042613992818,0.0348524160661846));
#57078=DIRECTION('center_axis',(-0.649305557988371,0.124943459173594,-0.75019425775938));
#57079=DIRECTION('ref_axis',(-0.755033118392644,-0.224258043872452,0.616143911670627));
#57080=DIRECTION('',(0.,0.986412876468473,0.164285231037953));
#57081=DIRECTION('',(0.755033118392644,0.224258043872452,-0.616143911670627));
#57082=DIRECTION('center_axis',(0.649305557988371,-0.124943459173594,0.75019425775938));
#57083=DIRECTION('ref_axis',(0.760527640763576,0.106671313608347,-0.640483363162275));
#57084=DIRECTION('',(-0.0519254248777281,0.976828045559515,0.207631210706978));
#57085=DIRECTION('center_axis',(-0.649305557988371,0.253315153038431,-0.717100917309779));
#57086=DIRECTION('ref_axis',(-0.755033118392644,-0.327843327723121,0.567841300538901));
#57087=DIRECTION('',(0.,0.942899217429894,0.333078167657523));
#57088=DIRECTION('',(0.755033118392644,0.327843327723121,-0.567841300538901));
#57089=DIRECTION('center_axis',(0.649305557988371,-0.253315153038431,0.717100917309779));
#57090=DIRECTION('ref_axis',(0.760527640763576,0.216269505504612,-0.612229702500115));
#57091=DIRECTION('',(-0.0519254248777281,0.925933051260728,0.374101236076903));
#57092=DIRECTION('center_axis',(-0.649305557988371,0.373989994161848,-0.662218828358294));
#57093=DIRECTION('ref_axis',(-0.755033118392644,-0.421467257957652,0.502285118831862));
#57094=DIRECTION('',(0.,0.870736042799734,0.491750692698505));
#57095=DIRECTION('',(0.755033118392644,0.421467257957652,-0.502285118831862));
#57096=DIRECTION('center_axis',(0.649305557988371,-0.373989994161848,0.662218828358294));
#57097=DIRECTION('ref_axis',(0.760527640763576,0.31929645791377,-0.565373752130667));
#57098=DIRECTION('',(-0.0519254248777281,0.846904049744115,0.52920438469299));
#57099=DIRECTION('center_axis',(-0.649305557988371,0.483301338560726,-0.587215555406038));
#57100=DIRECTION('ref_axis',(-0.755033118392644,-0.502285118831862,0.421467257957652));
#57101=DIRECTION('',(0.,0.772115994122802,0.6354816217797));
#57102=DIRECTION('',(0.755033118392644,0.502285118831862,-0.421467257957652));
#57103=DIRECTION('center_axis',(0.649305557988371,-0.483301338560726,0.587215555406038));
#57104=DIRECTION('ref_axis',(0.760527640763576,0.412621749021022,-0.501339206395651));
#57105=DIRECTION('',(-0.0519254248777281,0.742142297230154,0.66822792587052));
#57106=DIRECTION('center_axis',(-0.649305557988371,0.577927816349714,-0.494370034948178));
#57107=DIRECTION('ref_axis',(-0.755033118392644,-0.567841300538901,0.327843327723122));
#57108=DIRECTION('',(0.,0.650035591673994,0.759903763352335));
#57109=DIRECTION('',(0.755033118392644,0.567841300538901,-0.327843327723122));
#57110=DIRECTION('center_axis',(0.649305557988371,-0.577927816349714,0.494370034948178));
#57111=DIRECTION('ref_axis',(0.760527640763576,0.49340973708095,-0.422071722564183));
#57112=DIRECTION('',(-0.0519254248777281,0.614830926556978,0.786947699660121));
#57113=DIRECTION('center_axis',(-0.649305557988371,0.654994249884502,-0.386503331141725));
#57114=DIRECTION('ref_axis',(-0.755033118392644,-0.616143911670627,0.224258043872453));
#57115=DIRECTION('',(0.,0.508204186706052,0.861236613605367));
#57116=DIRECTION('',(0.755033118392644,0.616143911670627,-0.224258043872453));
#57117=DIRECTION('center_axis',(0.649305557988371,-0.654994249884502,0.386503331141725));
#57118=DIRECTION('ref_axis',(0.760527640763576,0.559205719957048,-0.329979803021199));
#57119=DIRECTION('',(-0.0519254248777281,0.468838229299828,0.881756465810299));
#57120=DIRECTION('center_axis',(-0.649305557988371,0.712159014579631,-0.266892919198654));
#57121=DIRECTION('ref_axis',(-0.755033118392644,-0.645725301830105,0.113858792838765));
#57122=DIRECTION('',(0.,0.350931254688773,0.936401225160755));
#57123=DIRECTION('',(0.755033118392644,0.645725301830105,-0.113858792838765));
#57124=DIRECTION('center_axis',(0.649305557988371,-0.712159014579631,0.266892919198654));
#57125=DIRECTION('ref_axis',(0.760527640763576,0.608010520003998,-0.227861614141253));
#57126=DIRECTION('',(-0.0519254248777281,0.308600119688995,0.949773507937132));
#57127=DIRECTION('center_axis',(-0.649305557988371,0.747685187986609,-0.139173100960066));
#57128=DIRECTION('ref_axis',(-0.755033118392644,-0.655686655446243,4.01492281917938E-17));
#57129=DIRECTION('',(0.,0.182995454077559,0.983113759331517));
#57130=DIRECTION('',(0.755033118392644,0.655686655446243,-4.01492281917938E-17));
#57131=DIRECTION('center_axis',(0.649305557988371,-0.747685187986609,0.139173100960066));
#57132=DIRECTION('ref_axis',(0.760527640763576,0.638341228068795,-0.118819965419165));
#57133=DIRECTION('',(-0.0519254248777281,0.138985351600607,0.98893216263388));
#57134=DIRECTION('center_axis',(-0.649305557988371,0.760493325303573,-0.00722457847379251));
#57135=DIRECTION('ref_axis',(-0.755033118392644,-0.645725301830105,-0.113858792838765));
#57136=DIRECTION('',(0.,0.00949942919436693,0.999954879404557));
#57137=DIRECTION('',(0.755033118392644,0.645725301830105,0.113858792838765));
#57138=DIRECTION('center_axis',(0.649305557988371,-0.760493325303573,0.00722457847379251));
#57139=DIRECTION('ref_axis',(0.760527640763576,0.649276260934969,-0.00616803217361943));
#57140=DIRECTION('',(-0.0519254248777281,-0.0348524160661846,0.998042613992818));
#57141=DIRECTION('center_axis',(-0.649305557988371,0.75019425775938,0.124943459173594));
#57142=DIRECTION('ref_axis',(-0.755033118392644,-0.616143911670627,-0.224258043872452));
#57143=DIRECTION('',(0.,-0.164285231037953,0.986412876468473));
#57144=DIRECTION('',(0.755033118392644,0.616143911670627,0.224258043872452));
#57145=DIRECTION('center_axis',(0.649305557988371,-0.75019425775938,-0.124943459173594));
#57146=DIRECTION('ref_axis',(0.760527640763576,0.640483363162275,0.106671313608347));
#57147=DIRECTION('',(-0.0519254248777281,-0.207631210706978,0.976828045559515));
#57148=DIRECTION('center_axis',(-0.649305557988371,0.717100917309779,0.253315153038431));
#57149=DIRECTION('ref_axis',(-0.755033118392644,-0.567841300538901,-0.327843327723121));
#57150=DIRECTION('',(0.,-0.333078167657523,0.942899217429894));
#57151=DIRECTION('',(0.755033118392644,0.567841300538901,0.327843327723121));
#57152=DIRECTION('center_axis',(0.649305557988371,-0.717100917309779,-0.253315153038431));
#57153=DIRECTION('ref_axis',(0.760527640763576,0.612229702500115,0.216269505504612));
#57154=DIRECTION('',(-0.0519254248777281,-0.374101236076902,0.925933051260728));
#57155=DIRECTION('center_axis',(-0.649305557988371,0.662218828358294,0.373989994161848));
#57156=DIRECTION('ref_axis',(-0.755033118392644,-0.502285118831862,-0.421467257957652));
#57157=DIRECTION('',(0.,-0.491750692698505,0.870736042799734));
#57158=DIRECTION('',(0.755033118392644,0.502285118831862,0.421467257957652));
#57159=DIRECTION('center_axis',(0.649305557988371,-0.662218828358294,-0.373989994161848));
#57160=DIRECTION('ref_axis',(0.760527640763576,0.565373752130667,0.31929645791377));
#57161=DIRECTION('',(-0.0519254248777281,-0.52920438469299,0.846904049744114));
#57162=DIRECTION('center_axis',(-0.649305557988371,0.587215555406038,0.483301338560726));
#57163=DIRECTION('ref_axis',(-0.755033118392644,-0.421467257957652,-0.502285118831862));
#57164=DIRECTION('',(0.,-0.6354816217797,0.772115994122802));
#57165=DIRECTION('',(0.755033118392644,0.421467257957652,0.502285118831862));
#57166=DIRECTION('center_axis',(0.649305557988371,-0.587215555406038,-0.483301338560726));
#57167=DIRECTION('ref_axis',(0.760527640763576,0.501339206395651,0.412621749021022));
#57168=DIRECTION('',(-0.0519254248777281,-0.66822792587052,0.742142297230154));
#57169=DIRECTION('center_axis',(-0.649305557988371,0.494370034948177,0.577927816349714));
#57170=DIRECTION('ref_axis',(-0.755033118392644,-0.327843327723121,-0.567841300538901));
#57171=DIRECTION('',(0.,-0.759903763352335,0.650035591673993));
#57172=DIRECTION('',(0.755033118392644,0.327843327723121,0.567841300538901));
#57173=DIRECTION('center_axis',(0.649305557988371,-0.494370034948177,-0.577927816349714));
#57174=DIRECTION('ref_axis',(0.760527640763576,0.422071722564183,0.49340973708095));
#57175=DIRECTION('',(-0.0519254248777281,-0.786947699660121,0.614830926556977));
#57176=DIRECTION('center_axis',(-0.649305557988371,0.386503331141725,0.654994249884501));
#57177=DIRECTION('ref_axis',(-0.755033118392644,-0.224258043872452,-0.616143911670627));
#57178=DIRECTION('',(0.,-0.861236613605367,0.508204186706052));
#57179=DIRECTION('',(0.755033118392644,0.224258043872452,0.616143911670627));
#57180=DIRECTION('center_axis',(0.649305557988371,-0.386503331141725,-0.654994249884501));
#57181=DIRECTION('ref_axis',(0.760527640763576,0.329979803021199,0.559205719957048));
#57182=DIRECTION('',(-0.0519254248777281,-0.881756465810299,0.468838229299828));
#57183=DIRECTION('center_axis',(-0.649305557988371,0.266892919198654,0.712159014579631));
#57184=DIRECTION('ref_axis',(-0.755033118392644,-0.113858792838765,-0.645725301830104));
#57185=DIRECTION('',(0.,-0.936401225160755,0.350931254688773));
#57186=DIRECTION('',(0.755033118392644,0.113858792838765,0.645725301830104));
#57187=DIRECTION('center_axis',(0.649305557988371,-0.266892919198654,-0.712159014579631));
#57188=DIRECTION('ref_axis',(0.760527640763576,0.227861614141253,0.608010520003998));
#57189=DIRECTION('',(-0.0519254248777281,-0.949773507937132,0.308600119688995));
#57190=DIRECTION('center_axis',(-0.649305557988371,0.139173100960066,0.747685187986609));
#57191=DIRECTION('ref_axis',(-0.755033118392644,-8.02984563835875E-17,-0.655686655446243));
#57192=DIRECTION('',(0.,-0.983113759331517,0.182995454077559));
#57193=DIRECTION('',(0.755033118392644,8.02984563835875E-17,0.655686655446243));
#57194=DIRECTION('center_axis',(0.649305557988371,-0.139173100960066,-0.747685187986609));
#57195=DIRECTION('ref_axis',(0.760527640763576,0.118819965419165,0.638341228068795));
#57196=DIRECTION('',(-0.0519254248777281,-0.98893216263388,0.138985351600607));
#57197=DIRECTION('center_axis',(-0.649305557988371,0.00722457847379274,
0.760493325303573));
#57198=DIRECTION('ref_axis',(-0.755033118392644,0.113858792838764,-0.645725301830105));
#57199=DIRECTION('',(0.,-0.999954879404557,0.00949942919436722));
#57200=DIRECTION('',(0.755033118392644,-0.113858792838764,0.645725301830105));
#57201=DIRECTION('center_axis',(0.649305557988371,-0.00722457847379274,
-0.760493325303573));
#57202=DIRECTION('ref_axis',(0.760527640763576,0.00616803217361967,0.64927626093497));
#57203=DIRECTION('',(-0.0519254248777282,-0.998042613992818,-0.0348524160661843));
#57204=DIRECTION('center_axis',(-0.649305557988371,-0.124943459173594,0.75019425775938));
#57205=DIRECTION('ref_axis',(-0.755033118392644,0.224258043872452,-0.616143911670627));
#57206=DIRECTION('',(0.,-0.986412876468473,-0.164285231037953));
#57207=DIRECTION('',(0.755033118392644,-0.224258043872452,0.616143911670627));
#57208=DIRECTION('center_axis',(0.649305557988371,0.124943459173594,-0.75019425775938));
#57209=DIRECTION('ref_axis',(-0.760527640763576,0.106671313608347,-0.640483363162275));
#57210=DIRECTION('',(-0.0519254248777281,-0.976828045559515,-0.207631210706978));
#57211=DIRECTION('center_axis',(-0.649305557988371,-0.253315153038431,0.717100917309779));
#57212=DIRECTION('ref_axis',(-0.755033118392644,0.327843327723121,-0.567841300538901));
#57213=DIRECTION('',(0.,-0.942899217429894,-0.333078167657523));
#57214=DIRECTION('',(0.755033118392644,-0.327843327723121,0.567841300538901));
#57215=DIRECTION('center_axis',(0.649305557988371,0.253315153038431,-0.717100917309779));
#57216=DIRECTION('ref_axis',(-0.760527640763576,0.216269505504612,-0.612229702500115));
#57217=DIRECTION('',(-0.0519254248777281,-0.925933051260728,-0.374101236076902));
#57218=DIRECTION('center_axis',(-0.649305557988371,-0.373989994161848,0.662218828358294));
#57219=DIRECTION('ref_axis',(-0.755033118392644,0.421467257957652,-0.502285118831862));
#57220=DIRECTION('',(0.,-0.870736042799734,-0.491750692698505));
#57221=DIRECTION('',(0.755033118392644,-0.421467257957652,0.502285118831862));
#57222=DIRECTION('center_axis',(0.649305557988371,0.373989994161848,-0.662218828358294));
#57223=DIRECTION('ref_axis',(-0.760527640763576,0.31929645791377,-0.565373752130667));
#57224=DIRECTION('',(-0.0519254248777281,-0.846904049744115,-0.52920438469299));
#57225=DIRECTION('center_axis',(-0.649305557988371,-0.483301338560726,0.587215555406038));
#57226=DIRECTION('ref_axis',(-0.755033118392644,0.502285118831862,-0.421467257957652));
#57227=DIRECTION('',(0.,-0.772115994122802,-0.6354816217797));
#57228=DIRECTION('',(0.755033118392644,-0.502285118831862,0.421467257957652));
#57229=DIRECTION('center_axis',(0.649305557988371,0.483301338560726,-0.587215555406038));
#57230=DIRECTION('ref_axis',(-0.760527640763576,0.412621749021022,-0.501339206395651));
#57231=DIRECTION('',(-0.0519254248777281,-0.742142297230154,-0.66822792587052));
#57232=DIRECTION('center_axis',(-0.649305557988371,-0.577927816349714,0.494370034948178));
#57233=DIRECTION('ref_axis',(-0.755033118392644,0.567841300538901,-0.327843327723122));
#57234=DIRECTION('',(0.,-0.650035591673994,-0.759903763352334));
#57235=DIRECTION('',(0.755033118392644,-0.567841300538901,0.327843327723122));
#57236=DIRECTION('center_axis',(0.649305557988371,0.577927816349714,-0.494370034948178));
#57237=DIRECTION('ref_axis',(-0.760527640763576,0.49340973708095,-0.422071722564183));
#57238=DIRECTION('',(-0.0519254248777281,-0.614830926556978,-0.786947699660121));
#57239=DIRECTION('center_axis',(-0.649305557988371,-0.654994249884501,0.386503331141726));
#57240=DIRECTION('ref_axis',(-0.755033118392644,0.616143911670627,-0.224258043872453));
#57241=DIRECTION('',(0.,-0.508204186706052,-0.861236613605367));
#57242=DIRECTION('',(0.755033118392644,-0.616143911670627,0.224258043872453));
#57243=DIRECTION('center_axis',(0.649305557988371,0.654994249884501,-0.386503331141726));
#57244=DIRECTION('ref_axis',(-0.760527640763576,0.559205719957047,-0.329979803021199));
#57245=DIRECTION('',(-0.0519254248777281,-0.468838229299829,-0.881756465810299));
#57246=DIRECTION('center_axis',(-0.649305557988371,-0.712159014579631,0.266892919198654));
#57247=DIRECTION('ref_axis',(-0.755033118392644,0.645725301830105,-0.113858792838765));
#57248=DIRECTION('',(0.,-0.350931254688773,-0.936401225160755));
#57249=DIRECTION('',(0.755033118392644,-0.645725301830105,0.113858792838765));
#57250=DIRECTION('center_axis',(0.649305557988371,0.712159014579631,-0.266892919198654));
#57251=DIRECTION('ref_axis',(-0.760527640763576,0.608010520003998,-0.227861614141253));
#57252=DIRECTION('',(-0.0519254248777281,-0.308600119688995,-0.949773507937132));
#57253=DIRECTION('center_axis',(-0.649305557988371,-0.747685187986609,0.139173100960066));
#57254=DIRECTION('ref_axis',(-0.755033118392644,0.655686655446243,-1.20447684575381E-16));
#57255=DIRECTION('',(0.,-0.18299545407756,-0.983113759331517));
#57256=DIRECTION('',(0.755033118392644,-0.655686655446243,1.20447684575381E-16));
#57257=DIRECTION('center_axis',(0.649305557988371,0.747685187986609,-0.139173100960066));
#57258=DIRECTION('ref_axis',(-0.760527640763576,0.638341228068795,-0.118819965419165));
#57259=DIRECTION('',(-0.0519254248777281,-0.138985351600607,-0.98893216263388));
#57260=DIRECTION('center_axis',(-0.649305557988371,-0.760493325303573,0.00722457847379279));
#57261=DIRECTION('ref_axis',(-0.755033118392644,0.645725301830105,0.113858792838764));
#57262=DIRECTION('',(0.,-0.00949942919436729,-0.999954879404557));
#57263=DIRECTION('',(0.755033118392644,-0.645725301830105,-0.113858792838764));
#57264=DIRECTION('center_axis',(0.649305557988371,0.760493325303573,-0.00722457847379279));
#57265=DIRECTION('ref_axis',(-0.760527640763576,0.649276260934969,-0.00616803217361967));
#57266=DIRECTION('',(-0.0519254248777282,0.0348524160661842,-0.998042613992818));
#57267=DIRECTION('center_axis',(-0.649305557988371,-0.75019425775938,-0.124943459173593));
#57268=DIRECTION('ref_axis',(-0.755033118392644,0.616143911670627,0.224258043872452));
#57269=DIRECTION('',(0.,0.164285231037953,-0.986412876468473));
#57270=DIRECTION('',(0.755033118392644,-0.616143911670627,-0.224258043872452));
#57271=DIRECTION('center_axis',(0.649305557988371,0.75019425775938,0.124943459173593));
#57272=DIRECTION('ref_axis',(-0.760527640763576,0.640483363162275,0.106671313608346));
#57273=DIRECTION('',(-0.0519254248777281,0.207631210706978,-0.976828045559515));
#57274=DIRECTION('center_axis',(-0.649305557988371,-0.717100917309779,-0.253315153038431));
#57275=DIRECTION('ref_axis',(-0.755033118392644,0.567841300538901,0.327843327723122));
#57276=DIRECTION('',(0.,0.333078167657524,-0.942899217429894));
#57277=DIRECTION('',(0.755033118392644,-0.567841300538901,-0.327843327723122));
#57278=DIRECTION('center_axis',(0.649305557988371,0.717100917309779,0.253315153038431));
#57279=DIRECTION('ref_axis',(-0.760527640763576,0.612229702500115,0.216269505504612));
#57280=DIRECTION('',(-0.0519254248777281,0.374101236076903,-0.925933051260727));
#57281=DIRECTION('center_axis',(-0.649305557988371,-0.662218828358294,-0.373989994161848));
#57282=DIRECTION('ref_axis',(-0.755033118392644,0.502285118831863,0.421467257957652));
#57283=DIRECTION('',(0.,0.491750692698505,-0.870736042799734));
#57284=DIRECTION('',(0.755033118392644,-0.502285118831863,-0.421467257957652));
#57285=DIRECTION('center_axis',(0.649305557988371,0.662218828358294,0.373989994161848));
#57286=DIRECTION('ref_axis',(-0.760527640763576,0.565373752130667,0.31929645791377));
#57287=DIRECTION('',(-0.0519254248777281,0.52920438469299,-0.846904049744115));
#57288=DIRECTION('center_axis',(-0.649305557988371,-0.587215555406038,-0.483301338560726));
#57289=DIRECTION('ref_axis',(-0.755033118392644,0.421467257957652,0.502285118831862));
#57290=DIRECTION('',(0.,0.635481621779699,-0.772115994122802));
#57291=DIRECTION('',(0.755033118392644,-0.421467257957652,-0.502285118831862));
#57292=DIRECTION('center_axis',(0.649305557988371,0.587215555406038,0.483301338560726));
#57293=DIRECTION('ref_axis',(-0.760527640763576,0.501339206395651,0.412621749021022));
#57294=DIRECTION('',(-0.0519254248777281,0.66822792587052,-0.742142297230154));
#57295=DIRECTION('center_axis',(-0.649305557988371,-0.494370034948178,-0.577927816349714));
#57296=DIRECTION('ref_axis',(-0.755033118392644,0.327843327723122,0.567841300538901));
#57297=DIRECTION('',(0.,0.759903763352334,-0.650035591673994));
#57298=DIRECTION('',(0.755033118392644,-0.327843327723122,-0.567841300538901));
#57299=DIRECTION('center_axis',(0.649305557988371,0.494370034948178,0.577927816349714));
#57300=DIRECTION('ref_axis',(-0.760527640763576,0.422071722564183,0.49340973708095));
#57301=DIRECTION('',(-0.0519254248777281,0.786947699660121,-0.614830926556978));
#57302=DIRECTION('center_axis',(-0.649305557988371,-0.386503331141726,-0.654994249884501));
#57303=DIRECTION('ref_axis',(-0.755033118392644,0.224258043872453,0.616143911670627));
#57304=DIRECTION('',(0.,0.861236613605367,-0.508204186706052));
#57305=DIRECTION('',(0.755033118392644,-0.224258043872453,-0.616143911670627));
#57306=DIRECTION('center_axis',(0.649305557988371,0.386503331141726,0.654994249884501));
#57307=DIRECTION('ref_axis',(-0.760527640763576,0.329979803021199,0.559205719957047));
#57308=DIRECTION('',(-0.0519254248777281,0.881756465810299,-0.468838229299829));
#57309=DIRECTION('center_axis',(-0.649305557988371,-0.266892919198654,-0.712159014579631));
#57310=DIRECTION('ref_axis',(-0.755033118392644,0.113858792838765,0.645725301830104));
#57311=DIRECTION('',(0.,0.936401225160755,-0.350931254688773));
#57312=DIRECTION('',(0.755033118392644,-0.113858792838765,-0.645725301830104));
#57313=DIRECTION('center_axis',(0.649305557988371,0.266892919198654,0.712159014579631));
#57314=DIRECTION('ref_axis',(-0.760527640763576,0.227861614141253,0.608010520003998));
#57315=DIRECTION('',(-0.0519254248777281,0.949773507937132,-0.308600119688995));
#57316=DIRECTION('center_axis',(-1.,0.,0.));
#57317=DIRECTION('ref_axis',(0.,0.,1.));
#57318=DIRECTION('',(0.,-0.983113759331517,0.182995454077559));
#57319=DIRECTION('',(0.,0.,-1.));
#57320=DIRECTION('center_axis',(-1.,0.,0.));
#57321=DIRECTION('ref_axis',(0.,0.,1.));
#57322=DIRECTION('',(0.,-0.999954879404557,0.00949942919436634));
#57323=DIRECTION('',(0.,0.17364817766693,-0.984807753012208));
#57324=DIRECTION('center_axis',(-1.,0.,0.));
#57325=DIRECTION('ref_axis',(0.,0.,1.));
#57326=DIRECTION('',(0.,-0.986412876468473,-0.164285231037954));
#57327=DIRECTION('',(0.,0.342020143325669,-0.939692620785908));
#57328=DIRECTION('center_axis',(-1.,0.,0.));
#57329=DIRECTION('ref_axis',(0.,0.,1.));
#57330=DIRECTION('',(0.,-0.942899217429894,-0.333078167657524));
#57331=DIRECTION('',(0.,0.5,-0.866025403784439));
#57332=DIRECTION('center_axis',(-1.,0.,0.));
#57333=DIRECTION('ref_axis',(0.,0.,1.));
#57334=DIRECTION('',(0.,-0.870736042799734,-0.491750692698505));
#57335=DIRECTION('',(0.,0.642787609686539,-0.766044443118978));
#57336=DIRECTION('center_axis',(-1.,0.,0.));
#57337=DIRECTION('ref_axis',(0.,0.,1.));
#57338=DIRECTION('',(0.,-0.772115994122802,-0.6354816217797));
#57339=DIRECTION('',(0.,0.766044443118978,-0.642787609686539));
#57340=DIRECTION('center_axis',(-1.,0.,0.));
#57341=DIRECTION('ref_axis',(0.,0.,1.));
#57342=DIRECTION('',(0.,-0.650035591673993,-0.759903763352335));
#57343=DIRECTION('',(0.,0.866025403784439,-0.5));
#57344=DIRECTION('center_axis',(-1.,0.,0.));
#57345=DIRECTION('ref_axis',(0.,0.,1.));
#57346=DIRECTION('',(0.,-0.508204186706051,-0.861236613605368));
#57347=DIRECTION('',(0.,0.939692620785908,-0.342020143325669));
#57348=DIRECTION('center_axis',(-1.,0.,0.));
#57349=DIRECTION('ref_axis',(0.,0.,1.));
#57350=DIRECTION('',(0.,-0.350931254688773,-0.936401225160756));
#57351=DIRECTION('',(0.,0.984807753012208,-0.17364817766693));
#57352=DIRECTION('center_axis',(-1.,0.,0.));
#57353=DIRECTION('ref_axis',(0.,0.,1.));
#57354=DIRECTION('',(0.,-0.182995454077559,-0.983113759331517));
#57355=DIRECTION('',(0.,1.,-6.12323399573677E-17));
#57356=DIRECTION('center_axis',(-1.,0.,0.));
#57357=DIRECTION('ref_axis',(0.,0.,1.));
#57358=DIRECTION('',(0.,-0.00949942919436638,-0.999954879404557));
#57359=DIRECTION('',(0.,0.984807753012208,0.17364817766693));
#57360=DIRECTION('center_axis',(-1.,0.,0.));
#57361=DIRECTION('ref_axis',(0.,0.,1.));
#57362=DIRECTION('',(0.,0.164285231037954,-0.986412876468473));
#57363=DIRECTION('',(0.,0.939692620785908,0.342020143325669));
#57364=DIRECTION('center_axis',(-1.,0.,0.));
#57365=DIRECTION('ref_axis',(0.,0.,1.));
#57366=DIRECTION('',(0.,0.333078167657524,-0.942899217429894));
#57367=DIRECTION('',(0.,0.866025403784439,0.5));
#57368=DIRECTION('center_axis',(-1.,0.,0.));
#57369=DIRECTION('ref_axis',(0.,0.,1.));
#57370=DIRECTION('',(0.,0.491750692698505,-0.870736042799734));
#57371=DIRECTION('',(0.,0.766044443118978,0.642787609686539));
#57372=DIRECTION('center_axis',(-1.,0.,0.));
#57373=DIRECTION('ref_axis',(0.,0.,1.));
#57374=DIRECTION('',(0.,0.6354816217797,-0.772115994122802));
#57375=DIRECTION('',(0.,0.642787609686539,0.766044443118978));
#57376=DIRECTION('center_axis',(-1.,0.,0.));
#57377=DIRECTION('ref_axis',(0.,0.,1.));
#57378=DIRECTION('',(0.,0.759903763352335,-0.650035591673993));
#57379=DIRECTION('',(0.,0.5,0.866025403784439));
#57380=DIRECTION('center_axis',(-1.,0.,0.));
#57381=DIRECTION('ref_axis',(0.,0.,1.));
#57382=DIRECTION('',(0.,0.861236613605368,-0.508204186706051));
#57383=DIRECTION('',(0.,0.342020143325669,0.939692620785908));
#57384=DIRECTION('center_axis',(-1.,0.,0.));
#57385=DIRECTION('ref_axis',(0.,0.,1.));
#57386=DIRECTION('',(0.,0.936401225160755,-0.350931254688773));
#57387=DIRECTION('',(0.,0.173648177666931,0.984807753012208));
#57388=DIRECTION('center_axis',(-1.,0.,0.));
#57389=DIRECTION('ref_axis',(0.,0.,1.));
#57390=DIRECTION('',(0.,0.983113759331517,-0.182995454077559));
#57391=DIRECTION('',(0.,1.22464679914735E-16,1.));
#57392=DIRECTION('center_axis',(-1.,0.,0.));
#57393=DIRECTION('ref_axis',(0.,0.,1.));
#57394=DIRECTION('',(0.,0.999954879404557,-0.00949942919436667));
#57395=DIRECTION('',(0.,-0.17364817766693,0.984807753012208));
#57396=DIRECTION('center_axis',(-1.,0.,0.));
#57397=DIRECTION('ref_axis',(0.,0.,1.));
#57398=DIRECTION('',(0.,0.986412876468473,0.164285231037954));
#57399=DIRECTION('',(0.,-0.342020143325669,0.939692620785909));
#57400=DIRECTION('center_axis',(-1.,0.,0.));
#57401=DIRECTION('ref_axis',(0.,0.,1.));
#57402=DIRECTION('',(0.,0.942899217429894,0.333078167657524));
#57403=DIRECTION('',(0.,-0.5,0.866025403784439));
#57404=DIRECTION('center_axis',(-1.,0.,0.));
#57405=DIRECTION('ref_axis',(0.,0.,1.));
#57406=DIRECTION('',(0.,0.870736042799734,0.491750692698505));
#57407=DIRECTION('',(0.,-0.642787609686539,0.766044443118978));
#57408=DIRECTION('center_axis',(-1.,0.,0.));
#57409=DIRECTION('ref_axis',(0.,0.,1.));
#57410=DIRECTION('',(0.,0.772115994122802,0.6354816217797));
#57411=DIRECTION('',(0.,-0.766044443118978,0.642787609686539));
#57412=DIRECTION('center_axis',(-1.,0.,0.));
#57413=DIRECTION('ref_axis',(0.,0.,1.));
#57414=DIRECTION('',(0.,0.650035591673993,0.759903763352335));
#57415=DIRECTION('',(0.,-0.866025403784438,0.5));
#57416=DIRECTION('center_axis',(-1.,0.,0.));
#57417=DIRECTION('ref_axis',(0.,0.,1.));
#57418=DIRECTION('',(0.,0.508204186706052,0.861236613605367));
#57419=DIRECTION('',(0.,-0.939692620785908,0.342020143325669));
#57420=DIRECTION('center_axis',(-1.,0.,0.));
#57421=DIRECTION('ref_axis',(0.,0.,1.));
#57422=DIRECTION('',(0.,0.350931254688773,0.936401225160756));
#57423=DIRECTION('',(0.,-0.984807753012208,0.17364817766693));
#57424=DIRECTION('center_axis',(-1.,0.,0.));
#57425=DIRECTION('ref_axis',(0.,0.,1.));
#57426=DIRECTION('',(0.,0.182995454077559,0.983113759331517));
#57427=DIRECTION('',(0.,-1.,1.83697019872103E-16));
#57428=DIRECTION('center_axis',(-1.,0.,0.));
#57429=DIRECTION('ref_axis',(0.,0.,1.));
#57430=DIRECTION('',(0.,0.00949942919436674,0.999954879404557));
#57431=DIRECTION('',(0.,-0.984807753012208,-0.17364817766693));
#57432=DIRECTION('center_axis',(-1.,0.,0.));
#57433=DIRECTION('ref_axis',(0.,0.,1.));
#57434=DIRECTION('',(0.,-0.164285231037953,0.986412876468473));
#57435=DIRECTION('',(0.,-0.939692620785909,-0.342020143325668));
#57436=DIRECTION('center_axis',(-1.,0.,0.));
#57437=DIRECTION('ref_axis',(0.,0.,1.));
#57438=DIRECTION('',(0.,-0.333078167657524,0.942899217429894));
#57439=DIRECTION('',(0.,-0.866025403784439,-0.5));
#57440=DIRECTION('center_axis',(-1.,0.,0.));
#57441=DIRECTION('ref_axis',(0.,0.,1.));
#57442=DIRECTION('',(0.,-0.491750692698505,0.870736042799734));
#57443=DIRECTION('',(0.,-0.766044443118978,-0.642787609686539));
#57444=DIRECTION('center_axis',(-1.,0.,0.));
#57445=DIRECTION('ref_axis',(0.,0.,1.));
#57446=DIRECTION('',(0.,-0.6354816217797,0.772115994122802));
#57447=DIRECTION('',(0.,-0.64278760968654,-0.766044443118978));
#57448=DIRECTION('center_axis',(-1.,0.,0.));
#57449=DIRECTION('ref_axis',(0.,0.,1.));
#57450=DIRECTION('',(0.,-0.759903763352335,0.650035591673993));
#57451=DIRECTION('',(0.,-0.5,-0.866025403784438));
#57452=DIRECTION('center_axis',(-1.,0.,0.));
#57453=DIRECTION('ref_axis',(0.,0.,1.));
#57454=DIRECTION('',(0.,-0.861236613605367,0.508204186706052));
#57455=DIRECTION('',(0.,-0.342020143325669,-0.939692620785908));
#57456=DIRECTION('center_axis',(-1.,0.,0.));
#57457=DIRECTION('ref_axis',(0.,0.,1.));
#57458=DIRECTION('',(0.,-0.936401225160756,0.350931254688773));
#57459=DIRECTION('',(0.,-0.17364817766693,-0.984807753012208));
#57460=DIRECTION('center_axis',(0.649305557988371,-0.266892919198654,-0.712159014579631));
#57461=DIRECTION('ref_axis',(-0.755033118392643,-0.113858792838765,-0.645725301830105));
#57462=DIRECTION('',(0.0519254248777275,0.949773507937132,-0.308600119688995));
#57463=DIRECTION('center_axis',(-0.649305557988371,0.266892919198654,0.712159014579631));
#57464=DIRECTION('ref_axis',(0.760527640763576,0.227861614141253,0.608010520003998));
#57465=DIRECTION('',(0.755033118392643,0.113858792838765,0.645725301830105));
#57466=DIRECTION('center_axis',(0.649305557988371,-0.386503331141725,-0.654994249884501));
#57467=DIRECTION('ref_axis',(-0.755033118392643,-0.224258043872453,-0.616143911670627));
#57468=DIRECTION('',(0.0519254248777275,0.881756465810299,-0.468838229299829));
#57469=DIRECTION('center_axis',(-0.649305557988371,0.386503331141725,0.654994249884501));
#57470=DIRECTION('ref_axis',(0.760527640763576,0.329979803021199,0.559205719957048));
#57471=DIRECTION('',(0.755033118392644,0.224258043872453,0.616143911670627));
#57472=DIRECTION('center_axis',(0.649305557988371,-0.494370034948177,-0.577927816349714));
#57473=DIRECTION('ref_axis',(-0.755033118392643,-0.327843327723122,-0.567841300538901));
#57474=DIRECTION('',(0.0519254248777275,0.78694769966012,-0.614830926556978));
#57475=DIRECTION('center_axis',(-0.649305557988371,0.494370034948177,0.577927816349714));
#57476=DIRECTION('ref_axis',(0.760527640763576,0.422071722564183,0.49340973708095));
#57477=DIRECTION('',(0.755033118392644,0.327843327723122,0.567841300538901));
#57478=DIRECTION('center_axis',(0.649305557988371,-0.587215555406037,-0.483301338560726));
#57479=DIRECTION('ref_axis',(-0.755033118392644,-0.421467257957652,-0.502285118831862));
#57480=DIRECTION('',(0.0519254248777275,0.66822792587052,-0.742142297230154));
#57481=DIRECTION('center_axis',(-0.649305557988371,0.587215555406037,0.483301338560726));
#57482=DIRECTION('ref_axis',(0.760527640763576,0.501339206395651,0.412621749021023));
#57483=DIRECTION('',(0.755033118392644,0.421467257957652,0.502285118831862));
#57484=DIRECTION('center_axis',(0.649305557988371,-0.662218828358294,-0.373989994161848));
#57485=DIRECTION('ref_axis',(-0.755033118392643,-0.502285118831863,-0.421467257957652));
#57486=DIRECTION('',(0.0519254248777275,0.52920438469299,-0.846904049744115));
#57487=DIRECTION('center_axis',(-0.649305557988371,0.662218828358294,0.373989994161848));
#57488=DIRECTION('ref_axis',(0.760527640763576,0.565373752130667,0.319296457913771));
#57489=DIRECTION('',(0.755033118392644,0.502285118831863,0.421467257957652));
#57490=DIRECTION('center_axis',(0.649305557988371,-0.717100917309779,-0.253315153038431));
#57491=DIRECTION('ref_axis',(-0.755033118392643,-0.567841300538901,-0.327843327723122));
#57492=DIRECTION('',(0.0519254248777275,0.374101236076903,-0.925933051260727));
#57493=DIRECTION('center_axis',(-0.649305557988371,0.717100917309779,0.253315153038431));
#57494=DIRECTION('ref_axis',(0.760527640763576,0.612229702500115,0.216269505504613));
#57495=DIRECTION('',(0.755033118392644,0.567841300538901,0.327843327723122));
#57496=DIRECTION('center_axis',(0.649305557988371,-0.75019425775938,-0.124943459173594));
#57497=DIRECTION('ref_axis',(-0.755033118392643,-0.616143911670627,-0.224258043872452));
#57498=DIRECTION('',(0.0519254248777275,0.207631210706978,-0.976828045559515));
#57499=DIRECTION('center_axis',(-0.649305557988371,0.75019425775938,0.124943459173594));
#57500=DIRECTION('ref_axis',(0.760527640763576,0.640483363162275,0.106671313608347));
#57501=DIRECTION('',(0.755033118392643,0.616143911670627,0.224258043872452));
#57502=DIRECTION('center_axis',(0.649305557988371,-0.760493325303573,0.00722457847379238));
#57503=DIRECTION('ref_axis',(-0.755033118392643,-0.645725301830105,-0.113858792838764));
#57504=DIRECTION('',(0.0519254248777275,0.0348524160661842,-0.998042613992818));
#57505=DIRECTION('center_axis',(-0.649305557988371,0.760493325303573,-0.00722457847379238));
#57506=DIRECTION('ref_axis',(0.760527640763576,0.64927626093497,-0.00616803217361932));
#57507=DIRECTION('',(0.755033118392643,0.645725301830105,0.113858792838764));
#57508=DIRECTION('center_axis',(0.649305557988371,-0.747685187986609,0.139173100960065));
#57509=DIRECTION('ref_axis',(-0.755033118392643,-0.655686655446243,1.20447684575381E-16));
#57510=DIRECTION('',(0.0519254248777275,-0.138985351600607,-0.98893216263388));
#57511=DIRECTION('center_axis',(-0.649305557988371,0.747685187986609,-0.139173100960065));
#57512=DIRECTION('ref_axis',(0.760527640763576,0.638341228068795,-0.118819965419165));
#57513=DIRECTION('',(0.755033118392644,0.655686655446243,-1.20447684575381E-16));
#57514=DIRECTION('center_axis',(0.649305557988371,-0.712159014579631,0.266892919198654));
#57515=DIRECTION('ref_axis',(-0.755033118392643,-0.645725301830105,0.113858792838765));
#57516=DIRECTION('',(0.0519254248777275,-0.308600119688995,-0.949773507937132));
#57517=DIRECTION('center_axis',(-0.649305557988371,0.712159014579631,-0.266892919198654));
#57518=DIRECTION('ref_axis',(0.760527640763576,0.608010520003998,-0.227861614141252));
#57519=DIRECTION('',(0.755033118392643,0.645725301830105,-0.113858792838765));
#57520=DIRECTION('center_axis',(0.649305557988371,-0.654994249884501,0.386503331141725));
#57521=DIRECTION('ref_axis',(-0.755033118392643,-0.616143911670627,0.224258043872453));
#57522=DIRECTION('',(0.0519254248777275,-0.468838229299829,-0.881756465810299));
#57523=DIRECTION('center_axis',(-0.649305557988371,0.654994249884501,-0.386503331141725));
#57524=DIRECTION('ref_axis',(0.760527640763576,0.559205719957048,-0.329979803021199));
#57525=DIRECTION('',(0.755033118392644,0.616143911670627,-0.224258043872453));
#57526=DIRECTION('center_axis',(0.649305557988371,-0.577927816349714,0.494370034948177));
#57527=DIRECTION('ref_axis',(-0.755033118392643,-0.567841300538901,0.327843327723122));
#57528=DIRECTION('',(0.0519254248777275,-0.614830926556978,-0.78694769966012));
#57529=DIRECTION('center_axis',(-0.649305557988371,0.577927816349714,-0.494370034948177));
#57530=DIRECTION('ref_axis',(0.760527640763576,0.493409737080951,-0.422071722564183));
#57531=DIRECTION('',(0.755033118392644,0.567841300538901,-0.327843327723122));
#57532=DIRECTION('center_axis',(0.649305557988371,-0.483301338560726,0.587215555406037));
#57533=DIRECTION('ref_axis',(-0.755033118392643,-0.502285118831862,0.421467257957652));
#57534=DIRECTION('',(0.0519254248777275,-0.742142297230154,-0.66822792587052));
#57535=DIRECTION('center_axis',(-0.649305557988371,0.483301338560726,-0.587215555406037));
#57536=DIRECTION('ref_axis',(0.760527640763576,0.412621749021023,-0.501339206395651));
#57537=DIRECTION('',(0.755033118392644,0.502285118831862,-0.421467257957652));
#57538=DIRECTION('center_axis',(0.649305557988371,-0.373989994161849,0.662218828358294));
#57539=DIRECTION('ref_axis',(-0.755033118392643,-0.421467257957652,0.502285118831863));
#57540=DIRECTION('',(0.0519254248777275,-0.846904049744115,-0.52920438469299));
#57541=DIRECTION('center_axis',(-0.649305557988371,0.373989994161849,-0.662218828358294));
#57542=DIRECTION('ref_axis',(0.760527640763576,0.319296457913771,-0.565373752130667));
#57543=DIRECTION('',(0.755033118392644,0.421467257957652,-0.502285118831863));
#57544=DIRECTION('center_axis',(0.649305557988371,-0.253315153038431,0.717100917309779));
#57545=DIRECTION('ref_axis',(-0.755033118392643,-0.327843327723121,0.567841300538901));
#57546=DIRECTION('',(0.0519254248777275,-0.925933051260728,-0.374101236076902));
#57547=DIRECTION('center_axis',(-0.649305557988371,0.253315153038431,-0.717100917309779));
#57548=DIRECTION('ref_axis',(0.760527640763576,0.216269505504612,-0.612229702500115));
#57549=DIRECTION('',(0.755033118392644,0.327843327723121,-0.567841300538901));
#57550=DIRECTION('center_axis',(0.649305557988371,-0.124943459173594,0.75019425775938));
#57551=DIRECTION('ref_axis',(-0.755033118392643,-0.224258043872452,0.616143911670627));
#57552=DIRECTION('',(0.0519254248777275,-0.976828045559515,-0.207631210706978));
#57553=DIRECTION('center_axis',(-0.649305557988371,0.124943459173594,-0.75019425775938));
#57554=DIRECTION('ref_axis',(0.760527640763576,0.106671313608347,-0.640483363162275));
#57555=DIRECTION('',(0.755033118392644,0.224258043872452,-0.616143911670627));
#57556=DIRECTION('center_axis',(0.649305557988371,0.00722457847379232,0.760493325303573));
#57557=DIRECTION('ref_axis',(-0.755033118392643,-0.113858792838764,0.645725301830105));
#57558=DIRECTION('',(0.0519254248777275,-0.998042613992818,-0.0348524160661842));
#57559=DIRECTION('center_axis',(-0.649305557988371,-0.00722457847379232,
-0.760493325303573));
#57560=DIRECTION('ref_axis',(-0.760527640763576,0.00616803217361924,0.64927626093497));
#57561=DIRECTION('',(0.755033118392643,0.113858792838764,-0.645725301830105));
#57562=DIRECTION('center_axis',(0.649305557988371,0.139173100960065,0.747685187986609));
#57563=DIRECTION('ref_axis',(-0.755033118392643,8.02984563835875E-17,0.655686655446243));
#57564=DIRECTION('',(0.0519254248777275,-0.98893216263388,0.138985351600607));
#57565=DIRECTION('center_axis',(-0.649305557988371,-0.139173100960065,-0.747685187986609));
#57566=DIRECTION('ref_axis',(-0.760527640763576,0.118819965419165,0.638341228068795));
#57567=DIRECTION('',(0.755033118392644,-8.02984563835875E-17,-0.655686655446243));
#57568=DIRECTION('center_axis',(0.649305557988371,0.266892919198654,0.712159014579631));
#57569=DIRECTION('ref_axis',(-0.755033118392643,0.113858792838765,0.645725301830105));
#57570=DIRECTION('',(0.0519254248777275,-0.949773507937132,0.308600119688995));
#57571=DIRECTION('center_axis',(-0.649305557988371,-0.266892919198654,-0.712159014579631));
#57572=DIRECTION('ref_axis',(-0.760527640763576,0.227861614141253,0.608010520003998));
#57573=DIRECTION('',(0.755033118392644,-0.113858792838765,-0.645725301830105));
#57574=DIRECTION('center_axis',(0.649305557988371,0.386503331141725,0.654994249884502));
#57575=DIRECTION('ref_axis',(-0.755033118392643,0.224258043872453,0.616143911670627));
#57576=DIRECTION('',(0.0519254248777275,-0.881756465810299,0.468838229299828));
#57577=DIRECTION('center_axis',(-0.649305557988371,-0.386503331141725,-0.654994249884502));
#57578=DIRECTION('ref_axis',(-0.760527640763576,0.329979803021199,0.559205719957048));
#57579=DIRECTION('',(0.755033118392643,-0.224258043872453,-0.616143911670627));
#57580=DIRECTION('center_axis',(0.649305557988371,0.494370034948177,0.577927816349714));
#57581=DIRECTION('ref_axis',(-0.755033118392643,0.327843327723122,0.567841300538901));
#57582=DIRECTION('',(0.0519254248777275,-0.786947699660121,0.614830926556978));
#57583=DIRECTION('center_axis',(-0.649305557988371,-0.494370034948177,-0.577927816349714));
#57584=DIRECTION('ref_axis',(-0.760527640763576,0.422071722564183,0.493409737080951));
#57585=DIRECTION('',(0.755033118392644,-0.327843327723122,-0.567841300538901));
#57586=DIRECTION('center_axis',(0.649305557988371,0.587215555406037,0.483301338560726));
#57587=DIRECTION('ref_axis',(-0.755033118392644,0.421467257957652,0.502285118831862));
#57588=DIRECTION('',(0.0519254248777275,-0.66822792587052,0.742142297230154));
#57589=DIRECTION('center_axis',(-0.649305557988371,-0.587215555406037,-0.483301338560726));
#57590=DIRECTION('ref_axis',(-0.760527640763576,0.501339206395651,0.412621749021023));
#57591=DIRECTION('',(0.755033118392644,-0.421467257957652,-0.502285118831862));
#57592=DIRECTION('center_axis',(0.649305557988371,0.662218828358294,0.373989994161849));
#57593=DIRECTION('ref_axis',(-0.755033118392643,0.502285118831863,0.421467257957652));
#57594=DIRECTION('',(0.0519254248777275,-0.52920438469299,0.846904049744115));
#57595=DIRECTION('center_axis',(-0.649305557988371,-0.662218828358294,-0.373989994161849));
#57596=DIRECTION('ref_axis',(-0.760527640763576,0.565373752130667,0.319296457913771));
#57597=DIRECTION('',(0.755033118392644,-0.502285118831863,-0.421467257957652));
#57598=DIRECTION('center_axis',(0.649305557988371,0.717100917309779,0.253315153038431));
#57599=DIRECTION('ref_axis',(-0.755033118392643,0.567841300538901,0.327843327723121));
#57600=DIRECTION('',(0.0519254248777275,-0.374101236076902,0.925933051260728));
#57601=DIRECTION('center_axis',(-0.649305557988371,-0.717100917309779,-0.253315153038431));
#57602=DIRECTION('ref_axis',(-0.760527640763576,0.612229702500115,0.216269505504613));
#57603=DIRECTION('',(0.755033118392644,-0.567841300538901,-0.327843327723121));
#57604=DIRECTION('center_axis',(0.649305557988371,0.75019425775938,0.124943459173594));
#57605=DIRECTION('ref_axis',(-0.755033118392643,0.616143911670627,0.224258043872452));
#57606=DIRECTION('',(0.0519254248777275,-0.207631210706978,0.976828045559515));
#57607=DIRECTION('center_axis',(-0.649305557988371,-0.75019425775938,-0.124943459173594));
#57608=DIRECTION('ref_axis',(-0.760527640763576,0.640483363162275,0.106671313608347));
#57609=DIRECTION('',(0.755033118392644,-0.616143911670627,-0.224258043872452));
#57610=DIRECTION('center_axis',(0.649305557988371,0.760493325303573,-0.0072245784737921));
#57611=DIRECTION('ref_axis',(-0.755033118392643,0.645725301830105,0.113858792838765));
#57612=DIRECTION('',(0.0519254248777275,-0.0348524160661845,0.998042613992818));
#57613=DIRECTION('center_axis',(-0.649305557988371,-0.760493325303573,0.0072245784737921));
#57614=DIRECTION('ref_axis',(-0.760527640763576,0.64927626093497,-0.00616803217361908));
#57615=DIRECTION('',(0.755033118392643,-0.645725301830105,-0.113858792838765));
#57616=DIRECTION('center_axis',(0.649305557988371,0.747685187986609,-0.139173100960065));
#57617=DIRECTION('ref_axis',(-0.755033118392643,0.655686655446243,-4.01492281917938E-17));
#57618=DIRECTION('',(0.0519254248777275,0.138985351600607,0.98893216263388));
#57619=DIRECTION('center_axis',(-0.649305557988371,-0.747685187986609,0.139173100960065));
#57620=DIRECTION('ref_axis',(-0.760527640763576,0.638341228068795,-0.118819965419165));
#57621=DIRECTION('',(0.755033118392644,-0.655686655446243,4.01492281917938E-17));
#57622=DIRECTION('center_axis',(0.649305557988371,0.712159014579631,-0.266892919198654));
#57623=DIRECTION('ref_axis',(-0.755033118392643,0.645725301830105,-0.113858792838765));
#57624=DIRECTION('',(0.0519254248777275,0.308600119688995,0.949773507937132));
#57625=DIRECTION('center_axis',(-0.649305557988371,-0.712159014579631,0.266892919198654));
#57626=DIRECTION('ref_axis',(-0.760527640763576,0.608010520003998,-0.227861614141252));
#57627=DIRECTION('',(0.755033118392643,-0.645725301830105,0.113858792838765));
#57628=DIRECTION('center_axis',(0.649305557988371,0.654994249884502,-0.386503331141725));
#57629=DIRECTION('ref_axis',(-0.755033118392643,0.616143911670627,-0.224258043872453));
#57630=DIRECTION('',(0.0519254248777275,0.468838229299828,0.881756465810299));
#57631=DIRECTION('center_axis',(-0.649305557988371,-0.654994249884502,0.386503331141725));
#57632=DIRECTION('ref_axis',(-0.760527640763576,0.559205719957048,-0.329979803021199));
#57633=DIRECTION('',(0.755033118392644,-0.616143911670627,0.224258043872453));
#57634=DIRECTION('center_axis',(0.649305557988371,0.577927816349714,-0.494370034948177));
#57635=DIRECTION('ref_axis',(-0.755033118392643,0.567841300538901,-0.327843327723122));
#57636=DIRECTION('',(0.0519254248777275,0.614830926556978,0.786947699660121));
#57637=DIRECTION('center_axis',(-0.649305557988371,-0.577927816349714,0.494370034948177));
#57638=DIRECTION('ref_axis',(-0.760527640763576,0.493409737080951,-0.422071722564183));
#57639=DIRECTION('',(0.755033118392644,-0.567841300538901,0.327843327723122));
#57640=DIRECTION('center_axis',(0.649305557988371,0.483301338560726,-0.587215555406037));
#57641=DIRECTION('ref_axis',(-0.755033118392643,0.502285118831863,-0.421467257957652));
#57642=DIRECTION('',(0.0519254248777275,0.742142297230154,0.66822792587052));
#57643=DIRECTION('center_axis',(-0.649305557988371,-0.483301338560726,0.587215555406037));
#57644=DIRECTION('ref_axis',(-0.760527640763576,0.412621749021023,-0.501339206395651));
#57645=DIRECTION('',(0.755033118392644,-0.502285118831863,0.421467257957652));
#57646=DIRECTION('center_axis',(0.649305557988371,0.373989994161849,-0.662218828358294));
#57647=DIRECTION('ref_axis',(-0.755033118392643,0.421467257957652,-0.502285118831863));
#57648=DIRECTION('',(0.0519254248777275,0.846904049744115,0.52920438469299));
#57649=DIRECTION('center_axis',(-0.649305557988371,-0.373989994161849,0.662218828358294));
#57650=DIRECTION('ref_axis',(-0.760527640763576,0.319296457913771,-0.565373752130667));
#57651=DIRECTION('',(0.755033118392644,-0.421467257957652,0.502285118831863));
#57652=DIRECTION('center_axis',(0.649305557988371,0.253315153038431,-0.717100917309779));
#57653=DIRECTION('ref_axis',(-0.755033118392643,0.327843327723122,-0.567841300538901));
#57654=DIRECTION('',(0.0519254248777275,0.925933051260728,0.374101236076902));
#57655=DIRECTION('center_axis',(-0.649305557988371,-0.253315153038431,0.717100917309779));
#57656=DIRECTION('ref_axis',(-0.760527640763576,0.216269505504613,-0.612229702500115));
#57657=DIRECTION('',(0.755033118392644,-0.327843327723122,0.567841300538901));
#57658=DIRECTION('center_axis',(0.649305557988371,0.124943459173594,-0.75019425775938));
#57659=DIRECTION('ref_axis',(-0.755033118392643,0.224258043872452,-0.616143911670627));
#57660=DIRECTION('',(0.0519254248777275,0.976828045559515,0.207631210706978));
#57661=DIRECTION('center_axis',(-0.649305557988371,-0.124943459173594,0.75019425775938));
#57662=DIRECTION('ref_axis',(-0.760527640763576,0.106671313608347,-0.640483363162275));
#57663=DIRECTION('',(0.755033118392644,-0.224258043872452,0.616143911670627));
#57664=DIRECTION('center_axis',(0.649305557988371,-0.00722457847379207,
-0.760493325303573));
#57665=DIRECTION('ref_axis',(-0.755033118392643,0.113858792838765,-0.645725301830105));
#57666=DIRECTION('',(0.0519254248777275,0.998042613992818,0.0348524160661846));
#57667=DIRECTION('center_axis',(-0.649305557988371,0.00722457847379207,
0.760493325303573));
#57668=DIRECTION('ref_axis',(0.760527640763576,0.0061680321736191,0.64927626093497));
#57669=DIRECTION('',(0.755033118392643,-0.113858792838765,0.645725301830105));
#57670=DIRECTION('center_axis',(0.,1.,0.));
#57671=DIRECTION('ref_axis',(1.,0.,0.));
#57672=DIRECTION('',(0.755033118392644,0.,0.655686655446243));
#57673=DIRECTION('center_axis',(1.,0.,0.));
#57674=DIRECTION('ref_axis',(0.,0.,-1.));
#57675=DIRECTION('',(0.,-0.983113759331517,-0.182995454077559));
#57676=DIRECTION('',(0.,0.,1.));
#57677=DIRECTION('center_axis',(1.,0.,0.));
#57678=DIRECTION('ref_axis',(0.,0.,-1.));
#57679=DIRECTION('',(0.,-0.936401225160755,-0.350931254688773));
#57680=DIRECTION('',(0.,-0.17364817766693,0.984807753012208));
#57681=DIRECTION('center_axis',(1.,0.,0.));
#57682=DIRECTION('ref_axis',(0.,0.,-1.));
#57683=DIRECTION('',(0.,-0.861236613605367,-0.508204186706051));
#57684=DIRECTION('',(0.,-0.342020143325669,0.939692620785908));
#57685=DIRECTION('center_axis',(1.,0.,0.));
#57686=DIRECTION('ref_axis',(0.,0.,-1.));
#57687=DIRECTION('',(0.,-0.759903763352335,-0.650035591673993));
#57688=DIRECTION('',(0.,-0.5,0.866025403784439));
#57689=DIRECTION('center_axis',(1.,0.,0.));
#57690=DIRECTION('ref_axis',(0.,0.,-1.));
#57691=DIRECTION('',(0.,-0.6354816217797,-0.772115994122802));
#57692=DIRECTION('',(0.,-0.642787609686539,0.766044443118978));
#57693=DIRECTION('center_axis',(1.,0.,0.));
#57694=DIRECTION('ref_axis',(0.,0.,-1.));
#57695=DIRECTION('',(0.,-0.491750692698505,-0.870736042799734));
#57696=DIRECTION('',(0.,-0.766044443118978,0.642787609686539));
#57697=DIRECTION('center_axis',(1.,0.,0.));
#57698=DIRECTION('ref_axis',(0.,0.,-1.));
#57699=DIRECTION('',(0.,-0.333078167657524,-0.942899217429894));
#57700=DIRECTION('',(0.,-0.866025403784439,0.5));
#57701=DIRECTION('center_axis',(1.,0.,0.));
#57702=DIRECTION('ref_axis',(0.,0.,-1.));
#57703=DIRECTION('',(0.,-0.164285231037954,-0.986412876468473));
#57704=DIRECTION('',(0.,-0.939692620785908,0.342020143325669));
#57705=DIRECTION('center_axis',(1.,0.,0.));
#57706=DIRECTION('ref_axis',(0.,0.,-1.));
#57707=DIRECTION('',(0.,0.00949942919436663,-0.999954879404557));
#57708=DIRECTION('',(0.,-0.984807753012208,0.17364817766693));
#57709=DIRECTION('center_axis',(1.,0.,0.));
#57710=DIRECTION('ref_axis',(0.,0.,-1.));
#57711=DIRECTION('',(0.,0.182995454077559,-0.983113759331517));
#57712=DIRECTION('',(0.,-1.,6.12323399573677E-17));
#57713=DIRECTION('center_axis',(1.,0.,0.));
#57714=DIRECTION('ref_axis',(0.,0.,-1.));
#57715=DIRECTION('',(0.,0.350931254688773,-0.936401225160755));
#57716=DIRECTION('',(0.,-0.984807753012208,-0.17364817766693));
#57717=DIRECTION('center_axis',(1.,0.,0.));
#57718=DIRECTION('ref_axis',(0.,0.,-1.));
#57719=DIRECTION('',(0.,0.508204186706051,-0.861236613605367));
#57720=DIRECTION('',(0.,-0.939692620785908,-0.342020143325669));
#57721=DIRECTION('center_axis',(1.,0.,0.));
#57722=DIRECTION('ref_axis',(0.,0.,-1.));
#57723=DIRECTION('',(0.,0.650035591673993,-0.759903763352335));
#57724=DIRECTION('',(0.,-0.866025403784439,-0.5));
#57725=DIRECTION('center_axis',(1.,0.,0.));
#57726=DIRECTION('ref_axis',(0.,0.,-1.));
#57727=DIRECTION('',(0.,0.772115994122802,-0.6354816217797));
#57728=DIRECTION('',(0.,-0.766044443118978,-0.642787609686539));
#57729=DIRECTION('center_axis',(1.,0.,0.));
#57730=DIRECTION('ref_axis',(0.,0.,-1.));
#57731=DIRECTION('',(0.,0.870736042799734,-0.491750692698505));
#57732=DIRECTION('',(0.,-0.642787609686539,-0.766044443118978));
#57733=DIRECTION('center_axis',(1.,0.,0.));
#57734=DIRECTION('ref_axis',(0.,0.,-1.));
#57735=DIRECTION('',(0.,0.942899217429894,-0.333078167657523));
#57736=DIRECTION('',(0.,-0.5,-0.866025403784439));
#57737=DIRECTION('center_axis',(1.,0.,0.));
#57738=DIRECTION('ref_axis',(0.,0.,-1.));
#57739=DIRECTION('',(0.,0.986412876468473,-0.164285231037954));
#57740=DIRECTION('',(0.,-0.342020143325669,-0.939692620785908));
#57741=DIRECTION('center_axis',(1.,0.,0.));
#57742=DIRECTION('ref_axis',(0.,0.,-1.));
#57743=DIRECTION('',(0.,0.999954879404557,0.00949942919436638));
#57744=DIRECTION('',(0.,-0.173648177666931,-0.984807753012208));
#57745=DIRECTION('center_axis',(1.,0.,0.));
#57746=DIRECTION('ref_axis',(0.,0.,-1.));
#57747=DIRECTION('',(0.,0.983113759331517,0.182995454077559));
#57748=DIRECTION('',(0.,-1.22464679914735E-16,-1.));
#57749=DIRECTION('center_axis',(1.,0.,0.));
#57750=DIRECTION('ref_axis',(0.,0.,-1.));
#57751=DIRECTION('',(0.,0.936401225160756,0.350931254688773));
#57752=DIRECTION('',(0.,0.17364817766693,-0.984807753012208));
#57753=DIRECTION('center_axis',(1.,0.,0.));
#57754=DIRECTION('ref_axis',(0.,0.,-1.));
#57755=DIRECTION('',(0.,0.861236613605368,0.508204186706051));
#57756=DIRECTION('',(0.,0.342020143325669,-0.939692620785909));
#57757=DIRECTION('center_axis',(1.,0.,0.));
#57758=DIRECTION('ref_axis',(0.,0.,-1.));
#57759=DIRECTION('',(0.,0.759903763352335,0.650035591673993));
#57760=DIRECTION('',(0.,0.5,-0.866025403784439));
#57761=DIRECTION('center_axis',(1.,0.,0.));
#57762=DIRECTION('ref_axis',(0.,0.,-1.));
#57763=DIRECTION('',(0.,0.6354816217797,0.772115994122802));
#57764=DIRECTION('',(0.,0.642787609686539,-0.766044443118978));
#57765=DIRECTION('center_axis',(1.,0.,0.));
#57766=DIRECTION('ref_axis',(0.,0.,-1.));
#57767=DIRECTION('',(0.,0.491750692698505,0.870736042799734));
#57768=DIRECTION('',(0.,0.766044443118978,-0.642787609686539));
#57769=DIRECTION('center_axis',(1.,0.,0.));
#57770=DIRECTION('ref_axis',(0.,0.,-1.));
#57771=DIRECTION('',(0.,0.333078167657524,0.942899217429894));
#57772=DIRECTION('',(0.,0.866025403784438,-0.5));
#57773=DIRECTION('center_axis',(1.,0.,0.));
#57774=DIRECTION('ref_axis',(0.,0.,-1.));
#57775=DIRECTION('',(0.,0.164285231037954,0.986412876468473));
#57776=DIRECTION('',(0.,0.939692620785908,-0.342020143325669));
#57777=DIRECTION('center_axis',(1.,0.,0.));
#57778=DIRECTION('ref_axis',(0.,0.,-1.));
#57779=DIRECTION('',(0.,-0.00949942919436674,0.999954879404557));
#57780=DIRECTION('',(0.,0.984807753012208,-0.17364817766693));
#57781=DIRECTION('center_axis',(1.,0.,0.));
#57782=DIRECTION('ref_axis',(0.,0.,-1.));
#57783=DIRECTION('',(0.,-0.182995454077559,0.983113759331517));
#57784=DIRECTION('',(0.,1.,-1.83697019872103E-16));
#57785=DIRECTION('center_axis',(1.,0.,0.));
#57786=DIRECTION('ref_axis',(0.,0.,-1.));
#57787=DIRECTION('',(0.,-0.350931254688773,0.936401225160756));
#57788=DIRECTION('',(0.,0.984807753012208,0.17364817766693));
#57789=DIRECTION('center_axis',(1.,0.,0.));
#57790=DIRECTION('ref_axis',(0.,0.,-1.));
#57791=DIRECTION('',(0.,-0.508204186706051,0.861236613605368));
#57792=DIRECTION('',(0.,0.939692620785909,0.342020143325668));
#57793=DIRECTION('center_axis',(1.,0.,0.));
#57794=DIRECTION('ref_axis',(0.,0.,-1.));
#57795=DIRECTION('',(0.,-0.650035591673993,0.759903763352335));
#57796=DIRECTION('',(0.,0.866025403784439,0.5));
#57797=DIRECTION('center_axis',(1.,0.,0.));
#57798=DIRECTION('ref_axis',(0.,0.,-1.));
#57799=DIRECTION('',(0.,-0.772115994122802,0.6354816217797));
#57800=DIRECTION('',(0.,0.766044443118978,0.642787609686539));
#57801=DIRECTION('center_axis',(1.,0.,0.));
#57802=DIRECTION('ref_axis',(0.,0.,-1.));
#57803=DIRECTION('',(0.,-0.870736042799734,0.491750692698505));
#57804=DIRECTION('',(0.,0.64278760968654,0.766044443118978));
#57805=DIRECTION('center_axis',(1.,0.,0.));
#57806=DIRECTION('ref_axis',(0.,0.,-1.));
#57807=DIRECTION('',(0.,-0.942899217429894,0.333078167657524));
#57808=DIRECTION('',(0.,0.5,0.866025403784438));
#57809=DIRECTION('center_axis',(1.,0.,0.));
#57810=DIRECTION('ref_axis',(0.,0.,-1.));
#57811=DIRECTION('',(0.,-0.986412876468473,0.164285231037954));
#57812=DIRECTION('',(0.,0.342020143325669,0.939692620785908));
#57813=DIRECTION('center_axis',(1.,0.,0.));
#57814=DIRECTION('ref_axis',(0.,0.,-1.));
#57815=DIRECTION('',(0.,-0.999954879404557,-0.00949942919436667));
#57816=DIRECTION('',(0.,0.17364817766693,0.984807753012208));
#57817=DIRECTION('center_axis',(0.,0.984807753012208,-0.17364817766693));
#57818=DIRECTION('ref_axis',(1.,0.,0.));
#57819=DIRECTION('',(-0.755033118392644,-0.113858792838765,-0.645725301830104));
#57820=DIRECTION('center_axis',(0.,0.939692620785908,-0.342020143325669));
#57821=DIRECTION('ref_axis',(1.,0.,0.));
#57822=DIRECTION('',(-0.755033118392644,-0.224258043872453,-0.616143911670627));
#57823=DIRECTION('center_axis',(0.,0.866025403784438,-0.5));
#57824=DIRECTION('ref_axis',(1.,0.,0.));
#57825=DIRECTION('',(-0.755033118392644,-0.327843327723122,-0.567841300538901));
#57826=DIRECTION('center_axis',(0.,0.766044443118978,-0.64278760968654));
#57827=DIRECTION('ref_axis',(1.,0.,0.));
#57828=DIRECTION('',(-0.755033118392644,-0.421467257957652,-0.502285118831862));
#57829=DIRECTION('center_axis',(0.,0.642787609686539,-0.766044443118978));
#57830=DIRECTION('ref_axis',(1.,0.,0.));
#57831=DIRECTION('',(-0.755033118392644,-0.502285118831863,-0.421467257957652));
#57832=DIRECTION('center_axis',(0.,0.5,-0.866025403784439));
#57833=DIRECTION('ref_axis',(1.,0.,0.));
#57834=DIRECTION('',(-0.755033118392644,-0.567841300538901,-0.327843327723122));
#57835=DIRECTION('center_axis',(0.,0.342020143325668,-0.939692620785909));
#57836=DIRECTION('ref_axis',(1.,0.,0.));
#57837=DIRECTION('',(-0.755033118392644,-0.616143911670627,-0.224258043872452));
#57838=DIRECTION('center_axis',(0.,0.17364817766693,-0.984807753012208));
#57839=DIRECTION('ref_axis',(1.,0.,0.));
#57840=DIRECTION('',(-0.755033118392644,-0.645725301830105,-0.113858792838764));
#57841=DIRECTION('center_axis',(0.,-1.83697019872103E-16,-1.));
#57842=DIRECTION('ref_axis',(1.,0.,0.));
#57843=DIRECTION('',(-0.755033118392644,-0.655686655446243,1.20447684575381E-16));
#57844=DIRECTION('center_axis',(0.,-0.17364817766693,-0.984807753012208));
#57845=DIRECTION('ref_axis',(1.,0.,0.));
#57846=DIRECTION('',(-0.755033118392644,-0.645725301830105,0.113858792838765));
#57847=DIRECTION('center_axis',(0.,-0.342020143325669,-0.939692620785908));
#57848=DIRECTION('ref_axis',(1.,0.,0.));
#57849=DIRECTION('',(-0.755033118392644,-0.616143911670627,0.224258043872453));
#57850=DIRECTION('center_axis',(0.,-0.5,-0.866025403784438));
#57851=DIRECTION('ref_axis',(1.,0.,0.));
#57852=DIRECTION('',(-0.755033118392644,-0.567841300538901,0.327843327723122));
#57853=DIRECTION('center_axis',(0.,-0.642787609686539,-0.766044443118978));
#57854=DIRECTION('ref_axis',(1.,0.,0.));
#57855=DIRECTION('',(-0.755033118392644,-0.502285118831862,0.421467257957652));
#57856=DIRECTION('center_axis',(0.,-0.766044443118978,-0.642787609686539));
#57857=DIRECTION('ref_axis',(1.,0.,0.));
#57858=DIRECTION('',(-0.755033118392644,-0.421467257957652,0.502285118831862));
#57859=DIRECTION('center_axis',(0.,-0.866025403784439,-0.5));
#57860=DIRECTION('ref_axis',(1.,0.,0.));
#57861=DIRECTION('',(-0.755033118392644,-0.327843327723121,0.567841300538901));
#57862=DIRECTION('center_axis',(0.,-0.939692620785908,-0.342020143325669));
#57863=DIRECTION('ref_axis',(1.,0.,0.));
#57864=DIRECTION('',(-0.755033118392644,-0.224258043872452,0.616143911670627));
#57865=DIRECTION('center_axis',(0.,-0.984807753012208,-0.17364817766693));
#57866=DIRECTION('ref_axis',(1.,0.,0.));
#57867=DIRECTION('',(-0.755033118392644,-0.113858792838764,0.645725301830105));
#57868=DIRECTION('center_axis',(0.,-1.,1.22464679914735E-16));
#57869=DIRECTION('ref_axis',(1.,0.,0.));
#57870=DIRECTION('',(-0.755033118392644,8.02984563835875E-17,0.655686655446243));
#57871=DIRECTION('center_axis',(0.,-0.984807753012208,0.173648177666931));
#57872=DIRECTION('ref_axis',(1.,0.,0.));
#57873=DIRECTION('',(-0.755033118392644,0.113858792838765,0.645725301830104));
#57874=DIRECTION('center_axis',(0.,-0.939692620785908,0.342020143325669));
#57875=DIRECTION('ref_axis',(1.,0.,0.));
#57876=DIRECTION('',(-0.755033118392644,0.224258043872452,0.616143911670627));
#57877=DIRECTION('center_axis',(0.,-0.866025403784439,0.5));
#57878=DIRECTION('ref_axis',(1.,0.,0.));
#57879=DIRECTION('',(-0.755033118392644,0.327843327723121,0.567841300538901));
#57880=DIRECTION('center_axis',(0.,-0.766044443118978,0.642787609686539));
#57881=DIRECTION('ref_axis',(1.,0.,0.));
#57882=DIRECTION('',(-0.755033118392644,0.421467257957652,0.502285118831862));
#57883=DIRECTION('center_axis',(0.,-0.642787609686539,0.766044443118978));
#57884=DIRECTION('ref_axis',(1.,0.,0.));
#57885=DIRECTION('',(-0.755033118392644,0.502285118831862,0.421467257957652));
#57886=DIRECTION('center_axis',(0.,-0.5,0.866025403784439));
#57887=DIRECTION('ref_axis',(1.,0.,0.));
#57888=DIRECTION('',(-0.755033118392644,0.567841300538901,0.327843327723121));
#57889=DIRECTION('center_axis',(0.,-0.342020143325669,0.939692620785908));
#57890=DIRECTION('ref_axis',(1.,0.,0.));
#57891=DIRECTION('',(-0.755033118392644,0.616143911670627,0.224258043872452));
#57892=DIRECTION('center_axis',(0.,-0.17364817766693,0.984807753012208));
#57893=DIRECTION('ref_axis',(1.,0.,0.));
#57894=DIRECTION('',(-0.755033118392644,0.645725301830105,0.113858792838765));
#57895=DIRECTION('center_axis',(0.,6.12323399573677E-17,1.));
#57896=DIRECTION('ref_axis',(1.,0.,0.));
#57897=DIRECTION('',(-0.755033118392644,0.655686655446243,-4.01492281917938E-17));
#57898=DIRECTION('center_axis',(0.,0.17364817766693,0.984807753012208));
#57899=DIRECTION('ref_axis',(1.,0.,0.));
#57900=DIRECTION('',(-0.755033118392644,0.645725301830105,-0.113858792838765));
#57901=DIRECTION('center_axis',(0.,0.342020143325669,0.939692620785908));
#57902=DIRECTION('ref_axis',(1.,0.,0.));
#57903=DIRECTION('',(-0.755033118392644,0.616143911670627,-0.224258043872453));
#57904=DIRECTION('center_axis',(0.,0.5,0.866025403784439));
#57905=DIRECTION('ref_axis',(1.,0.,0.));
#57906=DIRECTION('',(-0.755033118392644,0.567841300538901,-0.327843327723122));
#57907=DIRECTION('center_axis',(0.,0.642787609686539,0.766044443118978));
#57908=DIRECTION('ref_axis',(1.,0.,0.));
#57909=DIRECTION('',(-0.755033118392644,0.502285118831862,-0.421467257957652));
#57910=DIRECTION('center_axis',(0.,0.766044443118978,0.642787609686539));
#57911=DIRECTION('ref_axis',(1.,0.,0.));
#57912=DIRECTION('',(-0.755033118392644,0.421467257957652,-0.502285118831862));
#57913=DIRECTION('center_axis',(0.,0.866025403784439,0.5));
#57914=DIRECTION('ref_axis',(1.,0.,0.));
#57915=DIRECTION('',(-0.755033118392644,0.327843327723121,-0.567841300538901));
#57916=DIRECTION('center_axis',(0.,0.939692620785908,0.342020143325669));
#57917=DIRECTION('ref_axis',(1.,0.,0.));
#57918=DIRECTION('',(-0.755033118392644,0.224258043872452,-0.616143911670627));
#57919=DIRECTION('center_axis',(0.,0.984807753012208,0.17364817766693));
#57920=DIRECTION('ref_axis',(1.,0.,0.));
#57921=DIRECTION('',(-0.755033118392644,0.113858792838765,-0.645725301830105));
#57922=DIRECTION('center_axis',(0.,1.,0.));
#57923=DIRECTION('ref_axis',(1.,0.,0.));
#57924=DIRECTION('',(-0.755033118392644,0.,-0.655686655446243));
#57925=DIRECTION('center_axis',(0.,0.0348994967025008,0.999390827019096));
#57926=DIRECTION('ref_axis',(1.,0.,0.));
#57927=DIRECTION('',(1.,0.,0.));
#57928=DIRECTION('',(-0.137844537491629,0.989850519773593,-0.0345663418323002));
#57929=DIRECTION('center_axis',(-0.99026806874157,-0.137058748836224,0.0241671553619711));
#57930=DIRECTION('ref_axis',(0.,0.17364817766693,0.984807753012208));
#57931=DIRECTION('center_axis',(0.99026806874157,0.137058748836224,-0.0241671553619711));
#57932=DIRECTION('ref_axis',(-0.139173100960066,0.975223671657125,-0.171958245538724));
#57933=DIRECTION('',(-0.137998583506848,0.989505769153514,-0.0428336755604259));
#57934=DIRECTION('center_axis',(-0.0617712249622997,0.0345646215150942,
0.997491655456914));
#57935=DIRECTION('ref_axis',(0.998052578482889,0.0108318757168334,0.0614306198252359));
#57936=DIRECTION('center_axis',(0.0617712249622997,-0.0345646215150942,
-0.997491655456914));
#57937=DIRECTION('ref_axis',(0.998090334472114,0.00213918413755091,0.061734173069449));
#57938=DIRECTION('',(0.0161503784824051,0.999303943318151,-0.0336272827279997));
#57939=DIRECTION('center_axis',(0.284551435696759,0.0276473787012797,0.958262022045047));
#57940=DIRECTION('ref_axis',(0.957826285221151,-0.0498974366850415,-0.282982425517402));
#57941=DIRECTION('center_axis',(-0.284551435696759,-0.0276473787012797,
-0.958262022045047));
#57942=DIRECTION('ref_axis',(-0.958660774436356,0.00820634526047714,0.284433077286297));
#57943=DIRECTION('',(0.0552259184163645,0.997451314500147,-0.0451771306857534));
#57944=DIRECTION('center_axis',(0.491310548314113,0.012242818584528,0.870898420315706));
#57945=DIRECTION('ref_axis',(0.86824314212446,-0.0861536225152694,-0.488601473065054));
#57946=DIRECTION('center_axis',(-0.491310548314113,-0.012242818584528,-0.870898420315706));
#57947=DIRECTION('ref_axis',(-0.870984468928858,0.00690600823120527,0.491262009456283));
#57948=DIRECTION('',(0.057078643955053,0.997299213951626,-0.0462201931597181));
#57949=DIRECTION('center_axis',(0.313150259135957,0.0260751666684335,0.949345564526583));
#57950=DIRECTION('ref_axis',(0.948683298050513,-0.0549123752965087,-0.311423555691114));
#57951=DIRECTION('center_axis',(-0.313150259135957,-0.0260751666684335,
-0.949345564526583));
#57952=DIRECTION('ref_axis',(-0.949703593340092,0.00859788807423112,0.313032204601348));
#57953=DIRECTION('',(0.0225789275220278,0.999136045839184,-0.0348905995476465));
#57954=DIRECTION('center_axis',(0.,0.034899496702501,0.999390827019096));
#57955=DIRECTION('ref_axis',(1.,0.,0.));
#57956=DIRECTION('',(1.,0.,0.));
#57957=DIRECTION('',(-0.0225789275220274,0.999136045839184,-0.0348905995476465));
#57958=DIRECTION('center_axis',(-0.313150259135956,0.0260751666684337,0.949345564526583));
#57959=DIRECTION('ref_axis',(0.948683298050514,0.0549123752965085,0.311423555691113));
#57960=DIRECTION('center_axis',(0.313150259135956,-0.0260751666684337,-0.949345564526583));
#57961=DIRECTION('ref_axis',(0.949703593340092,0.00859788807423116,0.313032204601347));
#57962=DIRECTION('',(-0.0570786439550527,0.997299213951626,-0.046220193159718));
#57963=DIRECTION('center_axis',(-0.491310548314114,0.0122428185845281,0.870898420315705));
#57964=DIRECTION('ref_axis',(0.868243142124459,0.0861536225152696,0.488601473065055));
#57965=DIRECTION('center_axis',(0.491310548314114,-0.0122428185845281,-0.870898420315705));
#57966=DIRECTION('ref_axis',(0.870984468928858,0.0069060082312054,0.491262009456284));
#57967=DIRECTION('',(-0.0552259184163635,0.997451314500147,-0.045177130685753));
#57968=DIRECTION('center_axis',(-0.284551435696759,0.0276473787012796,0.958262022045047));
#57969=DIRECTION('ref_axis',(0.957826285221151,0.0498974366850416,0.282982425517402));
#57970=DIRECTION('center_axis',(0.284551435696759,-0.0276473787012796,-0.958262022045047));
#57971=DIRECTION('ref_axis',(0.958660774436356,0.00820634526047709,0.284433077286297));
#57972=DIRECTION('',(-0.0161503784824052,0.999303943318151,-0.0336272827279996));
#57973=DIRECTION('center_axis',(0.0617712249622996,0.0345646215150941,0.997491655456914));
#57974=DIRECTION('ref_axis',(0.998052578482889,-0.0108318757168334,-0.0614306198252359));
#57975=DIRECTION('center_axis',(-0.0617712249622996,-0.0345646215150941,
-0.997491655456914));
#57976=DIRECTION('ref_axis',(-0.998090334472114,0.0021391841375509,0.061734173069449));
#57977=DIRECTION('',(0.137998583506848,0.989505769153514,-0.0428336755604258));
#57978=DIRECTION('center_axis',(0.99026806874157,-0.137058748836223,0.0241671553619711));
#57979=DIRECTION('ref_axis',(0.,-0.17364817766693,-0.984807753012208));
#57980=DIRECTION('center_axis',(-0.99026806874157,0.137058748836223,-0.0241671553619711));
#57981=DIRECTION('ref_axis',(0.139173100960065,0.975223671657125,-0.171958245538723));
#57982=DIRECTION('',(0.137844537491629,0.989850519773593,-0.0345663418323004));
#57983=DIRECTION('center_axis',(0.,0.034899496702501,0.999390827019096));
#57984=DIRECTION('ref_axis',(1.,0.,0.));
#57985=DIRECTION('',(1.,0.,0.));
#57986=DIRECTION('',(-0.051925424877728,0.998042613992818,-0.0348524160661846));
#57987=DIRECTION('center_axis',(-0.64930555798837,-0.00722457847379232,
0.760493325303574));
#57988=DIRECTION('ref_axis',(0.755033118392644,0.113858792838765,0.645725301830104));
#57989=DIRECTION('center_axis',(0.64930555798837,0.00722457847379232,-0.760493325303574));
#57990=DIRECTION('ref_axis',(-0.760527640763576,0.00616803217361924,-0.649276260934969));
#57991=DIRECTION('center_axis',(0.,-0.309016994374947,-0.951056516295154));
#57992=DIRECTION('ref_axis',(-1.,0.,0.));
#57993=DIRECTION('',(-1.,0.,0.));
#57994=DIRECTION('',(0.137844537491629,0.941977614300068,-0.306067080296576));
#57995=DIRECTION('center_axis',(0.99026806874157,-0.137058748836223,0.0241671553619711));
#57996=DIRECTION('ref_axis',(0.,-0.17364817766693,-0.984807753012208));
#57997=DIRECTION('center_axis',(-0.99026806874157,0.137058748836223,-0.0241671553619711));
#57998=DIRECTION('ref_axis',(0.139173100960065,0.975223671657125,-0.171958245538723));
#57999=DIRECTION('',(0.137998583506848,0.944481249352984,-0.298180416142191));
#58000=DIRECTION('center_axis',(0.0617712249622996,-0.308682119187541,-0.949157344732972));
#58001=DIRECTION('ref_axis',(-0.998052578482889,-0.0108318757168334,-0.0614306198252359));
#58002=DIRECTION('center_axis',(-0.0617712249622996,0.308682119187541,0.949157344732972));
#58003=DIRECTION('ref_axis',(0.998090334472114,0.0191041551727457,0.0587427909490065));
#58004=DIRECTION('',(-0.0161503784824054,0.950539749516609,-0.310182768482997));
#58005=DIRECTION('center_axis',(-0.284551435696759,-0.301764876373726,-0.909927711321104));
#58006=DIRECTION('ref_axis',(-0.957826285221151,0.0498974366850416,0.282982425517402));
#58007=DIRECTION('center_axis',(0.284551435696759,0.301764876373726,0.909927711321104));
#58008=DIRECTION('ref_axis',(-0.958660774436356,0.0895703997751286,0.27008639921553));
#58009=DIRECTION('',(-0.0552259184163638,0.952749128541176,-0.298695825212034));
#58010=DIRECTION('center_axis',(-0.491310548314114,-0.286360316256975,-0.822564109591763));
#58011=DIRECTION('ref_axis',(-0.868243142124459,0.0861536225152696,0.488601473065055));
#58012=DIRECTION('center_axis',(0.491310548314114,0.286360316256975,0.822564109591763));
#58013=DIRECTION('ref_axis',(-0.870984468928858,0.161531977910744,0.463997279083572));
#58014=DIRECTION('',(-0.0570786439550532,0.952962949154956,-0.297663645650825));
#58015=DIRECTION('center_axis',(-0.313150259135956,-0.30019266434088,-0.901011253802641));
#58016=DIRECTION('ref_axis',(-0.948683298050514,0.0549123752965085,0.311423555691113));
#58017=DIRECTION('center_axis',(0.313150259135956,0.30019266434088,0.901011253802641));
#58018=DIRECTION('ref_axis',(-0.949703593340092,0.0989839475056044,0.297094703643677));
#58019=DIRECTION('',(-0.0225789275220273,0.950814057294297,-0.30893821467004));
#58020=DIRECTION('center_axis',(0.,-0.309016994374947,-0.951056516295154));
#58021=DIRECTION('ref_axis',(-1.,0.,0.));
#58022=DIRECTION('',(-1.,0.,0.));
#58023=DIRECTION('',(0.0225789275220281,0.950814057294297,-0.30893821467004));
#58024=DIRECTION('center_axis',(0.313150259135957,-0.30019266434088,-0.901011253802641));
#58025=DIRECTION('ref_axis',(-0.948683298050513,-0.0549123752965087,-0.311423555691114));
#58026=DIRECTION('center_axis',(-0.313150259135957,0.30019266434088,0.901011253802641));
#58027=DIRECTION('ref_axis',(0.949703593340092,0.0989839475056049,0.297094703643678));
#58028=DIRECTION('',(0.0570786439550533,0.952962949154956,-0.297663645650825));
#58029=DIRECTION('center_axis',(0.491310548314113,-0.286360316256975,-0.822564109591764));
#58030=DIRECTION('ref_axis',(-0.86824314212446,-0.0861536225152694,-0.488601473065054));
#58031=DIRECTION('center_axis',(-0.491310548314113,0.286360316256975,0.822564109591764));
#58032=DIRECTION('ref_axis',(0.870984468928858,0.161531977910744,0.463997279083571));
#58033=DIRECTION('',(0.0552259184163649,0.952749128541176,-0.298695825212034));
#58034=DIRECTION('center_axis',(0.284551435696759,-0.301764876373726,-0.909927711321105));
#58035=DIRECTION('ref_axis',(-0.957826285221151,-0.0498974366850415,-0.282982425517402));
#58036=DIRECTION('center_axis',(-0.284551435696759,0.301764876373726,0.909927711321105));
#58037=DIRECTION('ref_axis',(0.958660774436356,0.0895703997751284,0.270086399215529));
#58038=DIRECTION('',(0.0161503784824051,0.950539749516609,-0.310182768482997));
#58039=DIRECTION('center_axis',(-0.0617712249622997,-0.308682119187541,
-0.949157344732972));
#58040=DIRECTION('ref_axis',(-0.998052578482889,0.0108318757168334,0.0614306198252359));
#58041=DIRECTION('center_axis',(0.0617712249622997,0.308682119187541,0.949157344732972));
#58042=DIRECTION('ref_axis',(-0.998090334472114,0.0191041551727457,0.0587427909490066));
#58043=DIRECTION('',(-0.137998583506848,0.944481249352984,-0.298180416142191));
#58044=DIRECTION('center_axis',(-0.99026806874157,-0.137058748836224,0.0241671553619711));
#58045=DIRECTION('ref_axis',(0.,0.17364817766693,0.984807753012208));
#58046=DIRECTION('center_axis',(0.99026806874157,0.137058748836224,-0.0241671553619711));
#58047=DIRECTION('ref_axis',(-0.139173100960066,0.975223671657125,-0.171958245538724));
#58048=DIRECTION('',(-0.137844537491629,0.941977614300068,-0.306067080296576));
#58049=DIRECTION('center_axis',(0.,-0.309016994374948,-0.951056516295154));
#58050=DIRECTION('ref_axis',(-1.,0.,0.));
#58051=DIRECTION('',(-1.,0.,0.));
#58052=DIRECTION('center_axis',(0.,0.984807753012208,-0.17364817766693));
#58053=DIRECTION('ref_axis',(1.,0.,0.));
#58054=DIRECTION('center_axis',(1.,0.,0.));
#58055=DIRECTION('ref_axis',(0.,1.,0.));
#58056=DIRECTION('center_axis',(1.,0.,0.));
#58057=DIRECTION('ref_axis',(0.,0.,-1.));
#58058=DIRECTION('',(-0.707106781186545,0.70710678118655,8.65956056235496E-17));
#58059=DIRECTION('center_axis',(1.,0.,0.));
#58060=DIRECTION('ref_axis',(0.,0.,-1.));
#58061=DIRECTION('center_axis',(1.,0.,0.));
#58062=DIRECTION('ref_axis',(0.,0.,-1.));
#58063=DIRECTION('center_axis',(1.,0.,0.));
#58064=DIRECTION('ref_axis',(0.,0.,-1.));
#58065=DIRECTION('center_axis',(1.,0.,0.));
#58066=DIRECTION('ref_axis',(0.,0.,-1.));
#58067=DIRECTION('center_axis',(1.,0.,0.));
#58068=DIRECTION('ref_axis',(0.,0.,-1.));
#58069=DIRECTION('center_axis',(1.,0.,0.));
#58070=DIRECTION('ref_axis',(0.,0.,-1.));
#58071=DIRECTION('center_axis',(1.,0.,0.));
#58072=DIRECTION('ref_axis',(0.,0.,-1.));
#58073=DIRECTION('center_axis',(1.,0.,0.));
#58074=DIRECTION('ref_axis',(0.,0.,-1.));
#58075=DIRECTION('center_axis',(1.,0.,0.));
#58076=DIRECTION('ref_axis',(0.,0.,-1.));
#58077=DIRECTION('center_axis',(1.,0.,0.));
#58078=DIRECTION('ref_axis',(0.,0.,-1.));
#58079=DIRECTION('center_axis',(1.,0.,0.));
#58080=DIRECTION('ref_axis',(0.,0.,-1.));
#58081=DIRECTION('center_axis',(1.,0.,0.));
#58082=DIRECTION('ref_axis',(0.,0.,-1.));
#58083=DIRECTION('center_axis',(1.,0.,0.));
#58084=DIRECTION('ref_axis',(0.,0.,-1.));
#58085=DIRECTION('center_axis',(1.,0.,0.));
#58086=DIRECTION('ref_axis',(0.,0.,-1.));
#58087=DIRECTION('center_axis',(1.,0.,0.));
#58088=DIRECTION('ref_axis',(0.,0.,-1.));
#58089=DIRECTION('center_axis',(1.,0.,0.));
#58090=DIRECTION('ref_axis',(0.,0.,-1.));
#58091=DIRECTION('center_axis',(1.,0.,0.));
#58092=DIRECTION('ref_axis',(0.,0.,-1.));
#58093=DIRECTION('center_axis',(1.,0.,0.));
#58094=DIRECTION('ref_axis',(0.,0.,-1.));
#58095=DIRECTION('center_axis',(1.,0.,0.));
#58096=DIRECTION('ref_axis',(0.,0.,-1.));
#58097=DIRECTION('center_axis',(1.,0.,0.));
#58098=DIRECTION('ref_axis',(0.,0.,-1.));
#58099=DIRECTION('center_axis',(1.,0.,0.));
#58100=DIRECTION('ref_axis',(0.,0.,-1.));
#58101=DIRECTION('center_axis',(1.,0.,0.));
#58102=DIRECTION('ref_axis',(0.,0.,-1.));
#58103=DIRECTION('center_axis',(1.,0.,0.));
#58104=DIRECTION('ref_axis',(0.,0.,-1.));
#58105=DIRECTION('center_axis',(1.,0.,0.));
#58106=DIRECTION('ref_axis',(0.,0.,-1.));
#58107=DIRECTION('center_axis',(1.,0.,0.));
#58108=DIRECTION('ref_axis',(0.,0.,-1.));
#58109=DIRECTION('center_axis',(1.,0.,0.));
#58110=DIRECTION('ref_axis',(0.,0.,-1.));
#58111=DIRECTION('center_axis',(1.,0.,0.));
#58112=DIRECTION('ref_axis',(0.,0.,-1.));
#58113=DIRECTION('center_axis',(1.,0.,0.));
#58114=DIRECTION('ref_axis',(0.,0.,-1.));
#58115=DIRECTION('center_axis',(1.,0.,0.));
#58116=DIRECTION('ref_axis',(0.,0.,-1.));
#58117=DIRECTION('center_axis',(1.,0.,0.));
#58118=DIRECTION('ref_axis',(0.,0.,-1.));
#58119=DIRECTION('center_axis',(1.,0.,0.));
#58120=DIRECTION('ref_axis',(0.,0.,-1.));
#58121=DIRECTION('center_axis',(1.,0.,0.));
#58122=DIRECTION('ref_axis',(0.,0.,-1.));
#58123=DIRECTION('center_axis',(1.,0.,0.));
#58124=DIRECTION('ref_axis',(0.,0.,-1.));
#58125=DIRECTION('center_axis',(1.,0.,0.));
#58126=DIRECTION('ref_axis',(0.,0.,-1.));
#58127=DIRECTION('center_axis',(1.,0.,0.));
#58128=DIRECTION('ref_axis',(0.,0.,-1.));
#58129=DIRECTION('center_axis',(1.,0.,0.));
#58130=DIRECTION('ref_axis',(0.,0.,-1.));
#58131=DIRECTION('center_axis',(1.,0.,0.));
#58132=DIRECTION('ref_axis',(0.,1.,0.));
#58133=DIRECTION('center_axis',(1.,0.,0.));
#58134=DIRECTION('ref_axis',(0.,0.,-1.));
#58135=DIRECTION('center_axis',(0.649305557988371,-0.124943459173594,-0.75019425775938));
#58136=DIRECTION('ref_axis',(0.760527640763576,0.106671313608347,0.640483363162275));
#58137=DIRECTION('',(1.,0.,0.));
#58138=DIRECTION('center_axis',(-0.99026806874157,0.130779935984066,-0.0476000039374394));
#58139=DIRECTION('ref_axis',(0.139173100960065,0.930547596796367,-0.338691626801824));
#58140=DIRECTION('center_axis',(-0.0617712249622996,-0.207252115456061,
-0.976335432321108));
#58141=DIRECTION('ref_axis',(-0.998090334472114,0.0128267117770656,0.0604248268374111));
#58142=DIRECTION('center_axis',(0.284551435696759,-0.193627806751036,-0.938902951798372));
#58143=DIRECTION('ref_axis',(0.958660774436356,0.0574729579753757,0.278686882824878));
#58144=DIRECTION('center_axis',(0.491310548314114,-0.163286746281596,-0.855541573276281));
#58145=DIRECTION('ref_axis',(0.870984468928858,0.0921078431475356,0.482599419928604));
#58146=DIRECTION('center_axis',(0.313150259135956,-0.190531153552384,-0.930394967059196));
#58147=DIRECTION('ref_axis',(0.949703593340092,0.0628247387151198,0.306783534438035));
#58148=DIRECTION('',(1.,0.,0.));
#58149=DIRECTION('center_axis',(-0.313150259135957,-0.190531153552384,-0.930394967059195));
#58150=DIRECTION('ref_axis',(-0.949703593340092,0.0628247387151199,0.306783534438037));
#58151=DIRECTION('center_axis',(-0.491310548314113,-0.163286746281596,-0.855541573276282));
#58152=DIRECTION('ref_axis',(-0.870984468928858,0.0921078431475352,0.482599419928602));
#58153=DIRECTION('center_axis',(-0.284551435696759,-0.193627806751036,-0.938902951798373));
#58154=DIRECTION('ref_axis',(-0.958660774436356,0.0574729579753756,0.278686882824878));
#58155=DIRECTION('center_axis',(0.0617712249622997,-0.207252115456061,-0.976335432321108));
#58156=DIRECTION('ref_axis',(0.998090334472114,0.0128267117770656,0.0604248268374111));
#58157=DIRECTION('center_axis',(0.99026806874157,0.130779935984066,-0.0476000039374395));
#58158=DIRECTION('ref_axis',(-0.139173100960066,0.930547596796366,-0.338691626801825));
#58159=DIRECTION('',(1.,0.,0.));
#58160=DIRECTION('center_axis',(0.,0.20791169081776,0.978147600733805));
#58161=DIRECTION('ref_axis',(1.,0.,0.));
#58162=DIRECTION('',(-0.137844537491629,0.968810083928407,-0.205926940351068));
#58163=DIRECTION('center_axis',(-0.99026806874157,-0.130779935984066,0.0476000039374395));
#58164=DIRECTION('ref_axis',(0.,0.342020143325669,0.939692620785908));
#58165=DIRECTION('',(-0.137998583506848,0.967034963408844,-0.21400880938634));
#58166=DIRECTION('center_axis',(-0.0617712249622997,0.207252115456061,0.976335432321108));
#58167=DIRECTION('ref_axis',(0.998052578482889,0.0213346303712045,0.0586164151972949));
#58168=DIRECTION('',(0.0161503784824051,0.978282954629779,-0.206643717435843));
#58169=DIRECTION('center_axis',(0.284551435696759,0.193627806751036,0.938902951798373));
#58170=DIRECTION('ref_axis',(0.957826285221151,-0.0982787650057295,-0.270018687665128));
#58171=DIRECTION('',(0.0552259184163645,0.974452861356161,-0.217696391632611));
#58172=DIRECTION('center_axis',(0.491310548314113,0.163286746281596,0.855541573276282));
#58173=DIRECTION('ref_axis',(0.86824314212446,-0.169689510806249,-0.46621809925847));
#58174=DIRECTION('',(0.057078643955053,0.974121945658943,-0.218697195660775));
#58175=DIRECTION('center_axis',(0.313150259135957,0.190531153552384,0.930394967059195));
#58176=DIRECTION('ref_axis',(0.948683298050513,-0.108156265856636,-0.297156898213637));
#58177=DIRECTION('',(0.0225789275220278,0.977898235227234,-0.207858686543084));
#58178=DIRECTION('center_axis',(0.,0.20791169081776,0.978147600733805));
#58179=DIRECTION('ref_axis',(1.,0.,0.));
#58180=DIRECTION('',(-0.0225789275220274,0.977898235227234,-0.207858686543084));
#58181=DIRECTION('center_axis',(-0.313150259135956,0.190531153552384,0.930394967059196));
#58182=DIRECTION('ref_axis',(0.948683298050514,0.108156265856635,0.297156898213636));
#58183=DIRECTION('',(-0.0570786439550527,0.974121945658943,-0.218697195660775));
#58184=DIRECTION('center_axis',(-0.491310548314114,0.163286746281596,0.855541573276281));
#58185=DIRECTION('ref_axis',(0.868243142124459,0.16968951080625,0.466218099258471));
#58186=DIRECTION('',(-0.0552259184163635,0.974452861356161,-0.217696391632611));
#58187=DIRECTION('center_axis',(-0.284551435696759,0.193627806751036,0.938902951798372));
#58188=DIRECTION('ref_axis',(0.957826285221151,0.0982787650057297,0.270018687665129));
#58189=DIRECTION('',(-0.0161503784824052,0.978282954629779,-0.206643717435843));
#58190=DIRECTION('center_axis',(0.0617712249622996,0.207252115456061,0.976335432321108));
#58191=DIRECTION('ref_axis',(0.998052578482889,-0.0213346303712045,-0.0586164151972949));
#58192=DIRECTION('',(0.137998583506848,0.967034963408844,-0.21400880938634));
#58193=DIRECTION('center_axis',(0.99026806874157,-0.130779935984066,0.0476000039374394));
#58194=DIRECTION('ref_axis',(0.,-0.342020143325669,-0.939692620785908));
#58195=DIRECTION('',(0.137844537491629,0.968810083928407,-0.205926940351068));
#58196=DIRECTION('center_axis',(0.,0.20791169081776,0.978147600733805));
#58197=DIRECTION('ref_axis',(1.,0.,0.));
#58198=DIRECTION('',(-0.0519254248777279,0.976828045559515,-0.207631210706979));
#58199=DIRECTION('center_axis',(-0.649305557988371,0.124943459173594,0.75019425775938));
#58200=DIRECTION('ref_axis',(0.755033118392644,0.224258043872453,0.616143911670627));
#58201=DIRECTION('center_axis',(0.,-0.469471562785891,-0.882947592858927));
#58202=DIRECTION('ref_axis',(-1.,0.,0.));
#58203=DIRECTION('',(-1.,0.,0.));
#58204=DIRECTION('',(0.137844537491629,0.874518866989312,-0.464989929744128));
#58205=DIRECTION('center_axis',(0.99026806874157,-0.130779935984066,0.0476000039374394));
#58206=DIRECTION('ref_axis',(0.,-0.342020143325669,-0.939692620785908));
#58207=DIRECTION('center_axis',(-0.99026806874157,0.130779935984066,-0.0476000039374394));
#58208=DIRECTION('ref_axis',(0.139173100960065,0.930547596796367,-0.338691626801824));
#58209=DIRECTION('',(0.137998583506848,0.878353971058416,-0.457657833403968));
#58210=DIRECTION('center_axis',(0.0617712249622996,-0.468811987424192,-0.881135424446229));
#58211=DIRECTION('ref_axis',(-0.998052578482889,-0.0213346303712045,-0.0586164151972949));
#58212=DIRECTION('center_axis',(-0.0617712249622996,0.468811987424192,0.881135424446229));
#58213=DIRECTION('ref_axis',(0.998090334472114,0.0290144987282327,0.0545329542285434));
#58214=DIRECTION('',(-0.0161503784824054,0.882236242379483,-0.470529890556387));
#58215=DIRECTION('center_axis',(-0.284551435696759,-0.455187678719167,-0.843702943923493));
#58216=DIRECTION('ref_axis',(-0.957826285221151,0.0982787650057297,0.270018687665129));
#58217=DIRECTION('center_axis',(0.284551435696759,0.455187678719167,0.843702943923493));
#58218=DIRECTION('ref_axis',(-0.958660774436356,0.13510963517535,0.250429443236754));
#58219=DIRECTION('',(-0.0552259184163638,0.886406742738185,-0.459601114406123));
#58220=DIRECTION('center_axis',(-0.491310548314114,-0.424846618249728,-0.760341565401402));
#58221=DIRECTION('ref_axis',(-0.868243142124459,0.16968951080625,0.466218099258471));
#58222=DIRECTION('center_axis',(0.491310548314114,0.424846618249728,0.760341565401402));
#58223=DIRECTION('ref_axis',(-0.870984468928858,0.239650226161174,0.428898384218936));
#58224=DIRECTION('',(-0.0570786439550532,0.886796551036219,-0.458621745531674));
#58225=DIRECTION('center_axis',(-0.313150259135956,-0.452091025520515,-0.835194959184317));
#58226=DIRECTION('ref_axis',(-0.948683298050514,0.108156265856635,0.297156898213636));
#58227=DIRECTION('center_axis',(0.313150259135956,0.452091025520515,0.835194959184317));
#58228=DIRECTION('ref_axis',(-0.949703593340092,0.149070112809494,0.27539278542453));
#58229=DIRECTION('',(-0.0225789275220273,0.88272249730729,-0.469351877358061));
#58230=DIRECTION('center_axis',(0.,-0.469471562785891,-0.882947592858927));
#58231=DIRECTION('ref_axis',(-1.,0.,0.));
#58232=DIRECTION('',(-1.,0.,0.));
#58233=DIRECTION('',(0.0225789275220281,0.88272249730729,-0.469351877358061));
#58234=DIRECTION('center_axis',(0.313150259135957,-0.452091025520515,-0.835194959184316));
#58235=DIRECTION('ref_axis',(-0.948683298050513,-0.108156265856636,-0.297156898213637));
#58236=DIRECTION('center_axis',(-0.313150259135957,0.452091025520515,0.835194959184316));
#58237=DIRECTION('ref_axis',(0.949703593340092,0.149070112809495,0.275392785424531));
#58238=DIRECTION('',(0.0570786439550534,0.886796551036219,-0.458621745531674));
#58239=DIRECTION('center_axis',(0.491310548314113,-0.424846618249728,-0.760341565401403));
#58240=DIRECTION('ref_axis',(-0.86824314212446,-0.169689510806249,-0.46621809925847));
#58241=DIRECTION('center_axis',(-0.491310548314113,0.424846618249728,0.760341565401403));
#58242=DIRECTION('ref_axis',(0.870984468928858,0.239650226161174,0.428898384218935));
#58243=DIRECTION('',(0.0552259184163649,0.886406742738185,-0.459601114406122));
#58244=DIRECTION('center_axis',(0.284551435696759,-0.455187678719167,-0.843702943923494));
#58245=DIRECTION('ref_axis',(-0.957826285221151,-0.0982787650057295,-0.270018687665128));
#58246=DIRECTION('center_axis',(-0.284551435696759,0.455187678719167,0.843702943923494));
#58247=DIRECTION('ref_axis',(0.958660774436356,0.135109635175349,0.250429443236754));
#58248=DIRECTION('',(0.0161503784824051,0.882236242379483,-0.470529890556387));
#58249=DIRECTION('center_axis',(-0.0617712249622997,-0.468811987424192,
-0.881135424446229));
#58250=DIRECTION('ref_axis',(-0.998052578482889,0.0213346303712045,0.0586164151972949));
#58251=DIRECTION('center_axis',(0.0617712249622997,0.468811987424192,0.881135424446229));
#58252=DIRECTION('ref_axis',(-0.998090334472114,0.0290144987282328,0.0545329542285435));
#58253=DIRECTION('',(-0.137998583506848,0.878353971058416,-0.457657833403968));
#58254=DIRECTION('center_axis',(-0.99026806874157,-0.130779935984066,0.0476000039374395));
#58255=DIRECTION('ref_axis',(0.,0.342020143325669,0.939692620785908));
#58256=DIRECTION('center_axis',(0.99026806874157,0.130779935984066,-0.0476000039374395));
#58257=DIRECTION('ref_axis',(-0.139173100960066,0.930547596796366,-0.338691626801825));
#58258=DIRECTION('',(-0.137844537491629,0.874518866989312,-0.464989929744128));
#58259=DIRECTION('center_axis',(0.,-0.469471562785892,-0.882947592858927));
#58260=DIRECTION('ref_axis',(-1.,0.,0.));
#58261=DIRECTION('',(-1.,0.,0.));
#58262=DIRECTION('center_axis',(0.,0.939692620785908,-0.342020143325669));
#58263=DIRECTION('ref_axis',(1.,0.,0.));
#58264=DIRECTION('center_axis',(1.,0.,0.));
#58265=DIRECTION('ref_axis',(0.,1.,0.));
#58266=DIRECTION('center_axis',(1.,0.,0.));
#58267=DIRECTION('ref_axis',(0.,0.,-1.));
#58268=DIRECTION('center_axis',(0.64930555798837,-0.253315153038432,-0.717100917309779));
#58269=DIRECTION('ref_axis',(0.760527640763576,0.216269505504613,0.612229702500115));
#58270=DIRECTION('',(1.,0.,0.));
#58271=DIRECTION('center_axis',(-0.99026806874157,0.120527440954873,-0.0695865504800327));
#58272=DIRECTION('ref_axis',(0.139173100960065,0.857597304086756,-0.495134034370783));
#58273=DIRECTION('center_axis',(-0.0617712249622996,-0.373642358743525,
-0.925513751123792));
#58274=DIRECTION('ref_axis',(-0.998090334472114,0.0231245062698635,0.0572795028183562));
#58275=DIRECTION('center_axis',(0.284551435696759,-0.353724951873058,-0.891015790469123));
#58276=DIRECTION('ref_axis',(0.958660774436356,0.104993283944912,0.264472928451193));
#58277=DIRECTION('center_axis',(0.491310548314114,-0.309369288819978,-0.814189528457782));
#58278=DIRECTION('ref_axis',(0.870984468928858,0.174511027858645,0.459273291233482));
#58279=DIRECTION('center_axis',(0.313150259135956,-0.34919794774906,-0.883174789320284));
#58280=DIRECTION('ref_axis',(0.949703593340092,0.115142691461001,0.291213401820783));
#58281=DIRECTION('',(1.,0.,0.));
#58282=DIRECTION('center_axis',(-0.313150259135957,-0.34919794774906,-0.883174789320284));
#58283=DIRECTION('ref_axis',(-0.949703593340092,0.115142691461001,0.291213401820784));
#58284=DIRECTION('center_axis',(-0.491310548314113,-0.309369288819978,-0.814189528457783));
#58285=DIRECTION('ref_axis',(-0.870984468928858,0.174511027858645,0.459273291233481));
#58286=DIRECTION('center_axis',(-0.284551435696759,-0.353724951873058,-0.891015790469123));
#58287=DIRECTION('ref_axis',(-0.958660774436356,0.104993283944912,0.264472928451192));
#58288=DIRECTION('center_axis',(0.0617712249622997,-0.373642358743525,-0.925513751123792));
#58289=DIRECTION('ref_axis',(0.998090334472114,0.0231245062698635,0.0572795028183562));
#58290=DIRECTION('center_axis',(0.99026806874157,0.120527440954873,-0.0695865504800329));
#58291=DIRECTION('ref_axis',(-0.139173100960066,0.857597304086755,-0.495134034370784));
#58292=DIRECTION('',(1.,0.,0.));
#58293=DIRECTION('center_axis',(0.,0.374606593415912,0.927183854566787));
#58294=DIRECTION('ref_axis',(1.,0.,0.));
#58295=DIRECTION('',(-0.137844537491629,0.918332843924613,-0.371030552991328));
#58296=DIRECTION('center_axis',(-0.99026806874157,-0.120527440954873,0.0695865504800329));
#58297=DIRECTION('ref_axis',(0.,0.5,0.866025403784438));
#58298=DIRECTION('',(-0.137998583506848,0.9151812896443,-0.378681393832731));
#58299=DIRECTION('center_axis',(-0.0617712249622997,0.373642358743525,0.925513751123792));
#58300=DIRECTION('ref_axis',(0.998052578482889,0.0311891430775903,0.0540211804549215));
#58301=DIRECTION('',(0.0161503784824051,0.927537333400043,-0.373381387356163));
#58302=DIRECTION('center_axis',(0.284551435696759,0.353724951873058,0.891015790469123));
#58303=DIRECTION('ref_axis',(0.957826285221151,-0.143673942783173,-0.248850568624199));
#58304=DIRECTION('',(0.0552259184163645,0.921846151116809,-0.383601057879401));
#58305=DIRECTION('center_axis',(0.491310548314113,0.309369288819978,0.814189528457783));
#58306=DIRECTION('ref_axis',(0.86824314212446,-0.248069469178416,-0.429668924423658));
#58307=DIRECTION('',(0.057078643955053,0.921346474976903,-0.384529194537799));
#58308=DIRECTION('center_axis',(0.313150259135957,0.34919794774906,0.883174789320284));
#58309=DIRECTION('ref_axis',(0.948683298050513,-0.15811388300842,-0.273861278752584));
#58310=DIRECTION('',(0.0225789275220278,0.926947481578288,-0.37451109252948));
#58311=DIRECTION('center_axis',(0.,0.374606593415913,0.927183854566787));
#58312=DIRECTION('ref_axis',(1.,0.,0.));
#58313=DIRECTION('',(-0.0225789275220274,0.926947481578288,-0.37451109252948));
#58314=DIRECTION('center_axis',(-0.313150259135956,0.34919794774906,0.883174789320284));
#58315=DIRECTION('ref_axis',(0.948683298050514,0.158113883008419,0.273861278752584));
#58316=DIRECTION('',(-0.0570786439550527,0.921346474976903,-0.384529194537799));
#58317=DIRECTION('center_axis',(-0.491310548314114,0.309369288819978,0.814189528457782));
#58318=DIRECTION('ref_axis',(0.86824314212446,0.248069469178417,0.429668924423659));
#58319=DIRECTION('',(-0.0552259184163635,0.921846151116809,-0.3836010578794));
#58320=DIRECTION('center_axis',(-0.284551435696759,0.353724951873058,0.891015790469123));
#58321=DIRECTION('ref_axis',(0.957826285221151,0.143673942783173,0.248850568624199));
#58322=DIRECTION('',(-0.0161503784824052,0.927537333400043,-0.373381387356163));
#58323=DIRECTION('center_axis',(0.0617712249622996,0.373642358743525,0.925513751123792));
#58324=DIRECTION('ref_axis',(0.998052578482889,-0.0311891430775903,-0.0540211804549214));
#58325=DIRECTION('',(0.137998583506848,0.9151812896443,-0.378681393832731));
#58326=DIRECTION('center_axis',(0.99026806874157,-0.120527440954873,0.0695865504800327));
#58327=DIRECTION('ref_axis',(0.,-0.5,-0.866025403784438));
#58328=DIRECTION('',(0.137844537491629,0.918332843924613,-0.371030552991328));
#58329=DIRECTION('center_axis',(0.,0.374606593415913,0.927183854566787));
#58330=DIRECTION('ref_axis',(1.,0.,0.));
#58331=DIRECTION('',(-0.051925424877728,0.925933051260727,-0.374101236076903));
#58332=DIRECTION('center_axis',(-0.64930555798837,0.253315153038432,0.717100917309779));
#58333=DIRECTION('ref_axis',(0.755033118392644,0.327843327723122,0.567841300538901));
#58334=DIRECTION('center_axis',(0.,-0.615661475325659,-0.788010753606722));
#58335=DIRECTION('ref_axis',(-1.,0.,0.));
#58336=DIRECTION('',(-1.,0.,0.));
#58337=DIRECTION('',(0.137844537491629,0.780488306432985,-0.609784295472662));
#58338=DIRECTION('center_axis',(0.99026806874157,-0.120527440954873,0.0695865504800328));
#58339=DIRECTION('ref_axis',(0.,-0.5,-0.866025403784438));
#58340=DIRECTION('center_axis',(-0.99026806874157,0.120527440954873,-0.0695865504800328));
#58341=DIRECTION('ref_axis',(0.139173100960065,0.857597304086756,-0.495134034370783));
#58342=DIRECTION('',(0.137998583506848,0.785538351821794,-0.603229548983803));
#58343=DIRECTION('center_axis',(0.0617712249622996,-0.614697240653271,-0.786340650163726));
#58344=DIRECTION('ref_axis',(-0.998052578482889,-0.0311891430775903,-0.0540211804549214));
#58345=DIRECTION('center_axis',(-0.0617712249622996,0.614697240653271,0.786340650163726));
#58346=DIRECTION('ref_axis',(0.998090334472114,0.0380432514219071,0.0486661612888523));
#58347=DIRECTION('',(-0.0161503784824054,0.787126433450736,-0.616580200004833));
#58348=DIRECTION('center_axis',(-0.284551435696759,-0.594779833782805,-0.751842689509057));
#58349=DIRECTION('ref_axis',(-0.957826285221151,0.143673942783173,0.248850568624199));
#58350=DIRECTION('center_axis',(0.284551435696759,0.594779833782805,0.751842689509057));
#58351=DIRECTION('ref_axis',(-0.958660774436356,0.176543632679542,0.223163315348643));
#58352=DIRECTION('',(-0.0552259184163638,0.793131336600549,-0.606541656308366));
#58353=DIRECTION('center_axis',(-0.491310548314114,-0.550424170729724,-0.675016427497717));
#58354=DIRECTION('ref_axis',(-0.86824314212446,0.248069469178417,0.429668924423659));
#58355=DIRECTION('center_axis',(0.491310548314114,0.550424170729724,0.675016427497717));
#58356=DIRECTION('ref_axis',(-0.870984468928858,0.310486823558562,0.380767628982861));
#58357=DIRECTION('',(-0.0570786439550532,0.793685288454953,-0.605644855748342));
#58358=DIRECTION('center_axis',(-0.313150259135956,-0.590252829658806,-0.744001688360219));
#58359=DIRECTION('ref_axis',(-0.948683298050514,0.158113883008419,0.273861278752584));
#58360=DIRECTION('center_axis',(0.313150259135956,0.590252829658806,0.744001688360219));
#58361=DIRECTION('ref_axis',(-0.949703593340092,0.194626858168784,0.245323196775732));
#58362=DIRECTION('',(-0.0225789275220273,0.787809860918737,-0.615504520756066));
#58363=DIRECTION('center_axis',(0.,-0.615661475325659,-0.788010753606722));
#58364=DIRECTION('ref_axis',(-1.,0.,0.));
#58365=DIRECTION('',(-1.,0.,0.));
#58366=DIRECTION('',(0.0225789275220281,0.787809860918737,-0.615504520756066));
#58367=DIRECTION('center_axis',(0.313150259135957,-0.590252829658806,-0.744001688360218));
#58368=DIRECTION('ref_axis',(-0.948683298050513,-0.15811388300842,-0.273861278752584));
#58369=DIRECTION('center_axis',(-0.313150259135957,0.590252829658806,0.744001688360218));
#58370=DIRECTION('ref_axis',(0.949703593340092,0.194626858168784,0.245323196775733));
#58371=DIRECTION('',(0.0570786439550533,0.793685288454953,-0.605644855748343));
#58372=DIRECTION('center_axis',(0.491310548314113,-0.550424170729725,-0.675016427497717));
#58373=DIRECTION('ref_axis',(-0.86824314212446,-0.248069469178416,-0.429668924423658));
#58374=DIRECTION('center_axis',(-0.491310548314113,0.550424170729725,0.675016427497717));
#58375=DIRECTION('ref_axis',(0.870984468928858,0.310486823558562,0.38076762898286));
#58376=DIRECTION('',(0.0552259184163649,0.793131336600549,-0.606541656308365));
#58377=DIRECTION('center_axis',(0.284551435696759,-0.594779833782805,-0.751842689509057));
#58378=DIRECTION('ref_axis',(-0.957826285221151,-0.143673942783173,-0.248850568624199));
#58379=DIRECTION('center_axis',(-0.284551435696759,0.594779833782805,0.751842689509057));
#58380=DIRECTION('ref_axis',(0.958660774436356,0.176543632679541,0.223163315348643));
#58381=DIRECTION('',(0.0161503784824051,0.787126433450736,-0.616580200004833));
#58382=DIRECTION('center_axis',(-0.0617712249622997,-0.614697240653271,
-0.786340650163726));
#58383=DIRECTION('ref_axis',(-0.998052578482889,0.0311891430775903,0.0540211804549215));
#58384=DIRECTION('center_axis',(0.0617712249622997,0.614697240653271,0.786340650163726));
#58385=DIRECTION('ref_axis',(-0.998090334472114,0.0380432514219072,0.0486661612888524));
#58386=DIRECTION('',(-0.137998583506848,0.785538351821794,-0.603229548983803));
#58387=DIRECTION('center_axis',(-0.99026806874157,-0.120527440954873,0.0695865504800329));
#58388=DIRECTION('ref_axis',(0.,0.5,0.866025403784438));
#58389=DIRECTION('center_axis',(0.99026806874157,0.120527440954873,-0.0695865504800329));
#58390=DIRECTION('ref_axis',(-0.139173100960066,0.857597304086755,-0.495134034370784));
#58391=DIRECTION('',(-0.137844537491629,0.780488306432985,-0.609784295472662));
#58392=DIRECTION('center_axis',(0.,-0.615661475325659,-0.788010753606722));
#58393=DIRECTION('ref_axis',(-1.,0.,0.));
#58394=DIRECTION('',(-1.,0.,0.));
#58395=DIRECTION('center_axis',(0.,0.866025403784438,-0.5));
#58396=DIRECTION('ref_axis',(1.,0.,0.));
#58397=DIRECTION('center_axis',(1.,0.,0.));
#58398=DIRECTION('ref_axis',(0.,1.,0.));
#58399=DIRECTION('center_axis',(1.,0.,0.));
#58400=DIRECTION('ref_axis',(0.,0.,-1.));
#58401=DIRECTION('center_axis',(0.64930555798837,-0.373989994161849,-0.662218828358294));
#58402=DIRECTION('ref_axis',(0.760527640763576,0.319296457913771,0.565373752130667));
#58403=DIRECTION('',(1.,0.,0.));
#58404=DIRECTION('center_axis',(-0.99026806874157,0.106612780622095,-0.0894587448987839));
#58405=DIRECTION('ref_axis',(0.139173100960065,0.758589351257639,-0.636532044855303));
#58406=DIRECTION('center_axis',(-0.0617712249622996,-0.528679668032723,
-0.846570802931135));
#58407=DIRECTION('ref_axis',(-0.998090334472114,0.0327196743412163,0.0523937700909925));
#58408=DIRECTION('center_axis',(0.284551435696759,-0.50307434332588,-0.816055565222214));
#58409=DIRECTION('ref_axis',(0.958660774436356,0.149323442110948,0.242223097976277));
#58410=DIRECTION('center_axis',(0.491310548314114,-0.446051802065978,-0.748098746816874));
#58411=DIRECTION('ref_axis',(0.870984468928858,0.25161178329511,0.42199237598773));
#58412=DIRECTION('center_axis',(0.313150259135956,-0.497254539006069,-0.809119792515883));
#58413=DIRECTION('ref_axis',(0.949703593340092,0.163962091791853,0.266794897350299));
#58414=DIRECTION('',(1.,0.,0.));
#58415=DIRECTION('center_axis',(-0.313150259135957,-0.497254539006068,-0.809119792515883));
#58416=DIRECTION('ref_axis',(-0.949703593340092,0.163962091791853,0.2667948973503));
#58417=DIRECTION('center_axis',(-0.491310548314113,-0.446051802065979,-0.748098746816875));
#58418=DIRECTION('ref_axis',(-0.870984468928858,0.25161178329511,0.421992375987729));
#58419=DIRECTION('center_axis',(-0.284551435696759,-0.503074343325881,-0.816055565222214));
#58420=DIRECTION('ref_axis',(-0.958660774436356,0.149323442110948,0.242223097976277));
#58421=DIRECTION('center_axis',(0.0617712249622997,-0.528679668032723,-0.846570802931135));
#58422=DIRECTION('ref_axis',(0.998090334472114,0.0327196743412163,0.0523937700909926));
#58423=DIRECTION('center_axis',(0.99026806874157,0.106612780622095,-0.0894587448987841));
#58424=DIRECTION('ref_axis',(-0.139173100960066,0.758589351257642,-0.636532044855299));
#58425=DIRECTION('',(1.,0.,0.));
#58426=DIRECTION('center_axis',(0.,0.529919264233205,0.848048096156426));
#58427=DIRECTION('ref_axis',(1.,0.,0.));
#58428=DIRECTION('',(-0.137844537491629,0.839952525157012,-0.524860590029465));
#58429=DIRECTION('center_axis',(-0.99026806874157,-0.106612780622095,0.0894587448987841));
#58430=DIRECTION('ref_axis',(0.,0.64278760968654,0.766044443118978));
#58431=DIRECTION('',(-0.137998583506848,0.835520295497991,-0.531847935749547));
#58432=DIRECTION('center_axis',(-0.0617712249622997,0.528679668032723,0.846570802931135));
#58433=DIRECTION('ref_axis',(0.998052578482889,0.0400959894540315,0.0477845394804615));
#58434=DIRECTION('',(0.0161503784824051,0.848608959651483,-0.528774052761765));
#58435=DIRECTION('center_axis',(0.284551435696759,0.503074343325881,0.816055565222214));
#58436=DIRECTION('ref_axis',(0.957826285221151,-0.184703660511672,-0.220121250980087));
#58437=DIRECTION('',(0.0552259184163645,0.841229612052432,-0.537850200094026));
#58438=DIRECTION('center_axis',(0.491310548314113,0.446051802065979,0.748098746816875));
#58439=DIRECTION('ref_axis',(0.86824314212446,-0.318911962258806,-0.3800644767432));
#58440=DIRECTION('',(0.057078643955053,0.840576357876501,-0.538677468419953));
#58441=DIRECTION('center_axis',(0.313150259135957,0.497254539006068,0.809119792515883));
#58442=DIRECTION('ref_axis',(0.948683298050513,-0.203267289834479,-0.242244522917128));
#58443=DIRECTION('',(0.0225789275220278,0.847831897759644,-0.529784168481124));
#58444=DIRECTION('center_axis',(0.,0.529919264233205,0.848048096156426));
#58445=DIRECTION('ref_axis',(1.,0.,0.));
#58446=DIRECTION('',(-0.0225789275220274,0.847831897759644,-0.529784168481124));
#58447=DIRECTION('center_axis',(-0.313150259135956,0.497254539006069,0.809119792515883));
#58448=DIRECTION('ref_axis',(0.948683298050514,0.203267289834478,0.242244522917128));
#58449=DIRECTION('',(-0.0570786439550527,0.840576357876501,-0.538677468419953));
#58450=DIRECTION('center_axis',(-0.491310548314114,0.446051802065978,0.748098746816874));
#58451=DIRECTION('ref_axis',(0.86824314212446,0.318911962258806,0.380064476743201));
#58452=DIRECTION('',(-0.0552259184163635,0.841229612052432,-0.537850200094025));
#58453=DIRECTION('center_axis',(-0.284551435696759,0.50307434332588,0.816055565222214));
#58454=DIRECTION('ref_axis',(0.957826285221151,0.184703660511673,0.220121250980087));
#58455=DIRECTION('',(-0.0161503784824052,0.848608959651484,-0.528774052761765));
#58456=DIRECTION('center_axis',(0.0617712249622996,0.528679668032723,0.846570802931135));
#58457=DIRECTION('ref_axis',(0.998052578482889,-0.0400959894540314,-0.0477845394804615));
#58458=DIRECTION('',(0.137998583506848,0.835520295497991,-0.531847935749547));
#58459=DIRECTION('center_axis',(0.99026806874157,-0.106612780622095,0.0894587448987839));
#58460=DIRECTION('ref_axis',(0.,-0.64278760968654,-0.766044443118978));
#58461=DIRECTION('',(0.137844537491629,0.839952525157012,-0.524860590029466));
#58462=DIRECTION('center_axis',(0.,0.529919264233205,0.848048096156426));
#58463=DIRECTION('ref_axis',(1.,0.,0.));
#58464=DIRECTION('',(-0.051925424877728,0.846904049744114,-0.52920438469299));
#58465=DIRECTION('center_axis',(-0.64930555798837,0.373989994161849,0.662218828358294));
#58466=DIRECTION('ref_axis',(0.755033118392644,0.421467257957652,0.502285118831862));
#58467=DIRECTION('center_axis',(0.,-0.743144825477394,-0.669130606358858));
#58468=DIRECTION('ref_axis',(-1.,0.,0.));
#58469=DIRECTION('',(-1.,0.,0.));
#58470=DIRECTION('',(0.137844537491629,0.662743003631831,-0.736050673949001));
#58471=DIRECTION('center_axis',(0.99026806874157,-0.106612780622095,0.0894587448987839));
#58472=DIRECTION('ref_axis',(0.,-0.64278760968654,-0.766044443118978));
#58473=DIRECTION('center_axis',(-0.99026806874157,0.106612780622095,-0.0894587448987839));
#58474=DIRECTION('ref_axis',(0.139173100960065,0.758589351257639,-0.636532044855303));
#58475=DIRECTION('',(0.137998583506848,0.668854547266653,-0.730472439966645));
#58476=DIRECTION('center_axis',(0.0617712249622996,-0.741905229276912,-0.667653313133567));
#58477=DIRECTION('ref_axis',(-0.998052578482889,-0.0400959894540314,-0.0477845394804615));
#58478=DIRECTION('center_axis',(-0.0617712249622996,0.741905229276912,0.667653313133567));
#58479=DIRECTION('ref_axis',(0.998090334472114,0.045916079171941,0.0413206716646654));
#58480=DIRECTION('',(-0.0161503784824054,0.668100186146782,-0.743896032080768));
#58481=DIRECTION('center_axis',(-0.284551435696759,-0.71629990457007,-0.637138075424646));
#58482=DIRECTION('ref_axis',(-0.957826285221151,0.184703660511673,0.220121250980087));
#58483=DIRECTION('center_axis',(0.284551435696759,0.71629990457007,0.637138075424646));
#58484=DIRECTION('ref_axis',(-0.958660774436356,0.212613441240154,0.18911648304975));
#58485=DIRECTION('',(-0.0552259184163638,0.675757036144127,-0.735052736908566));
#58486=DIRECTION('center_axis',(-0.491310548314114,-0.659277363310168,-0.569181257019306));
#58487=DIRECTION('ref_axis',(-0.86824314212446,0.318911962258806,0.380064476743201));
#58488=DIRECTION('center_axis',(0.491310548314114,0.659277363310168,0.569181257019306));
#58489=DIRECTION('ref_axis',(-0.870984468928858,0.371889435936037,0.32106744201786));
#58490=DIRECTION('',(-0.0570786439550532,0.676458300008118,-0.734265753494183));
#58491=DIRECTION('center_axis',(-0.313150259135956,-0.710480100250258,-0.630202302718315));
#58492=DIRECTION('ref_axis',(-0.948683298050514,0.203267289834478,0.242244522917128));
#58493=DIRECTION('center_axis',(0.313150259135956,0.710480100250258,0.630202302718315));
#58494=DIRECTION('ref_axis',(-0.949703593340092,0.234269964928557,0.207799586932431));
#58495=DIRECTION('',(-0.0225789275220273,0.668960020557194,-0.742955370751214));
#58496=DIRECTION('center_axis',(0.,-0.743144825477394,-0.669130606358858));
#58497=DIRECTION('ref_axis',(-1.,0.,0.));
#58498=DIRECTION('',(-1.,0.,0.));
#58499=DIRECTION('',(0.0225789275220281,0.668960020557194,-0.742955370751214));
#58500=DIRECTION('center_axis',(0.313150259135957,-0.710480100250258,-0.630202302718315));
#58501=DIRECTION('ref_axis',(-0.948683298050513,-0.203267289834479,-0.242244522917128));
#58502=DIRECTION('center_axis',(-0.313150259135957,0.710480100250258,0.630202302718315));
#58503=DIRECTION('ref_axis',(0.949703593340092,0.234269964928558,0.207799586932432));
#58504=DIRECTION('',(0.0570786439550534,0.676458300008118,-0.734265753494183));
#58505=DIRECTION('center_axis',(0.491310548314113,-0.659277363310168,-0.569181257019307));
#58506=DIRECTION('ref_axis',(-0.86824314212446,-0.318911962258806,-0.3800644767432));
#58507=DIRECTION('center_axis',(-0.491310548314113,0.659277363310168,0.569181257019307));
#58508=DIRECTION('ref_axis',(0.870984468928858,0.371889435936036,0.321067442017859));
#58509=DIRECTION('',(0.0552259184163649,0.675757036144127,-0.735052736908566));
#58510=DIRECTION('center_axis',(0.284551435696759,-0.71629990457007,-0.637138075424646));
#58511=DIRECTION('ref_axis',(-0.957826285221151,-0.184703660511672,-0.220121250980087));
#58512=DIRECTION('center_axis',(-0.284551435696759,0.71629990457007,0.637138075424646));
#58513=DIRECTION('ref_axis',(0.958660774436356,0.212613441240154,0.189116483049749));
#58514=DIRECTION('',(0.016150378482405,0.668100186146782,-0.743896032080768));
#58515=DIRECTION('center_axis',(-0.0617712249622997,-0.741905229276912,
-0.667653313133567));
#58516=DIRECTION('ref_axis',(-0.998052578482889,0.0400959894540315,0.0477845394804615));
#58517=DIRECTION('center_axis',(0.0617712249622997,0.741905229276912,0.667653313133567));
#58518=DIRECTION('ref_axis',(-0.998090334472114,0.045916079171941,0.0413206716646654));
#58519=DIRECTION('',(-0.137998583506848,0.668854547266653,-0.730472439966645));
#58520=DIRECTION('center_axis',(-0.99026806874157,-0.106612780622095,0.0894587448987841));
#58521=DIRECTION('ref_axis',(0.,0.64278760968654,0.766044443118978));
#58522=DIRECTION('center_axis',(0.99026806874157,0.106612780622095,-0.0894587448987841));
#58523=DIRECTION('ref_axis',(-0.139173100960066,0.758589351257642,-0.636532044855299));
#58524=DIRECTION('',(-0.137844537491629,0.662743003631831,-0.736050673949001));
#58525=DIRECTION('center_axis',(0.,-0.743144825477394,-0.669130606358858));
#58526=DIRECTION('ref_axis',(-1.,0.,0.));
#58527=DIRECTION('',(-1.,0.,0.));
#58528=DIRECTION('center_axis',(0.,0.766044443118978,-0.64278760968654));
#58529=DIRECTION('ref_axis',(1.,0.,0.));
#58530=DIRECTION('center_axis',(1.,0.,0.));
#58531=DIRECTION('ref_axis',(0.,1.,0.));
#58532=DIRECTION('center_axis',(1.,0.,0.));
#58533=DIRECTION('ref_axis',(0.,0.,-1.));
#58534=DIRECTION('center_axis',(0.64930555798837,-0.483301338560726,-0.587215555406038));
#58535=DIRECTION('ref_axis',(0.760527640763576,0.412621749021023,0.501339206395651));
#58536=DIRECTION('',(1.,0.,0.));
#58537=DIRECTION('center_axis',(-0.99026806874157,0.0894587448987838,-0.106612780622095));
#58538=DIRECTION('ref_axis',(0.139173100960065,0.636532044855299,-0.758589351257642));
#58539=DIRECTION('center_axis',(-0.0617712249622996,-0.667653313133568,
-0.741905229276912));
#58540=DIRECTION('ref_axis',(-0.998090334472114,0.0413206716646654,0.045916079171941));
#58541=DIRECTION('center_axis',(0.284551435696759,-0.637138075424647,-0.716299904570069));
#58542=DIRECTION('ref_axis',(0.958660774436356,0.18911648304975,0.212613441240154));
#58543=DIRECTION('center_axis',(0.491310548314114,-0.569181257019307,-0.659277363310167));
#58544=DIRECTION('ref_axis',(0.870984468928858,0.32106744201786,0.371889435936037));
#58545=DIRECTION('center_axis',(0.313150259135956,-0.630202302718316,-0.710480100250258));
#58546=DIRECTION('ref_axis',(0.949703593340092,0.207799586932431,0.234269964928557));
#58547=DIRECTION('',(1.,0.,0.));
#58548=DIRECTION('center_axis',(-0.313150259135957,-0.630202302718315,-0.710480100250257));
#58549=DIRECTION('ref_axis',(-0.949703593340092,0.207799586932432,0.234269964928558));
#58550=DIRECTION('center_axis',(-0.491310548314113,-0.569181257019307,-0.659277363310168));
#58551=DIRECTION('ref_axis',(-0.870984468928858,0.321067442017859,0.371889435936036));
#58552=DIRECTION('center_axis',(-0.284551435696759,-0.637138075424647,-0.71629990457007));
#58553=DIRECTION('ref_axis',(-0.958660774436356,0.18911648304975,0.212613441240154));
#58554=DIRECTION('center_axis',(0.0617712249622997,-0.667653313133568,-0.741905229276912));
#58555=DIRECTION('ref_axis',(0.998090334472114,0.0413206716646654,0.045916079171941));
#58556=DIRECTION('center_axis',(0.99026806874157,0.0894587448987841,-0.106612780622095));
#58557=DIRECTION('ref_axis',(-0.139173100960066,0.636532044855299,-0.758589351257642));
#58558=DIRECTION('',(1.,0.,0.));
#58559=DIRECTION('center_axis',(0.,0.669130606358858,0.743144825477394));
#58560=DIRECTION('ref_axis',(1.,0.,0.));
#58561=DIRECTION('',(-0.137844537491629,0.736050673949001,-0.662743003631831));
#58562=DIRECTION('center_axis',(-0.99026806874157,-0.0894587448987841,0.106612780622095));
#58563=DIRECTION('ref_axis',(0.,0.766044443118978,0.642787609686539));
#58564=DIRECTION('',(-0.137998583506848,0.730472439966645,-0.668854547266653));
#58565=DIRECTION('center_axis',(-0.0617712249622997,0.667653313133568,0.741905229276912));
#58566=DIRECTION('ref_axis',(0.998052578482889,0.0477845394804616,0.0400959894540315));
#58567=DIRECTION('',(0.0161503784824051,0.743896032080767,-0.668100186146782));
#58568=DIRECTION('center_axis',(0.284551435696759,0.637138075424647,0.71629990457007));
#58569=DIRECTION('ref_axis',(0.957826285221151,-0.220121250980087,-0.184703660511672));
#58570=DIRECTION('',(0.0552259184163645,0.735052736908566,-0.675757036144128));
#58571=DIRECTION('center_axis',(0.491310548314113,0.569181257019307,0.659277363310168));
#58572=DIRECTION('ref_axis',(0.86824314212446,-0.3800644767432,-0.318911962258805));
#58573=DIRECTION('',(0.057078643955053,0.734265753494182,-0.676458300008118));
#58574=DIRECTION('center_axis',(0.313150259135957,0.630202302718315,0.710480100250257));
#58575=DIRECTION('ref_axis',(0.948683298050513,-0.242244522917128,-0.203267289834479));
#58576=DIRECTION('',(0.0225789275220278,0.742955370751214,-0.668960020557194));
#58577=DIRECTION('center_axis',(0.,0.669130606358858,0.743144825477394));
#58578=DIRECTION('ref_axis',(1.,0.,0.));
#58579=DIRECTION('',(-0.0225789275220274,0.742955370751214,-0.668960020557194));
#58580=DIRECTION('center_axis',(-0.313150259135956,0.630202302718316,0.710480100250258));
#58581=DIRECTION('ref_axis',(0.948683298050514,0.242244522917128,0.203267289834478));
#58582=DIRECTION('',(-0.0570786439550527,0.734265753494182,-0.676458300008118));
#58583=DIRECTION('center_axis',(-0.491310548314114,0.569181257019307,0.659277363310167));
#58584=DIRECTION('ref_axis',(0.868243142124459,0.380064476743201,0.318911962258806));
#58585=DIRECTION('',(-0.0552259184163635,0.735052736908566,-0.675757036144127));
#58586=DIRECTION('center_axis',(-0.284551435696759,0.637138075424647,0.716299904570069));
#58587=DIRECTION('ref_axis',(0.957826285221151,0.220121250980087,0.184703660511673));
#58588=DIRECTION('',(-0.0161503784824052,0.743896032080767,-0.668100186146782));
#58589=DIRECTION('center_axis',(0.0617712249622996,0.667653313133568,0.741905229276912));
#58590=DIRECTION('ref_axis',(0.998052578482889,-0.0477845394804615,-0.0400959894540314));
#58591=DIRECTION('',(0.137998583506848,0.730472439966645,-0.668854547266653));
#58592=DIRECTION('center_axis',(0.99026806874157,-0.0894587448987838,0.106612780622095));
#58593=DIRECTION('ref_axis',(0.,-0.766044443118978,-0.642787609686539));
#58594=DIRECTION('',(0.137844537491629,0.736050673949,-0.662743003631831));
#58595=DIRECTION('center_axis',(0.,0.669130606358858,0.743144825477394));
#58596=DIRECTION('ref_axis',(1.,0.,0.));
#58597=DIRECTION('',(-0.0519254248777279,0.742142297230154,-0.66822792587052));
#58598=DIRECTION('center_axis',(-0.64930555798837,0.483301338560726,0.587215555406038));
#58599=DIRECTION('ref_axis',(0.755033118392644,0.502285118831863,0.421467257957652));
#58600=DIRECTION('center_axis',(0.,-0.848048096156426,-0.529919264233205));
#58601=DIRECTION('ref_axis',(-1.,0.,0.));
#58602=DIRECTION('',(-1.,0.,0.));
#58603=DIRECTION('',(0.137844537491629,0.524860590029465,-0.839952525157012));
#58604=DIRECTION('center_axis',(0.99026806874157,-0.0894587448987838,0.106612780622095));
#58605=DIRECTION('ref_axis',(0.,-0.766044443118978,-0.642787609686539));
#58606=DIRECTION('center_axis',(-0.99026806874157,0.0894587448987838,-0.106612780622095));
#58607=DIRECTION('ref_axis',(0.139173100960065,0.636532044855299,-0.758589351257642));
#58608=DIRECTION('',(0.137998583506848,0.531847935749546,-0.835520295497991));
#58609=DIRECTION('center_axis',(0.0617712249622996,-0.846570802931135,-0.528679668032723));
#58610=DIRECTION('ref_axis',(-0.998052578482889,-0.0477845394804615,-0.0400959894540314));
#58611=DIRECTION('center_axis',(-0.0617712249622996,0.846570802931135,0.528679668032723));
#58612=DIRECTION('ref_axis',(0.998090334472114,0.0523937700909925,0.0327196743412163));
#58613=DIRECTION('',(-0.0161503784824054,0.528774052761765,-0.848608959651484));
#58614=DIRECTION('center_axis',(-0.284551435696759,-0.816055565222214,-0.50307434332588));
#58615=DIRECTION('ref_axis',(-0.957826285221151,0.220121250980087,0.184703660511673));
#58616=DIRECTION('center_axis',(0.284551435696759,0.816055565222214,0.50307434332588));
#58617=DIRECTION('ref_axis',(-0.958660774436356,0.242223097976277,0.149323442110948));
#58618=DIRECTION('',(-0.0552259184163638,0.537850200094025,-0.841229612052433));
#58619=DIRECTION('center_axis',(-0.491310548314114,-0.748098746816874,-0.446051802065978));
#58620=DIRECTION('ref_axis',(-0.868243142124459,0.380064476743201,0.318911962258806));
#58621=DIRECTION('center_axis',(0.491310548314114,0.748098746816874,0.446051802065978));
#58622=DIRECTION('ref_axis',(-0.870984468928858,0.421992375987731,0.25161178329511));
#58623=DIRECTION('',(-0.0570786439550532,0.538677468419953,-0.840576357876501));
#58624=DIRECTION('center_axis',(-0.313150259135956,-0.809119792515883,-0.497254539006068));
#58625=DIRECTION('ref_axis',(-0.948683298050514,0.242244522917128,0.203267289834478));
#58626=DIRECTION('center_axis',(0.313150259135956,0.809119792515883,0.497254539006068));
#58627=DIRECTION('ref_axis',(-0.949703593340092,0.266794897350299,0.163962091791853));
#58628=DIRECTION('',(-0.0225789275220273,0.529784168481124,-0.847831897759644));
#58629=DIRECTION('center_axis',(0.,-0.848048096156426,-0.529919264233205));
#58630=DIRECTION('ref_axis',(-1.,0.,0.));
#58631=DIRECTION('',(-1.,0.,0.));
#58632=DIRECTION('',(0.0225789275220281,0.529784168481124,-0.847831897759644));
#58633=DIRECTION('center_axis',(0.313150259135957,-0.809119792515883,-0.497254539006068));
#58634=DIRECTION('ref_axis',(-0.948683298050513,-0.242244522917128,-0.203267289834479));
#58635=DIRECTION('center_axis',(-0.313150259135957,0.809119792515883,0.497254539006068));
#58636=DIRECTION('ref_axis',(0.949703593340092,0.2667948973503,0.163962091791853));
#58637=DIRECTION('',(0.0570786439550534,0.538677468419952,-0.840576357876501));
#58638=DIRECTION('center_axis',(0.491310548314113,-0.748098746816875,-0.446051802065978));
#58639=DIRECTION('ref_axis',(-0.86824314212446,-0.3800644767432,-0.318911962258805));
#58640=DIRECTION('center_axis',(-0.491310548314113,0.748098746816875,0.446051802065978));
#58641=DIRECTION('ref_axis',(0.870984468928858,0.421992375987729,0.25161178329511));
#58642=DIRECTION('',(0.0552259184163649,0.537850200094025,-0.841229612052432));
#58643=DIRECTION('center_axis',(0.284551435696759,-0.816055565222214,-0.50307434332588));
#58644=DIRECTION('ref_axis',(-0.957826285221151,-0.220121250980087,-0.184703660511672));
#58645=DIRECTION('center_axis',(-0.284551435696759,0.816055565222214,0.50307434332588));
#58646=DIRECTION('ref_axis',(0.958660774436356,0.242223097976277,0.149323442110947));
#58647=DIRECTION('',(0.0161503784824051,0.528774052761765,-0.848608959651484));
#58648=DIRECTION('center_axis',(-0.0617712249622997,-0.846570802931135,
-0.528679668032723));
#58649=DIRECTION('ref_axis',(-0.998052578482889,0.0477845394804616,0.0400959894540315));
#58650=DIRECTION('center_axis',(0.0617712249622997,0.846570802931135,0.528679668032723));
#58651=DIRECTION('ref_axis',(-0.998090334472114,0.0523937700909926,0.0327196743412163));
#58652=DIRECTION('',(-0.137998583506848,0.531847935749546,-0.835520295497991));
#58653=DIRECTION('center_axis',(-0.99026806874157,-0.0894587448987841,0.106612780622095));
#58654=DIRECTION('ref_axis',(0.,0.766044443118978,0.642787609686539));
#58655=DIRECTION('center_axis',(0.99026806874157,0.0894587448987841,-0.106612780622095));
#58656=DIRECTION('ref_axis',(-0.139173100960066,0.636532044855299,-0.758589351257642));
#58657=DIRECTION('',(-0.137844537491629,0.524860590029465,-0.839952525157012));
#58658=DIRECTION('center_axis',(0.,-0.848048096156426,-0.529919264233205));
#58659=DIRECTION('ref_axis',(-1.,0.,0.));
#58660=DIRECTION('',(-1.,0.,0.));
#58661=DIRECTION('center_axis',(0.,0.642787609686539,-0.766044443118978));
#58662=DIRECTION('ref_axis',(1.,0.,0.));
#58663=DIRECTION('center_axis',(1.,0.,0.));
#58664=DIRECTION('ref_axis',(0.,1.,0.));
#58665=DIRECTION('center_axis',(1.,0.,0.));
#58666=DIRECTION('ref_axis',(0.,0.,-1.));
#58667=DIRECTION('center_axis',(0.649305557988371,-0.577927816349714,-0.494370034948177));
#58668=DIRECTION('ref_axis',(0.760527640763576,0.49340973708095,0.422071722564183));
#58669=DIRECTION('',(1.,0.,0.));
#58670=DIRECTION('center_axis',(-0.99026806874157,0.0695865504800327,-0.120527440954873));
#58671=DIRECTION('ref_axis',(0.139173100960065,0.495134034370783,-0.857597304086756));
#58672=DIRECTION('center_axis',(-0.0617712249622996,-0.786340650163727,
-0.614697240653271));
#58673=DIRECTION('ref_axis',(-0.998090334472114,0.0486661612888524,0.0380432514219071));
#58674=DIRECTION('center_axis',(0.284551435696759,-0.751842689509058,-0.594779833782804));
#58675=DIRECTION('ref_axis',(0.958660774436356,0.223163315348643,0.176543632679541));
#58676=DIRECTION('center_axis',(0.491310548314114,-0.675016427497717,-0.550424170729724));
#58677=DIRECTION('ref_axis',(0.870984468928858,0.380767628982861,0.310486823558562));
#58678=DIRECTION('center_axis',(0.313150259135956,-0.744001688360219,-0.590252829658806));
#58679=DIRECTION('ref_axis',(0.949703593340092,0.245323196775732,0.194626858168784));
#58680=DIRECTION('',(1.,0.,0.));
#58681=DIRECTION('center_axis',(-0.313150259135957,-0.744001688360219,-0.590252829658806));
#58682=DIRECTION('ref_axis',(-0.949703593340092,0.245323196775733,0.194626858168784));
#58683=DIRECTION('center_axis',(-0.491310548314113,-0.675016427497717,-0.550424170729724));
#58684=DIRECTION('ref_axis',(-0.870984468928858,0.38076762898286,0.310486823558561));
#58685=DIRECTION('center_axis',(-0.284551435696759,-0.751842689509058,-0.594779833782804));
#58686=DIRECTION('ref_axis',(-0.958660774436356,0.223163315348643,0.176543632679541));
#58687=DIRECTION('center_axis',(0.0617712249622997,-0.786340650163727,-0.61469724065327));
#58688=DIRECTION('ref_axis',(0.998090334472114,0.0486661612888524,0.0380432514219071));
#58689=DIRECTION('center_axis',(0.99026806874157,0.0695865504800329,-0.120527440954873));
#58690=DIRECTION('ref_axis',(-0.139173100960066,0.495134034370784,-0.857597304086755));
#58691=DIRECTION('',(1.,0.,0.));
#58692=DIRECTION('center_axis',(0.,0.788010753606722,0.615661475325659));
#58693=DIRECTION('ref_axis',(1.,0.,0.));
#58694=DIRECTION('',(-0.137844537491629,0.609784295472662,-0.780488306432985));
#58695=DIRECTION('center_axis',(-0.99026806874157,-0.0695865504800329,0.120527440954873));
#58696=DIRECTION('ref_axis',(0.,0.866025403784439,0.5));
#58697=DIRECTION('',(-0.137998583506848,0.603229548983803,-0.785538351821795));
#58698=DIRECTION('center_axis',(-0.0617712249622997,0.786340650163727,0.61469724065327));
#58699=DIRECTION('ref_axis',(0.998052578482889,0.0540211804549215,0.0311891430775903));
#58700=DIRECTION('',(0.0161503784824051,0.616580200004832,-0.787126433450736));
#58701=DIRECTION('center_axis',(0.284551435696759,0.751842689509058,0.594779833782804));
#58702=DIRECTION('ref_axis',(0.957826285221151,-0.248850568624199,-0.143673942783173));
#58703=DIRECTION('',(0.0552259184163645,0.606541656308365,-0.79313133660055));
#58704=DIRECTION('center_axis',(0.491310548314113,0.675016427497717,0.550424170729724));
#58705=DIRECTION('ref_axis',(0.86824314212446,-0.429668924423658,-0.248069469178416));
#58706=DIRECTION('',(0.057078643955053,0.605644855748342,-0.793685288454953));
#58707=DIRECTION('center_axis',(0.313150259135957,0.744001688360219,0.590252829658806));
#58708=DIRECTION('ref_axis',(0.948683298050513,-0.273861278752585,-0.15811388300842));
#58709=DIRECTION('',(0.0225789275220278,0.615504520756066,-0.787809860918738));
#58710=DIRECTION('center_axis',(0.,0.788010753606722,0.615661475325658));
#58711=DIRECTION('ref_axis',(1.,0.,0.));
#58712=DIRECTION('',(-0.0225789275220274,0.615504520756066,-0.787809860918738));
#58713=DIRECTION('center_axis',(-0.313150259135956,0.744001688360219,0.590252829658806));
#58714=DIRECTION('ref_axis',(0.948683298050514,0.273861278752584,0.158113883008419));
#58715=DIRECTION('',(-0.0570786439550527,0.605644855748342,-0.793685288454953));
#58716=DIRECTION('center_axis',(-0.491310548314114,0.675016427497717,0.550424170729724));
#58717=DIRECTION('ref_axis',(0.868243142124459,0.429668924423659,0.248069469178417));
#58718=DIRECTION('',(-0.0552259184163635,0.606541656308365,-0.793131336600549));
#58719=DIRECTION('center_axis',(-0.284551435696759,0.751842689509058,0.594779833782804));
#58720=DIRECTION('ref_axis',(0.957826285221151,0.248850568624199,0.143673942783173));
#58721=DIRECTION('',(-0.0161503784824052,0.616580200004832,-0.787126433450736));
#58722=DIRECTION('center_axis',(0.0617712249622996,0.786340650163727,0.614697240653271));
#58723=DIRECTION('ref_axis',(0.998052578482889,-0.0540211804549215,-0.0311891430775903));
#58724=DIRECTION('',(0.137998583506848,0.603229548983803,-0.785538351821795));
#58725=DIRECTION('center_axis',(0.99026806874157,-0.0695865504800327,0.120527440954873));
#58726=DIRECTION('ref_axis',(0.,-0.866025403784439,-0.5));
#58727=DIRECTION('',(0.137844537491629,0.609784295472662,-0.780488306432985));
#58728=DIRECTION('center_axis',(0.,0.788010753606722,0.615661475325658));
#58729=DIRECTION('ref_axis',(1.,0.,0.));
#58730=DIRECTION('',(-0.051925424877728,0.614830926556978,-0.786947699660121));
#58731=DIRECTION('center_axis',(-0.649305557988371,0.577927816349714,0.494370034948177));
#58732=DIRECTION('ref_axis',(0.755033118392644,0.567841300538901,0.327843327723122));
#58733=DIRECTION('center_axis',(0.,-0.927183854566787,-0.374606593415912));
#58734=DIRECTION('ref_axis',(-1.,0.,0.));
#58735=DIRECTION('',(-1.,0.,0.));
#58736=DIRECTION('',(0.137844537491629,0.371030552991328,-0.918332843924613));
#58737=DIRECTION('center_axis',(0.99026806874157,-0.0695865504800327,0.120527440954873));
#58738=DIRECTION('ref_axis',(0.,-0.866025403784439,-0.5));
#58739=DIRECTION('center_axis',(-0.99026806874157,0.0695865504800327,-0.120527440954873));
#58740=DIRECTION('ref_axis',(0.139173100960065,0.495134034370783,-0.857597304086756));
#58741=DIRECTION('',(0.137998583506848,0.378681393832731,-0.9151812896443));
#58742=DIRECTION('center_axis',(0.0617712249622996,-0.925513751123792,-0.373642358743524));
#58743=DIRECTION('ref_axis',(-0.998052578482889,-0.0540211804549215,-0.0311891430775903));
#58744=DIRECTION('center_axis',(-0.0617712249622996,0.925513751123792,0.373642358743524));
#58745=DIRECTION('ref_axis',(0.998090334472114,0.0572795028183562,0.0231245062698634));
#58746=DIRECTION('',(-0.0161503784824054,0.373381387356163,-0.927537333400043));
#58747=DIRECTION('center_axis',(-0.284551435696759,-0.891015790469123,-0.353724951873058));
#58748=DIRECTION('ref_axis',(-0.957826285221151,0.248850568624199,0.143673942783173));
#58749=DIRECTION('center_axis',(0.284551435696759,0.891015790469123,0.353724951873058));
#58750=DIRECTION('ref_axis',(-0.958660774436356,0.264472928451193,0.104993283944912));
#58751=DIRECTION('',(-0.0552259184163638,0.3836010578794,-0.921846151116809));
#58752=DIRECTION('center_axis',(-0.491310548314114,-0.814189528457782,-0.309369288819978));
#58753=DIRECTION('ref_axis',(-0.868243142124459,0.429668924423659,0.248069469178417));
#58754=DIRECTION('center_axis',(0.491310548314114,0.814189528457782,0.309369288819978));
#58755=DIRECTION('ref_axis',(-0.870984468928858,0.459273291233482,0.174511027858645));
#58756=DIRECTION('',(-0.0570786439550532,0.384529194537798,-0.921346474976903));
#58757=DIRECTION('center_axis',(-0.313150259135956,-0.883174789320284,-0.34919794774906));
#58758=DIRECTION('ref_axis',(-0.948683298050514,0.273861278752584,0.158113883008419));
#58759=DIRECTION('center_axis',(0.313150259135956,0.883174789320284,0.34919794774906));
#58760=DIRECTION('ref_axis',(-0.949703593340092,0.291213401820783,0.115142691461001));
#58761=DIRECTION('',(-0.0225789275220273,0.374511092529479,-0.926947481578288));
#58762=DIRECTION('center_axis',(0.,-0.927183854566787,-0.374606593415912));
#58763=DIRECTION('ref_axis',(-1.,0.,0.));
#58764=DIRECTION('',(-1.,0.,0.));
#58765=DIRECTION('',(0.0225789275220281,0.374511092529479,-0.926947481578288));
#58766=DIRECTION('center_axis',(0.313150259135957,-0.883174789320284,-0.349197947749059));
#58767=DIRECTION('ref_axis',(-0.948683298050513,-0.273861278752585,-0.15811388300842));
#58768=DIRECTION('center_axis',(-0.313150259135957,0.883174789320284,0.349197947749059));
#58769=DIRECTION('ref_axis',(0.949703593340092,0.291213401820785,0.115142691461001));
#58770=DIRECTION('',(0.0570786439550534,0.384529194537798,-0.921346474976903));
#58771=DIRECTION('center_axis',(0.491310548314113,-0.814189528457783,-0.309369288819978));
#58772=DIRECTION('ref_axis',(-0.86824314212446,-0.429668924423658,-0.248069469178416));
#58773=DIRECTION('center_axis',(-0.491310548314113,0.814189528457783,0.309369288819978));
#58774=DIRECTION('ref_axis',(0.870984468928858,0.459273291233481,0.174511027858644));
#58775=DIRECTION('',(0.0552259184163649,0.3836010578794,-0.921846151116809));
#58776=DIRECTION('center_axis',(0.284551435696759,-0.891015790469123,-0.353724951873058));
#58777=DIRECTION('ref_axis',(-0.957826285221151,-0.248850568624199,-0.143673942783173));
#58778=DIRECTION('center_axis',(-0.284551435696759,0.891015790469123,0.353724951873058));
#58779=DIRECTION('ref_axis',(0.958660774436356,0.264472928451193,0.104993283944912));
#58780=DIRECTION('',(0.0161503784824051,0.373381387356163,-0.927537333400043));
#58781=DIRECTION('center_axis',(-0.0617712249622997,-0.925513751123792,
-0.373642358743524));
#58782=DIRECTION('ref_axis',(-0.998052578482889,0.0540211804549215,0.0311891430775903));
#58783=DIRECTION('center_axis',(0.0617712249622997,0.925513751123792,0.373642358743524));
#58784=DIRECTION('ref_axis',(-0.998090334472114,0.0572795028183562,0.0231245062698635));
#58785=DIRECTION('',(-0.137998583506848,0.378681393832731,-0.9151812896443));
#58786=DIRECTION('center_axis',(-0.99026806874157,-0.0695865504800329,0.120527440954873));
#58787=DIRECTION('ref_axis',(0.,0.866025403784439,0.5));
#58788=DIRECTION('center_axis',(0.99026806874157,0.0695865504800329,-0.120527440954873));
#58789=DIRECTION('ref_axis',(-0.139173100960066,0.495134034370784,-0.857597304086755));
#58790=DIRECTION('',(-0.137844537491629,0.371030552991328,-0.918332843924613));
#58791=DIRECTION('center_axis',(0.,-0.927183854566787,-0.374606593415912));
#58792=DIRECTION('ref_axis',(-1.,0.,0.));
#58793=DIRECTION('',(-1.,0.,0.));
#58794=DIRECTION('center_axis',(0.,0.5,-0.866025403784439));
#58795=DIRECTION('ref_axis',(1.,0.,0.));
#58796=DIRECTION('center_axis',(1.,0.,0.));
#58797=DIRECTION('ref_axis',(0.,1.,0.));
#58798=DIRECTION('center_axis',(1.,0.,0.));
#58799=DIRECTION('ref_axis',(0.,0.,-1.));
#58800=DIRECTION('center_axis',(0.64930555798837,-0.654994249884502,-0.386503331141725));
#58801=DIRECTION('ref_axis',(0.760527640763576,0.559205719957048,0.329979803021198));
#58802=DIRECTION('',(1.,0.,0.));
#58803=DIRECTION('center_axis',(-0.99026806874157,0.0476000039374393,-0.130779935984066));
#58804=DIRECTION('ref_axis',(0.139173100960065,0.338691626801823,-0.930547596796367));
#58805=DIRECTION('center_axis',(-0.0617712249622996,-0.88113542444623,-0.468811987424191));
#58806=DIRECTION('ref_axis',(-0.998090334472114,0.0545329542285434,0.0290144987282327));
#58807=DIRECTION('center_axis',(0.284551435696759,-0.843702943923494,-0.455187678719166));
#58808=DIRECTION('ref_axis',(0.958660774436356,0.250429443236755,0.135109635175349));
#58809=DIRECTION('center_axis',(0.491310548314114,-0.760341565401403,-0.424846618249727));
#58810=DIRECTION('ref_axis',(0.870984468928858,0.428898384218936,0.239650226161174));
#58811=DIRECTION('center_axis',(0.313150259135956,-0.835194959184317,-0.452091025520514));
#58812=DIRECTION('ref_axis',(0.949703593340092,0.27539278542453,0.149070112809494));
#58813=DIRECTION('',(1.,0.,0.));
#58814=DIRECTION('center_axis',(-0.313150259135957,-0.835194959184317,-0.452091025520514));
#58815=DIRECTION('ref_axis',(-0.949703593340092,0.275392785424531,0.149070112809494));
#58816=DIRECTION('center_axis',(-0.491310548314113,-0.760341565401403,-0.424846618249727));
#58817=DIRECTION('ref_axis',(-0.870984468928858,0.428898384218935,0.239650226161173));
#58818=DIRECTION('center_axis',(-0.284551435696759,-0.843702943923494,-0.455187678719166));
#58819=DIRECTION('ref_axis',(-0.958660774436356,0.250429443236754,0.135109635175349));
#58820=DIRECTION('center_axis',(0.0617712249622997,-0.88113542444623,-0.468811987424191));
#58821=DIRECTION('ref_axis',(0.998090334472114,0.0545329542285435,0.0290144987282327));
#58822=DIRECTION('center_axis',(0.99026806874157,0.0476000039374394,-0.130779935984066));
#58823=DIRECTION('ref_axis',(-0.139173100960066,0.338691626801824,-0.930547596796366));
#58824=DIRECTION('',(1.,0.,0.));
#58825=DIRECTION('center_axis',(0.,0.882947592858927,0.469471562785891));
#58826=DIRECTION('ref_axis',(1.,0.,0.));
#58827=DIRECTION('',(-0.137844537491629,0.464989929744127,-0.874518866989312));
#58828=DIRECTION('center_axis',(-0.99026806874157,-0.0476000039374394,0.130779935984066));
#58829=DIRECTION('ref_axis',(0.,0.939692620785909,0.342020143325668));
#58830=DIRECTION('',(-0.137998583506848,0.457657833403967,-0.878353971058417));
#58831=DIRECTION('center_axis',(-0.0617712249622997,0.88113542444623,0.468811987424191));
#58832=DIRECTION('ref_axis',(0.998052578482889,0.058616415197295,0.0213346303712044));
#58833=DIRECTION('',(0.0161503784824051,0.470529890556386,-0.882236242379484));
#58834=DIRECTION('center_axis',(0.284551435696759,0.843702943923494,0.455187678719166));
#58835=DIRECTION('ref_axis',(0.957826285221151,-0.270018687665128,-0.0982787650057291));
#58836=DIRECTION('',(0.0552259184163645,0.459601114406121,-0.886406742738186));
#58837=DIRECTION('center_axis',(0.491310548314113,0.760341565401403,0.424846618249727));
#58838=DIRECTION('ref_axis',(0.86824314212446,-0.46621809925847,-0.169689510806249));
#58839=DIRECTION('',(0.057078643955053,0.458621745531673,-0.886796551036219));
#58840=DIRECTION('center_axis',(0.313150259135957,0.835194959184317,0.452091025520514));
#58841=DIRECTION('ref_axis',(0.948683298050513,-0.297156898213637,-0.108156265856635));
#58842=DIRECTION('',(0.0225789275220278,0.46935187735806,-0.88272249730729));
#58843=DIRECTION('center_axis',(0.,0.882947592858927,0.46947156278589));
#58844=DIRECTION('ref_axis',(1.,0.,0.));
#58845=DIRECTION('',(-0.0225789275220274,0.46935187735806,-0.88272249730729));
#58846=DIRECTION('center_axis',(-0.313150259135956,0.835194959184317,0.452091025520514));
#58847=DIRECTION('ref_axis',(0.948683298050514,0.297156898213636,0.108156265856635));
#58848=DIRECTION('',(-0.0570786439550527,0.458621745531673,-0.886796551036219));
#58849=DIRECTION('center_axis',(-0.491310548314114,0.760341565401403,0.424846618249727));
#58850=DIRECTION('ref_axis',(0.868243142124459,0.466218099258471,0.169689510806249));
#58851=DIRECTION('',(-0.0552259184163635,0.459601114406122,-0.886406742738186));
#58852=DIRECTION('center_axis',(-0.284551435696759,0.843702943923494,0.455187678719166));
#58853=DIRECTION('ref_axis',(0.957826285221151,0.270018687665129,0.0982787650057294));
#58854=DIRECTION('',(-0.0161503784824052,0.470529890556386,-0.882236242379483));
#58855=DIRECTION('center_axis',(0.0617712249622996,0.88113542444623,0.468811987424191));
#58856=DIRECTION('ref_axis',(0.998052578482889,-0.0586164151972949,-0.0213346303712044));
#58857=DIRECTION('',(0.137998583506848,0.457657833403967,-0.878353971058417));
#58858=DIRECTION('center_axis',(0.99026806874157,-0.0476000039374393,0.130779935984066));
#58859=DIRECTION('ref_axis',(0.,-0.939692620785909,-0.342020143325668));
#58860=DIRECTION('',(0.137844537491629,0.464989929744127,-0.874518866989312));
#58861=DIRECTION('center_axis',(0.,0.882947592858927,0.46947156278589));
#58862=DIRECTION('ref_axis',(1.,0.,0.));
#58863=DIRECTION('',(-0.0519254248777279,0.468838229299828,-0.881756465810299));
#58864=DIRECTION('center_axis',(-0.64930555798837,0.654994249884502,0.386503331141725));
#58865=DIRECTION('ref_axis',(0.755033118392644,0.616143911670627,0.224258043872452));
#58866=DIRECTION('center_axis',(0.,-0.978147600733806,-0.207911690817759));
#58867=DIRECTION('ref_axis',(-1.,0.,0.));
#58868=DIRECTION('',(-1.,0.,0.));
#58869=DIRECTION('',(0.137844537491629,0.205926940351067,-0.968810083928407));
#58870=DIRECTION('center_axis',(0.99026806874157,-0.0476000039374393,0.130779935984066));
#58871=DIRECTION('ref_axis',(0.,-0.939692620785909,-0.342020143325668));
#58872=DIRECTION('center_axis',(-0.99026806874157,0.0476000039374393,-0.130779935984066));
#58873=DIRECTION('ref_axis',(0.139173100960065,0.338691626801823,-0.930547596796367));
#58874=DIRECTION('',(0.137998583506848,0.214008809386338,-0.967034963408845));
#58875=DIRECTION('center_axis',(0.0617712249622996,-0.976335432321108,-0.207252115456059));
#58876=DIRECTION('ref_axis',(-0.998052578482889,-0.0586164151972949,-0.0213346303712044));
#58877=DIRECTION('center_axis',(-0.0617712249622996,0.976335432321108,0.207252115456059));
#58878=DIRECTION('ref_axis',(0.998090334472114,0.0604248268374111,0.0128267117770655));
#58879=DIRECTION('',(-0.0161503784824054,0.206643717435841,-0.97828295462978));
#58880=DIRECTION('center_axis',(-0.284551435696759,-0.938902951798373,-0.193627806751034));
#58881=DIRECTION('ref_axis',(-0.957826285221151,0.270018687665129,0.0982787650057294));
#58882=DIRECTION('center_axis',(0.284551435696759,0.938902951798373,0.193627806751034));
#58883=DIRECTION('ref_axis',(-0.958660774436356,0.278686882824879,0.0574729579753753));
#58884=DIRECTION('',(-0.0552259184163638,0.21769639163261,-0.974452861356162));
#58885=DIRECTION('center_axis',(-0.491310548314114,-0.855541573276281,-0.163286746281595));
#58886=DIRECTION('ref_axis',(-0.868243142124459,0.466218099258471,0.169689510806249));
#58887=DIRECTION('center_axis',(0.491310548314114,0.855541573276281,0.163286746281595));
#58888=DIRECTION('ref_axis',(-0.870984468928858,0.482599419928604,0.0921078431475349));
#58889=DIRECTION('',(-0.0570786439550532,0.218697195660774,-0.974121945658943));
#58890=DIRECTION('center_axis',(-0.313150259135956,-0.930394967059196,-0.190531153552383));
#58891=DIRECTION('ref_axis',(-0.948683298050514,0.297156898213636,0.108156265856635));
#58892=DIRECTION('center_axis',(0.313150259135956,0.930394967059196,0.190531153552383));
#58893=DIRECTION('ref_axis',(-0.949703593340092,0.306783534438035,0.0628247387151194));
#58894=DIRECTION('',(-0.0225789275220273,0.207858686543083,-0.977898235227234));
#58895=DIRECTION('center_axis',(0.,-0.978147600733806,-0.207911690817759));
#58896=DIRECTION('ref_axis',(-1.,0.,0.));
#58897=DIRECTION('',(-1.,0.,0.));
#58898=DIRECTION('',(0.0225789275220281,0.207858686543083,-0.977898235227234));
#58899=DIRECTION('center_axis',(0.313150259135957,-0.930394967059196,-0.190531153552383));
#58900=DIRECTION('ref_axis',(-0.948683298050513,-0.297156898213637,-0.108156265856635));
#58901=DIRECTION('center_axis',(-0.313150259135957,0.930394967059196,0.190531153552383));
#58902=DIRECTION('ref_axis',(0.949703593340092,0.306783534438037,0.0628247387151195));
#58903=DIRECTION('',(0.0570786439550534,0.218697195660774,-0.974121945658944));
#58904=DIRECTION('center_axis',(0.491310548314113,-0.855541573276282,-0.163286746281595));
#58905=DIRECTION('ref_axis',(-0.86824314212446,-0.46621809925847,-0.169689510806249));
#58906=DIRECTION('center_axis',(-0.491310548314113,0.855541573276282,0.163286746281595));
#58907=DIRECTION('ref_axis',(0.870984468928858,0.482599419928603,0.0921078431475346));
#58908=DIRECTION('',(0.0552259184163649,0.21769639163261,-0.974452861356161));
#58909=DIRECTION('center_axis',(0.284551435696759,-0.938902951798373,-0.193627806751034));
#58910=DIRECTION('ref_axis',(-0.957826285221151,-0.270018687665128,-0.0982787650057291));
#58911=DIRECTION('center_axis',(-0.284551435696759,0.938902951798373,0.193627806751034));
#58912=DIRECTION('ref_axis',(0.958660774436356,0.278686882824878,0.0574729579753753));
#58913=DIRECTION('',(0.0161503784824051,0.206643717435841,-0.97828295462978));
#58914=DIRECTION('center_axis',(-0.0617712249622997,-0.976335432321108,
-0.207252115456059));
#58915=DIRECTION('ref_axis',(-0.998052578482889,0.058616415197295,0.0213346303712044));
#58916=DIRECTION('center_axis',(0.0617712249622997,0.976335432321108,0.207252115456059));
#58917=DIRECTION('ref_axis',(-0.998090334472114,0.0604248268374112,0.0128267117770655));
#58918=DIRECTION('',(-0.137998583506848,0.214008809386338,-0.967034963408845));
#58919=DIRECTION('center_axis',(-0.99026806874157,-0.0476000039374394,0.130779935984066));
#58920=DIRECTION('ref_axis',(0.,0.939692620785909,0.342020143325668));
#58921=DIRECTION('center_axis',(0.99026806874157,0.0476000039374394,-0.130779935984066));
#58922=DIRECTION('ref_axis',(-0.139173100960066,0.338691626801824,-0.930547596796366));
#58923=DIRECTION('',(-0.137844537491629,0.205926940351067,-0.968810083928407));
#58924=DIRECTION('center_axis',(0.,-0.978147600733806,-0.207911690817759));
#58925=DIRECTION('ref_axis',(-1.,0.,0.));
#58926=DIRECTION('',(-1.,0.,0.));
#58927=DIRECTION('center_axis',(0.,0.342020143325668,-0.939692620785909));
#58928=DIRECTION('ref_axis',(1.,0.,0.));
#58929=DIRECTION('center_axis',(1.,0.,0.));
#58930=DIRECTION('ref_axis',(0.,1.,0.));
#58931=DIRECTION('center_axis',(1.,0.,0.));
#58932=DIRECTION('ref_axis',(0.,0.,-1.));
#58933=DIRECTION('center_axis',(0.649305557988371,-0.712159014579632,-0.266892919198654));
#58934=DIRECTION('ref_axis',(0.760527640763576,0.608010520003998,0.227861614141252));
#58935=DIRECTION('',(1.,0.,0.));
#58936=DIRECTION('center_axis',(-0.99026806874157,0.024167155361971,-0.137058748836223));
#58937=DIRECTION('ref_axis',(0.139173100960065,0.171958245538723,-0.975223671657125));
#58938=DIRECTION('center_axis',(-0.0617712249622996,-0.949157344732972,
-0.30868211918754));
#58939=DIRECTION('ref_axis',(-0.998090334472114,0.0587427909490065,0.0191041551727457));
#58940=DIRECTION('center_axis',(0.284551435696759,-0.909927711321105,-0.301764876373726));
#58941=DIRECTION('ref_axis',(0.958660774436356,0.27008639921553,0.0895703997751285));
#58942=DIRECTION('center_axis',(0.491310548314114,-0.822564109591763,-0.286360316256974));
#58943=DIRECTION('ref_axis',(0.870984468928858,0.463997279083573,0.161531977910744));
#58944=DIRECTION('center_axis',(0.313150259135956,-0.901011253802641,-0.30019266434088));
#58945=DIRECTION('ref_axis',(0.949703593340092,0.297094703643677,0.0989839475056044));
#58946=DIRECTION('',(1.,0.,0.));
#58947=DIRECTION('center_axis',(-0.313150259135957,-0.901011253802641,-0.30019266434088));
#58948=DIRECTION('ref_axis',(-0.949703593340092,0.297094703643678,0.0989839475056048));
#58949=DIRECTION('center_axis',(-0.491310548314113,-0.822564109591764,-0.286360316256974));
#58950=DIRECTION('ref_axis',(-0.870984468928858,0.463997279083571,0.161531977910743));
#58951=DIRECTION('center_axis',(-0.284551435696759,-0.909927711321105,-0.301764876373726));
#58952=DIRECTION('ref_axis',(-0.958660774436356,0.270086399215529,0.0895703997751283));
#58953=DIRECTION('center_axis',(0.0617712249622997,-0.949157344732972,-0.30868211918754));
#58954=DIRECTION('ref_axis',(0.998090334472114,0.0587427909490066,0.0191041551727457));
#58955=DIRECTION('center_axis',(0.99026806874157,0.0241671553619711,-0.137058748836224));
#58956=DIRECTION('ref_axis',(-0.139173100960066,0.171958245538724,-0.975223671657125));
#58957=DIRECTION('',(1.,0.,0.));
#58958=DIRECTION('center_axis',(0.,0.951056516295154,0.309016994374947));
#58959=DIRECTION('ref_axis',(1.,0.,0.));
#58960=DIRECTION('',(-0.137844537491629,0.306067080296576,-0.941977614300068));
#58961=DIRECTION('center_axis',(-0.99026806874157,-0.0241671553619711,0.137058748836224));
#58962=DIRECTION('ref_axis',(0.,0.984807753012208,0.17364817766693));
#58963=DIRECTION('',(-0.137998583506848,0.298180416142191,-0.944481249352984));
#58964=DIRECTION('center_axis',(-0.0617712249622997,0.949157344732972,0.30868211918754));
#58965=DIRECTION('ref_axis',(0.998052578482889,0.0614306198252359,0.0108318757168334));
#58966=DIRECTION('',(0.0161503784824051,0.310182768482997,-0.950539749516609));
#58967=DIRECTION('center_axis',(0.284551435696759,0.909927711321105,0.301764876373726));
#58968=DIRECTION('ref_axis',(0.957826285221151,-0.282982425517402,-0.0498974366850414));
#58969=DIRECTION('',(0.0552259184163645,0.298695825212034,-0.952749128541176));
#58970=DIRECTION('center_axis',(0.491310548314113,0.822564109591764,0.286360316256974));
#58971=DIRECTION('ref_axis',(0.86824314212446,-0.488601473065054,-0.0861536225152692));
#58972=DIRECTION('',(0.057078643955053,0.297663645650825,-0.952962949154956));
#58973=DIRECTION('center_axis',(0.313150259135957,0.901011253802641,0.30019266434088));
#58974=DIRECTION('ref_axis',(0.948683298050513,-0.311423555691114,-0.0549123752965085));
#58975=DIRECTION('',(0.0225789275220278,0.30893821467004,-0.950814057294297));
#58976=DIRECTION('center_axis',(0.,0.951056516295154,0.309016994374947));
#58977=DIRECTION('ref_axis',(1.,0.,0.));
#58978=DIRECTION('',(-0.0225789275220274,0.30893821467004,-0.950814057294297));
#58979=DIRECTION('center_axis',(-0.313150259135956,0.901011253802641,0.30019266434088));
#58980=DIRECTION('ref_axis',(0.948683298050514,0.311423555691113,0.0549123752965084));
#58981=DIRECTION('',(-0.0570786439550527,0.297663645650825,-0.952962949154956));
#58982=DIRECTION('center_axis',(-0.491310548314114,0.822564109591763,0.286360316256974));
#58983=DIRECTION('ref_axis',(0.86824314212446,0.488601473065055,0.0861536225152694));
#58984=DIRECTION('',(-0.0552259184163635,0.298695825212034,-0.952749128541176));
#58985=DIRECTION('center_axis',(-0.284551435696759,0.909927711321105,0.301764876373726));
#58986=DIRECTION('ref_axis',(0.957826285221151,0.282982425517402,0.0498974366850415));
#58987=DIRECTION('',(-0.0161503784824052,0.310182768482997,-0.950539749516609));
#58988=DIRECTION('center_axis',(0.0617712249622996,0.949157344732972,0.30868211918754));
#58989=DIRECTION('ref_axis',(0.998052578482889,-0.0614306198252359,-0.0108318757168334));
#58990=DIRECTION('',(0.137998583506848,0.298180416142191,-0.944481249352984));
#58991=DIRECTION('center_axis',(0.99026806874157,-0.024167155361971,0.137058748836223));
#58992=DIRECTION('ref_axis',(0.,-0.984807753012208,-0.17364817766693));
#58993=DIRECTION('',(0.137844537491629,0.306067080296576,-0.941977614300068));
#58994=DIRECTION('center_axis',(0.,0.951056516295154,0.309016994374947));
#58995=DIRECTION('ref_axis',(1.,0.,0.));
#58996=DIRECTION('',(-0.051925424877728,0.308600119688995,-0.949773507937132));
#58997=DIRECTION('center_axis',(-0.649305557988371,0.712159014579632,0.266892919198654));
#58998=DIRECTION('ref_axis',(0.755033118392644,0.645725301830105,0.113858792838764));
#58999=DIRECTION('center_axis',(0.,-0.999390827019096,-0.0348994967025006));
#59000=DIRECTION('ref_axis',(-1.,0.,0.));
#59001=DIRECTION('',(-1.,0.,0.));
#59002=DIRECTION('',(0.137844537491629,0.0345663418323,-0.989850519773593));
#59003=DIRECTION('center_axis',(0.99026806874157,-0.024167155361971,0.137058748836223));
#59004=DIRECTION('ref_axis',(0.,-0.984807753012208,-0.17364817766693));
#59005=DIRECTION('center_axis',(-0.99026806874157,0.024167155361971,-0.137058748836223));
#59006=DIRECTION('ref_axis',(0.139173100960065,0.171958245538723,-0.975223671657125));
#59007=DIRECTION('',(0.137998583506848,0.0428336755604254,-0.989505769153514));
#59008=DIRECTION('center_axis',(0.0617712249622996,-0.997491655456914,-0.0345646215150937));
#59009=DIRECTION('ref_axis',(-0.998052578482889,-0.0614306198252359,-0.0108318757168334));
#59010=DIRECTION('center_axis',(-0.0617712249622996,0.997491655456914,0.0345646215150937));
#59011=DIRECTION('ref_axis',(0.998090334472114,0.061734173069449,0.00213918413755088));
#59012=DIRECTION('',(-0.0161503784824054,0.0336272827279992,-0.999303943318151));
#59013=DIRECTION('center_axis',(-0.284551435696759,-0.958262022045047,-0.0276473787012791));
#59014=DIRECTION('ref_axis',(-0.957826285221151,0.282982425517402,0.0498974366850415));
#59015=DIRECTION('center_axis',(0.284551435696759,0.958262022045047,0.0276473787012791));
#59016=DIRECTION('ref_axis',(-0.958660774436356,0.284433077286297,0.00820634526047697));
#59017=DIRECTION('',(-0.0552259184163638,0.0451771306857526,-0.997451314500147));
#59018=DIRECTION('center_axis',(-0.491310548314114,-0.870898420315705,-0.0122428185845276));
#59019=DIRECTION('ref_axis',(-0.86824314212446,0.488601473065055,0.0861536225152694));
#59020=DIRECTION('center_axis',(0.491310548314114,0.870898420315705,0.0122428185845276));
#59021=DIRECTION('ref_axis',(-0.870984468928858,0.491262009456284,0.0069060082312051));
#59022=DIRECTION('',(-0.0570786439550532,0.0462201931597179,-0.997299213951626));
#59023=DIRECTION('center_axis',(-0.313150259135956,-0.949345564526583,-0.0260751666684333));
#59024=DIRECTION('ref_axis',(-0.948683298050514,0.311423555691113,0.0549123752965084));
#59025=DIRECTION('center_axis',(0.313150259135956,0.949345564526583,0.0260751666684333));
#59026=DIRECTION('ref_axis',(-0.949703593340092,0.313032204601347,0.00859788807423104));
#59027=DIRECTION('',(-0.0225789275220273,0.0348905995476461,-0.999136045839184));
#59028=DIRECTION('center_axis',(0.,-0.999390827019096,-0.0348994967025006));
#59029=DIRECTION('ref_axis',(-1.,0.,0.));
#59030=DIRECTION('',(-1.,0.,0.));
#59031=DIRECTION('',(0.0225789275220281,0.0348905995476461,-0.999136045839184));
#59032=DIRECTION('center_axis',(0.313150259135957,-0.949345564526583,-0.0260751666684331));
#59033=DIRECTION('ref_axis',(-0.948683298050513,-0.311423555691114,-0.0549123752965085));
#59034=DIRECTION('center_axis',(-0.313150259135957,0.949345564526583,0.0260751666684331));
#59035=DIRECTION('ref_axis',(0.949703593340092,0.313032204601348,0.00859788807423098));
#59036=DIRECTION('',(0.0570786439550534,0.0462201931597177,-0.997299213951626));
#59037=DIRECTION('center_axis',(0.491310548314113,-0.870898420315706,-0.0122428185845275));
#59038=DIRECTION('ref_axis',(-0.86824314212446,-0.488601473065054,-0.0861536225152692));
#59039=DIRECTION('center_axis',(-0.491310548314113,0.870898420315706,0.0122428185845275));
#59040=DIRECTION('ref_axis',(0.870984468928858,0.491262009456283,0.00690600823120502));
#59041=DIRECTION('',(0.0552259184163649,0.045177130685753,-0.997451314500147));
#59042=DIRECTION('center_axis',(0.284551435696759,-0.958262022045047,-0.0276473787012793));
#59043=DIRECTION('ref_axis',(-0.957826285221151,-0.282982425517402,-0.0498974366850414));
#59044=DIRECTION('center_axis',(-0.284551435696759,0.958262022045047,0.0276473787012793));
#59045=DIRECTION('ref_axis',(0.958660774436356,0.284433077286297,0.008206345260477));
#59046=DIRECTION('',(0.0161503784824051,0.0336272827279992,-0.999303943318151));
#59047=DIRECTION('center_axis',(-0.0617712249622997,-0.997491655456914,
-0.0345646215150937));
#59048=DIRECTION('ref_axis',(-0.998052578482889,0.0614306198252359,0.0108318757168334));
#59049=DIRECTION('center_axis',(0.0617712249622997,0.997491655456914,0.0345646215150937));
#59050=DIRECTION('ref_axis',(-0.998090334472114,0.061734173069449,0.00213918413755088));
#59051=DIRECTION('',(-0.137998583506848,0.0428336755604254,-0.989505769153514));
#59052=DIRECTION('center_axis',(-0.99026806874157,-0.0241671553619711,0.137058748836224));
#59053=DIRECTION('ref_axis',(0.,0.984807753012208,0.17364817766693));
#59054=DIRECTION('center_axis',(0.99026806874157,0.0241671553619711,-0.137058748836224));
#59055=DIRECTION('ref_axis',(-0.139173100960066,0.171958245538724,-0.975223671657125));
#59056=DIRECTION('',(-0.137844537491629,0.0345663418322999,-0.989850519773593));
#59057=DIRECTION('center_axis',(0.,-0.999390827019096,-0.0348994967025006));
#59058=DIRECTION('ref_axis',(-1.,0.,0.));
#59059=DIRECTION('',(-1.,0.,0.));
#59060=DIRECTION('center_axis',(0.,0.17364817766693,-0.984807753012208));
#59061=DIRECTION('ref_axis',(1.,0.,0.));
#59062=DIRECTION('center_axis',(1.,0.,0.));
#59063=DIRECTION('ref_axis',(0.,1.,0.));
#59064=DIRECTION('center_axis',(1.,0.,0.));
#59065=DIRECTION('ref_axis',(0.,0.,-1.));
#59066=DIRECTION('center_axis',(0.649305557988371,-0.747685187986609,-0.139173100960065));
#59067=DIRECTION('ref_axis',(0.760527640763576,0.638341228068795,0.118819965419165));
#59068=DIRECTION('',(1.,0.,0.));
#59069=DIRECTION('center_axis',(-0.99026806874157,-2.55656838927233E-17,
-0.139173100960065));
#59070=DIRECTION('ref_axis',(-0.139173100960065,0.,0.99026806874157));
#59071=DIRECTION('center_axis',(-0.0617712249622996,-0.988339599396795,
-0.139173100960065));
#59072=DIRECTION('ref_axis',(-0.998090334472114,0.0611677576917705,0.00861334152950384));
#59073=DIRECTION('center_axis',(0.284551435696759,-0.948504785655862,-0.139173100960065));
#59074=DIRECTION('ref_axis',(0.958660774436356,0.281536916624453,0.0413096131025498));
#59075=DIRECTION('center_axis',(0.491310548314114,-0.859793459549701,-0.139173100960065));
#59076=DIRECTION('ref_axis',(0.870984468928858,0.484997851417207,0.0785056622506208));
#59077=DIRECTION('center_axis',(0.313150259135956,-0.939450777407866,-0.139173100960065));
#59078=DIRECTION('ref_axis',(0.949703593340092,0.309769549629784,0.0458902050450514));
#59079=DIRECTION('',(1.,0.,0.));
#59080=DIRECTION('center_axis',(-0.313150259135957,-0.939450777407865,-0.139173100960065));
#59081=DIRECTION('ref_axis',(-0.949703593340092,0.309769549629785,0.0458902050450517));
#59082=DIRECTION('center_axis',(-0.491310548314113,-0.859793459549702,-0.139173100960065));
#59083=DIRECTION('ref_axis',(-0.870984468928858,0.484997851417206,0.0785056622506207));
#59084=DIRECTION('center_axis',(-0.284551435696759,-0.948504785655862,-0.139173100960065));
#59085=DIRECTION('ref_axis',(-0.958660774436356,0.281536916624453,0.0413096131025497));
#59086=DIRECTION('center_axis',(0.0617712249622997,-0.988339599396795,-0.139173100960065));
#59087=DIRECTION('ref_axis',(0.998090334472114,0.0611677576917706,0.00861334152950384));
#59088=DIRECTION('center_axis',(0.99026806874157,-2.55656838927234E-17,
-0.139173100960066));
#59089=DIRECTION('ref_axis',(0.139173100960066,0.,0.99026806874157));
#59090=DIRECTION('',(1.,0.,0.));
#59091=DIRECTION('center_axis',(0.,0.99026806874157,0.139173100960065));
#59092=DIRECTION('ref_axis',(1.,0.,0.));
#59093=DIRECTION('',(-0.137844537491629,0.137844537491629,-0.980814848463989));
#59094=DIRECTION('center_axis',(-0.99026806874157,2.55656838927234E-17,
0.139173100960066));
#59095=DIRECTION('ref_axis',(0.,1.,-1.83697019872103E-16));
#59096=DIRECTION('',(-0.137998583506848,0.129642937822505,-0.981910942816534));
#59097=DIRECTION('center_axis',(-0.0617712249622997,0.988339599396795,0.139173100960065));
#59098=DIRECTION('ref_axis',(0.998052578482889,0.0623782861551806,-1.14587052714359E-17));
#59099=DIRECTION('',(0.0161503784824051,0.140410899949307,-0.989961587360995));
#59100=DIRECTION('center_axis',(0.284551435696759,0.948504785655862,0.139173100960065));
#59101=DIRECTION('ref_axis',(0.957826285221151,-0.287347885566345,5.27849502450877E-17));
#59102=DIRECTION('',(0.0552259184163645,0.128714814516259,-0.990142714187765));
#59103=DIRECTION('center_axis',(0.491310548314113,0.859793459549702,0.139173100960065));
#59104=DIRECTION('ref_axis',(0.86824314212446,-0.496138938356832,9.11392444186591E-17));
#59105=DIRECTION('',(0.057078643955053,0.12766118652195,-0.99017405028614));
#59106=DIRECTION('center_axis',(0.313150259135957,0.939450777407865,0.139173100960065));
#59107=DIRECTION('ref_axis',(0.948683298050513,-0.31622776601684,5.80900982181061E-17));
#59108=DIRECTION('',(0.0225789275220278,0.13913762065955,-0.990015613285545));
#59109=DIRECTION('center_axis',(0.,0.99026806874157,0.139173100960065));
#59110=DIRECTION('ref_axis',(1.,0.,0.));
#59111=DIRECTION('',(-0.0225789275220274,0.13913762065955,-0.990015613285545));
#59112=DIRECTION('center_axis',(-0.313150259135956,0.939450777407866,0.139173100960065));
#59113=DIRECTION('ref_axis',(0.948683298050514,0.316227766016839,-5.80900982181059E-17));
#59114=DIRECTION('',(-0.0570786439550527,0.12766118652195,-0.99017405028614));
#59115=DIRECTION('center_axis',(-0.491310548314114,0.859793459549701,0.139173100960065));
#59116=DIRECTION('ref_axis',(0.868243142124459,0.496138938356833,-9.11392444186592E-17));
#59117=DIRECTION('',(-0.0552259184163635,0.128714814516259,-0.990142714187765));
#59118=DIRECTION('center_axis',(-0.284551435696759,0.948504785655862,0.139173100960065));
#59119=DIRECTION('ref_axis',(0.957826285221151,0.287347885566346,-5.27849502450878E-17));
#59120=DIRECTION('',(-0.0161503784824052,0.140410899949307,-0.989961587360995));
#59121=DIRECTION('center_axis',(0.0617712249622996,0.988339599396795,0.139173100960065));
#59122=DIRECTION('ref_axis',(0.998052578482889,-0.0623782861551805,1.14587052714359E-17));
#59123=DIRECTION('',(0.137998583506848,0.129642937822505,-0.981910942816534));
#59124=DIRECTION('center_axis',(0.99026806874157,2.55656838927233E-17,0.139173100960065));
#59125=DIRECTION('ref_axis',(0.,-1.,1.83697019872103E-16));
#59126=DIRECTION('',(0.137844537491629,0.137844537491628,-0.980814848463989));
#59127=DIRECTION('center_axis',(0.,0.99026806874157,0.139173100960065));
#59128=DIRECTION('ref_axis',(1.,0.,0.));
#59129=DIRECTION('',(-0.051925424877728,0.138985351600606,-0.98893216263388));
#59130=DIRECTION('center_axis',(-0.649305557988371,0.747685187986609,0.139173100960065));
#59131=DIRECTION('ref_axis',(0.755033118392644,0.655686655446243,-1.20447684575381E-16));
#59132=DIRECTION('center_axis',(0.,-0.99026806874157,0.139173100960066));
#59133=DIRECTION('ref_axis',(-1.,0.,0.));
#59134=DIRECTION('',(-1.,0.,0.));
#59135=DIRECTION('',(0.137844537491629,-0.137844537491629,-0.980814848463989));
#59136=DIRECTION('center_axis',(0.99026806874157,2.55656838927233E-17,0.139173100960065));
#59137=DIRECTION('ref_axis',(0.,-1.,1.83697019872103E-16));
#59138=DIRECTION('center_axis',(-0.99026806874157,-2.55656838927233E-17,
-0.139173100960065));
#59139=DIRECTION('ref_axis',(-0.139173100960065,0.,0.99026806874157));
#59140=DIRECTION('',(0.137998583506848,-0.129642937822505,-0.981910942816534));
#59141=DIRECTION('center_axis',(0.0617712249622996,-0.988339599396795,0.139173100960066));
#59142=DIRECTION('ref_axis',(-0.998052578482889,-0.0623782861551805,1.14587052714359E-17));
#59143=DIRECTION('center_axis',(-0.0617712249622996,0.988339599396795,-0.139173100960066));
#59144=DIRECTION('ref_axis',(0.998090334472114,0.0611677576917705,-0.00861334152950386));
#59145=DIRECTION('',(-0.0161503784824054,-0.140410899949307,-0.989961587360995));
#59146=DIRECTION('center_axis',(-0.284551435696759,-0.948504785655862,0.139173100960066));
#59147=DIRECTION('ref_axis',(-0.957826285221151,0.287347885566346,-5.27849502450878E-17));
#59148=DIRECTION('center_axis',(0.284551435696759,0.948504785655862,-0.139173100960066));
#59149=DIRECTION('ref_axis',(-0.958660774436356,0.281536916624453,-0.0413096131025499));
#59150=DIRECTION('',(-0.0552259184163638,-0.12871481451626,-0.990142714187765));
#59151=DIRECTION('center_axis',(-0.491310548314114,-0.859793459549701,0.139173100960066));
#59152=DIRECTION('ref_axis',(-0.868243142124459,0.496138938356833,-9.11392444186592E-17));
#59153=DIRECTION('center_axis',(0.491310548314114,0.859793459549701,-0.139173100960066));
#59154=DIRECTION('ref_axis',(-0.870984468928858,0.484997851417207,-0.078505662250621));
#59155=DIRECTION('',(-0.0570786439550532,-0.12766118652195,-0.99017405028614));
#59156=DIRECTION('center_axis',(-0.313150259135956,-0.939450777407866,0.139173100960066));
#59157=DIRECTION('ref_axis',(-0.948683298050514,0.316227766016839,-5.80900982181059E-17));
#59158=DIRECTION('center_axis',(0.313150259135956,0.939450777407866,-0.139173100960066));
#59159=DIRECTION('ref_axis',(-0.949703593340092,0.309769549629784,-0.0458902050450515));
#59160=DIRECTION('',(-0.0225789275220273,-0.139137620659551,-0.990015613285545));
#59161=DIRECTION('center_axis',(0.,-0.99026806874157,0.139173100960066));
#59162=DIRECTION('ref_axis',(-1.,0.,0.));
#59163=DIRECTION('',(-1.,0.,0.));
#59164=DIRECTION('',(0.0225789275220281,-0.139137620659551,-0.990015613285545));
#59165=DIRECTION('center_axis',(0.313150259135957,-0.939450777407865,0.139173100960066));
#59166=DIRECTION('ref_axis',(-0.948683298050513,-0.31622776601684,5.80900982181061E-17));
#59167=DIRECTION('center_axis',(-0.313150259135957,0.939450777407865,-0.139173100960066));
#59168=DIRECTION('ref_axis',(0.949703593340092,0.309769549629785,-0.0458902050450518));
#59169=DIRECTION('',(0.0570786439550534,-0.12766118652195,-0.99017405028614));
#59170=DIRECTION('center_axis',(0.491310548314113,-0.859793459549702,0.139173100960066));
#59171=DIRECTION('ref_axis',(-0.86824314212446,-0.496138938356832,9.11392444186591E-17));
#59172=DIRECTION('center_axis',(-0.491310548314113,0.859793459549702,-0.139173100960066));
#59173=DIRECTION('ref_axis',(0.870984468928858,0.484997851417206,-0.0785056622506209));
#59174=DIRECTION('',(0.0552259184163649,-0.128714814516259,-0.990142714187765));
#59175=DIRECTION('center_axis',(0.284551435696759,-0.948504785655862,0.139173100960066));
#59176=DIRECTION('ref_axis',(-0.957826285221151,-0.287347885566345,5.27849502450877E-17));
#59177=DIRECTION('center_axis',(-0.284551435696759,0.948504785655862,-0.139173100960066));
#59178=DIRECTION('ref_axis',(0.958660774436356,0.281536916624453,-0.0413096131025498));
#59179=DIRECTION('',(0.0161503784824051,-0.140410899949307,-0.989961587360995));
#59180=DIRECTION('center_axis',(-0.0617712249622997,-0.988339599396795,
0.139173100960066));
#59181=DIRECTION('ref_axis',(-0.998052578482889,0.0623782861551806,-1.14587052714359E-17));
#59182=DIRECTION('center_axis',(0.0617712249622997,0.988339599396795,-0.139173100960066));
#59183=DIRECTION('ref_axis',(-0.998090334472114,0.0611677576917706,-0.00861334152950387));
#59184=DIRECTION('',(-0.137998583506848,-0.129642937822505,-0.981910942816533));
#59185=DIRECTION('center_axis',(-0.99026806874157,2.55656838927234E-17,
0.139173100960066));
#59186=DIRECTION('ref_axis',(0.,1.,-1.83697019872103E-16));
#59187=DIRECTION('center_axis',(0.99026806874157,-2.55656838927234E-17,
-0.139173100960066));
#59188=DIRECTION('ref_axis',(0.139173100960066,0.,0.99026806874157));
#59189=DIRECTION('',(-0.137844537491629,-0.137844537491629,-0.980814848463989));
#59190=DIRECTION('center_axis',(0.,-0.99026806874157,0.139173100960066));
#59191=DIRECTION('ref_axis',(-1.,0.,0.));
#59192=DIRECTION('',(-1.,0.,0.));
#59193=DIRECTION('center_axis',(0.,-1.83697019872103E-16,-1.));
#59194=DIRECTION('ref_axis',(1.,0.,0.));
#59195=DIRECTION('center_axis',(1.,0.,0.));
#59196=DIRECTION('ref_axis',(0.,1.,0.));
#59197=DIRECTION('center_axis',(1.,0.,0.));
#59198=DIRECTION('ref_axis',(0.,0.,-1.));
#59199=DIRECTION('center_axis',(0.64930555798837,-0.760493325303574,-0.00722457847379238));
#59200=DIRECTION('ref_axis',(0.760527640763576,0.649276260934969,0.00616803217361931));
#59201=DIRECTION('',(1.,0.,0.));
#59202=DIRECTION('center_axis',(-0.99026806874157,-0.0241671553619711,-0.137058748836223));
#59203=DIRECTION('ref_axis',(-0.139173100960065,0.171958245538723,0.975223671657125));
#59204=DIRECTION('center_axis',(-0.0617712249622996,-0.997491655456914,
0.0345646215150941));
#59205=DIRECTION('ref_axis',(-0.998090334472114,0.061734173069449,-0.0021391841375509));
#59206=DIRECTION('center_axis',(0.284551435696759,-0.958262022045047,0.0276473787012795));
#59207=DIRECTION('ref_axis',(0.958660774436356,0.284433077286297,-0.00820634526047709));
#59208=DIRECTION('center_axis',(0.491310548314114,-0.870898420315705,0.012242818584528));
#59209=DIRECTION('ref_axis',(0.870984468928858,0.491262009456284,-0.00690600823120533));
#59210=DIRECTION('center_axis',(0.313150259135956,-0.949345564526583,0.0260751666684337));
#59211=DIRECTION('ref_axis',(0.949703593340092,0.313032204601347,-0.00859788807423114));
#59212=DIRECTION('',(1.,0.,0.));
#59213=DIRECTION('center_axis',(-0.313150259135957,-0.949345564526583,0.0260751666684335));
#59214=DIRECTION('ref_axis',(-0.949703593340092,0.313032204601348,-0.00859788807423111));
#59215=DIRECTION('center_axis',(-0.491310548314113,-0.870898420315706,0.012242818584528));
#59216=DIRECTION('ref_axis',(-0.870984468928858,0.491262009456283,-0.00690600823120528));
#59217=DIRECTION('center_axis',(-0.284551435696759,-0.958262022045047,0.0276473787012796));
#59218=DIRECTION('ref_axis',(-0.958660774436356,0.284433077286297,-0.00820634526047711));
#59219=DIRECTION('center_axis',(0.0617712249622997,-0.997491655456914,0.0345646215150942));
#59220=DIRECTION('ref_axis',(0.998090334472114,0.061734173069449,-0.00213918413755091));
#59221=DIRECTION('center_axis',(0.99026806874157,-0.0241671553619711,-0.137058748836224));
#59222=DIRECTION('ref_axis',(0.139173100960066,0.171958245538724,0.975223671657125));
#59223=DIRECTION('',(1.,0.,0.));
#59224=DIRECTION('center_axis',(0.,0.999390827019096,-0.0348994967025008));
#59225=DIRECTION('ref_axis',(1.,0.,0.));
#59226=DIRECTION('',(-0.137844537491629,-0.0345663418323001,-0.989850519773593));
#59227=DIRECTION('center_axis',(-0.99026806874157,0.0241671553619711,0.137058748836224));
#59228=DIRECTION('ref_axis',(0.,0.984807753012208,-0.17364817766693));
#59229=DIRECTION('',(-0.137998583506848,-0.0428336755604259,-0.989505769153514));
#59230=DIRECTION('center_axis',(-0.0617712249622997,0.997491655456914,-0.0345646215150942));
#59231=DIRECTION('ref_axis',(0.998052578482889,0.0614306198252359,-0.0108318757168334));
#59232=DIRECTION('',(0.0161503784824051,-0.0336272827279996,-0.999303943318151));
#59233=DIRECTION('center_axis',(0.284551435696759,0.958262022045047,-0.0276473787012796));
#59234=DIRECTION('ref_axis',(0.957826285221151,-0.282982425517402,0.0498974366850415));
#59235=DIRECTION('',(0.0552259184163645,-0.0451771306857534,-0.997451314500147));
#59236=DIRECTION('center_axis',(0.491310548314113,0.870898420315706,-0.012242818584528));
#59237=DIRECTION('ref_axis',(0.86824314212446,-0.488601473065054,0.0861536225152694));
#59238=DIRECTION('',(0.057078643955053,-0.0462201931597181,-0.997299213951626));
#59239=DIRECTION('center_axis',(0.313150259135957,0.949345564526583,-0.0260751666684335));
#59240=DIRECTION('ref_axis',(0.948683298050513,-0.311423555691114,0.0549123752965087));
#59241=DIRECTION('',(0.0225789275220278,-0.0348905995476464,-0.999136045839184));
#59242=DIRECTION('center_axis',(0.,0.999390827019096,-0.0348994967025009));
#59243=DIRECTION('ref_axis',(1.,0.,0.));
#59244=DIRECTION('',(-0.0225789275220274,-0.0348905995476464,-0.999136045839184));
#59245=DIRECTION('center_axis',(-0.313150259135956,0.949345564526583,-0.0260751666684337));
#59246=DIRECTION('ref_axis',(0.948683298050514,0.311423555691113,-0.0549123752965085));
#59247=DIRECTION('',(-0.0570786439550527,-0.046220193159718,-0.997299213951626));
#59248=DIRECTION('center_axis',(-0.491310548314114,0.870898420315705,-0.012242818584528));
#59249=DIRECTION('ref_axis',(0.868243142124459,0.488601473065055,-0.0861536225152696));
#59250=DIRECTION('',(-0.0552259184163635,-0.0451771306857529,-0.997451314500147));
#59251=DIRECTION('center_axis',(-0.284551435696759,0.958262022045047,-0.0276473787012795));
#59252=DIRECTION('ref_axis',(0.957826285221151,0.282982425517402,-0.0498974366850416));
#59253=DIRECTION('',(-0.0161503784824052,-0.0336272827279995,-0.999303943318151));
#59254=DIRECTION('center_axis',(0.0617712249622996,0.997491655456914,-0.0345646215150941));
#59255=DIRECTION('ref_axis',(0.998052578482889,-0.0614306198252359,0.0108318757168334));
#59256=DIRECTION('',(0.137998583506848,-0.0428336755604257,-0.989505769153514));
#59257=DIRECTION('center_axis',(0.99026806874157,0.0241671553619711,0.137058748836223));
#59258=DIRECTION('ref_axis',(0.,-0.984807753012208,0.17364817766693));
#59259=DIRECTION('',(0.137844537491629,-0.0345663418323003,-0.989850519773593));
#59260=DIRECTION('center_axis',(0.,0.999390827019096,-0.0348994967025009));
#59261=DIRECTION('ref_axis',(1.,0.,0.));
#59262=DIRECTION('',(-0.051925424877728,-0.0348524160661845,-0.998042613992818));
#59263=DIRECTION('center_axis',(-0.64930555798837,0.760493325303574,0.00722457847379238));
#59264=DIRECTION('ref_axis',(0.755033118392644,0.645725301830105,-0.113858792838765));
#59265=DIRECTION('center_axis',(0.,-0.951056516295154,0.309016994374947));
#59266=DIRECTION('ref_axis',(-1.,0.,0.));
#59267=DIRECTION('',(-1.,0.,0.));
#59268=DIRECTION('',(0.137844537491629,-0.306067080296576,-0.941977614300068));
#59269=DIRECTION('center_axis',(0.99026806874157,0.0241671553619711,0.137058748836223));
#59270=DIRECTION('ref_axis',(0.,-0.984807753012208,0.17364817766693));
#59271=DIRECTION('center_axis',(-0.99026806874157,-0.0241671553619711,-0.137058748836223));
#59272=DIRECTION('ref_axis',(-0.139173100960065,0.171958245538723,0.975223671657125));
#59273=DIRECTION('',(0.137998583506848,-0.298180416142191,-0.944481249352984));
#59274=DIRECTION('center_axis',(0.0617712249622996,-0.949157344732972,0.308682119187541));
#59275=DIRECTION('ref_axis',(-0.998052578482889,-0.0614306198252359,0.0108318757168334));
#59276=DIRECTION('center_axis',(-0.0617712249622996,0.949157344732972,-0.308682119187541));
#59277=DIRECTION('ref_axis',(0.998090334472114,0.0587427909490065,-0.0191041551727457));
#59278=DIRECTION('',(-0.0161503784824054,-0.310182768482997,-0.950539749516609));
#59279=DIRECTION('center_axis',(-0.284551435696759,-0.909927711321104,0.301764876373726));
#59280=DIRECTION('ref_axis',(-0.957826285221151,0.282982425517402,-0.0498974366850416));
#59281=DIRECTION('center_axis',(0.284551435696759,0.909927711321104,-0.301764876373726));
#59282=DIRECTION('ref_axis',(-0.958660774436356,0.27008639921553,-0.0895703997751286));
#59283=DIRECTION('',(-0.0552259184163638,-0.298695825212034,-0.952749128541176));
#59284=DIRECTION('center_axis',(-0.491310548314114,-0.822564109591763,0.286360316256975));
#59285=DIRECTION('ref_axis',(-0.868243142124459,0.488601473065055,-0.0861536225152696));
#59286=DIRECTION('center_axis',(0.491310548314114,0.822564109591763,-0.286360316256975));
#59287=DIRECTION('ref_axis',(-0.870984468928858,0.463997279083572,-0.161531977910744));
#59288=DIRECTION('',(-0.0570786439550532,-0.297663645650825,-0.952962949154956));
#59289=DIRECTION('center_axis',(-0.313150259135956,-0.901011253802641,0.30019266434088));
#59290=DIRECTION('ref_axis',(-0.948683298050514,0.311423555691113,-0.0549123752965085));
#59291=DIRECTION('center_axis',(0.313150259135956,0.901011253802641,-0.30019266434088));
#59292=DIRECTION('ref_axis',(-0.949703593340092,0.297094703643677,-0.0989839475056044));
#59293=DIRECTION('',(-0.0225789275220273,-0.30893821467004,-0.950814057294297));
#59294=DIRECTION('center_axis',(0.,-0.951056516295154,0.309016994374947));
#59295=DIRECTION('ref_axis',(-1.,0.,0.));
#59296=DIRECTION('',(-1.,0.,0.));
#59297=DIRECTION('',(0.0225789275220281,-0.30893821467004,-0.950814057294297));
#59298=DIRECTION('center_axis',(0.313150259135957,-0.901011253802641,0.30019266434088));
#59299=DIRECTION('ref_axis',(-0.948683298050513,-0.311423555691114,0.0549123752965087));
#59300=DIRECTION('center_axis',(-0.313150259135957,0.901011253802641,-0.30019266434088));
#59301=DIRECTION('ref_axis',(0.949703593340092,0.297094703643678,-0.0989839475056049));
#59302=DIRECTION('',(0.0570786439550533,-0.297663645650825,-0.952962949154956));
#59303=DIRECTION('center_axis',(0.491310548314113,-0.822564109591764,0.286360316256975));
#59304=DIRECTION('ref_axis',(-0.86824314212446,-0.488601473065054,0.0861536225152694));
#59305=DIRECTION('center_axis',(-0.491310548314113,0.822564109591764,-0.286360316256975));
#59306=DIRECTION('ref_axis',(0.870984468928858,0.463997279083571,-0.161531977910744));
#59307=DIRECTION('',(0.0552259184163649,-0.298695825212034,-0.952749128541176));
#59308=DIRECTION('center_axis',(0.284551435696759,-0.909927711321105,0.301764876373726));
#59309=DIRECTION('ref_axis',(-0.957826285221151,-0.282982425517402,0.0498974366850415));
#59310=DIRECTION('center_axis',(-0.284551435696759,0.909927711321105,-0.301764876373726));
#59311=DIRECTION('ref_axis',(0.958660774436356,0.270086399215529,-0.0895703997751284));
#59312=DIRECTION('',(0.0161503784824051,-0.310182768482997,-0.950539749516609));
#59313=DIRECTION('center_axis',(-0.0617712249622997,-0.949157344732972,
0.308682119187541));
#59314=DIRECTION('ref_axis',(-0.998052578482889,0.0614306198252359,-0.0108318757168334));
#59315=DIRECTION('center_axis',(0.0617712249622997,0.949157344732972,-0.308682119187541));
#59316=DIRECTION('ref_axis',(-0.998090334472114,0.0587427909490066,-0.0191041551727457));
#59317=DIRECTION('',(-0.137998583506848,-0.298180416142191,-0.944481249352984));
#59318=DIRECTION('center_axis',(-0.99026806874157,0.0241671553619711,0.137058748836224));
#59319=DIRECTION('ref_axis',(0.,0.984807753012208,-0.17364817766693));
#59320=DIRECTION('center_axis',(0.99026806874157,-0.0241671553619711,-0.137058748836224));
#59321=DIRECTION('ref_axis',(0.139173100960066,0.171958245538724,0.975223671657125));
#59322=DIRECTION('',(-0.137844537491629,-0.306067080296576,-0.941977614300068));
#59323=DIRECTION('center_axis',(0.,-0.951056516295154,0.309016994374948));
#59324=DIRECTION('ref_axis',(-1.,0.,0.));
#59325=DIRECTION('',(-1.,0.,0.));
#59326=DIRECTION('center_axis',(0.,-0.17364817766693,-0.984807753012208));
#59327=DIRECTION('ref_axis',(1.,0.,0.));
#59328=DIRECTION('center_axis',(1.,0.,0.));
#59329=DIRECTION('ref_axis',(0.,1.,0.));
#59330=DIRECTION('center_axis',(1.,0.,0.));
#59331=DIRECTION('ref_axis',(0.,0.,-1.));
#59332=DIRECTION('center_axis',(0.64930555798837,-0.75019425775938,0.124943459173594));
#59333=DIRECTION('ref_axis',(0.760527640763576,0.640483363162275,-0.106671313608347));
#59334=DIRECTION('',(1.,0.,0.));
#59335=DIRECTION('center_axis',(-0.99026806874157,-0.0476000039374394,-0.130779935984066));
#59336=DIRECTION('ref_axis',(-0.139173100960065,0.338691626801824,0.930547596796367));
#59337=DIRECTION('center_axis',(-0.0617712249622996,-0.976335432321108,
0.207252115456061));
#59338=DIRECTION('ref_axis',(-0.998090334472114,0.0604248268374111,-0.0128267117770656));
#59339=DIRECTION('center_axis',(0.284551435696759,-0.938902951798372,0.193627806751035));
#59340=DIRECTION('ref_axis',(0.958660774436356,0.278686882824878,-0.0574729579753757));
#59341=DIRECTION('center_axis',(0.491310548314114,-0.855541573276281,0.163286746281596));
#59342=DIRECTION('ref_axis',(0.870984468928858,0.482599419928604,-0.0921078431475355));
#59343=DIRECTION('center_axis',(0.313150259135956,-0.930394967059196,0.190531153552384));
#59344=DIRECTION('ref_axis',(0.949703593340092,0.306783534438035,-0.0628247387151197));
#59345=DIRECTION('',(1.,0.,0.));
#59346=DIRECTION('center_axis',(-0.313150259135957,-0.930394967059195,0.190531153552384));
#59347=DIRECTION('ref_axis',(-0.949703593340092,0.306783534438037,-0.0628247387151199));
#59348=DIRECTION('center_axis',(-0.491310548314113,-0.855541573276282,0.163286746281596));
#59349=DIRECTION('ref_axis',(-0.870984468928858,0.482599419928602,-0.0921078431475352));
#59350=DIRECTION('center_axis',(-0.284551435696759,-0.938902951798373,0.193627806751036));
#59351=DIRECTION('ref_axis',(-0.958660774436356,0.278686882824878,-0.0574729579753756));
#59352=DIRECTION('center_axis',(0.0617712249622997,-0.976335432321108,0.207252115456061));
#59353=DIRECTION('ref_axis',(0.998090334472114,0.0604248268374111,-0.0128267117770656));
#59354=DIRECTION('center_axis',(0.99026806874157,-0.0476000039374395,-0.130779935984066));
#59355=DIRECTION('ref_axis',(0.139173100960066,0.338691626801825,0.930547596796366));
#59356=DIRECTION('',(1.,0.,0.));
#59357=DIRECTION('center_axis',(0.,0.978147600733806,-0.20791169081776));
#59358=DIRECTION('ref_axis',(1.,0.,0.));
#59359=DIRECTION('',(-0.137844537491629,-0.205926940351068,-0.968810083928407));
#59360=DIRECTION('center_axis',(-0.99026806874157,0.0476000039374395,0.130779935984066));
#59361=DIRECTION('ref_axis',(0.,0.939692620785908,-0.342020143325669));
#59362=DIRECTION('',(-0.137998583506848,-0.21400880938634,-0.967034963408844));
#59363=DIRECTION('center_axis',(-0.0617712249622997,0.976335432321108,-0.207252115456061));
#59364=DIRECTION('ref_axis',(0.998052578482889,0.058616415197295,-0.0213346303712045));
#59365=DIRECTION('',(0.0161503784824051,-0.206643717435843,-0.978282954629779));
#59366=DIRECTION('center_axis',(0.284551435696759,0.938902951798373,-0.193627806751036));
#59367=DIRECTION('ref_axis',(0.957826285221151,-0.270018687665128,0.0982787650057295));
#59368=DIRECTION('',(0.0552259184163645,-0.217696391632611,-0.974452861356161));
#59369=DIRECTION('center_axis',(0.491310548314113,0.855541573276282,-0.163286746281596));
#59370=DIRECTION('ref_axis',(0.86824314212446,-0.46621809925847,0.169689510806249));
#59371=DIRECTION('',(0.057078643955053,-0.218697195660775,-0.974121945658943));
#59372=DIRECTION('center_axis',(0.313150259135957,0.930394967059195,-0.190531153552384));
#59373=DIRECTION('ref_axis',(0.948683298050513,-0.297156898213637,0.108156265856636));
#59374=DIRECTION('',(0.0225789275220278,-0.207858686543084,-0.977898235227234));
#59375=DIRECTION('center_axis',(0.,0.978147600733806,-0.20791169081776));
#59376=DIRECTION('ref_axis',(1.,0.,0.));
#59377=DIRECTION('',(-0.0225789275220274,-0.207858686543084,-0.977898235227234));
#59378=DIRECTION('center_axis',(-0.313150259135956,0.930394967059196,-0.190531153552384));
#59379=DIRECTION('ref_axis',(0.948683298050514,0.297156898213636,-0.108156265856635));
#59380=DIRECTION('',(-0.0570786439550527,-0.218697195660775,-0.974121945658943));
#59381=DIRECTION('center_axis',(-0.491310548314114,0.855541573276281,-0.163286746281596));
#59382=DIRECTION('ref_axis',(0.868243142124459,0.466218099258471,-0.16968951080625));
#59383=DIRECTION('',(-0.0552259184163635,-0.217696391632611,-0.974452861356161));
#59384=DIRECTION('center_axis',(-0.284551435696759,0.938902951798372,-0.193627806751035));
#59385=DIRECTION('ref_axis',(0.957826285221151,0.270018687665129,-0.0982787650057297));
#59386=DIRECTION('',(-0.0161503784824052,-0.206643717435842,-0.978282954629779));
#59387=DIRECTION('center_axis',(0.0617712249622996,0.976335432321108,-0.207252115456061));
#59388=DIRECTION('ref_axis',(0.998052578482889,-0.0586164151972949,0.0213346303712045));
#59389=DIRECTION('',(0.137998583506848,-0.214008809386339,-0.967034963408844));
#59390=DIRECTION('center_axis',(0.99026806874157,0.0476000039374394,0.130779935984066));
#59391=DIRECTION('ref_axis',(0.,-0.939692620785908,0.342020143325669));
#59392=DIRECTION('',(0.137844537491629,-0.205926940351068,-0.968810083928407));
#59393=DIRECTION('center_axis',(0.,0.978147600733805,-0.20791169081776));
#59394=DIRECTION('ref_axis',(1.,0.,0.));
#59395=DIRECTION('',(-0.0519254248777279,-0.207631210706979,-0.976828045559515));
#59396=DIRECTION('center_axis',(-0.64930555798837,0.75019425775938,-0.124943459173594));
#59397=DIRECTION('ref_axis',(0.755033118392644,0.616143911670627,-0.224258043872453));
#59398=DIRECTION('center_axis',(0.,-0.882947592858927,0.469471562785891));
#59399=DIRECTION('ref_axis',(-1.,0.,0.));
#59400=DIRECTION('',(-1.,0.,0.));
#59401=DIRECTION('',(0.137844537491629,-0.464989929744128,-0.874518866989312));
#59402=DIRECTION('center_axis',(0.99026806874157,0.0476000039374394,0.130779935984066));
#59403=DIRECTION('ref_axis',(0.,-0.939692620785908,0.342020143325669));
#59404=DIRECTION('center_axis',(-0.99026806874157,-0.0476000039374394,-0.130779935984066));
#59405=DIRECTION('ref_axis',(-0.139173100960065,0.338691626801824,0.930547596796367));
#59406=DIRECTION('',(0.137998583506848,-0.457657833403968,-0.878353971058416));
#59407=DIRECTION('center_axis',(0.0617712249622996,-0.881135424446229,0.468811987424192));
#59408=DIRECTION('ref_axis',(-0.998052578482889,-0.0586164151972949,0.0213346303712045));
#59409=DIRECTION('center_axis',(-0.0617712249622996,0.881135424446229,-0.468811987424192));
#59410=DIRECTION('ref_axis',(0.998090334472114,0.0545329542285434,-0.0290144987282327));
#59411=DIRECTION('',(-0.0161503784824054,-0.470529890556387,-0.882236242379483));
#59412=DIRECTION('center_axis',(-0.284551435696759,-0.843702943923494,0.455187678719167));
#59413=DIRECTION('ref_axis',(-0.957826285221151,0.270018687665129,-0.0982787650057297));
#59414=DIRECTION('center_axis',(0.284551435696759,0.843702943923494,-0.455187678719167));
#59415=DIRECTION('ref_axis',(-0.958660774436356,0.250429443236754,-0.13510963517535));
#59416=DIRECTION('',(-0.0552259184163638,-0.459601114406123,-0.886406742738185));
#59417=DIRECTION('center_axis',(-0.491310548314114,-0.760341565401402,0.424846618249728));
#59418=DIRECTION('ref_axis',(-0.868243142124459,0.466218099258471,-0.16968951080625));
#59419=DIRECTION('center_axis',(0.491310548314114,0.760341565401402,-0.424846618249728));
#59420=DIRECTION('ref_axis',(-0.870984468928858,0.428898384218936,-0.239650226161174));
#59421=DIRECTION('',(-0.0570786439550532,-0.458621745531674,-0.886796551036219));
#59422=DIRECTION('center_axis',(-0.313150259135956,-0.835194959184317,0.452091025520515));
#59423=DIRECTION('ref_axis',(-0.948683298050514,0.297156898213636,-0.108156265856635));
#59424=DIRECTION('center_axis',(0.313150259135956,0.835194959184317,-0.452091025520515));
#59425=DIRECTION('ref_axis',(-0.949703593340092,0.27539278542453,-0.149070112809494));
#59426=DIRECTION('',(-0.0225789275220273,-0.469351877358061,-0.88272249730729));
#59427=DIRECTION('center_axis',(0.,-0.882947592858927,0.469471562785891));
#59428=DIRECTION('ref_axis',(-1.,0.,0.));
#59429=DIRECTION('',(-1.,0.,0.));
#59430=DIRECTION('',(0.0225789275220281,-0.469351877358061,-0.88272249730729));
#59431=DIRECTION('center_axis',(0.313150259135957,-0.835194959184316,0.452091025520515));
#59432=DIRECTION('ref_axis',(-0.948683298050513,-0.297156898213637,0.108156265856636));
#59433=DIRECTION('center_axis',(-0.313150259135957,0.835194959184316,-0.452091025520515));
#59434=DIRECTION('ref_axis',(0.949703593340092,0.275392785424531,-0.149070112809495));
#59435=DIRECTION('',(0.0570786439550534,-0.458621745531674,-0.886796551036219));
#59436=DIRECTION('center_axis',(0.491310548314113,-0.760341565401403,0.424846618249728));
#59437=DIRECTION('ref_axis',(-0.86824314212446,-0.46621809925847,0.169689510806249));
#59438=DIRECTION('center_axis',(-0.491310548314113,0.760341565401403,-0.424846618249728));
#59439=DIRECTION('ref_axis',(0.870984468928858,0.428898384218935,-0.239650226161174));
#59440=DIRECTION('',(0.0552259184163649,-0.459601114406122,-0.886406742738185));
#59441=DIRECTION('center_axis',(0.284551435696759,-0.843702943923494,0.455187678719167));
#59442=DIRECTION('ref_axis',(-0.957826285221151,-0.270018687665128,0.0982787650057295));
#59443=DIRECTION('center_axis',(-0.284551435696759,0.843702943923494,-0.455187678719167));
#59444=DIRECTION('ref_axis',(0.958660774436356,0.250429443236754,-0.135109635175349));
#59445=DIRECTION('',(0.0161503784824051,-0.470529890556387,-0.882236242379483));
#59446=DIRECTION('center_axis',(-0.0617712249622997,-0.881135424446229,
0.468811987424192));
#59447=DIRECTION('ref_axis',(-0.998052578482889,0.058616415197295,-0.0213346303712045));
#59448=DIRECTION('center_axis',(0.0617712249622997,0.881135424446229,-0.468811987424192));
#59449=DIRECTION('ref_axis',(-0.998090334472114,0.0545329542285434,-0.0290144987282328));
#59450=DIRECTION('',(-0.137998583506848,-0.457657833403968,-0.878353971058416));
#59451=DIRECTION('center_axis',(-0.99026806874157,0.0476000039374395,0.130779935984066));
#59452=DIRECTION('ref_axis',(0.,0.939692620785908,-0.342020143325669));
#59453=DIRECTION('center_axis',(0.99026806874157,-0.0476000039374395,-0.130779935984066));
#59454=DIRECTION('ref_axis',(0.139173100960066,0.338691626801825,0.930547596796366));
#59455=DIRECTION('',(-0.137844537491629,-0.464989929744128,-0.874518866989312));
#59456=DIRECTION('center_axis',(0.,-0.882947592858927,0.469471562785891));
#59457=DIRECTION('ref_axis',(-1.,0.,0.));
#59458=DIRECTION('',(-1.,0.,0.));
#59459=DIRECTION('center_axis',(0.,-0.342020143325669,-0.939692620785908));
#59460=DIRECTION('ref_axis',(1.,0.,0.));
#59461=DIRECTION('center_axis',(1.,0.,0.));
#59462=DIRECTION('ref_axis',(0.,1.,0.));
#59463=DIRECTION('center_axis',(1.,0.,0.));
#59464=DIRECTION('ref_axis',(0.,0.,-1.));
#59465=DIRECTION('center_axis',(0.64930555798837,-0.717100917309779,0.253315153038432));
#59466=DIRECTION('ref_axis',(0.760527640763576,0.612229702500115,-0.216269505504613));
#59467=DIRECTION('',(1.,0.,0.));
#59468=DIRECTION('center_axis',(-0.99026806874157,-0.0695865504800327,-0.120527440954873));
#59469=DIRECTION('ref_axis',(-0.139173100960065,0.495134034370783,0.857597304086756));
#59470=DIRECTION('center_axis',(-0.0617712249622996,-0.925513751123792,
0.373642358743525));
#59471=DIRECTION('ref_axis',(-0.998090334472114,0.0572795028183562,-0.0231245062698635));
#59472=DIRECTION('center_axis',(0.284551435696759,-0.891015790469123,0.353724951873058));
#59473=DIRECTION('ref_axis',(0.958660774436356,0.264472928451193,-0.104993283944912));
#59474=DIRECTION('center_axis',(0.491310548314114,-0.814189528457782,0.309369288819978));
#59475=DIRECTION('ref_axis',(0.870984468928858,0.459273291233482,-0.174511027858645));
#59476=DIRECTION('center_axis',(0.313150259135956,-0.883174789320284,0.34919794774906));
#59477=DIRECTION('ref_axis',(0.949703593340092,0.291213401820783,-0.115142691461001));
#59478=DIRECTION('',(1.,0.,0.));
#59479=DIRECTION('center_axis',(-0.313150259135957,-0.883174789320284,0.34919794774906));
#59480=DIRECTION('ref_axis',(-0.949703593340092,0.291213401820784,-0.115142691461001));
#59481=DIRECTION('center_axis',(-0.491310548314113,-0.814189528457783,0.309369288819978));
#59482=DIRECTION('ref_axis',(-0.870984468928858,0.459273291233481,-0.174511027858645));
#59483=DIRECTION('center_axis',(-0.284551435696759,-0.891015790469123,0.353724951873058));
#59484=DIRECTION('ref_axis',(-0.958660774436356,0.264472928451193,-0.104993283944912));
#59485=DIRECTION('center_axis',(0.0617712249622997,-0.925513751123792,0.373642358743525));
#59486=DIRECTION('ref_axis',(0.998090334472114,0.0572795028183562,-0.0231245062698635));
#59487=DIRECTION('center_axis',(0.99026806874157,-0.0695865504800329,-0.120527440954873));
#59488=DIRECTION('ref_axis',(0.139173100960066,0.495134034370784,0.857597304086755));
#59489=DIRECTION('',(1.,0.,0.));
#59490=DIRECTION('center_axis',(0.,0.927183854566787,-0.374606593415912));
#59491=DIRECTION('ref_axis',(1.,0.,0.));
#59492=DIRECTION('',(-0.137844537491629,-0.371030552991328,-0.918332843924613));
#59493=DIRECTION('center_axis',(-0.99026806874157,0.0695865504800329,0.120527440954873));
#59494=DIRECTION('ref_axis',(0.,0.866025403784438,-0.5));
#59495=DIRECTION('',(-0.137998583506848,-0.378681393832731,-0.9151812896443));
#59496=DIRECTION('center_axis',(-0.0617712249622997,0.925513751123792,-0.373642358743525));
#59497=DIRECTION('ref_axis',(0.998052578482889,0.0540211804549215,-0.0311891430775903));
#59498=DIRECTION('',(0.0161503784824051,-0.373381387356163,-0.927537333400043));
#59499=DIRECTION('center_axis',(0.284551435696759,0.891015790469123,-0.353724951873058));
#59500=DIRECTION('ref_axis',(0.957826285221151,-0.248850568624199,0.143673942783173));
#59501=DIRECTION('',(0.0552259184163645,-0.383601057879401,-0.921846151116809));
#59502=DIRECTION('center_axis',(0.491310548314113,0.814189528457783,-0.309369288819978));
#59503=DIRECTION('ref_axis',(0.86824314212446,-0.429668924423658,0.248069469178416));
#59504=DIRECTION('',(0.057078643955053,-0.384529194537799,-0.921346474976903));
#59505=DIRECTION('center_axis',(0.313150259135957,0.883174789320284,-0.34919794774906));
#59506=DIRECTION('ref_axis',(0.948683298050513,-0.273861278752584,0.15811388300842));
#59507=DIRECTION('',(0.0225789275220278,-0.37451109252948,-0.926947481578288));
#59508=DIRECTION('center_axis',(0.,0.927183854566787,-0.374606593415913));
#59509=DIRECTION('ref_axis',(1.,0.,0.));
#59510=DIRECTION('',(-0.0225789275220274,-0.37451109252948,-0.926947481578288));
#59511=DIRECTION('center_axis',(-0.313150259135956,0.883174789320284,-0.34919794774906));
#59512=DIRECTION('ref_axis',(0.948683298050514,0.273861278752584,-0.158113883008419));
#59513=DIRECTION('',(-0.0570786439550527,-0.384529194537799,-0.921346474976903));
#59514=DIRECTION('center_axis',(-0.491310548314114,0.814189528457782,-0.309369288819978));
#59515=DIRECTION('ref_axis',(0.86824314212446,0.429668924423659,-0.248069469178417));
#59516=DIRECTION('',(-0.0552259184163635,-0.3836010578794,-0.921846151116809));
#59517=DIRECTION('center_axis',(-0.284551435696759,0.891015790469123,-0.353724951873058));
#59518=DIRECTION('ref_axis',(0.957826285221151,0.248850568624199,-0.143673942783173));
#59519=DIRECTION('',(-0.0161503784824052,-0.373381387356163,-0.927537333400043));
#59520=DIRECTION('center_axis',(0.0617712249622996,0.925513751123792,-0.373642358743525));
#59521=DIRECTION('ref_axis',(0.998052578482889,-0.0540211804549214,0.0311891430775903));
#59522=DIRECTION('',(0.137998583506848,-0.378681393832731,-0.9151812896443));
#59523=DIRECTION('center_axis',(0.99026806874157,0.0695865504800327,0.120527440954873));
#59524=DIRECTION('ref_axis',(0.,-0.866025403784438,0.5));
#59525=DIRECTION('',(0.137844537491629,-0.371030552991328,-0.918332843924613));
#59526=DIRECTION('center_axis',(0.,0.927183854566787,-0.374606593415913));
#59527=DIRECTION('ref_axis',(1.,0.,0.));
#59528=DIRECTION('',(-0.051925424877728,-0.374101236076903,-0.925933051260727));
#59529=DIRECTION('center_axis',(-0.64930555798837,0.717100917309779,-0.253315153038432));
#59530=DIRECTION('ref_axis',(0.755033118392644,0.567841300538901,-0.327843327723122));
#59531=DIRECTION('center_axis',(0.,-0.788010753606722,0.615661475325659));
#59532=DIRECTION('ref_axis',(-1.,0.,0.));
#59533=DIRECTION('',(-1.,0.,0.));
#59534=DIRECTION('',(0.137844537491629,-0.609784295472662,-0.780488306432985));
#59535=DIRECTION('center_axis',(0.99026806874157,0.0695865504800328,0.120527440954873));
#59536=DIRECTION('ref_axis',(0.,-0.866025403784438,0.5));
#59537=DIRECTION('center_axis',(-0.99026806874157,-0.0695865504800328,-0.120527440954873));
#59538=DIRECTION('ref_axis',(-0.139173100960065,0.495134034370783,0.857597304086756));
#59539=DIRECTION('',(0.137998583506848,-0.603229548983803,-0.785538351821794));
#59540=DIRECTION('center_axis',(0.0617712249622996,-0.786340650163726,0.614697240653271));
#59541=DIRECTION('ref_axis',(-0.998052578482889,-0.0540211804549214,0.0311891430775903));
#59542=DIRECTION('center_axis',(-0.0617712249622996,0.786340650163726,-0.614697240653271));
#59543=DIRECTION('ref_axis',(0.998090334472114,0.0486661612888523,-0.0380432514219071));
#59544=DIRECTION('',(-0.0161503784824054,-0.616580200004833,-0.787126433450736));
#59545=DIRECTION('center_axis',(-0.284551435696759,-0.751842689509057,0.594779833782805));
#59546=DIRECTION('ref_axis',(-0.957826285221151,0.248850568624199,-0.143673942783173));
#59547=DIRECTION('center_axis',(0.284551435696759,0.751842689509057,-0.594779833782805));
#59548=DIRECTION('ref_axis',(-0.958660774436356,0.223163315348643,-0.176543632679542));
#59549=DIRECTION('',(-0.0552259184163638,-0.606541656308366,-0.793131336600549));
#59550=DIRECTION('center_axis',(-0.491310548314114,-0.675016427497717,0.550424170729724));
#59551=DIRECTION('ref_axis',(-0.86824314212446,0.429668924423659,-0.248069469178417));
#59552=DIRECTION('center_axis',(0.491310548314114,0.675016427497717,-0.550424170729724));
#59553=DIRECTION('ref_axis',(-0.870984468928858,0.380767628982861,-0.310486823558562));
#59554=DIRECTION('',(-0.0570786439550532,-0.605644855748342,-0.793685288454953));
#59555=DIRECTION('center_axis',(-0.313150259135956,-0.744001688360219,0.590252829658806));
#59556=DIRECTION('ref_axis',(-0.948683298050514,0.273861278752584,-0.158113883008419));
#59557=DIRECTION('center_axis',(0.313150259135956,0.744001688360219,-0.590252829658806));
#59558=DIRECTION('ref_axis',(-0.949703593340092,0.245323196775732,-0.194626858168784));
#59559=DIRECTION('',(-0.0225789275220273,-0.615504520756066,-0.787809860918737));
#59560=DIRECTION('center_axis',(0.,-0.788010753606722,0.615661475325659));
#59561=DIRECTION('ref_axis',(-1.,0.,0.));
#59562=DIRECTION('',(-1.,0.,0.));
#59563=DIRECTION('',(0.0225789275220281,-0.615504520756066,-0.787809860918737));
#59564=DIRECTION('center_axis',(0.313150259135957,-0.744001688360218,0.590252829658806));
#59565=DIRECTION('ref_axis',(-0.948683298050513,-0.273861278752584,0.15811388300842));
#59566=DIRECTION('center_axis',(-0.313150259135957,0.744001688360218,-0.590252829658806));
#59567=DIRECTION('ref_axis',(0.949703593340092,0.245323196775733,-0.194626858168784));
#59568=DIRECTION('',(0.0570786439550533,-0.605644855748343,-0.793685288454953));
#59569=DIRECTION('center_axis',(0.491310548314113,-0.675016427497717,0.550424170729725));
#59570=DIRECTION('ref_axis',(-0.86824314212446,-0.429668924423658,0.248069469178416));
#59571=DIRECTION('center_axis',(-0.491310548314113,0.675016427497717,-0.550424170729725));
#59572=DIRECTION('ref_axis',(0.870984468928858,0.38076762898286,-0.310486823558562));
#59573=DIRECTION('',(0.0552259184163649,-0.606541656308365,-0.793131336600549));
#59574=DIRECTION('center_axis',(0.284551435696759,-0.751842689509057,0.594779833782805));
#59575=DIRECTION('ref_axis',(-0.957826285221151,-0.248850568624199,0.143673942783173));
#59576=DIRECTION('center_axis',(-0.284551435696759,0.751842689509057,-0.594779833782805));
#59577=DIRECTION('ref_axis',(0.958660774436356,0.223163315348643,-0.176543632679541));
#59578=DIRECTION('',(0.0161503784824051,-0.616580200004833,-0.787126433450736));
#59579=DIRECTION('center_axis',(-0.0617712249622997,-0.786340650163726,
0.614697240653271));
#59580=DIRECTION('ref_axis',(-0.998052578482889,0.0540211804549215,-0.0311891430775903));
#59581=DIRECTION('center_axis',(0.0617712249622997,0.786340650163726,-0.614697240653271));
#59582=DIRECTION('ref_axis',(-0.998090334472114,0.0486661612888524,-0.0380432514219072));
#59583=DIRECTION('',(-0.137998583506848,-0.603229548983803,-0.785538351821794));
#59584=DIRECTION('center_axis',(-0.99026806874157,0.0695865504800329,0.120527440954873));
#59585=DIRECTION('ref_axis',(0.,0.866025403784438,-0.5));
#59586=DIRECTION('center_axis',(0.99026806874157,-0.0695865504800329,-0.120527440954873));
#59587=DIRECTION('ref_axis',(0.139173100960066,0.495134034370784,0.857597304086755));
#59588=DIRECTION('',(-0.137844537491629,-0.609784295472662,-0.780488306432985));
#59589=DIRECTION('center_axis',(0.,-0.788010753606722,0.615661475325659));
#59590=DIRECTION('ref_axis',(-1.,0.,0.));
#59591=DIRECTION('',(-1.,0.,0.));
#59592=DIRECTION('center_axis',(0.,-0.5,-0.866025403784438));
#59593=DIRECTION('ref_axis',(1.,0.,0.));
#59594=DIRECTION('center_axis',(1.,0.,0.));
#59595=DIRECTION('ref_axis',(0.,1.,0.));
#59596=DIRECTION('center_axis',(1.,0.,0.));
#59597=DIRECTION('ref_axis',(0.,0.,-1.));
#59598=DIRECTION('center_axis',(0.649305557988371,-0.662218828358294,0.373989994161849));
#59599=DIRECTION('ref_axis',(0.760527640763576,0.565373752130667,-0.319296457913771));
#59600=DIRECTION('',(1.,0.,0.));
#59601=DIRECTION('center_axis',(-0.99026806874157,-0.0894587448987839,-0.106612780622095));
#59602=DIRECTION('ref_axis',(-0.139173100960065,0.636532044855303,0.758589351257639));
#59603=DIRECTION('center_axis',(-0.0617712249622996,-0.846570802931135,
0.528679668032723));
#59604=DIRECTION('ref_axis',(-0.998090334472114,0.0523937700909925,-0.0327196743412163));
#59605=DIRECTION('center_axis',(0.284551435696759,-0.816055565222214,0.50307434332588));
#59606=DIRECTION('ref_axis',(0.958660774436356,0.242223097976277,-0.149323442110948));
#59607=DIRECTION('center_axis',(0.491310548314114,-0.748098746816874,0.446051802065978));
#59608=DIRECTION('ref_axis',(0.870984468928858,0.42199237598773,-0.25161178329511));
#59609=DIRECTION('center_axis',(0.313150259135956,-0.809119792515883,0.497254539006069));
#59610=DIRECTION('ref_axis',(0.949703593340092,0.266794897350299,-0.163962091791853));
#59611=DIRECTION('',(1.,0.,0.));
#59612=DIRECTION('center_axis',(-0.313150259135957,-0.809119792515883,0.497254539006068));
#59613=DIRECTION('ref_axis',(-0.949703593340092,0.2667948973503,-0.163962091791853));
#59614=DIRECTION('center_axis',(-0.491310548314113,-0.748098746816875,0.446051802065979));
#59615=DIRECTION('ref_axis',(-0.870984468928858,0.421992375987729,-0.25161178329511));
#59616=DIRECTION('center_axis',(-0.284551435696759,-0.816055565222214,0.503074343325881));
#59617=DIRECTION('ref_axis',(-0.958660774436356,0.242223097976277,-0.149323442110948));
#59618=DIRECTION('center_axis',(0.0617712249622997,-0.846570802931135,0.528679668032723));
#59619=DIRECTION('ref_axis',(0.998090334472114,0.0523937700909926,-0.0327196743412163));
#59620=DIRECTION('center_axis',(0.99026806874157,-0.0894587448987841,-0.106612780622095));
#59621=DIRECTION('ref_axis',(0.139173100960066,0.636532044855299,0.758589351257642));
#59622=DIRECTION('',(1.,0.,0.));
#59623=DIRECTION('center_axis',(0.,0.848048096156426,-0.529919264233205));
#59624=DIRECTION('ref_axis',(1.,0.,0.));
#59625=DIRECTION('',(-0.137844537491629,-0.524860590029465,-0.839952525157012));
#59626=DIRECTION('center_axis',(-0.99026806874157,0.0894587448987841,0.106612780622095));
#59627=DIRECTION('ref_axis',(0.,0.766044443118978,-0.642787609686539));
#59628=DIRECTION('',(-0.137998583506848,-0.531847935749547,-0.835520295497991));
#59629=DIRECTION('center_axis',(-0.0617712249622997,0.846570802931135,-0.528679668032723));
#59630=DIRECTION('ref_axis',(0.998052578482889,0.0477845394804615,-0.0400959894540315));
#59631=DIRECTION('',(0.0161503784824051,-0.528774052761765,-0.848608959651484));
#59632=DIRECTION('center_axis',(0.284551435696759,0.816055565222214,-0.503074343325881));
#59633=DIRECTION('ref_axis',(0.957826285221151,-0.220121250980087,0.184703660511672));
#59634=DIRECTION('',(0.0552259184163645,-0.537850200094026,-0.841229612052432));
#59635=DIRECTION('center_axis',(0.491310548314113,0.748098746816875,-0.446051802065979));
#59636=DIRECTION('ref_axis',(0.86824314212446,-0.3800644767432,0.318911962258805));
#59637=DIRECTION('',(0.057078643955053,-0.538677468419953,-0.840576357876501));
#59638=DIRECTION('center_axis',(0.313150259135957,0.809119792515883,-0.497254539006068));
#59639=DIRECTION('ref_axis',(0.948683298050513,-0.242244522917128,0.203267289834479));
#59640=DIRECTION('',(0.0225789275220278,-0.529784168481124,-0.847831897759644));
#59641=DIRECTION('center_axis',(0.,0.848048096156426,-0.529919264233205));
#59642=DIRECTION('ref_axis',(1.,0.,0.));
#59643=DIRECTION('',(-0.0225789275220274,-0.529784168481124,-0.847831897759644));
#59644=DIRECTION('center_axis',(-0.313150259135956,0.809119792515883,-0.497254539006069));
#59645=DIRECTION('ref_axis',(0.948683298050514,0.242244522917128,-0.203267289834478));
#59646=DIRECTION('',(-0.0570786439550527,-0.538677468419953,-0.840576357876501));
#59647=DIRECTION('center_axis',(-0.491310548314114,0.748098746816874,-0.446051802065978));
#59648=DIRECTION('ref_axis',(0.86824314212446,0.380064476743201,-0.318911962258806));
#59649=DIRECTION('',(-0.0552259184163635,-0.537850200094025,-0.841229612052432));
#59650=DIRECTION('center_axis',(-0.284551435696759,0.816055565222214,-0.50307434332588));
#59651=DIRECTION('ref_axis',(0.957826285221151,0.220121250980087,-0.184703660511673));
#59652=DIRECTION('',(-0.0161503784824052,-0.528774052761765,-0.848608959651484));
#59653=DIRECTION('center_axis',(0.0617712249622996,0.846570802931135,-0.528679668032723));
#59654=DIRECTION('ref_axis',(0.998052578482889,-0.0477845394804615,0.0400959894540314));
#59655=DIRECTION('',(0.137998583506848,-0.531847935749547,-0.835520295497991));
#59656=DIRECTION('center_axis',(0.99026806874157,0.0894587448987839,0.106612780622095));
#59657=DIRECTION('ref_axis',(0.,-0.766044443118978,0.642787609686539));
#59658=DIRECTION('',(0.137844537491629,-0.524860590029465,-0.839952525157012));
#59659=DIRECTION('center_axis',(0.,0.848048096156426,-0.529919264233205));
#59660=DIRECTION('ref_axis',(1.,0.,0.));
#59661=DIRECTION('',(-0.051925424877728,-0.52920438469299,-0.846904049744114));
#59662=DIRECTION('center_axis',(-0.649305557988371,0.662218828358294,-0.373989994161849));
#59663=DIRECTION('ref_axis',(0.755033118392644,0.502285118831862,-0.421467257957652));
#59664=DIRECTION('center_axis',(0.,-0.669130606358858,0.743144825477394));
#59665=DIRECTION('ref_axis',(-1.,0.,0.));
#59666=DIRECTION('',(-1.,0.,0.));
#59667=DIRECTION('',(0.137844537491629,-0.736050673949001,-0.662743003631831));
#59668=DIRECTION('center_axis',(0.99026806874157,0.0894587448987839,0.106612780622095));
#59669=DIRECTION('ref_axis',(0.,-0.766044443118978,0.642787609686539));
#59670=DIRECTION('center_axis',(-0.99026806874157,-0.0894587448987839,-0.106612780622095));
#59671=DIRECTION('ref_axis',(-0.139173100960065,0.636532044855303,0.758589351257639));
#59672=DIRECTION('',(0.137998583506848,-0.730472439966645,-0.668854547266653));
#59673=DIRECTION('center_axis',(0.0617712249622996,-0.667653313133567,0.741905229276912));
#59674=DIRECTION('ref_axis',(-0.998052578482889,-0.0477845394804615,0.0400959894540314));
#59675=DIRECTION('center_axis',(-0.0617712249622996,0.667653313133567,-0.741905229276912));
#59676=DIRECTION('ref_axis',(0.998090334472114,0.0413206716646654,-0.045916079171941));
#59677=DIRECTION('',(-0.0161503784824054,-0.743896032080768,-0.668100186146782));
#59678=DIRECTION('center_axis',(-0.284551435696759,-0.637138075424646,0.71629990457007));
#59679=DIRECTION('ref_axis',(-0.957826285221151,0.220121250980087,-0.184703660511673));
#59680=DIRECTION('center_axis',(0.284551435696759,0.637138075424646,-0.71629990457007));
#59681=DIRECTION('ref_axis',(-0.958660774436356,0.18911648304975,-0.212613441240154));
#59682=DIRECTION('',(-0.0552259184163638,-0.735052736908566,-0.675757036144127));
#59683=DIRECTION('center_axis',(-0.491310548314114,-0.569181257019306,0.659277363310168));
#59684=DIRECTION('ref_axis',(-0.86824314212446,0.380064476743201,-0.318911962258806));
#59685=DIRECTION('center_axis',(0.491310548314114,0.569181257019306,-0.659277363310168));
#59686=DIRECTION('ref_axis',(-0.870984468928858,0.32106744201786,-0.371889435936037));
#59687=DIRECTION('',(-0.0570786439550532,-0.734265753494182,-0.676458300008118));
#59688=DIRECTION('center_axis',(-0.313150259135956,-0.630202302718315,0.710480100250258));
#59689=DIRECTION('ref_axis',(-0.948683298050514,0.242244522917128,-0.203267289834478));
#59690=DIRECTION('center_axis',(0.313150259135956,0.630202302718315,-0.710480100250258));
#59691=DIRECTION('ref_axis',(-0.949703593340092,0.207799586932431,-0.234269964928557));
#59692=DIRECTION('',(-0.0225789275220273,-0.742955370751214,-0.668960020557194));
#59693=DIRECTION('center_axis',(0.,-0.669130606358858,0.743144825477394));
#59694=DIRECTION('ref_axis',(-1.,0.,0.));
#59695=DIRECTION('',(-1.,0.,0.));
#59696=DIRECTION('',(0.0225789275220281,-0.742955370751214,-0.668960020557194));
#59697=DIRECTION('center_axis',(0.313150259135957,-0.630202302718315,0.710480100250258));
#59698=DIRECTION('ref_axis',(-0.948683298050513,-0.242244522917128,0.203267289834479));
#59699=DIRECTION('center_axis',(-0.313150259135957,0.630202302718315,-0.710480100250258));
#59700=DIRECTION('ref_axis',(0.949703593340092,0.207799586932432,-0.234269964928558));
#59701=DIRECTION('',(0.0570786439550534,-0.734265753494183,-0.676458300008118));
#59702=DIRECTION('center_axis',(0.491310548314113,-0.569181257019307,0.659277363310168));
#59703=DIRECTION('ref_axis',(-0.86824314212446,-0.3800644767432,0.318911962258805));
#59704=DIRECTION('center_axis',(-0.491310548314113,0.569181257019307,-0.659277363310168));
#59705=DIRECTION('ref_axis',(0.870984468928858,0.321067442017859,-0.371889435936036));
#59706=DIRECTION('',(0.0552259184163649,-0.735052736908566,-0.675757036144127));
#59707=DIRECTION('center_axis',(0.284551435696759,-0.637138075424647,0.71629990457007));
#59708=DIRECTION('ref_axis',(-0.957826285221151,-0.220121250980087,0.184703660511672));
#59709=DIRECTION('center_axis',(-0.284551435696759,0.637138075424647,-0.71629990457007));
#59710=DIRECTION('ref_axis',(0.958660774436356,0.189116483049749,-0.212613441240154));
#59711=DIRECTION('',(0.0161503784824051,-0.743896032080768,-0.668100186146782));
#59712=DIRECTION('center_axis',(-0.0617712249622997,-0.667653313133567,
0.741905229276912));
#59713=DIRECTION('ref_axis',(-0.998052578482889,0.0477845394804615,-0.0400959894540315));
#59714=DIRECTION('center_axis',(0.0617712249622997,0.667653313133567,-0.741905229276912));
#59715=DIRECTION('ref_axis',(-0.998090334472114,0.0413206716646654,-0.045916079171941));
#59716=DIRECTION('',(-0.137998583506848,-0.730472439966645,-0.668854547266653));
#59717=DIRECTION('center_axis',(-0.99026806874157,0.0894587448987841,0.106612780622095));
#59718=DIRECTION('ref_axis',(0.,0.766044443118978,-0.642787609686539));
#59719=DIRECTION('center_axis',(0.99026806874157,-0.0894587448987841,-0.106612780622095));
#59720=DIRECTION('ref_axis',(0.139173100960066,0.636532044855299,0.758589351257642));
#59721=DIRECTION('',(-0.137844537491629,-0.736050673949,-0.662743003631831));
#59722=DIRECTION('center_axis',(0.,-0.669130606358858,0.743144825477394));
#59723=DIRECTION('ref_axis',(-1.,0.,0.));
#59724=DIRECTION('',(-1.,0.,0.));
#59725=DIRECTION('center_axis',(0.,-0.642787609686539,-0.766044443118978));
#59726=DIRECTION('ref_axis',(1.,0.,0.));
#59727=DIRECTION('center_axis',(1.,0.,0.));
#59728=DIRECTION('ref_axis',(0.,1.,0.));
#59729=DIRECTION('center_axis',(1.,0.,0.));
#59730=DIRECTION('ref_axis',(0.,0.,-1.));
#59731=DIRECTION('center_axis',(0.64930555798837,-0.587215555406038,0.483301338560726));
#59732=DIRECTION('ref_axis',(0.760527640763576,0.501339206395651,-0.412621749021023));
#59733=DIRECTION('',(1.,0.,0.));
#59734=DIRECTION('center_axis',(-0.99026806874157,-0.106612780622095,-0.0894587448987838));
#59735=DIRECTION('ref_axis',(-0.139173100960065,0.758589351257642,0.636532044855299));
#59736=DIRECTION('center_axis',(-0.0617712249622996,-0.741905229276912,
0.667653313133568));
#59737=DIRECTION('ref_axis',(-0.998090334472114,0.045916079171941,-0.0413206716646654));
#59738=DIRECTION('center_axis',(0.284551435696759,-0.71629990457007,0.637138075424647));
#59739=DIRECTION('ref_axis',(0.958660774436356,0.212613441240154,-0.18911648304975));
#59740=DIRECTION('center_axis',(0.491310548314114,-0.659277363310167,0.569181257019307));
#59741=DIRECTION('ref_axis',(0.870984468928858,0.371889435936037,-0.32106744201786));
#59742=DIRECTION('center_axis',(0.313150259135956,-0.710480100250258,0.630202302718316));
#59743=DIRECTION('ref_axis',(0.949703593340092,0.234269964928557,-0.207799586932431));
#59744=DIRECTION('',(1.,0.,0.));
#59745=DIRECTION('center_axis',(-0.313150259135957,-0.710480100250258,0.630202302718315));
#59746=DIRECTION('ref_axis',(-0.949703593340092,0.234269964928558,-0.207799586932432));
#59747=DIRECTION('center_axis',(-0.491310548314113,-0.659277363310168,0.569181257019307));
#59748=DIRECTION('ref_axis',(-0.870984468928858,0.371889435936036,-0.321067442017859));
#59749=DIRECTION('center_axis',(-0.284551435696759,-0.71629990457007,0.637138075424647));
#59750=DIRECTION('ref_axis',(-0.958660774436356,0.212613441240154,-0.189116483049749));
#59751=DIRECTION('center_axis',(0.0617712249622997,-0.741905229276912,0.667653313133568));
#59752=DIRECTION('ref_axis',(0.998090334472114,0.045916079171941,-0.0413206716646654));
#59753=DIRECTION('center_axis',(0.99026806874157,-0.106612780622095,-0.0894587448987841));
#59754=DIRECTION('ref_axis',(0.139173100960066,0.758589351257642,0.636532044855299));
#59755=DIRECTION('',(1.,0.,0.));
#59756=DIRECTION('center_axis',(0.,0.743144825477394,-0.669130606358858));
#59757=DIRECTION('ref_axis',(1.,0.,0.));
#59758=DIRECTION('',(-0.137844537491629,-0.662743003631831,-0.736050673949001));
#59759=DIRECTION('center_axis',(-0.99026806874157,0.106612780622095,0.0894587448987841));
#59760=DIRECTION('ref_axis',(0.,0.642787609686539,-0.766044443118978));
#59761=DIRECTION('',(-0.137998583506848,-0.668854547266653,-0.730472439966645));
#59762=DIRECTION('center_axis',(-0.0617712249622997,0.741905229276912,-0.667653313133568));
#59763=DIRECTION('ref_axis',(0.998052578482889,0.0400959894540315,-0.0477845394804616));
#59764=DIRECTION('',(0.0161503784824051,-0.668100186146782,-0.743896032080767));
#59765=DIRECTION('center_axis',(0.284551435696759,0.71629990457007,-0.637138075424647));
#59766=DIRECTION('ref_axis',(0.957826285221151,-0.184703660511672,0.220121250980087));
#59767=DIRECTION('',(0.0552259184163645,-0.675757036144128,-0.735052736908566));
#59768=DIRECTION('center_axis',(0.491310548314113,0.659277363310168,-0.569181257019307));
#59769=DIRECTION('ref_axis',(0.86824314212446,-0.318911962258805,0.3800644767432));
#59770=DIRECTION('',(0.057078643955053,-0.676458300008118,-0.734265753494182));
#59771=DIRECTION('center_axis',(0.313150259135957,0.710480100250258,-0.630202302718315));
#59772=DIRECTION('ref_axis',(0.948683298050513,-0.203267289834479,0.242244522917128));
#59773=DIRECTION('',(0.0225789275220278,-0.668960020557194,-0.742955370751214));
#59774=DIRECTION('center_axis',(0.,0.743144825477394,-0.669130606358858));
#59775=DIRECTION('ref_axis',(1.,0.,0.));
#59776=DIRECTION('',(-0.0225789275220274,-0.668960020557194,-0.742955370751214));
#59777=DIRECTION('center_axis',(-0.313150259135956,0.710480100250258,-0.630202302718316));
#59778=DIRECTION('ref_axis',(0.948683298050514,0.203267289834478,-0.242244522917128));
#59779=DIRECTION('',(-0.0570786439550527,-0.676458300008118,-0.734265753494182));
#59780=DIRECTION('center_axis',(-0.491310548314114,0.659277363310167,-0.569181257019307));
#59781=DIRECTION('ref_axis',(0.868243142124459,0.318911962258806,-0.380064476743201));
#59782=DIRECTION('',(-0.0552259184163635,-0.675757036144127,-0.735052736908566));
#59783=DIRECTION('center_axis',(-0.284551435696759,0.71629990457007,-0.637138075424647));
#59784=DIRECTION('ref_axis',(0.957826285221151,0.184703660511673,-0.220121250980087));
#59785=DIRECTION('',(-0.0161503784824052,-0.668100186146782,-0.743896032080767));
#59786=DIRECTION('center_axis',(0.0617712249622996,0.741905229276912,-0.667653313133568));
#59787=DIRECTION('ref_axis',(0.998052578482889,-0.0400959894540314,0.0477845394804615));
#59788=DIRECTION('',(0.137998583506848,-0.668854547266653,-0.730472439966645));
#59789=DIRECTION('center_axis',(0.99026806874157,0.106612780622095,0.0894587448987838));
#59790=DIRECTION('ref_axis',(0.,-0.642787609686539,0.766044443118978));
#59791=DIRECTION('',(0.137844537491629,-0.662743003631831,-0.736050673949001));
#59792=DIRECTION('center_axis',(0.,0.743144825477394,-0.669130606358858));
#59793=DIRECTION('ref_axis',(1.,0.,0.));
#59794=DIRECTION('',(-0.0519254248777279,-0.66822792587052,-0.742142297230154));
#59795=DIRECTION('center_axis',(-0.64930555798837,0.587215555406038,-0.483301338560726));
#59796=DIRECTION('ref_axis',(0.755033118392644,0.421467257957652,-0.502285118831862));
#59797=DIRECTION('center_axis',(0.,-0.529919264233205,0.848048096156426));
#59798=DIRECTION('ref_axis',(-1.,0.,0.));
#59799=DIRECTION('',(-1.,0.,0.));
#59800=DIRECTION('',(0.137844537491629,-0.839952525157012,-0.524860590029465));
#59801=DIRECTION('center_axis',(0.99026806874157,0.106612780622095,0.0894587448987839));
#59802=DIRECTION('ref_axis',(0.,-0.642787609686539,0.766044443118978));
#59803=DIRECTION('center_axis',(-0.99026806874157,-0.106612780622095,-0.0894587448987839));
#59804=DIRECTION('ref_axis',(-0.139173100960065,0.758589351257639,0.636532044855303));
#59805=DIRECTION('',(0.137998583506848,-0.835520295497991,-0.531847935749546));
#59806=DIRECTION('center_axis',(0.0617712249622996,-0.528679668032723,0.846570802931135));
#59807=DIRECTION('ref_axis',(-0.998052578482889,-0.0400959894540314,0.0477845394804615));
#59808=DIRECTION('center_axis',(-0.0617712249622996,0.528679668032723,-0.846570802931135));
#59809=DIRECTION('ref_axis',(0.998090334472114,0.0327196743412163,-0.0523937700909925));
#59810=DIRECTION('',(-0.0161503784824054,-0.848608959651484,-0.528774052761765));
#59811=DIRECTION('center_axis',(-0.284551435696759,-0.50307434332588,0.816055565222214));
#59812=DIRECTION('ref_axis',(-0.957826285221151,0.184703660511673,-0.220121250980087));
#59813=DIRECTION('center_axis',(0.284551435696759,0.50307434332588,-0.816055565222214));
#59814=DIRECTION('ref_axis',(-0.958660774436356,0.149323442110948,-0.242223097976277));
#59815=DIRECTION('',(-0.0552259184163638,-0.841229612052433,-0.537850200094025));
#59816=DIRECTION('center_axis',(-0.491310548314114,-0.446051802065978,0.748098746816874));
#59817=DIRECTION('ref_axis',(-0.868243142124459,0.318911962258806,-0.380064476743201));
#59818=DIRECTION('center_axis',(0.491310548314114,0.446051802065978,-0.748098746816874));
#59819=DIRECTION('ref_axis',(-0.870984468928858,0.25161178329511,-0.421992375987731));
#59820=DIRECTION('',(-0.0570786439550532,-0.840576357876501,-0.538677468419953));
#59821=DIRECTION('center_axis',(-0.313150259135956,-0.497254539006068,0.809119792515883));
#59822=DIRECTION('ref_axis',(-0.948683298050514,0.203267289834478,-0.242244522917128));
#59823=DIRECTION('center_axis',(0.313150259135956,0.497254539006068,-0.809119792515883));
#59824=DIRECTION('ref_axis',(-0.949703593340092,0.163962091791853,-0.266794897350299));
#59825=DIRECTION('',(-0.0225789275220273,-0.847831897759644,-0.529784168481124));
#59826=DIRECTION('center_axis',(0.,-0.529919264233205,0.848048096156426));
#59827=DIRECTION('ref_axis',(-1.,0.,0.));
#59828=DIRECTION('',(-1.,0.,0.));
#59829=DIRECTION('',(0.0225789275220281,-0.847831897759644,-0.529784168481124));
#59830=DIRECTION('center_axis',(0.313150259135957,-0.497254539006068,0.809119792515883));
#59831=DIRECTION('ref_axis',(-0.948683298050513,-0.203267289834479,0.242244522917128));
#59832=DIRECTION('center_axis',(-0.313150259135957,0.497254539006068,-0.809119792515883));
#59833=DIRECTION('ref_axis',(0.949703593340092,0.163962091791853,-0.2667948973503));
#59834=DIRECTION('',(0.0570786439550534,-0.840576357876501,-0.538677468419953));
#59835=DIRECTION('center_axis',(0.491310548314113,-0.446051802065978,0.748098746816875));
#59836=DIRECTION('ref_axis',(-0.86824314212446,-0.318911962258805,0.3800644767432));
#59837=DIRECTION('center_axis',(-0.491310548314113,0.446051802065978,-0.748098746816875));
#59838=DIRECTION('ref_axis',(0.870984468928858,0.25161178329511,-0.421992375987729));
#59839=DIRECTION('',(0.0552259184163649,-0.841229612052432,-0.537850200094026));
#59840=DIRECTION('center_axis',(0.284551435696759,-0.50307434332588,0.816055565222214));
#59841=DIRECTION('ref_axis',(-0.957826285221151,-0.184703660511672,0.220121250980087));
#59842=DIRECTION('center_axis',(-0.284551435696759,0.50307434332588,-0.816055565222214));
#59843=DIRECTION('ref_axis',(0.958660774436356,0.149323442110947,-0.242223097976277));
#59844=DIRECTION('',(0.0161503784824051,-0.848608959651484,-0.528774052761765));
#59845=DIRECTION('center_axis',(-0.0617712249622997,-0.528679668032723,
0.846570802931135));
#59846=DIRECTION('ref_axis',(-0.998052578482889,0.0400959894540315,-0.0477845394804616));
#59847=DIRECTION('center_axis',(0.0617712249622997,0.528679668032723,-0.846570802931135));
#59848=DIRECTION('ref_axis',(-0.998090334472114,0.0327196743412163,-0.0523937700909926));
#59849=DIRECTION('',(-0.137998583506848,-0.835520295497991,-0.531847935749546));
#59850=DIRECTION('center_axis',(-0.99026806874157,0.106612780622095,0.0894587448987841));
#59851=DIRECTION('ref_axis',(0.,0.642787609686539,-0.766044443118978));
#59852=DIRECTION('center_axis',(0.99026806874157,-0.106612780622095,-0.0894587448987841));
#59853=DIRECTION('ref_axis',(0.139173100960066,0.758589351257642,0.636532044855299));
#59854=DIRECTION('',(-0.137844537491629,-0.839952525157012,-0.524860590029465));
#59855=DIRECTION('center_axis',(0.,-0.529919264233205,0.848048096156426));
#59856=DIRECTION('ref_axis',(-1.,0.,0.));
#59857=DIRECTION('',(-1.,0.,0.));
#59858=DIRECTION('center_axis',(0.,-0.766044443118978,-0.642787609686539));
#59859=DIRECTION('ref_axis',(1.,0.,0.));
#59860=DIRECTION('center_axis',(1.,0.,0.));
#59861=DIRECTION('ref_axis',(0.,1.,0.));
#59862=DIRECTION('center_axis',(1.,0.,0.));
#59863=DIRECTION('ref_axis',(0.,0.,-1.));
#59864=DIRECTION('center_axis',(0.649305557988371,-0.494370034948177,0.577927816349714));
#59865=DIRECTION('ref_axis',(0.760527640763576,0.422071722564183,-0.49340973708095));
#59866=DIRECTION('',(1.,0.,0.));
#59867=DIRECTION('center_axis',(-0.99026806874157,-0.120527440954873,-0.0695865504800326));
#59868=DIRECTION('ref_axis',(-0.139173100960065,0.857597304086756,0.495134034370783));
#59869=DIRECTION('center_axis',(-0.0617712249622996,-0.61469724065327,0.786340650163727));
#59870=DIRECTION('ref_axis',(-0.998090334472114,0.0380432514219071,-0.0486661612888524));
#59871=DIRECTION('center_axis',(0.284551435696759,-0.594779833782804,0.751842689509058));
#59872=DIRECTION('ref_axis',(0.958660774436356,0.176543632679541,-0.223163315348643));
#59873=DIRECTION('center_axis',(0.491310548314114,-0.550424170729724,0.675016427497717));
#59874=DIRECTION('ref_axis',(0.870984468928858,0.310486823558562,-0.380767628982861));
#59875=DIRECTION('center_axis',(0.313150259135956,-0.590252829658806,0.744001688360219));
#59876=DIRECTION('ref_axis',(0.949703593340092,0.194626858168784,-0.245323196775732));
#59877=DIRECTION('',(1.,0.,0.));
#59878=DIRECTION('center_axis',(-0.313150259135957,-0.590252829658806,0.744001688360219));
#59879=DIRECTION('ref_axis',(-0.949703593340092,0.194626858168784,-0.245323196775733));
#59880=DIRECTION('center_axis',(-0.491310548314113,-0.550424170729724,0.675016427497718));
#59881=DIRECTION('ref_axis',(-0.870984468928858,0.310486823558561,-0.38076762898286));
#59882=DIRECTION('center_axis',(-0.284551435696759,-0.594779833782804,0.751842689509058));
#59883=DIRECTION('ref_axis',(-0.958660774436356,0.176543632679541,-0.223163315348643));
#59884=DIRECTION('center_axis',(0.0617712249622997,-0.61469724065327,0.786340650163727));
#59885=DIRECTION('ref_axis',(0.998090334472114,0.0380432514219071,-0.0486661612888524));
#59886=DIRECTION('center_axis',(0.99026806874157,-0.120527440954873,-0.0695865504800328));
#59887=DIRECTION('ref_axis',(0.139173100960066,0.857597304086755,0.495134034370784));
#59888=DIRECTION('',(1.,0.,0.));
#59889=DIRECTION('center_axis',(0.,0.615661475325658,-0.788010753606722));
#59890=DIRECTION('ref_axis',(1.,0.,0.));
#59891=DIRECTION('',(-0.137844537491629,-0.780488306432985,-0.609784295472661));
#59892=DIRECTION('center_axis',(-0.99026806874157,0.120527440954873,0.0695865504800328));
#59893=DIRECTION('ref_axis',(0.,0.5,-0.866025403784439));
#59894=DIRECTION('',(-0.137998583506848,-0.785538351821795,-0.603229548983802));
#59895=DIRECTION('center_axis',(-0.0617712249622997,0.61469724065327,-0.786340650163727));
#59896=DIRECTION('ref_axis',(0.998052578482889,0.0311891430775903,-0.0540211804549215));
#59897=DIRECTION('',(0.0161503784824051,-0.787126433450736,-0.616580200004832));
#59898=DIRECTION('center_axis',(0.284551435696759,0.594779833782804,-0.751842689509058));
#59899=DIRECTION('ref_axis',(0.957826285221151,-0.143673942783173,0.248850568624199));
#59900=DIRECTION('',(0.0552259184163645,-0.79313133660055,-0.606541656308365));
#59901=DIRECTION('center_axis',(0.491310548314113,0.550424170729724,-0.675016427497718));
#59902=DIRECTION('ref_axis',(0.86824314212446,-0.248069469178416,0.429668924423658));
#59903=DIRECTION('',(0.057078643955053,-0.793685288454953,-0.605644855748342));
#59904=DIRECTION('center_axis',(0.313150259135957,0.590252829658806,-0.744001688360219));
#59905=DIRECTION('ref_axis',(0.948683298050513,-0.15811388300842,0.273861278752585));
#59906=DIRECTION('',(0.0225789275220278,-0.787809860918738,-0.615504520756066));
#59907=DIRECTION('center_axis',(0.,0.615661475325658,-0.788010753606722));
#59908=DIRECTION('ref_axis',(1.,0.,0.));
#59909=DIRECTION('',(-0.0225789275220274,-0.787809860918738,-0.615504520756066));
#59910=DIRECTION('center_axis',(-0.313150259135956,0.590252829658806,-0.744001688360219));
#59911=DIRECTION('ref_axis',(0.948683298050513,0.158113883008419,-0.273861278752584));
#59912=DIRECTION('',(-0.0570786439550527,-0.793685288454953,-0.605644855748342));
#59913=DIRECTION('center_axis',(-0.491310548314114,0.550424170729724,-0.675016427497717));
#59914=DIRECTION('ref_axis',(0.868243142124459,0.248069469178416,-0.429668924423659));
#59915=DIRECTION('',(-0.0552259184163635,-0.79313133660055,-0.606541656308365));
#59916=DIRECTION('center_axis',(-0.284551435696759,0.594779833782804,-0.751842689509058));
#59917=DIRECTION('ref_axis',(0.957826285221151,0.143673942783173,-0.248850568624199));
#59918=DIRECTION('',(-0.0161503784824052,-0.787126433450736,-0.616580200004832));
#59919=DIRECTION('center_axis',(0.0617712249622996,0.61469724065327,-0.786340650163727));
#59920=DIRECTION('ref_axis',(0.998052578482889,-0.0311891430775902,0.0540211804549215));
#59921=DIRECTION('',(0.137998583506848,-0.785538351821795,-0.603229548983802));
#59922=DIRECTION('center_axis',(0.99026806874157,0.120527440954873,0.0695865504800326));
#59923=DIRECTION('ref_axis',(0.,-0.5,0.866025403784439));
#59924=DIRECTION('',(0.137844537491629,-0.780488306432985,-0.609784295472661));
#59925=DIRECTION('center_axis',(0.,0.615661475325658,-0.788010753606722));
#59926=DIRECTION('ref_axis',(1.,0.,0.));
#59927=DIRECTION('',(-0.0519254248777279,-0.786947699660121,-0.614830926556977));
#59928=DIRECTION('center_axis',(-0.649305557988371,0.494370034948177,-0.577927816349714));
#59929=DIRECTION('ref_axis',(0.755033118392644,0.327843327723121,-0.567841300538901));
#59930=DIRECTION('center_axis',(0.,-0.374606593415912,0.927183854566788));
#59931=DIRECTION('ref_axis',(-1.,0.,0.));
#59932=DIRECTION('',(-1.,0.,0.));
#59933=DIRECTION('',(0.137844537491629,-0.918332843924614,-0.371030552991327));
#59934=DIRECTION('center_axis',(0.99026806874157,0.120527440954873,0.0695865504800327));
#59935=DIRECTION('ref_axis',(0.,-0.5,0.866025403784439));
#59936=DIRECTION('center_axis',(-0.99026806874157,-0.120527440954873,-0.0695865504800327));
#59937=DIRECTION('ref_axis',(-0.139173100960065,0.857597304086756,0.495134034370783));
#59938=DIRECTION('',(0.137998583506848,-0.9151812896443,-0.378681393832731));
#59939=DIRECTION('center_axis',(0.0617712249622996,-0.373642358743524,0.925513751123792));
#59940=DIRECTION('ref_axis',(-0.998052578482889,-0.0311891430775902,0.0540211804549215));
#59941=DIRECTION('center_axis',(-0.0617712249622996,0.373642358743524,-0.925513751123792));
#59942=DIRECTION('ref_axis',(0.998090334472114,0.0231245062698634,-0.0572795028183562));
#59943=DIRECTION('',(-0.0161503784824054,-0.927537333400043,-0.373381387356162));
#59944=DIRECTION('center_axis',(-0.284551435696759,-0.353724951873057,0.891015790469123));
#59945=DIRECTION('ref_axis',(-0.957826285221151,0.143673942783173,-0.248850568624199));
#59946=DIRECTION('center_axis',(0.284551435696759,0.353724951873057,-0.891015790469123));
#59947=DIRECTION('ref_axis',(-0.958660774436356,0.104993283944912,-0.264472928451193));
#59948=DIRECTION('',(-0.0552259184163638,-0.921846151116809,-0.383601057879399));
#59949=DIRECTION('center_axis',(-0.491310548314114,-0.309369288819977,0.814189528457782));
#59950=DIRECTION('ref_axis',(-0.868243142124459,0.248069469178416,-0.429668924423659));
#59951=DIRECTION('center_axis',(0.491310548314114,0.309369288819977,-0.814189528457782));
#59952=DIRECTION('ref_axis',(-0.870984468928858,0.174511027858645,-0.459273291233482));
#59953=DIRECTION('',(-0.0570786439550532,-0.921346474976903,-0.384529194537798));
#59954=DIRECTION('center_axis',(-0.313150259135956,-0.349197947749059,0.883174789320284));
#59955=DIRECTION('ref_axis',(-0.948683298050513,0.158113883008419,-0.273861278752584));
#59956=DIRECTION('center_axis',(0.313150259135956,0.349197947749059,-0.883174789320284));
#59957=DIRECTION('ref_axis',(-0.949703593340092,0.115142691461001,-0.291213401820784));
#59958=DIRECTION('',(-0.0225789275220273,-0.926947481578288,-0.374511092529479));
#59959=DIRECTION('center_axis',(0.,-0.374606593415912,0.927183854566788));
#59960=DIRECTION('ref_axis',(-1.,0.,0.));
#59961=DIRECTION('',(-1.,0.,0.));
#59962=DIRECTION('',(0.0225789275220281,-0.926947481578288,-0.374511092529479));
#59963=DIRECTION('center_axis',(0.313150259135957,-0.349197947749059,0.883174789320284));
#59964=DIRECTION('ref_axis',(-0.948683298050513,-0.15811388300842,0.273861278752585));
#59965=DIRECTION('center_axis',(-0.313150259135957,0.349197947749059,-0.883174789320284));
#59966=DIRECTION('ref_axis',(0.949703593340092,0.115142691461001,-0.291213401820785));
#59967=DIRECTION('',(0.0570786439550533,-0.921346474976903,-0.384529194537798));
#59968=DIRECTION('center_axis',(0.491310548314113,-0.309369288819977,0.814189528457783));
#59969=DIRECTION('ref_axis',(-0.86824314212446,-0.248069469178416,0.429668924423658));
#59970=DIRECTION('center_axis',(-0.491310548314113,0.309369288819977,-0.814189528457783));
#59971=DIRECTION('ref_axis',(0.870984468928858,0.174511027858644,-0.459273291233481));
#59972=DIRECTION('',(0.0552259184163649,-0.921846151116809,-0.3836010578794));
#59973=DIRECTION('center_axis',(0.284551435696759,-0.353724951873058,0.891015790469123));
#59974=DIRECTION('ref_axis',(-0.957826285221151,-0.143673942783173,0.248850568624199));
#59975=DIRECTION('center_axis',(-0.284551435696759,0.353724951873058,-0.891015790469123));
#59976=DIRECTION('ref_axis',(0.958660774436356,0.104993283944912,-0.264472928451193));
#59977=DIRECTION('',(0.016150378482405,-0.927537333400043,-0.373381387356162));
#59978=DIRECTION('center_axis',(-0.0617712249622997,-0.373642358743524,
0.925513751123792));
#59979=DIRECTION('ref_axis',(-0.998052578482889,0.0311891430775903,-0.0540211804549215));
#59980=DIRECTION('center_axis',(0.0617712249622997,0.373642358743524,-0.925513751123792));
#59981=DIRECTION('ref_axis',(-0.998090334472114,0.0231245062698634,-0.0572795028183563));
#59982=DIRECTION('',(-0.137998583506848,-0.9151812896443,-0.378681393832731));
#59983=DIRECTION('center_axis',(-0.99026806874157,0.120527440954873,0.0695865504800328));
#59984=DIRECTION('ref_axis',(0.,0.5,-0.866025403784439));
#59985=DIRECTION('center_axis',(0.99026806874157,-0.120527440954873,-0.0695865504800328));
#59986=DIRECTION('ref_axis',(0.139173100960066,0.857597304086755,0.495134034370784));
#59987=DIRECTION('',(-0.137844537491629,-0.918332843924614,-0.371030552991327));
#59988=DIRECTION('center_axis',(0.,-0.374606593415912,0.927183854566788));
#59989=DIRECTION('ref_axis',(-1.,0.,0.));
#59990=DIRECTION('',(-1.,0.,0.));
#59991=DIRECTION('center_axis',(0.,-0.866025403784439,-0.5));
#59992=DIRECTION('ref_axis',(1.,0.,0.));
#59993=DIRECTION('center_axis',(1.,0.,0.));
#59994=DIRECTION('ref_axis',(0.,1.,0.));
#59995=DIRECTION('center_axis',(1.,0.,0.));
#59996=DIRECTION('ref_axis',(0.,0.,-1.));
#59997=DIRECTION('center_axis',(0.649305557988371,-0.386503331141725,0.654994249884502));
#59998=DIRECTION('ref_axis',(0.760527640763576,0.329979803021199,-0.559205719957048));
#59999=DIRECTION('',(1.,0.,0.));
#60000=DIRECTION('center_axis',(-0.99026806874157,-0.130779935984066,-0.0476000039374393));
#60001=DIRECTION('ref_axis',(-0.139173100960065,0.930547596796367,0.338691626801823));
#60002=DIRECTION('center_axis',(-0.0617712249622996,-0.468811987424191,
0.881135424446229));
#60003=DIRECTION('ref_axis',(-0.998090334472114,0.0290144987282327,-0.0545329542285434));
#60004=DIRECTION('center_axis',(0.284551435696759,-0.455187678719166,0.843702943923494));
#60005=DIRECTION('ref_axis',(0.958660774436356,0.135109635175349,-0.250429443236754));
#60006=DIRECTION('center_axis',(0.491310548314114,-0.424846618249727,0.760341565401402));
#60007=DIRECTION('ref_axis',(0.870984468928858,0.239650226161174,-0.428898384218936));
#60008=DIRECTION('center_axis',(0.313150259135956,-0.452091025520515,0.835194959184317));
#60009=DIRECTION('ref_axis',(0.949703593340092,0.149070112809494,-0.27539278542453));
#60010=DIRECTION('',(1.,0.,0.));
#60011=DIRECTION('center_axis',(-0.313150259135957,-0.452091025520515,0.835194959184317));
#60012=DIRECTION('ref_axis',(-0.949703593340092,0.149070112809494,-0.275392785424531));
#60013=DIRECTION('center_axis',(-0.491310548314113,-0.424846618249727,0.760341565401403));
#60014=DIRECTION('ref_axis',(-0.870984468928858,0.239650226161173,-0.428898384218935));
#60015=DIRECTION('center_axis',(-0.284551435696759,-0.455187678719166,0.843702943923494));
#60016=DIRECTION('ref_axis',(-0.958660774436356,0.135109635175349,-0.250429443236754));
#60017=DIRECTION('center_axis',(0.0617712249622997,-0.468811987424191,0.881135424446229));
#60018=DIRECTION('ref_axis',(0.998090334472114,0.0290144987282327,-0.0545329542285435));
#60019=DIRECTION('center_axis',(0.99026806874157,-0.130779935984066,-0.0476000039374394));
#60020=DIRECTION('ref_axis',(0.139173100960066,0.930547596796366,0.338691626801825));
#60021=DIRECTION('',(1.,0.,0.));
#60022=DIRECTION('center_axis',(0.,0.469471562785891,-0.882947592858927));
#60023=DIRECTION('ref_axis',(1.,0.,0.));
#60024=DIRECTION('',(-0.137844537491629,-0.874518866989312,-0.464989929744128));
#60025=DIRECTION('center_axis',(-0.99026806874157,0.130779935984066,0.0476000039374394));
#60026=DIRECTION('ref_axis',(0.,0.342020143325669,-0.939692620785909));
#60027=DIRECTION('',(-0.137998583506848,-0.878353971058417,-0.457657833403968));
#60028=DIRECTION('center_axis',(-0.0617712249622997,0.468811987424191,-0.881135424446229));
#60029=DIRECTION('ref_axis',(0.998052578482889,0.0213346303712044,-0.058616415197295));
#60030=DIRECTION('',(0.0161503784824051,-0.882236242379483,-0.470529890556386));
#60031=DIRECTION('center_axis',(0.284551435696759,0.455187678719166,-0.843702943923494));
#60032=DIRECTION('ref_axis',(0.957826285221151,-0.0982787650057293,0.270018687665128));
#60033=DIRECTION('',(0.0552259184163645,-0.886406742738186,-0.459601114406122));
#60034=DIRECTION('center_axis',(0.491310548314113,0.424846618249727,-0.760341565401403));
#60035=DIRECTION('ref_axis',(0.86824314212446,-0.169689510806249,0.46621809925847));
#60036=DIRECTION('',(0.057078643955053,-0.886796551036219,-0.458621745531673));
#60037=DIRECTION('center_axis',(0.313150259135957,0.452091025520515,-0.835194959184317));
#60038=DIRECTION('ref_axis',(0.948683298050513,-0.108156265856636,0.297156898213637));
#60039=DIRECTION('',(0.0225789275220278,-0.88272249730729,-0.469351877358061));
#60040=DIRECTION('center_axis',(0.,0.469471562785891,-0.882947592858927));
#60041=DIRECTION('ref_axis',(1.,0.,0.));
#60042=DIRECTION('',(-0.0225789275220274,-0.88272249730729,-0.46935187735806));
#60043=DIRECTION('center_axis',(-0.313150259135956,0.452091025520515,-0.835194959184317));
#60044=DIRECTION('ref_axis',(0.948683298050514,0.108156265856635,-0.297156898213636));
#60045=DIRECTION('',(-0.0570786439550527,-0.886796551036219,-0.458621745531673));
#60046=DIRECTION('center_axis',(-0.491310548314114,0.424846618249727,-0.760341565401402));
#60047=DIRECTION('ref_axis',(0.868243142124459,0.169689510806249,-0.466218099258471));
#60048=DIRECTION('',(-0.0552259184163635,-0.886406742738186,-0.459601114406122));
#60049=DIRECTION('center_axis',(-0.284551435696759,0.455187678719166,-0.843702943923494));
#60050=DIRECTION('ref_axis',(0.957826285221151,0.0982787650057295,-0.270018687665129));
#60051=DIRECTION('',(-0.0161503784824052,-0.882236242379483,-0.470529890556386));
#60052=DIRECTION('center_axis',(0.0617712249622996,0.468811987424191,-0.881135424446229));
#60053=DIRECTION('ref_axis',(0.998052578482889,-0.0213346303712044,0.0586164151972949));
#60054=DIRECTION('',(0.137998583506848,-0.878353971058417,-0.457657833403968));
#60055=DIRECTION('center_axis',(0.99026806874157,0.130779935984066,0.0476000039374393));
#60056=DIRECTION('ref_axis',(0.,-0.342020143325669,0.939692620785909));
#60057=DIRECTION('',(0.137844537491629,-0.874518866989312,-0.464989929744127));
#60058=DIRECTION('center_axis',(0.,0.469471562785891,-0.882947592858927));
#60059=DIRECTION('ref_axis',(1.,0.,0.));
#60060=DIRECTION('',(-0.0519254248777279,-0.881756465810299,-0.468838229299828));
#60061=DIRECTION('center_axis',(-0.649305557988371,0.386503331141725,-0.654994249884502));
#60062=DIRECTION('ref_axis',(0.755033118392644,0.224258043872452,-0.616143911670627));
#60063=DIRECTION('center_axis',(0.,-0.207911690817759,0.978147600733806));
#60064=DIRECTION('ref_axis',(-1.,0.,0.));
#60065=DIRECTION('',(-1.,0.,0.));
#60066=DIRECTION('',(0.137844537491629,-0.968810083928407,-0.205926940351068));
#60067=DIRECTION('center_axis',(0.99026806874157,0.130779935984066,0.0476000039374393));
#60068=DIRECTION('ref_axis',(0.,-0.342020143325669,0.939692620785909));
#60069=DIRECTION('center_axis',(-0.99026806874157,-0.130779935984066,-0.0476000039374393));
#60070=DIRECTION('ref_axis',(-0.139173100960065,0.930547596796367,0.338691626801823));
#60071=DIRECTION('',(0.137998583506848,-0.967034963408845,-0.214008809386339));
#60072=DIRECTION('center_axis',(0.0617712249622996,-0.20725211545606,0.976335432321108));
#60073=DIRECTION('ref_axis',(-0.998052578482889,-0.0213346303712044,0.0586164151972949));
#60074=DIRECTION('center_axis',(-0.0617712249622996,0.20725211545606,-0.976335432321108));
#60075=DIRECTION('ref_axis',(0.998090334472114,0.0128267117770656,-0.0604248268374111));
#60076=DIRECTION('',(-0.0161503784824054,-0.978282954629779,-0.206643717435842));
#60077=DIRECTION('center_axis',(-0.284551435696759,-0.193627806751035,0.938902951798373));
#60078=DIRECTION('ref_axis',(-0.957826285221151,0.0982787650057295,-0.270018687665129));
#60079=DIRECTION('center_axis',(0.284551435696759,0.193627806751035,-0.938902951798373));
#60080=DIRECTION('ref_axis',(-0.958660774436356,0.0574729579753754,-0.278686882824879));
#60081=DIRECTION('',(-0.0552259184163638,-0.974452861356161,-0.21769639163261));
#60082=DIRECTION('center_axis',(-0.491310548314114,-0.163286746281596,0.855541573276281));
#60083=DIRECTION('ref_axis',(-0.868243142124459,0.169689510806249,-0.466218099258471));
#60084=DIRECTION('center_axis',(0.491310548314114,0.163286746281596,-0.855541573276281));
#60085=DIRECTION('ref_axis',(-0.870984468928858,0.0921078431475352,-0.482599419928604));
#60086=DIRECTION('',(-0.0570786439550532,-0.974121945658943,-0.218697195660774));
#60087=DIRECTION('center_axis',(-0.313150259135956,-0.190531153552383,0.930394967059196));
#60088=DIRECTION('ref_axis',(-0.948683298050514,0.108156265856635,-0.297156898213636));
#60089=DIRECTION('center_axis',(0.313150259135956,0.190531153552383,-0.930394967059196));
#60090=DIRECTION('ref_axis',(-0.949703593340092,0.0628247387151195,-0.306783534438035));
#60091=DIRECTION('',(-0.0225789275220273,-0.977898235227234,-0.207858686543083));
#60092=DIRECTION('center_axis',(0.,-0.207911690817759,0.978147600733806));
#60093=DIRECTION('ref_axis',(-1.,0.,0.));
#60094=DIRECTION('',(-1.,0.,0.));
#60095=DIRECTION('',(0.0225789275220281,-0.977898235227234,-0.207858686543083));
#60096=DIRECTION('center_axis',(0.313150259135957,-0.190531153552383,0.930394967059195));
#60097=DIRECTION('ref_axis',(-0.948683298050513,-0.108156265856636,0.297156898213637));
#60098=DIRECTION('center_axis',(-0.313150259135957,0.190531153552383,-0.930394967059195));
#60099=DIRECTION('ref_axis',(0.949703593340092,0.0628247387151197,-0.306783534438037));
#60100=DIRECTION('',(0.0570786439550534,-0.974121945658943,-0.218697195660774));
#60101=DIRECTION('center_axis',(0.491310548314113,-0.163286746281596,0.855541573276282));
#60102=DIRECTION('ref_axis',(-0.86824314212446,-0.169689510806249,0.46621809925847));
#60103=DIRECTION('center_axis',(-0.491310548314113,0.163286746281596,-0.855541573276282));
#60104=DIRECTION('ref_axis',(0.870984468928858,0.0921078431475348,-0.482599419928602));
#60105=DIRECTION('',(0.0552259184163649,-0.974452861356161,-0.21769639163261));
#60106=DIRECTION('center_axis',(0.284551435696759,-0.193627806751035,0.938902951798373));
#60107=DIRECTION('ref_axis',(-0.957826285221151,-0.0982787650057293,0.270018687665128));
#60108=DIRECTION('center_axis',(-0.284551435696759,0.193627806751035,-0.938902951798373));
#60109=DIRECTION('ref_axis',(0.958660774436356,0.0574729579753754,-0.278686882824878));
#60110=DIRECTION('',(0.0161503784824051,-0.978282954629779,-0.206643717435842));
#60111=DIRECTION('center_axis',(-0.0617712249622997,-0.20725211545606,0.976335432321108));
#60112=DIRECTION('ref_axis',(-0.998052578482889,0.0213346303712044,-0.058616415197295));
#60113=DIRECTION('center_axis',(0.0617712249622997,0.20725211545606,-0.976335432321108));
#60114=DIRECTION('ref_axis',(-0.998090334472114,0.0128267117770656,-0.0604248268374111));
#60115=DIRECTION('',(-0.137998583506848,-0.967034963408845,-0.214008809386339));
#60116=DIRECTION('center_axis',(-0.99026806874157,0.130779935984066,0.0476000039374394));
#60117=DIRECTION('ref_axis',(0.,0.342020143325669,-0.939692620785909));
#60118=DIRECTION('center_axis',(0.99026806874157,-0.130779935984066,-0.0476000039374394));
#60119=DIRECTION('ref_axis',(0.139173100960066,0.930547596796366,0.338691626801825));
#60120=DIRECTION('',(-0.137844537491629,-0.968810083928407,-0.205926940351068));
#60121=DIRECTION('center_axis',(0.,-0.207911690817759,0.978147600733806));
#60122=DIRECTION('ref_axis',(-1.,0.,0.));
#60123=DIRECTION('',(-1.,0.,0.));
#60124=DIRECTION('center_axis',(0.,-0.939692620785908,-0.342020143325669));
#60125=DIRECTION('ref_axis',(1.,0.,0.));
#60126=DIRECTION('center_axis',(1.,0.,0.));
#60127=DIRECTION('ref_axis',(0.,1.,0.));
#60128=DIRECTION('center_axis',(1.,0.,0.));
#60129=DIRECTION('ref_axis',(0.,0.,-1.));
#60130=DIRECTION('center_axis',(0.649305557988371,-0.266892919198654,0.712159014579632));
#60131=DIRECTION('ref_axis',(0.760527640763576,0.227861614141252,-0.608010520003998));
#60132=DIRECTION('',(1.,0.,0.));
#60133=DIRECTION('center_axis',(-0.99026806874157,-0.137058748836223,-0.024167155361971));
#60134=DIRECTION('ref_axis',(-0.139173100960065,0.975223671657125,0.171958245538723));
#60135=DIRECTION('center_axis',(-0.0617712249622996,-0.30868211918754,0.949157344732972));
#60136=DIRECTION('ref_axis',(-0.998090334472114,0.0191041551727457,-0.0587427909490065));
#60137=DIRECTION('center_axis',(0.284551435696759,-0.301764876373726,0.909927711321105));
#60138=DIRECTION('ref_axis',(0.958660774436356,0.0895703997751285,-0.27008639921553));
#60139=DIRECTION('center_axis',(0.491310548314114,-0.286360316256974,0.822564109591763));
#60140=DIRECTION('ref_axis',(0.870984468928858,0.161531977910744,-0.463997279083573));
#60141=DIRECTION('center_axis',(0.313150259135956,-0.30019266434088,0.901011253802641));
#60142=DIRECTION('ref_axis',(0.949703593340092,0.0989839475056044,-0.297094703643677));
#60143=DIRECTION('',(1.,0.,0.));
#60144=DIRECTION('center_axis',(-0.313150259135957,-0.30019266434088,0.901011253802641));
#60145=DIRECTION('ref_axis',(-0.949703593340092,0.0989839475056048,-0.297094703643678));
#60146=DIRECTION('center_axis',(-0.491310548314113,-0.286360316256974,0.822564109591764));
#60147=DIRECTION('ref_axis',(-0.870984468928858,0.161531977910743,-0.463997279083571));
#60148=DIRECTION('center_axis',(-0.284551435696759,-0.301764876373726,0.909927711321105));
#60149=DIRECTION('ref_axis',(-0.958660774436356,0.0895703997751283,-0.270086399215529));
#60150=DIRECTION('center_axis',(0.0617712249622997,-0.30868211918754,0.949157344732972));
#60151=DIRECTION('ref_axis',(0.998090334472114,0.0191041551727457,-0.0587427909490066));
#60152=DIRECTION('center_axis',(0.99026806874157,-0.137058748836224,-0.0241671553619711));
#60153=DIRECTION('ref_axis',(0.139173100960066,0.975223671657125,0.171958245538724));
#60154=DIRECTION('',(1.,0.,0.));
#60155=DIRECTION('center_axis',(0.,0.309016994374947,-0.951056516295154));
#60156=DIRECTION('ref_axis',(1.,0.,0.));
#60157=DIRECTION('',(-0.137844537491629,-0.941977614300068,-0.306067080296576));
#60158=DIRECTION('center_axis',(-0.99026806874157,0.137058748836224,0.0241671553619711));
#60159=DIRECTION('ref_axis',(0.,0.17364817766693,-0.984807753012208));
#60160=DIRECTION('',(-0.137998583506848,-0.944481249352984,-0.298180416142191));
#60161=DIRECTION('center_axis',(-0.0617712249622997,0.30868211918754,-0.949157344732972));
#60162=DIRECTION('ref_axis',(0.998052578482889,0.0108318757168334,-0.0614306198252359));
#60163=DIRECTION('',(0.0161503784824051,-0.950539749516609,-0.310182768482997));
#60164=DIRECTION('center_axis',(0.284551435696759,0.301764876373726,-0.909927711321105));
#60165=DIRECTION('ref_axis',(0.957826285221151,-0.0498974366850414,0.282982425517402));
#60166=DIRECTION('',(0.0552259184163645,-0.952749128541176,-0.298695825212034));
#60167=DIRECTION('center_axis',(0.491310548314113,0.286360316256974,-0.822564109591764));
#60168=DIRECTION('ref_axis',(0.86824314212446,-0.0861536225152693,0.488601473065054));
#60169=DIRECTION('',(0.057078643955053,-0.952962949154956,-0.297663645650825));
#60170=DIRECTION('center_axis',(0.313150259135957,0.30019266434088,-0.901011253802641));
#60171=DIRECTION('ref_axis',(0.948683298050513,-0.0549123752965086,0.311423555691114));
#60172=DIRECTION('',(0.0225789275220278,-0.950814057294297,-0.30893821467004));
#60173=DIRECTION('center_axis',(0.,0.309016994374947,-0.951056516295154));
#60174=DIRECTION('ref_axis',(1.,0.,0.));
#60175=DIRECTION('',(-0.0225789275220274,-0.950814057294297,-0.30893821467004));
#60176=DIRECTION('center_axis',(-0.313150259135956,0.30019266434088,-0.901011253802641));
#60177=DIRECTION('ref_axis',(0.948683298050514,0.0549123752965084,-0.311423555691113));
#60178=DIRECTION('',(-0.0570786439550527,-0.952962949154956,-0.297663645650825));
#60179=DIRECTION('center_axis',(-0.491310548314114,0.286360316256974,-0.822564109591763));
#60180=DIRECTION('ref_axis',(0.868243142124459,0.0861536225152694,-0.488601473065055));
#60181=DIRECTION('',(-0.0552259184163635,-0.952749128541176,-0.298695825212034));
#60182=DIRECTION('center_axis',(-0.284551435696759,0.301764876373726,-0.909927711321105));
#60183=DIRECTION('ref_axis',(0.957826285221151,0.0498974366850415,-0.282982425517402));
#60184=DIRECTION('',(-0.0161503784824052,-0.950539749516609,-0.310182768482997));
#60185=DIRECTION('center_axis',(0.0617712249622996,0.30868211918754,-0.949157344732972));
#60186=DIRECTION('ref_axis',(0.998052578482889,-0.0108318757168334,0.0614306198252359));
#60187=DIRECTION('',(0.137998583506848,-0.944481249352984,-0.298180416142191));
#60188=DIRECTION('center_axis',(0.99026806874157,0.137058748836223,0.024167155361971));
#60189=DIRECTION('ref_axis',(0.,-0.17364817766693,0.984807753012208));
#60190=DIRECTION('',(0.137844537491629,-0.941977614300068,-0.306067080296576));
#60191=DIRECTION('center_axis',(0.,0.309016994374947,-0.951056516295154));
#60192=DIRECTION('ref_axis',(1.,0.,0.));
#60193=DIRECTION('',(-0.051925424877728,-0.949773507937132,-0.308600119688995));
#60194=DIRECTION('center_axis',(-0.649305557988371,0.266892919198654,-0.712159014579632));
#60195=DIRECTION('ref_axis',(0.755033118392644,0.113858792838764,-0.645725301830105));
#60196=DIRECTION('center_axis',(0.,-0.0348994967025007,0.999390827019096));
#60197=DIRECTION('ref_axis',(-1.,0.,0.));
#60198=DIRECTION('',(-1.,0.,0.));
#60199=DIRECTION('',(0.137844537491629,-0.989850519773593,-0.0345663418323));
#60200=DIRECTION('center_axis',(0.99026806874157,0.137058748836223,0.024167155361971));
#60201=DIRECTION('ref_axis',(0.,-0.17364817766693,0.984807753012208));
#60202=DIRECTION('center_axis',(-0.99026806874157,-0.137058748836223,-0.024167155361971));
#60203=DIRECTION('ref_axis',(-0.139173100960065,0.975223671657125,0.171958245538723));
#60204=DIRECTION('',(0.137998583506848,-0.989505769153514,-0.0428336755604255));
#60205=DIRECTION('center_axis',(0.0617712249622996,-0.0345646215150938,
0.997491655456914));
#60206=DIRECTION('ref_axis',(-0.998052578482889,-0.0108318757168334,0.0614306198252359));
#60207=DIRECTION('center_axis',(-0.0617712249622996,0.0345646215150938,
-0.997491655456914));
#60208=DIRECTION('ref_axis',(0.998090334472114,0.00213918413755088,-0.061734173069449));
#60209=DIRECTION('',(-0.0161503784824054,-0.999303943318151,-0.0336272827279993));
#60210=DIRECTION('center_axis',(-0.284551435696759,-0.0276473787012792,
0.958262022045047));
#60211=DIRECTION('ref_axis',(-0.957826285221151,0.0498974366850415,-0.282982425517402));
#60212=DIRECTION('center_axis',(0.284551435696759,0.0276473787012792,-0.958262022045047));
#60213=DIRECTION('ref_axis',(-0.958660774436356,0.00820634526047697,-0.284433077286297));
#60214=DIRECTION('',(-0.0552259184163638,-0.997451314500147,-0.0451771306857527));
#60215=DIRECTION('center_axis',(-0.491310548314114,-0.0122428185845277,
0.870898420315705));
#60216=DIRECTION('ref_axis',(-0.868243142124459,0.0861536225152694,-0.488601473065055));
#60217=DIRECTION('center_axis',(0.491310548314114,0.0122428185845277,-0.870898420315705));
#60218=DIRECTION('ref_axis',(-0.870984468928858,0.00690600823120518,-0.491262009456284));
#60219=DIRECTION('',(-0.0570786439550532,-0.997299213951626,-0.0462201931597179));
#60220=DIRECTION('center_axis',(-0.313150259135956,-0.0260751666684334,
0.949345564526583));
#60221=DIRECTION('ref_axis',(-0.948683298050514,0.0549123752965084,-0.311423555691113));
#60222=DIRECTION('center_axis',(0.313150259135956,0.0260751666684334,-0.949345564526583));
#60223=DIRECTION('ref_axis',(-0.949703593340092,0.00859788807423102,-0.313032204601347));
#60224=DIRECTION('',(-0.0225789275220273,-0.999136045839184,-0.0348905995476462));
#60225=DIRECTION('center_axis',(0.,-0.0348994967025007,0.999390827019096));
#60226=DIRECTION('ref_axis',(-1.,0.,0.));
#60227=DIRECTION('',(-1.,0.,0.));
#60228=DIRECTION('',(0.0225789275220281,-0.999136045839184,-0.0348905995476462));
#60229=DIRECTION('center_axis',(0.313150259135957,-0.0260751666684331,0.949345564526583));
#60230=DIRECTION('ref_axis',(-0.948683298050513,-0.0549123752965086,0.311423555691114));
#60231=DIRECTION('center_axis',(-0.313150259135957,0.0260751666684331,-0.949345564526583));
#60232=DIRECTION('ref_axis',(0.949703593340092,0.00859788807423098,-0.313032204601348));
#60233=DIRECTION('',(0.0570786439550534,-0.997299213951626,-0.0462201931597178));
#60234=DIRECTION('center_axis',(0.491310548314113,-0.0122428185845276,0.870898420315706));
#60235=DIRECTION('ref_axis',(-0.86824314212446,-0.0861536225152693,0.488601473065054));
#60236=DIRECTION('center_axis',(-0.491310548314113,0.0122428185845276,-0.870898420315706));
#60237=DIRECTION('ref_axis',(0.870984468928858,0.00690600823120505,-0.491262009456283));
#60238=DIRECTION('',(0.0552259184163649,-0.997451314500147,-0.0451771306857531));
#60239=DIRECTION('center_axis',(0.284551435696759,-0.0276473787012793,0.958262022045047));
#60240=DIRECTION('ref_axis',(-0.957826285221151,-0.0498974366850414,0.282982425517402));
#60241=DIRECTION('center_axis',(-0.284551435696759,0.0276473787012793,-0.958262022045047));
#60242=DIRECTION('ref_axis',(0.958660774436356,0.00820634526047701,-0.284433077286297));
#60243=DIRECTION('',(0.0161503784824051,-0.999303943318151,-0.0336272827279993));
#60244=DIRECTION('center_axis',(-0.0617712249622997,-0.0345646215150938,
0.997491655456914));
#60245=DIRECTION('ref_axis',(-0.998052578482889,0.0108318757168334,-0.0614306198252359));
#60246=DIRECTION('center_axis',(0.0617712249622997,0.0345646215150938,-0.997491655456914));
#60247=DIRECTION('ref_axis',(-0.998090334472114,0.00213918413755088,-0.061734173069449));
#60248=DIRECTION('',(-0.137998583506848,-0.989505769153514,-0.0428336755604255));
#60249=DIRECTION('center_axis',(-0.99026806874157,0.137058748836224,0.0241671553619711));
#60250=DIRECTION('ref_axis',(0.,0.17364817766693,-0.984807753012208));
#60251=DIRECTION('center_axis',(0.99026806874157,-0.137058748836224,-0.0241671553619711));
#60252=DIRECTION('ref_axis',(0.139173100960066,0.975223671657125,0.171958245538724));
#60253=DIRECTION('',(-0.137844537491629,-0.989850519773593,-0.0345663418323));
#60254=DIRECTION('center_axis',(0.,-0.0348994967025007,0.999390827019096));
#60255=DIRECTION('ref_axis',(-1.,0.,0.));
#60256=DIRECTION('',(-1.,0.,0.));
#60257=DIRECTION('center_axis',(0.,-0.984807753012208,-0.17364817766693));
#60258=DIRECTION('ref_axis',(1.,0.,0.));
#60259=DIRECTION('center_axis',(1.,0.,0.));
#60260=DIRECTION('ref_axis',(0.,1.,0.));
#60261=DIRECTION('center_axis',(1.,0.,0.));
#60262=DIRECTION('ref_axis',(0.,0.,-1.));
#60263=DIRECTION('center_axis',(0.649305557988371,-0.139173100960065,0.747685187986609));
#60264=DIRECTION('ref_axis',(0.760527640763576,0.118819965419165,-0.638341228068795));
#60265=DIRECTION('',(1.,0.,0.));
#60266=DIRECTION('center_axis',(-0.99026806874157,-0.139173100960065,1.70437892618156E-17));
#60267=DIRECTION('ref_axis',(-0.139173100960065,0.99026806874157,0.));
#60268=DIRECTION('center_axis',(-0.0617712249622996,-0.139173100960065,
0.988339599396795));
#60269=DIRECTION('ref_axis',(-0.998090334472114,0.00861334152950385,-0.0611677576917705));
#60270=DIRECTION('center_axis',(0.284551435696759,-0.139173100960065,0.948504785655862));
#60271=DIRECTION('ref_axis',(0.958660774436356,0.0413096131025498,-0.281536916624453));
#60272=DIRECTION('center_axis',(0.491310548314114,-0.139173100960065,0.859793459549701));
#60273=DIRECTION('ref_axis',(0.870984468928858,0.0785056622506208,-0.484997851417207));
#60274=DIRECTION('center_axis',(0.313150259135956,-0.139173100960065,0.939450777407866));
#60275=DIRECTION('ref_axis',(0.949703593340092,0.0458902050450515,-0.309769549629784));
#60276=DIRECTION('',(1.,0.,0.));
#60277=DIRECTION('center_axis',(-0.313150259135957,-0.139173100960065,0.939450777407865));
#60278=DIRECTION('ref_axis',(-0.949703593340092,0.0458902050450517,-0.309769549629785));
#60279=DIRECTION('center_axis',(-0.491310548314113,-0.139173100960065,0.859793459549702));
#60280=DIRECTION('ref_axis',(-0.870984468928858,0.0785056622506207,-0.484997851417206));
#60281=DIRECTION('center_axis',(-0.284551435696759,-0.139173100960065,0.948504785655862));
#60282=DIRECTION('ref_axis',(-0.958660774436356,0.0413096131025497,-0.281536916624453));
#60283=DIRECTION('center_axis',(0.0617712249622997,-0.139173100960065,0.988339599396795));
#60284=DIRECTION('ref_axis',(0.998090334472114,0.00861334152950384,-0.0611677576917706));
#60285=DIRECTION('center_axis',(0.99026806874157,-0.139173100960066,1.70437892618156E-17));
#60286=DIRECTION('ref_axis',(0.139173100960066,0.99026806874157,0.));
#60287=DIRECTION('',(1.,0.,0.));
#60288=DIRECTION('center_axis',(0.,0.139173100960066,-0.99026806874157));
#60289=DIRECTION('ref_axis',(1.,0.,0.));
#60290=DIRECTION('',(-0.137844537491629,-0.980814848463989,-0.137844537491629));
#60291=DIRECTION('center_axis',(-0.99026806874157,0.139173100960066,-1.70437892618156E-17));
#60292=DIRECTION('ref_axis',(0.,-1.22464679914735E-16,-1.));
#60293=DIRECTION('',(-0.137998583506848,-0.981910942816533,-0.129642937822505));
#60294=DIRECTION('center_axis',(-0.0617712249622997,0.139173100960065,-0.988339599396795));
#60295=DIRECTION('ref_axis',(0.998052578482889,-7.63913684762395E-18,-0.0623782861551806));
#60296=DIRECTION('',(0.0161503784824051,-0.989961587360995,-0.140410899949307));
#60297=DIRECTION('center_axis',(0.284551435696759,0.139173100960065,-0.948504785655862));
#60298=DIRECTION('ref_axis',(0.957826285221151,3.51899668300585E-17,0.287347885566345));
#60299=DIRECTION('',(0.0552259184163645,-0.990142714187765,-0.128714814516259));
#60300=DIRECTION('center_axis',(0.491310548314113,0.139173100960065,-0.859793459549702));
#60301=DIRECTION('ref_axis',(0.86824314212446,6.0759496279106E-17,0.496138938356832));
#60302=DIRECTION('',(0.057078643955053,-0.99017405028614,-0.12766118652195));
#60303=DIRECTION('center_axis',(0.313150259135957,0.139173100960065,-0.939450777407865));
#60304=DIRECTION('ref_axis',(0.948683298050513,3.87267321454041E-17,0.31622776601684));
#60305=DIRECTION('',(0.0225789275220278,-0.990015613285545,-0.13913762065955));
#60306=DIRECTION('center_axis',(0.,0.139173100960065,-0.99026806874157));
#60307=DIRECTION('ref_axis',(1.,0.,0.));
#60308=DIRECTION('',(-0.0225789275220274,-0.990015613285545,-0.13913762065955));
#60309=DIRECTION('center_axis',(-0.313150259135956,0.139173100960065,-0.939450777407866));
#60310=DIRECTION('ref_axis',(0.948683298050514,-3.8726732145404E-17,-0.316227766016839));
#60311=DIRECTION('',(-0.0570786439550527,-0.99017405028614,-0.12766118652195));
#60312=DIRECTION('center_axis',(-0.491310548314114,0.139173100960065,-0.859793459549701));
#60313=DIRECTION('ref_axis',(0.868243142124459,-6.07594962791062E-17,-0.496138938356833));
#60314=DIRECTION('',(-0.0552259184163635,-0.990142714187765,-0.128714814516259));
#60315=DIRECTION('center_axis',(-0.284551435696759,0.139173100960065,-0.948504785655862));
#60316=DIRECTION('ref_axis',(0.957826285221151,-3.51899668300585E-17,-0.287347885566346));
#60317=DIRECTION('',(-0.0161503784824052,-0.989961587360995,-0.140410899949307));
#60318=DIRECTION('center_axis',(0.0617712249622996,0.139173100960065,-0.988339599396795));
#60319=DIRECTION('ref_axis',(0.998052578482889,7.63913684762395E-18,0.0623782861551805));
#60320=DIRECTION('',(0.137998583506848,-0.981910942816534,-0.129642937822505));
#60321=DIRECTION('center_axis',(0.99026806874157,0.139173100960065,-1.70437892618156E-17));
#60322=DIRECTION('ref_axis',(0.,1.22464679914735E-16,1.));
#60323=DIRECTION('',(0.137844537491629,-0.980814848463989,-0.137844537491628));
#60324=DIRECTION('center_axis',(0.,0.139173100960065,-0.99026806874157));
#60325=DIRECTION('ref_axis',(1.,0.,0.));
#60326=DIRECTION('',(-0.051925424877728,-0.98893216263388,-0.138985351600607));
#60327=DIRECTION('center_axis',(-0.649305557988371,0.139173100960065,-0.747685187986609));
#60328=DIRECTION('ref_axis',(0.755033118392644,-8.02984563835875E-17,-0.655686655446243));
#60329=DIRECTION('center_axis',(0.,0.139173100960066,0.99026806874157));
#60330=DIRECTION('ref_axis',(-1.,0.,0.));
#60331=DIRECTION('',(-1.,0.,0.));
#60332=DIRECTION('',(0.137844537491629,-0.980814848463989,0.137844537491629));
#60333=DIRECTION('center_axis',(0.99026806874157,0.139173100960065,-1.70437892618156E-17));
#60334=DIRECTION('ref_axis',(0.,1.22464679914735E-16,1.));
#60335=DIRECTION('center_axis',(-0.99026806874157,-0.139173100960065,1.70437892618156E-17));
#60336=DIRECTION('ref_axis',(-0.139173100960065,0.99026806874157,0.));
#60337=DIRECTION('',(0.137998583506848,-0.981910942816534,0.129642937822505));
#60338=DIRECTION('center_axis',(0.0617712249622996,0.139173100960066,0.988339599396795));
#60339=DIRECTION('ref_axis',(-0.998052578482889,7.63913684762395E-18,0.0623782861551805));
#60340=DIRECTION('center_axis',(-0.0617712249622996,-0.139173100960066,
-0.988339599396795));
#60341=DIRECTION('ref_axis',(-0.998090334472114,0.00861334152950386,0.0611677576917705));
#60342=DIRECTION('',(-0.0161503784824054,-0.989961587360995,0.140410899949307));
#60343=DIRECTION('center_axis',(-0.284551435696759,0.139173100960066,0.948504785655862));
#60344=DIRECTION('ref_axis',(-0.957826285221151,-3.51899668300585E-17,-0.287347885566346));
#60345=DIRECTION('center_axis',(0.284551435696759,-0.139173100960066,-0.948504785655862));
#60346=DIRECTION('ref_axis',(0.958660774436356,0.0413096131025499,0.281536916624453));
#60347=DIRECTION('',(-0.0552259184163638,-0.990142714187765,0.12871481451626));
#60348=DIRECTION('center_axis',(-0.491310548314114,0.139173100960066,0.859793459549701));
#60349=DIRECTION('ref_axis',(-0.868243142124459,-6.07594962791062E-17,-0.496138938356833));
#60350=DIRECTION('center_axis',(0.491310548314114,-0.139173100960066,-0.859793459549701));
#60351=DIRECTION('ref_axis',(0.870984468928858,0.078505662250621,0.484997851417207));
#60352=DIRECTION('',(-0.0570786439550532,-0.99017405028614,0.12766118652195));
#60353=DIRECTION('center_axis',(-0.313150259135956,0.139173100960065,0.939450777407866));
#60354=DIRECTION('ref_axis',(-0.948683298050514,-3.8726732145404E-17,-0.316227766016839));
#60355=DIRECTION('center_axis',(0.313150259135956,-0.139173100960065,-0.939450777407866));
#60356=DIRECTION('ref_axis',(0.949703593340092,0.0458902050450515,0.309769549629784));
#60357=DIRECTION('',(-0.0225789275220273,-0.990015613285545,0.139137620659551));
#60358=DIRECTION('center_axis',(0.,0.139173100960066,0.99026806874157));
#60359=DIRECTION('ref_axis',(-1.,0.,0.));
#60360=DIRECTION('',(-1.,0.,0.));
#60361=DIRECTION('',(0.0225789275220281,-0.990015613285545,0.139137620659551));
#60362=DIRECTION('center_axis',(0.313150259135957,0.139173100960066,0.939450777407865));
#60363=DIRECTION('ref_axis',(-0.948683298050513,3.87267321454041E-17,0.31622776601684));
#60364=DIRECTION('center_axis',(-0.313150259135957,-0.139173100960066,-0.939450777407865));
#60365=DIRECTION('ref_axis',(-0.949703593340092,0.0458902050450518,0.309769549629785));
#60366=DIRECTION('',(0.0570786439550534,-0.99017405028614,0.12766118652195));
#60367=DIRECTION('center_axis',(0.491310548314113,0.139173100960066,0.859793459549702));
#60368=DIRECTION('ref_axis',(-0.86824314212446,6.0759496279106E-17,0.496138938356832));
#60369=DIRECTION('center_axis',(-0.491310548314113,-0.139173100960066,-0.859793459549702));
#60370=DIRECTION('ref_axis',(-0.870984468928858,0.0785056622506208,0.484997851417206));
#60371=DIRECTION('',(0.0552259184163649,-0.990142714187765,0.128714814516259));
#60372=DIRECTION('center_axis',(0.284551435696759,0.139173100960066,0.948504785655862));
#60373=DIRECTION('ref_axis',(-0.957826285221151,3.51899668300585E-17,0.287347885566345));
#60374=DIRECTION('center_axis',(-0.284551435696759,-0.139173100960066,-0.948504785655862));
#60375=DIRECTION('ref_axis',(-0.958660774436356,0.0413096131025497,0.281536916624453));
#60376=DIRECTION('',(0.0161503784824051,-0.989961587360995,0.140410899949307));
#60377=DIRECTION('center_axis',(-0.0617712249622997,0.139173100960066,0.988339599396795));
#60378=DIRECTION('ref_axis',(-0.998052578482889,-7.63913684762395E-18,-0.0623782861551806));
#60379=DIRECTION('center_axis',(0.0617712249622997,-0.139173100960066,-0.988339599396795));
#60380=DIRECTION('ref_axis',(0.998090334472114,0.00861334152950386,0.0611677576917706));
#60381=DIRECTION('',(-0.137998583506848,-0.981910942816533,0.129642937822505));
#60382=DIRECTION('center_axis',(-0.99026806874157,0.139173100960066,-1.70437892618156E-17));
#60383=DIRECTION('ref_axis',(0.,-1.22464679914735E-16,-1.));
#60384=DIRECTION('center_axis',(0.99026806874157,-0.139173100960066,1.70437892618156E-17));
#60385=DIRECTION('ref_axis',(0.139173100960066,0.99026806874157,0.));
#60386=DIRECTION('',(-0.137844537491629,-0.980814848463989,0.137844537491629));
#60387=DIRECTION('center_axis',(0.,0.139173100960066,0.99026806874157));
#60388=DIRECTION('ref_axis',(-1.,0.,0.));
#60389=DIRECTION('',(-1.,0.,0.));
#60390=DIRECTION('center_axis',(0.,-1.,1.22464679914735E-16));
#60391=DIRECTION('ref_axis',(1.,0.,0.));
#60392=DIRECTION('center_axis',(1.,0.,0.));
#60393=DIRECTION('ref_axis',(0.,1.,0.));
#60394=DIRECTION('center_axis',(1.,0.,0.));
#60395=DIRECTION('ref_axis',(0.,0.,-1.));
#60396=DIRECTION('center_axis',(0.649305557988371,-0.0072245784737921,0.760493325303574));
#60397=DIRECTION('ref_axis',(0.760527640763576,0.00616803217361909,-0.649276260934969));
#60398=DIRECTION('',(1.,0.,0.));
#60399=DIRECTION('center_axis',(-0.99026806874157,-0.137058748836223,0.0241671553619711));
#60400=DIRECTION('ref_axis',(-0.139173100960065,0.975223671657125,-0.171958245538723));
#60401=DIRECTION('center_axis',(-0.0617712249622996,0.0345646215150944,
0.997491655456914));
#60402=DIRECTION('ref_axis',(0.998090334472114,0.00213918413755092,0.061734173069449));
#60403=DIRECTION('center_axis',(0.284551435696759,0.0276473787012799,0.958262022045047));
#60404=DIRECTION('ref_axis',(-0.958660774436356,0.00820634526047722,0.284433077286297));
#60405=DIRECTION('center_axis',(0.491310548314114,0.0122428185845284,0.870898420315705));
#60406=DIRECTION('ref_axis',(-0.870984468928858,0.00690600823120551,0.491262009456284));
#60407=DIRECTION('center_axis',(0.313150259135956,0.026075166668434,0.949345564526583));
#60408=DIRECTION('ref_axis',(-0.949703593340092,0.00859788807423123,0.313032204601347));
#60409=DIRECTION('',(1.,0.,0.));
#60410=DIRECTION('center_axis',(-0.313150259135957,0.0260751666684338,0.949345564526583));
#60411=DIRECTION('ref_axis',(0.949703593340092,0.00859788807423126,0.313032204601348));
#60412=DIRECTION('center_axis',(-0.491310548314113,0.0122428185845283,0.870898420315706));
#60413=DIRECTION('ref_axis',(0.870984468928858,0.00690600823120549,0.491262009456283));
#60414=DIRECTION('center_axis',(-0.284551435696759,0.02764737870128,0.958262022045047));
#60415=DIRECTION('ref_axis',(0.958660774436356,0.0082063452604772,0.284433077286297));
#60416=DIRECTION('center_axis',(0.0617712249622997,0.0345646215150945,0.997491655456914));
#60417=DIRECTION('ref_axis',(-0.998090334472114,0.00213918413755093,0.061734173069449));
#60418=DIRECTION('center_axis',(0.99026806874157,-0.137058748836224,0.0241671553619712));
#60419=DIRECTION('ref_axis',(0.139173100960066,0.975223671657125,-0.171958245538724));
#60420=DIRECTION('',(1.,0.,0.));
#60421=DIRECTION('center_axis',(0.,-0.0348994967025011,-0.999390827019096));
#60422=DIRECTION('ref_axis',(1.,0.,0.));
#60423=DIRECTION('',(-0.137844537491629,-0.989850519773593,0.0345663418323005));
#60424=DIRECTION('center_axis',(-0.99026806874157,0.137058748836224,-0.0241671553619712));
#60425=DIRECTION('ref_axis',(0.,-0.173648177666931,-0.984807753012208));
#60426=DIRECTION('',(-0.137998583506848,-0.989505769153514,0.0428336755604262));
#60427=DIRECTION('center_axis',(-0.0617712249622997,-0.0345646215150945,
-0.997491655456914));
#60428=DIRECTION('ref_axis',(0.998052578482889,-0.0108318757168334,-0.0614306198252359));
#60429=DIRECTION('',(0.0161503784824051,-0.999303943318151,0.033627282728));
#60430=DIRECTION('center_axis',(0.284551435696759,-0.02764737870128,-0.958262022045047));
#60431=DIRECTION('ref_axis',(0.957826285221151,0.0498974366850416,0.282982425517402));
#60432=DIRECTION('',(0.0552259184163645,-0.997451314500147,0.0451771306857537));
#60433=DIRECTION('center_axis',(0.491310548314113,-0.0122428185845283,-0.870898420315706));
#60434=DIRECTION('ref_axis',(0.86824314212446,0.0861536225152695,0.488601473065054));
#60435=DIRECTION('',(0.057078643955053,-0.997299213951626,0.0462201931597184));
#60436=DIRECTION('center_axis',(0.313150259135957,-0.0260751666684338,-0.949345564526583));
#60437=DIRECTION('ref_axis',(0.948683298050513,0.0549123752965088,0.311423555691114));
#60438=DIRECTION('',(0.0225789275220278,-0.999136045839184,0.0348905995476467));
#60439=DIRECTION('center_axis',(0.,-0.0348994967025013,-0.999390827019096));
#60440=DIRECTION('ref_axis',(1.,0.,0.));
#60441=DIRECTION('',(-0.0225789275220274,-0.999136045839184,0.0348905995476468));
#60442=DIRECTION('center_axis',(-0.313150259135956,-0.026075166668434,-0.949345564526583));
#60443=DIRECTION('ref_axis',(0.948683298050514,-0.0549123752965086,-0.311423555691113));
#60444=DIRECTION('',(-0.0570786439550527,-0.997299213951626,0.0462201931597183));
#60445=DIRECTION('center_axis',(-0.491310548314114,-0.0122428185845284,
-0.870898420315705));
#60446=DIRECTION('ref_axis',(0.868243142124459,-0.0861536225152698,-0.488601473065055));
#60447=DIRECTION('',(-0.0552259184163635,-0.997451314500147,0.0451771306857533));
#60448=DIRECTION('center_axis',(-0.284551435696759,-0.0276473787012799,
-0.958262022045047));
#60449=DIRECTION('ref_axis',(0.957826285221151,-0.0498974366850417,-0.282982425517402));
#60450=DIRECTION('',(-0.0161503784824052,-0.999303943318151,0.0336272827279999));
#60451=DIRECTION('center_axis',(0.0617712249622996,-0.0345646215150944,
-0.997491655456914));
#60452=DIRECTION('ref_axis',(0.998052578482889,0.0108318757168334,0.0614306198252359));
#60453=DIRECTION('',(0.137998583506848,-0.989505769153514,0.0428336755604261));
#60454=DIRECTION('center_axis',(0.99026806874157,0.137058748836223,-0.0241671553619711));
#60455=DIRECTION('ref_axis',(0.,0.173648177666931,0.984807753012208));
#60456=DIRECTION('',(0.137844537491629,-0.989850519773593,0.0345663418323007));
#60457=DIRECTION('center_axis',(0.,-0.0348994967025013,-0.999390827019096));
#60458=DIRECTION('ref_axis',(1.,0.,0.));
#60459=DIRECTION('',(-0.051925424877728,-0.998042613992818,0.0348524160661849));
#60460=DIRECTION('center_axis',(-0.649305557988371,0.0072245784737921,-0.760493325303574));
#60461=DIRECTION('ref_axis',(0.755033118392644,-0.113858792838765,-0.645725301830104));
#60462=DIRECTION('center_axis',(0.,0.309016994374948,0.951056516295154));
#60463=DIRECTION('ref_axis',(-1.,0.,0.));
#60464=DIRECTION('',(-1.,0.,0.));
#60465=DIRECTION('',(0.137844537491629,-0.941977614300068,0.306067080296576));
#60466=DIRECTION('center_axis',(0.99026806874157,0.137058748836223,-0.0241671553619711));
#60467=DIRECTION('ref_axis',(0.,0.173648177666931,0.984807753012208));
#60468=DIRECTION('center_axis',(-0.99026806874157,-0.137058748836223,0.0241671553619711));
#60469=DIRECTION('ref_axis',(-0.139173100960065,0.975223671657125,-0.171958245538723));
#60470=DIRECTION('',(0.137998583506848,-0.944481249352984,0.298180416142191));
#60471=DIRECTION('center_axis',(0.0617712249622996,0.308682119187541,0.949157344732972));
#60472=DIRECTION('ref_axis',(-0.998052578482889,0.0108318757168334,0.0614306198252359));
#60473=DIRECTION('center_axis',(-0.0617712249622996,-0.308682119187541,
-0.949157344732972));
#60474=DIRECTION('ref_axis',(-0.998090334472114,0.0191041551727458,0.0587427909490065));
#60475=DIRECTION('',(-0.0161503784824054,-0.950539749516609,0.310182768482998));
#60476=DIRECTION('center_axis',(-0.284551435696759,0.301764876373726,0.909927711321104));
#60477=DIRECTION('ref_axis',(-0.957826285221151,-0.0498974366850417,-0.282982425517402));
#60478=DIRECTION('center_axis',(0.284551435696759,-0.301764876373726,-0.909927711321104));
#60479=DIRECTION('ref_axis',(0.958660774436356,0.0895703997751287,0.27008639921553));
#60480=DIRECTION('',(-0.0552259184163638,-0.952749128541176,0.298695825212035));
#60481=DIRECTION('center_axis',(-0.491310548314114,0.286360316256975,0.822564109591763));
#60482=DIRECTION('ref_axis',(-0.868243142124459,-0.0861536225152698,-0.488601473065055));
#60483=DIRECTION('center_axis',(0.491310548314114,-0.286360316256975,-0.822564109591763));
#60484=DIRECTION('ref_axis',(0.870984468928858,0.161531977910744,0.463997279083572));
#60485=DIRECTION('',(-0.0570786439550532,-0.952962949154956,0.297663645650826));
#60486=DIRECTION('center_axis',(-0.313150259135956,0.30019266434088,0.901011253802641));
#60487=DIRECTION('ref_axis',(-0.948683298050514,-0.0549123752965086,-0.311423555691113));
#60488=DIRECTION('center_axis',(0.313150259135956,-0.30019266434088,-0.901011253802641));
#60489=DIRECTION('ref_axis',(0.949703593340092,0.0989839475056046,0.297094703643677));
#60490=DIRECTION('',(-0.0225789275220273,-0.950814057294297,0.308938214670041));
#60491=DIRECTION('center_axis',(0.,0.309016994374948,0.951056516295154));
#60492=DIRECTION('ref_axis',(-1.,0.,0.));
#60493=DIRECTION('',(-1.,0.,0.));
#60494=DIRECTION('',(0.0225789275220281,-0.950814057294297,0.308938214670041));
#60495=DIRECTION('center_axis',(0.313150259135957,0.30019266434088,0.901011253802641));
#60496=DIRECTION('ref_axis',(-0.948683298050513,0.0549123752965088,0.311423555691114));
#60497=DIRECTION('center_axis',(-0.313150259135957,-0.30019266434088,-0.901011253802641));
#60498=DIRECTION('ref_axis',(-0.949703593340092,0.098983947505605,0.297094703643678));
#60499=DIRECTION('',(0.0570786439550534,-0.952962949154956,0.297663645650826));
#60500=DIRECTION('center_axis',(0.491310548314113,0.286360316256975,0.822564109591764));
#60501=DIRECTION('ref_axis',(-0.86824314212446,0.0861536225152695,0.488601473065054));
#60502=DIRECTION('center_axis',(-0.491310548314113,-0.286360316256975,-0.822564109591764));
#60503=DIRECTION('ref_axis',(-0.870984468928858,0.161531977910744,0.463997279083571));
#60504=DIRECTION('',(0.0552259184163649,-0.952749128541176,0.298695825212034));
#60505=DIRECTION('center_axis',(0.284551435696759,0.301764876373726,0.909927711321105));
#60506=DIRECTION('ref_axis',(-0.957826285221151,0.0498974366850416,0.282982425517402));
#60507=DIRECTION('center_axis',(-0.284551435696759,-0.301764876373726,-0.909927711321105));
#60508=DIRECTION('ref_axis',(-0.958660774436356,0.0895703997751285,0.270086399215529));
#60509=DIRECTION('',(0.016150378482405,-0.950539749516609,0.310182768482998));
#60510=DIRECTION('center_axis',(-0.0617712249622997,0.308682119187541,0.949157344732972));
#60511=DIRECTION('ref_axis',(-0.998052578482889,-0.0108318757168334,-0.0614306198252359));
#60512=DIRECTION('center_axis',(0.0617712249622997,-0.308682119187541,-0.949157344732972));
#60513=DIRECTION('ref_axis',(0.998090334472114,0.0191041551727458,0.0587427909490066));
#60514=DIRECTION('',(-0.137998583506848,-0.944481249352984,0.298180416142191));
#60515=DIRECTION('center_axis',(-0.99026806874157,0.137058748836224,-0.0241671553619712));
#60516=DIRECTION('ref_axis',(0.,-0.173648177666931,-0.984807753012208));
#60517=DIRECTION('center_axis',(0.99026806874157,-0.137058748836224,0.0241671553619712));
#60518=DIRECTION('ref_axis',(0.139173100960066,0.975223671657125,-0.171958245538724));
#60519=DIRECTION('',(-0.137844537491629,-0.941977614300068,0.306067080296576));
#60520=DIRECTION('center_axis',(0.,0.309016994374948,0.951056516295154));
#60521=DIRECTION('ref_axis',(-1.,0.,0.));
#60522=DIRECTION('',(-1.,0.,0.));
#60523=DIRECTION('center_axis',(0.,-0.984807753012208,0.173648177666931));
#60524=DIRECTION('ref_axis',(1.,0.,0.));
#60525=DIRECTION('center_axis',(1.,0.,0.));
#60526=DIRECTION('ref_axis',(0.,1.,0.));
#60527=DIRECTION('center_axis',(1.,0.,0.));
#60528=DIRECTION('ref_axis',(0.,0.,-1.));
#60529=DIRECTION('center_axis',(0.64930555798837,0.124943459173594,0.75019425775938));
#60530=DIRECTION('ref_axis',(-0.760527640763576,0.106671313608347,0.640483363162275));
#60531=DIRECTION('',(1.,0.,0.));
#60532=DIRECTION('center_axis',(-0.99026806874157,-0.130779935984066,0.0476000039374394));
#60533=DIRECTION('ref_axis',(-0.139173100960065,0.930547596796367,-0.338691626801824));
#60534=DIRECTION('center_axis',(-0.0617712249622996,0.20725211545606,0.976335432321108));
#60535=DIRECTION('ref_axis',(0.998090334472114,0.0128267117770656,0.0604248268374111));
#60536=DIRECTION('center_axis',(0.284551435696759,0.193627806751035,0.938902951798373));
#60537=DIRECTION('ref_axis',(-0.958660774436356,0.0574729579753755,0.278686882824878));
#60538=DIRECTION('center_axis',(0.491310548314114,0.163286746281596,0.855541573276281));
#60539=DIRECTION('ref_axis',(-0.870984468928858,0.0921078431475353,0.482599419928604));
#60540=DIRECTION('center_axis',(0.313150259135956,0.190531153552384,0.930394967059196));
#60541=DIRECTION('ref_axis',(-0.949703593340092,0.0628247387151196,0.306783534438036));
#60542=DIRECTION('',(1.,0.,0.));
#60543=DIRECTION('center_axis',(-0.313150259135957,0.190531153552383,0.930394967059195));
#60544=DIRECTION('ref_axis',(0.949703593340092,0.0628247387151198,0.306783534438036));
#60545=DIRECTION('center_axis',(-0.491310548314113,0.163286746281596,0.855541573276282));
#60546=DIRECTION('ref_axis',(0.870984468928858,0.092107843147535,0.482599419928602));
#60547=DIRECTION('center_axis',(-0.284551435696759,0.193627806751035,0.938902951798373));
#60548=DIRECTION('ref_axis',(0.958660774436356,0.0574729579753754,0.278686882824878));
#60549=DIRECTION('center_axis',(0.0617712249622997,0.20725211545606,0.976335432321108));
#60550=DIRECTION('ref_axis',(-0.998090334472114,0.0128267117770656,0.0604248268374112));
#60551=DIRECTION('center_axis',(0.99026806874157,-0.130779935984066,0.0476000039374395));
#60552=DIRECTION('ref_axis',(0.139173100960066,0.930547596796366,-0.338691626801825));
#60553=DIRECTION('',(1.,0.,0.));
#60554=DIRECTION('center_axis',(0.,-0.207911690817759,-0.978147600733806));
#60555=DIRECTION('ref_axis',(1.,0.,0.));
#60556=DIRECTION('',(-0.137844537491629,-0.968810083928407,0.205926940351068));
#60557=DIRECTION('center_axis',(-0.99026806874157,0.130779935984066,-0.0476000039374395));
#60558=DIRECTION('ref_axis',(0.,-0.342020143325669,-0.939692620785908));
#60559=DIRECTION('',(-0.137998583506848,-0.967034963408845,0.214008809386339));
#60560=DIRECTION('center_axis',(-0.0617712249622997,-0.20725211545606,-0.976335432321108));
#60561=DIRECTION('ref_axis',(0.998052578482889,-0.0213346303712044,-0.058616415197295));
#60562=DIRECTION('',(0.0161503784824051,-0.978282954629779,0.206643717435842));
#60563=DIRECTION('center_axis',(0.284551435696759,-0.193627806751035,-0.938902951798373));
#60564=DIRECTION('ref_axis',(0.957826285221151,0.0982787650057294,0.270018687665128));
#60565=DIRECTION('',(0.0552259184163645,-0.974452861356161,0.217696391632611));
#60566=DIRECTION('center_axis',(0.491310548314113,-0.163286746281596,-0.855541573276282));
#60567=DIRECTION('ref_axis',(0.86824314212446,0.169689510806249,0.46621809925847));
#60568=DIRECTION('',(0.057078643955053,-0.974121945658943,0.218697195660774));
#60569=DIRECTION('center_axis',(0.313150259135957,-0.190531153552383,-0.930394967059195));
#60570=DIRECTION('ref_axis',(0.948683298050513,0.108156265856636,0.297156898213637));
#60571=DIRECTION('',(0.0225789275220278,-0.977898235227234,0.207858686543084));
#60572=DIRECTION('center_axis',(0.,-0.20791169081776,-0.978147600733806));
#60573=DIRECTION('ref_axis',(1.,0.,0.));
#60574=DIRECTION('',(-0.0225789275220274,-0.977898235227234,0.207858686543084));
#60575=DIRECTION('center_axis',(-0.313150259135956,-0.190531153552384,-0.930394967059196));
#60576=DIRECTION('ref_axis',(0.948683298050514,-0.108156265856635,-0.297156898213636));
#60577=DIRECTION('',(-0.0570786439550527,-0.974121945658943,0.218697195660774));
#60578=DIRECTION('center_axis',(-0.491310548314114,-0.163286746281596,-0.855541573276281));
#60579=DIRECTION('ref_axis',(0.868243142124459,-0.169689510806249,-0.466218099258471));
#60580=DIRECTION('',(-0.0552259184163635,-0.974452861356161,0.21769639163261));
#60581=DIRECTION('center_axis',(-0.284551435696759,-0.193627806751035,-0.938902951798373));
#60582=DIRECTION('ref_axis',(0.957826285221151,-0.0982787650057296,-0.270018687665129));
#60583=DIRECTION('',(-0.0161503784824052,-0.978282954629779,0.206643717435842));
#60584=DIRECTION('center_axis',(0.0617712249622996,-0.20725211545606,-0.976335432321108));
#60585=DIRECTION('ref_axis',(0.998052578482889,0.0213346303712044,0.0586164151972949));
#60586=DIRECTION('',(0.137998583506848,-0.967034963408845,0.214008809386339));
#60587=DIRECTION('center_axis',(0.99026806874157,0.130779935984066,-0.0476000039374394));
#60588=DIRECTION('ref_axis',(0.,0.342020143325669,0.939692620785908));
#60589=DIRECTION('',(0.137844537491629,-0.968810083928407,0.205926940351068));
#60590=DIRECTION('center_axis',(0.,-0.20791169081776,-0.978147600733806));
#60591=DIRECTION('ref_axis',(1.,0.,0.));
#60592=DIRECTION('',(-0.0519254248777279,-0.976828045559515,0.207631210706978));
#60593=DIRECTION('center_axis',(-0.64930555798837,-0.124943459173594,-0.75019425775938));
#60594=DIRECTION('ref_axis',(0.755033118392644,-0.224258043872452,-0.616143911670627));
#60595=DIRECTION('center_axis',(0.,0.469471562785891,0.882947592858927));
#60596=DIRECTION('ref_axis',(-1.,0.,0.));
#60597=DIRECTION('',(-1.,0.,0.));
#60598=DIRECTION('',(0.137844537491629,-0.874518866989312,0.464989929744128));
#60599=DIRECTION('center_axis',(0.99026806874157,0.130779935984066,-0.0476000039374394));
#60600=DIRECTION('ref_axis',(0.,0.342020143325669,0.939692620785908));
#60601=DIRECTION('center_axis',(-0.99026806874157,-0.130779935984066,0.0476000039374394));
#60602=DIRECTION('ref_axis',(-0.139173100960065,0.930547596796367,-0.338691626801824));
#60603=DIRECTION('',(0.137998583506848,-0.878353971058417,0.457657833403968));
#60604=DIRECTION('center_axis',(0.0617712249622996,0.468811987424192,0.881135424446229));
#60605=DIRECTION('ref_axis',(-0.998052578482889,0.0213346303712044,0.0586164151972949));
#60606=DIRECTION('center_axis',(-0.0617712249622996,-0.468811987424192,
-0.881135424446229));
#60607=DIRECTION('ref_axis',(-0.998090334472114,0.0290144987282327,0.0545329542285434));
#60608=DIRECTION('',(-0.0161503784824054,-0.882236242379483,0.470529890556386));
#60609=DIRECTION('center_axis',(-0.284551435696759,0.455187678719167,0.843702943923494));
#60610=DIRECTION('ref_axis',(-0.957826285221151,-0.0982787650057296,-0.270018687665129));
#60611=DIRECTION('center_axis',(0.284551435696759,-0.455187678719167,-0.843702943923494));
#60612=DIRECTION('ref_axis',(0.958660774436356,0.135109635175349,0.250429443236754));
#60613=DIRECTION('',(-0.0552259184163638,-0.886406742738186,0.459601114406122));
#60614=DIRECTION('center_axis',(-0.491310548314114,0.424846618249727,0.760341565401402));
#60615=DIRECTION('ref_axis',(-0.868243142124459,-0.169689510806249,-0.466218099258471));
#60616=DIRECTION('center_axis',(0.491310548314114,-0.424846618249727,-0.760341565401402));
#60617=DIRECTION('ref_axis',(0.870984468928858,0.239650226161174,0.428898384218936));
#60618=DIRECTION('',(-0.0570786439550532,-0.886796551036219,0.458621745531673));
#60619=DIRECTION('center_axis',(-0.313150259135956,0.452091025520515,0.835194959184317));
#60620=DIRECTION('ref_axis',(-0.948683298050514,-0.108156265856635,-0.297156898213636));
#60621=DIRECTION('center_axis',(0.313150259135956,-0.452091025520515,-0.835194959184317));
#60622=DIRECTION('ref_axis',(0.949703593340092,0.149070112809494,0.27539278542453));
#60623=DIRECTION('',(-0.0225789275220273,-0.88272249730729,0.469351877358061));
#60624=DIRECTION('center_axis',(0.,0.469471562785891,0.882947592858927));
#60625=DIRECTION('ref_axis',(-1.,0.,0.));
#60626=DIRECTION('',(-1.,0.,0.));
#60627=DIRECTION('',(0.0225789275220281,-0.88272249730729,0.469351877358061));
#60628=DIRECTION('center_axis',(0.313150259135957,0.452091025520515,0.835194959184317));
#60629=DIRECTION('ref_axis',(-0.948683298050513,0.108156265856636,0.297156898213637));
#60630=DIRECTION('center_axis',(-0.313150259135957,-0.452091025520515,-0.835194959184317));
#60631=DIRECTION('ref_axis',(-0.949703593340092,0.149070112809494,0.275392785424531));
#60632=DIRECTION('',(0.0570786439550533,-0.886796551036219,0.458621745531673));
#60633=DIRECTION('center_axis',(0.491310548314113,0.424846618249728,0.760341565401403));
#60634=DIRECTION('ref_axis',(-0.86824314212446,0.169689510806249,0.46621809925847));
#60635=DIRECTION('center_axis',(-0.491310548314113,-0.424846618249728,-0.760341565401403));
#60636=DIRECTION('ref_axis',(-0.870984468928858,0.239650226161173,0.428898384218935));
#60637=DIRECTION('',(0.0552259184163649,-0.886406742738186,0.459601114406122));
#60638=DIRECTION('center_axis',(0.284551435696759,0.455187678719167,0.843702943923494));
#60639=DIRECTION('ref_axis',(-0.957826285221151,0.0982787650057294,0.270018687665128));
#60640=DIRECTION('center_axis',(-0.284551435696759,-0.455187678719167,-0.843702943923494));
#60641=DIRECTION('ref_axis',(-0.958660774436356,0.135109635175349,0.250429443236754));
#60642=DIRECTION('',(0.0161503784824051,-0.882236242379483,0.470529890556386));
#60643=DIRECTION('center_axis',(-0.0617712249622997,0.468811987424192,0.881135424446229));
#60644=DIRECTION('ref_axis',(-0.998052578482889,-0.0213346303712044,-0.058616415197295));
#60645=DIRECTION('center_axis',(0.0617712249622997,-0.468811987424192,-0.881135424446229));
#60646=DIRECTION('ref_axis',(0.998090334472114,0.0290144987282327,0.0545329542285434));
#60647=DIRECTION('',(-0.137998583506848,-0.878353971058417,0.457657833403968));
#60648=DIRECTION('center_axis',(-0.99026806874157,0.130779935984066,-0.0476000039374395));
#60649=DIRECTION('ref_axis',(0.,-0.342020143325669,-0.939692620785908));
#60650=DIRECTION('center_axis',(0.99026806874157,-0.130779935984066,0.0476000039374395));
#60651=DIRECTION('ref_axis',(0.139173100960066,0.930547596796366,-0.338691626801825));
#60652=DIRECTION('',(-0.137844537491629,-0.874518866989312,0.464989929744128));
#60653=DIRECTION('center_axis',(0.,0.469471562785891,0.882947592858927));
#60654=DIRECTION('ref_axis',(-1.,0.,0.));
#60655=DIRECTION('',(-1.,0.,0.));
#60656=DIRECTION('center_axis',(0.,-0.939692620785908,0.342020143325669));
#60657=DIRECTION('ref_axis',(1.,0.,0.));
#60658=DIRECTION('center_axis',(1.,0.,0.));
#60659=DIRECTION('ref_axis',(0.,1.,0.));
#60660=DIRECTION('center_axis',(1.,0.,0.));
#60661=DIRECTION('ref_axis',(0.,0.,-1.));
#60662=DIRECTION('center_axis',(0.64930555798837,0.253315153038431,0.717100917309779));
#60663=DIRECTION('ref_axis',(-0.760527640763576,0.216269505504612,0.612229702500115));
#60664=DIRECTION('',(1.,0.,0.));
#60665=DIRECTION('center_axis',(-0.99026806874157,-0.120527440954873,0.0695865504800327));
#60666=DIRECTION('ref_axis',(-0.139173100960065,0.857597304086756,-0.495134034370783));
#60667=DIRECTION('center_axis',(-0.0617712249622996,0.373642358743524,0.925513751123792));
#60668=DIRECTION('ref_axis',(0.998090334472114,0.0231245062698634,0.0572795028183562));
#60669=DIRECTION('center_axis',(0.284551435696759,0.353724951873058,0.891015790469123));
#60670=DIRECTION('ref_axis',(-0.958660774436356,0.104993283944912,0.264472928451193));
#60671=DIRECTION('center_axis',(0.491310548314114,0.309369288819977,0.814189528457782));
#60672=DIRECTION('ref_axis',(-0.870984468928858,0.174511027858645,0.459273291233482));
#60673=DIRECTION('center_axis',(0.313150259135956,0.34919794774906,0.883174789320284));
#60674=DIRECTION('ref_axis',(-0.949703593340092,0.115142691461001,0.291213401820784));
#60675=DIRECTION('',(1.,0.,0.));
#60676=DIRECTION('center_axis',(-0.313150259135957,0.349197947749059,0.883174789320284));
#60677=DIRECTION('ref_axis',(0.949703593340092,0.115142691461001,0.291213401820785));
#60678=DIRECTION('center_axis',(-0.491310548314113,0.309369288819978,0.814189528457783));
#60679=DIRECTION('ref_axis',(0.870984468928858,0.174511027858644,0.459273291233481));
#60680=DIRECTION('center_axis',(-0.284551435696759,0.353724951873058,0.891015790469123));
#60681=DIRECTION('ref_axis',(0.958660774436356,0.104993283944912,0.264472928451193));
#60682=DIRECTION('center_axis',(0.0617712249622997,0.373642358743524,0.925513751123792));
#60683=DIRECTION('ref_axis',(-0.998090334472114,0.0231245062698634,0.0572795028183563));
#60684=DIRECTION('center_axis',(0.99026806874157,-0.120527440954873,0.0695865504800329));
#60685=DIRECTION('ref_axis',(0.139173100960066,0.857597304086755,-0.495134034370784));
#60686=DIRECTION('',(1.,0.,0.));
#60687=DIRECTION('center_axis',(0.,-0.374606593415912,-0.927183854566788));
#60688=DIRECTION('ref_axis',(1.,0.,0.));
#60689=DIRECTION('',(-0.137844537491629,-0.918332843924614,0.371030552991327));
#60690=DIRECTION('center_axis',(-0.99026806874157,0.120527440954873,-0.0695865504800329));
#60691=DIRECTION('ref_axis',(0.,-0.5,-0.866025403784439));
#60692=DIRECTION('',(-0.137998583506848,-0.9151812896443,0.378681393832731));
#60693=DIRECTION('center_axis',(-0.0617712249622997,-0.373642358743524,
-0.925513751123792));
#60694=DIRECTION('ref_axis',(0.998052578482889,-0.0311891430775903,-0.0540211804549215));
#60695=DIRECTION('',(0.0161503784824051,-0.927537333400043,0.373381387356163));
#60696=DIRECTION('center_axis',(0.284551435696759,-0.353724951873058,-0.891015790469123));
#60697=DIRECTION('ref_axis',(0.957826285221151,0.143673942783173,0.248850568624199));
#60698=DIRECTION('',(0.0552259184163645,-0.921846151116809,0.3836010578794));
#60699=DIRECTION('center_axis',(0.491310548314113,-0.309369288819978,-0.814189528457783));
#60700=DIRECTION('ref_axis',(0.86824314212446,0.248069469178416,0.429668924423658));
#60701=DIRECTION('',(0.057078643955053,-0.921346474976903,0.384529194537798));
#60702=DIRECTION('center_axis',(0.313150259135957,-0.349197947749059,-0.883174789320284));
#60703=DIRECTION('ref_axis',(0.948683298050513,0.15811388300842,0.273861278752585));
#60704=DIRECTION('',(0.0225789275220278,-0.926947481578288,0.374511092529479));
#60705=DIRECTION('center_axis',(0.,-0.374606593415912,-0.927183854566788));
#60706=DIRECTION('ref_axis',(1.,0.,0.));
#60707=DIRECTION('',(-0.0225789275220274,-0.926947481578288,0.374511092529479));
#60708=DIRECTION('center_axis',(-0.313150259135956,-0.34919794774906,-0.883174789320284));
#60709=DIRECTION('ref_axis',(0.948683298050514,-0.158113883008419,-0.273861278752584));
#60710=DIRECTION('',(-0.0570786439550527,-0.921346474976903,0.384529194537798));
#60711=DIRECTION('center_axis',(-0.491310548314114,-0.309369288819977,-0.814189528457782));
#60712=DIRECTION('ref_axis',(0.868243142124459,-0.248069469178417,-0.429668924423659));
#60713=DIRECTION('',(-0.0552259184163635,-0.921846151116809,0.3836010578794));
#60714=DIRECTION('center_axis',(-0.284551435696759,-0.353724951873058,-0.891015790469123));
#60715=DIRECTION('ref_axis',(0.957826285221151,-0.143673942783173,-0.248850568624199));
#60716=DIRECTION('',(-0.0161503784824052,-0.927537333400043,0.373381387356162));
#60717=DIRECTION('center_axis',(0.0617712249622996,-0.373642358743524,-0.925513751123792));
#60718=DIRECTION('ref_axis',(0.998052578482889,0.0311891430775903,0.0540211804549215));
#60719=DIRECTION('',(0.137998583506848,-0.9151812896443,0.378681393832731));
#60720=DIRECTION('center_axis',(0.99026806874157,0.120527440954873,-0.0695865504800327));
#60721=DIRECTION('ref_axis',(0.,0.5,0.866025403784439));
#60722=DIRECTION('',(0.137844537491629,-0.918332843924614,0.371030552991328));
#60723=DIRECTION('center_axis',(0.,-0.374606593415912,-0.927183854566787));
#60724=DIRECTION('ref_axis',(1.,0.,0.));
#60725=DIRECTION('',(-0.051925424877728,-0.925933051260728,0.374101236076902));
#60726=DIRECTION('center_axis',(-0.64930555798837,-0.253315153038431,-0.717100917309779));
#60727=DIRECTION('ref_axis',(0.755033118392644,-0.327843327723121,-0.567841300538901));
#60728=DIRECTION('center_axis',(0.,0.615661475325658,0.788010753606722));
#60729=DIRECTION('ref_axis',(-1.,0.,0.));
#60730=DIRECTION('',(-1.,0.,0.));
#60731=DIRECTION('',(0.137844537491629,-0.780488306432985,0.609784295472661));
#60732=DIRECTION('center_axis',(0.99026806874157,0.120527440954873,-0.0695865504800327));
#60733=DIRECTION('ref_axis',(0.,0.5,0.866025403784439));
#60734=DIRECTION('center_axis',(-0.99026806874157,-0.120527440954873,0.0695865504800327));
#60735=DIRECTION('ref_axis',(-0.139173100960065,0.857597304086756,-0.495134034370783));
#60736=DIRECTION('',(0.137998583506848,-0.785538351821795,0.603229548983803));
#60737=DIRECTION('center_axis',(0.0617712249622996,0.61469724065327,0.786340650163727));
#60738=DIRECTION('ref_axis',(-0.998052578482889,0.0311891430775903,0.0540211804549215));
#60739=DIRECTION('center_axis',(-0.0617712249622996,-0.61469724065327,-0.786340650163727));
#60740=DIRECTION('ref_axis',(-0.998090334472114,0.0380432514219071,0.0486661612888524));
#60741=DIRECTION('',(-0.0161503784824054,-0.787126433450736,0.616580200004832));
#60742=DIRECTION('center_axis',(-0.284551435696759,0.594779833782804,0.751842689509058));
#60743=DIRECTION('ref_axis',(-0.957826285221151,-0.143673942783173,-0.248850568624199));
#60744=DIRECTION('center_axis',(0.284551435696759,-0.594779833782804,-0.751842689509058));
#60745=DIRECTION('ref_axis',(0.958660774436356,0.176543632679541,0.223163315348643));
#60746=DIRECTION('',(-0.0552259184163638,-0.793131336600549,0.606541656308365));
#60747=DIRECTION('center_axis',(-0.491310548314114,0.550424170729724,0.675016427497717));
#60748=DIRECTION('ref_axis',(-0.868243142124459,-0.248069469178417,-0.429668924423659));
#60749=DIRECTION('center_axis',(0.491310548314114,-0.550424170729724,-0.675016427497717));
#60750=DIRECTION('ref_axis',(0.870984468928858,0.310486823558562,0.380767628982861));
#60751=DIRECTION('',(-0.0570786439550532,-0.793685288454953,0.605644855748342));
#60752=DIRECTION('center_axis',(-0.313150259135956,0.590252829658806,0.744001688360219));
#60753=DIRECTION('ref_axis',(-0.948683298050514,-0.158113883008419,-0.273861278752584));
#60754=DIRECTION('center_axis',(0.313150259135956,-0.590252829658806,-0.744001688360219));
#60755=DIRECTION('ref_axis',(0.949703593340092,0.194626858168784,0.245323196775732));
#60756=DIRECTION('',(-0.0225789275220273,-0.787809860918738,0.615504520756066));
#60757=DIRECTION('center_axis',(0.,0.615661475325658,0.788010753606722));
#60758=DIRECTION('ref_axis',(-1.,0.,0.));
#60759=DIRECTION('',(-1.,0.,0.));
#60760=DIRECTION('',(0.0225789275220281,-0.787809860918738,0.615504520756066));
#60761=DIRECTION('center_axis',(0.313150259135957,0.590252829658806,0.744001688360219));
#60762=DIRECTION('ref_axis',(-0.948683298050513,0.15811388300842,0.273861278752585));
#60763=DIRECTION('center_axis',(-0.313150259135957,-0.590252829658806,-0.744001688360219));
#60764=DIRECTION('ref_axis',(-0.949703593340092,0.194626858168784,0.245323196775733));
#60765=DIRECTION('',(0.0570786439550533,-0.793685288454953,0.605644855748342));
#60766=DIRECTION('center_axis',(0.491310548314113,0.550424170729724,0.675016427497717));
#60767=DIRECTION('ref_axis',(-0.86824314212446,0.248069469178416,0.429668924423658));
#60768=DIRECTION('center_axis',(-0.491310548314113,-0.550424170729724,-0.675016427497717));
#60769=DIRECTION('ref_axis',(-0.870984468928858,0.310486823558561,0.38076762898286));
#60770=DIRECTION('',(0.0552259184163649,-0.79313133660055,0.606541656308365));
#60771=DIRECTION('center_axis',(0.284551435696759,0.594779833782804,0.751842689509058));
#60772=DIRECTION('ref_axis',(-0.957826285221151,0.143673942783173,0.248850568624199));
#60773=DIRECTION('center_axis',(-0.284551435696759,-0.594779833782804,-0.751842689509058));
#60774=DIRECTION('ref_axis',(-0.958660774436356,0.176543632679541,0.223163315348643));
#60775=DIRECTION('',(0.016150378482405,-0.787126433450736,0.616580200004832));
#60776=DIRECTION('center_axis',(-0.0617712249622997,0.61469724065327,0.786340650163727));
#60777=DIRECTION('ref_axis',(-0.998052578482889,-0.0311891430775903,-0.0540211804549215));
#60778=DIRECTION('center_axis',(0.0617712249622997,-0.61469724065327,-0.786340650163727));
#60779=DIRECTION('ref_axis',(0.998090334472114,0.0380432514219071,0.0486661612888524));
#60780=DIRECTION('',(-0.137998583506848,-0.785538351821795,0.603229548983803));
#60781=DIRECTION('center_axis',(-0.99026806874157,0.120527440954873,-0.0695865504800329));
#60782=DIRECTION('ref_axis',(0.,-0.5,-0.866025403784439));
#60783=DIRECTION('center_axis',(0.99026806874157,-0.120527440954873,0.0695865504800329));
#60784=DIRECTION('ref_axis',(0.139173100960066,0.857597304086755,-0.495134034370784));
#60785=DIRECTION('',(-0.137844537491629,-0.780488306432985,0.609784295472661));
#60786=DIRECTION('center_axis',(0.,0.615661475325658,0.788010753606722));
#60787=DIRECTION('ref_axis',(-1.,0.,0.));
#60788=DIRECTION('',(-1.,0.,0.));
#60789=DIRECTION('center_axis',(0.,-0.866025403784439,0.5));
#60790=DIRECTION('ref_axis',(1.,0.,0.));
#60791=DIRECTION('center_axis',(1.,0.,0.));
#60792=DIRECTION('ref_axis',(0.,1.,0.));
#60793=DIRECTION('center_axis',(1.,0.,0.));
#60794=DIRECTION('ref_axis',(0.,0.,-1.));
#60795=DIRECTION('center_axis',(0.64930555798837,0.373989994161848,0.662218828358294));
#60796=DIRECTION('ref_axis',(-0.760527640763576,0.319296457913771,0.565373752130667));
#60797=DIRECTION('',(1.,0.,0.));
#60798=DIRECTION('center_axis',(-0.99026806874157,-0.106612780622095,0.0894587448987839));
#60799=DIRECTION('ref_axis',(-0.139173100960065,0.758589351257639,-0.636532044855303));
#60800=DIRECTION('center_axis',(-0.0617712249622996,0.528679668032723,0.846570802931135));
#60801=DIRECTION('ref_axis',(0.998090334472114,0.0327196743412163,0.0523937700909925));
#60802=DIRECTION('center_axis',(0.284551435696759,0.50307434332588,0.816055565222214));
#60803=DIRECTION('ref_axis',(-0.958660774436356,0.149323442110948,0.242223097976277));
#60804=DIRECTION('center_axis',(0.491310548314114,0.446051802065978,0.748098746816874));
#60805=DIRECTION('ref_axis',(-0.870984468928858,0.25161178329511,0.42199237598773));
#60806=DIRECTION('center_axis',(0.313150259135956,0.497254539006069,0.809119792515883));
#60807=DIRECTION('ref_axis',(-0.949703593340092,0.163962091791853,0.266794897350299));
#60808=DIRECTION('',(1.,0.,0.));
#60809=DIRECTION('center_axis',(-0.313150259135957,0.497254539006068,0.809119792515883));
#60810=DIRECTION('ref_axis',(0.949703593340092,0.163962091791853,0.2667948973503));
#60811=DIRECTION('center_axis',(-0.491310548314113,0.446051802065979,0.748098746816875));
#60812=DIRECTION('ref_axis',(0.870984468928858,0.25161178329511,0.421992375987729));
#60813=DIRECTION('center_axis',(-0.284551435696759,0.503074343325881,0.816055565222214));
#60814=DIRECTION('ref_axis',(0.958660774436356,0.149323442110948,0.242223097976277));
#60815=DIRECTION('center_axis',(0.0617712249622997,0.528679668032723,0.846570802931135));
#60816=DIRECTION('ref_axis',(-0.998090334472114,0.0327196743412163,0.0523937700909926));
#60817=DIRECTION('center_axis',(0.99026806874157,-0.106612780622095,0.0894587448987841));
#60818=DIRECTION('ref_axis',(0.139173100960066,0.758589351257642,-0.636532044855299));
#60819=DIRECTION('',(1.,0.,0.));
#60820=DIRECTION('center_axis',(0.,-0.529919264233205,-0.848048096156426));
#60821=DIRECTION('ref_axis',(1.,0.,0.));
#60822=DIRECTION('',(-0.137844537491629,-0.839952525157012,0.524860590029465));
#60823=DIRECTION('center_axis',(-0.99026806874157,0.106612780622095,-0.0894587448987841));
#60824=DIRECTION('ref_axis',(0.,-0.642787609686539,-0.766044443118978));
#60825=DIRECTION('',(-0.137998583506848,-0.835520295497991,0.531847935749547));
#60826=DIRECTION('center_axis',(-0.0617712249622997,-0.528679668032723,
-0.846570802931135));
#60827=DIRECTION('ref_axis',(0.998052578482889,-0.0400959894540315,-0.0477845394804615));
#60828=DIRECTION('',(0.0161503784824051,-0.848608959651484,0.528774052761765));
#60829=DIRECTION('center_axis',(0.284551435696759,-0.503074343325881,-0.816055565222214));
#60830=DIRECTION('ref_axis',(0.957826285221151,0.184703660511672,0.220121250980087));
#60831=DIRECTION('',(0.0552259184163645,-0.841229612052432,0.537850200094026));
#60832=DIRECTION('center_axis',(0.491310548314113,-0.446051802065979,-0.748098746816875));
#60833=DIRECTION('ref_axis',(0.86824314212446,0.318911962258805,0.3800644767432));
#60834=DIRECTION('',(0.057078643955053,-0.840576357876501,0.538677468419953));
#60835=DIRECTION('center_axis',(0.313150259135957,-0.497254539006068,-0.809119792515883));
#60836=DIRECTION('ref_axis',(0.948683298050513,0.203267289834479,0.242244522917128));
#60837=DIRECTION('',(0.0225789275220278,-0.847831897759644,0.529784168481124));
#60838=DIRECTION('center_axis',(0.,-0.529919264233205,-0.848048096156426));
#60839=DIRECTION('ref_axis',(1.,0.,0.));
#60840=DIRECTION('',(-0.0225789275220274,-0.847831897759644,0.529784168481124));
#60841=DIRECTION('center_axis',(-0.313150259135956,-0.497254539006069,-0.809119792515883));
#60842=DIRECTION('ref_axis',(0.948683298050514,-0.203267289834478,-0.242244522917128));
#60843=DIRECTION('',(-0.0570786439550527,-0.840576357876501,0.538677468419953));
#60844=DIRECTION('center_axis',(-0.491310548314114,-0.446051802065978,-0.748098746816874));
#60845=DIRECTION('ref_axis',(0.868243142124459,-0.318911962258806,-0.380064476743201));
#60846=DIRECTION('',(-0.0552259184163635,-0.841229612052433,0.537850200094025));
#60847=DIRECTION('center_axis',(-0.284551435696759,-0.50307434332588,-0.816055565222214));
#60848=DIRECTION('ref_axis',(0.957826285221151,-0.184703660511673,-0.220121250980087));
#60849=DIRECTION('',(-0.0161503784824052,-0.848608959651484,0.528774052761765));
#60850=DIRECTION('center_axis',(0.0617712249622996,-0.528679668032723,-0.846570802931135));
#60851=DIRECTION('ref_axis',(0.998052578482889,0.0400959894540314,0.0477845394804615));
#60852=DIRECTION('',(0.137998583506848,-0.835520295497991,0.531847935749547));
#60853=DIRECTION('center_axis',(0.99026806874157,0.106612780622095,-0.0894587448987839));
#60854=DIRECTION('ref_axis',(0.,0.642787609686539,0.766044443118978));
#60855=DIRECTION('',(0.137844537491629,-0.839952525157012,0.524860590029465));
#60856=DIRECTION('center_axis',(0.,-0.529919264233205,-0.848048096156426));
#60857=DIRECTION('ref_axis',(1.,0.,0.));
#60858=DIRECTION('',(-0.051925424877728,-0.846904049744114,0.52920438469299));
#60859=DIRECTION('center_axis',(-0.64930555798837,-0.373989994161848,-0.662218828358294));
#60860=DIRECTION('ref_axis',(0.755033118392644,-0.421467257957652,-0.502285118831862));
#60861=DIRECTION('center_axis',(0.,0.743144825477394,0.669130606358858));
#60862=DIRECTION('ref_axis',(-1.,0.,0.));
#60863=DIRECTION('',(-1.,0.,0.));
#60864=DIRECTION('',(0.137844537491629,-0.662743003631831,0.736050673949001));
#60865=DIRECTION('center_axis',(0.99026806874157,0.106612780622095,-0.0894587448987839));
#60866=DIRECTION('ref_axis',(0.,0.642787609686539,0.766044443118978));
#60867=DIRECTION('center_axis',(-0.99026806874157,-0.106612780622095,0.0894587448987839));
#60868=DIRECTION('ref_axis',(-0.139173100960065,0.758589351257639,-0.636532044855303));
#60869=DIRECTION('',(0.137998583506848,-0.668854547266653,0.730472439966645));
#60870=DIRECTION('center_axis',(0.0617712249622996,0.741905229276912,0.667653313133567));
#60871=DIRECTION('ref_axis',(-0.998052578482889,0.0400959894540314,0.0477845394804615));
#60872=DIRECTION('center_axis',(-0.0617712249622996,-0.741905229276912,
-0.667653313133567));
#60873=DIRECTION('ref_axis',(-0.998090334472114,0.045916079171941,0.0413206716646654));
#60874=DIRECTION('',(-0.0161503784824054,-0.668100186146782,0.743896032080768));
#60875=DIRECTION('center_axis',(-0.284551435696759,0.71629990457007,0.637138075424646));
#60876=DIRECTION('ref_axis',(-0.957826285221151,-0.184703660511673,-0.220121250980087));
#60877=DIRECTION('center_axis',(0.284551435696759,-0.71629990457007,-0.637138075424646));
#60878=DIRECTION('ref_axis',(0.958660774436356,0.212613441240154,0.18911648304975));
#60879=DIRECTION('',(-0.0552259184163638,-0.675757036144127,0.735052736908566));
#60880=DIRECTION('center_axis',(-0.491310548314114,0.659277363310168,0.569181257019306));
#60881=DIRECTION('ref_axis',(-0.868243142124459,-0.318911962258806,-0.380064476743201));
#60882=DIRECTION('center_axis',(0.491310548314114,-0.659277363310168,-0.569181257019306));
#60883=DIRECTION('ref_axis',(0.870984468928858,0.371889435936037,0.32106744201786));
#60884=DIRECTION('',(-0.0570786439550532,-0.676458300008118,0.734265753494182));
#60885=DIRECTION('center_axis',(-0.313150259135956,0.710480100250258,0.630202302718315));
#60886=DIRECTION('ref_axis',(-0.948683298050514,-0.203267289834478,-0.242244522917128));
#60887=DIRECTION('center_axis',(0.313150259135956,-0.710480100250258,-0.630202302718315));
#60888=DIRECTION('ref_axis',(0.949703593340092,0.234269964928557,0.207799586932431));
#60889=DIRECTION('',(-0.0225789275220273,-0.668960020557194,0.742955370751214));
#60890=DIRECTION('center_axis',(0.,0.743144825477394,0.669130606358858));
#60891=DIRECTION('ref_axis',(-1.,0.,0.));
#60892=DIRECTION('',(-1.,0.,0.));
#60893=DIRECTION('',(0.0225789275220281,-0.668960020557194,0.742955370751214));
#60894=DIRECTION('center_axis',(0.313150259135957,0.710480100250258,0.630202302718315));
#60895=DIRECTION('ref_axis',(-0.948683298050513,0.203267289834479,0.242244522917128));
#60896=DIRECTION('center_axis',(-0.313150259135957,-0.710480100250258,-0.630202302718315));
#60897=DIRECTION('ref_axis',(-0.949703593340092,0.234269964928558,0.207799586932432));
#60898=DIRECTION('',(0.0570786439550534,-0.676458300008118,0.734265753494183));
#60899=DIRECTION('center_axis',(0.491310548314113,0.659277363310168,0.569181257019307));
#60900=DIRECTION('ref_axis',(-0.86824314212446,0.318911962258805,0.3800644767432));
#60901=DIRECTION('center_axis',(-0.491310548314113,-0.659277363310168,-0.569181257019307));
#60902=DIRECTION('ref_axis',(-0.870984468928858,0.371889435936036,0.321067442017859));
#60903=DIRECTION('',(0.0552259184163649,-0.675757036144127,0.735052736908566));
#60904=DIRECTION('center_axis',(0.284551435696759,0.71629990457007,0.637138075424647));
#60905=DIRECTION('ref_axis',(-0.957826285221151,0.184703660511672,0.220121250980087));
#60906=DIRECTION('center_axis',(-0.284551435696759,-0.71629990457007,-0.637138075424647));
#60907=DIRECTION('ref_axis',(-0.958660774436356,0.212613441240154,0.189116483049749));
#60908=DIRECTION('',(0.0161503784824051,-0.668100186146782,0.743896032080768));
#60909=DIRECTION('center_axis',(-0.0617712249622997,0.741905229276912,0.667653313133567));
#60910=DIRECTION('ref_axis',(-0.998052578482889,-0.0400959894540315,-0.0477845394804615));
#60911=DIRECTION('center_axis',(0.0617712249622997,-0.741905229276912,-0.667653313133567));
#60912=DIRECTION('ref_axis',(0.998090334472114,0.045916079171941,0.0413206716646654));
#60913=DIRECTION('',(-0.137998583506848,-0.668854547266653,0.730472439966645));
#60914=DIRECTION('center_axis',(-0.99026806874157,0.106612780622095,-0.0894587448987841));
#60915=DIRECTION('ref_axis',(0.,-0.642787609686539,-0.766044443118978));
#60916=DIRECTION('center_axis',(0.99026806874157,-0.106612780622095,0.0894587448987841));
#60917=DIRECTION('ref_axis',(0.139173100960066,0.758589351257642,-0.636532044855299));
#60918=DIRECTION('',(-0.137844537491629,-0.662743003631831,0.736050673949));
#60919=DIRECTION('center_axis',(0.,0.743144825477394,0.669130606358858));
#60920=DIRECTION('ref_axis',(-1.,0.,0.));
#60921=DIRECTION('',(-1.,0.,0.));
#60922=DIRECTION('center_axis',(0.,-0.766044443118978,0.642787609686539));
#60923=DIRECTION('ref_axis',(1.,0.,0.));
#60924=DIRECTION('center_axis',(1.,0.,0.));
#60925=DIRECTION('ref_axis',(0.,1.,0.));
#60926=DIRECTION('center_axis',(1.,0.,0.));
#60927=DIRECTION('ref_axis',(0.,0.,-1.));
#60928=DIRECTION('center_axis',(0.64930555798837,0.483301338560726,0.587215555406038));
#60929=DIRECTION('ref_axis',(-0.760527640763576,0.412621749021023,0.501339206395651));
#60930=DIRECTION('',(1.,0.,0.));
#60931=DIRECTION('center_axis',(-0.99026806874157,-0.0894587448987838,0.106612780622095));
#60932=DIRECTION('ref_axis',(-0.139173100960065,0.636532044855299,-0.758589351257642));
#60933=DIRECTION('center_axis',(-0.0617712249622996,0.667653313133567,0.741905229276912));
#60934=DIRECTION('ref_axis',(0.998090334472114,0.0413206716646654,0.045916079171941));
#60935=DIRECTION('center_axis',(0.284551435696759,0.637138075424646,0.71629990457007));
#60936=DIRECTION('ref_axis',(-0.958660774436356,0.18911648304975,0.212613441240154));
#60937=DIRECTION('center_axis',(0.491310548314114,0.569181257019307,0.659277363310167));
#60938=DIRECTION('ref_axis',(-0.870984468928858,0.32106744201786,0.371889435936037));
#60939=DIRECTION('center_axis',(0.313150259135956,0.630202302718315,0.710480100250258));
#60940=DIRECTION('ref_axis',(-0.949703593340092,0.207799586932431,0.234269964928557));
#60941=DIRECTION('',(1.,0.,0.));
#60942=DIRECTION('center_axis',(-0.313150259135957,0.630202302718315,0.710480100250258));
#60943=DIRECTION('ref_axis',(0.949703593340092,0.207799586932432,0.234269964928558));
#60944=DIRECTION('center_axis',(-0.491310548314113,0.569181257019307,0.659277363310168));
#60945=DIRECTION('ref_axis',(0.870984468928858,0.321067442017859,0.371889435936036));
#60946=DIRECTION('center_axis',(-0.284551435696759,0.637138075424647,0.71629990457007));
#60947=DIRECTION('ref_axis',(0.958660774436356,0.18911648304975,0.212613441240154));
#60948=DIRECTION('center_axis',(0.0617712249622997,0.667653313133568,0.741905229276912));
#60949=DIRECTION('ref_axis',(-0.998090334472114,0.0413206716646654,0.045916079171941));
#60950=DIRECTION('center_axis',(0.99026806874157,-0.0894587448987841,0.106612780622095));
#60951=DIRECTION('ref_axis',(0.139173100960066,0.636532044855299,-0.758589351257642));
#60952=DIRECTION('',(1.,0.,0.));
#60953=DIRECTION('center_axis',(0.,-0.669130606358858,-0.743144825477394));
#60954=DIRECTION('ref_axis',(1.,0.,0.));
#60955=DIRECTION('',(-0.137844537491629,-0.736050673949001,0.662743003631831));
#60956=DIRECTION('center_axis',(-0.99026806874157,0.0894587448987841,-0.106612780622095));
#60957=DIRECTION('ref_axis',(0.,-0.766044443118978,-0.642787609686539));
#60958=DIRECTION('',(-0.137998583506848,-0.730472439966645,0.668854547266653));
#60959=DIRECTION('center_axis',(-0.0617712249622997,-0.667653313133568,
-0.741905229276912));
#60960=DIRECTION('ref_axis',(0.998052578482889,-0.0477845394804615,-0.0400959894540315));
#60961=DIRECTION('',(0.0161503784824051,-0.743896032080767,0.668100186146782));
#60962=DIRECTION('center_axis',(0.284551435696759,-0.637138075424647,-0.71629990457007));
#60963=DIRECTION('ref_axis',(0.957826285221151,0.220121250980087,0.184703660511672));
#60964=DIRECTION('',(0.0552259184163645,-0.735052736908566,0.675757036144127));
#60965=DIRECTION('center_axis',(0.491310548314113,-0.569181257019307,-0.659277363310168));
#60966=DIRECTION('ref_axis',(0.86824314212446,0.3800644767432,0.318911962258805));
#60967=DIRECTION('',(0.057078643955053,-0.734265753494182,0.676458300008118));
#60968=DIRECTION('center_axis',(0.313150259135957,-0.630202302718315,-0.710480100250258));
#60969=DIRECTION('ref_axis',(0.948683298050513,0.242244522917128,0.203267289834479));
#60970=DIRECTION('',(0.0225789275220278,-0.742955370751214,0.668960020557194));
#60971=DIRECTION('center_axis',(0.,-0.669130606358858,-0.743144825477394));
#60972=DIRECTION('ref_axis',(1.,0.,0.));
#60973=DIRECTION('',(-0.0225789275220274,-0.742955370751214,0.668960020557194));
#60974=DIRECTION('center_axis',(-0.313150259135956,-0.630202302718315,-0.710480100250258));
#60975=DIRECTION('ref_axis',(0.948683298050513,-0.242244522917128,-0.203267289834478));
#60976=DIRECTION('',(-0.0570786439550527,-0.734265753494182,0.676458300008118));
#60977=DIRECTION('center_axis',(-0.491310548314114,-0.569181257019307,-0.659277363310167));
#60978=DIRECTION('ref_axis',(0.868243142124459,-0.380064476743201,-0.318911962258806));
#60979=DIRECTION('',(-0.0552259184163635,-0.735052736908566,0.675757036144127));
#60980=DIRECTION('center_axis',(-0.284551435696759,-0.637138075424646,-0.71629990457007));
#60981=DIRECTION('ref_axis',(0.957826285221151,-0.220121250980087,-0.184703660511673));
#60982=DIRECTION('',(-0.0161503784824052,-0.743896032080767,0.668100186146782));
#60983=DIRECTION('center_axis',(0.0617712249622996,-0.667653313133567,-0.741905229276912));
#60984=DIRECTION('ref_axis',(0.998052578482889,0.0477845394804615,0.0400959894540314));
#60985=DIRECTION('',(0.137998583506848,-0.730472439966645,0.668854547266653));
#60986=DIRECTION('center_axis',(0.99026806874157,0.0894587448987838,-0.106612780622095));
#60987=DIRECTION('ref_axis',(0.,0.766044443118978,0.642787609686539));
#60988=DIRECTION('',(0.137844537491629,-0.736050673949001,0.662743003631831));
#60989=DIRECTION('center_axis',(0.,-0.669130606358858,-0.743144825477394));
#60990=DIRECTION('ref_axis',(1.,0.,0.));
#60991=DIRECTION('',(-0.0519254248777279,-0.742142297230154,0.66822792587052));
#60992=DIRECTION('center_axis',(-0.64930555798837,-0.483301338560726,-0.587215555406038));
#60993=DIRECTION('ref_axis',(0.755033118392644,-0.502285118831862,-0.421467257957652));
#60994=DIRECTION('center_axis',(0.,0.848048096156426,0.529919264233205));
#60995=DIRECTION('ref_axis',(-1.,0.,0.));
#60996=DIRECTION('',(-1.,0.,0.));
#60997=DIRECTION('',(0.137844537491629,-0.524860590029465,0.839952525157012));
#60998=DIRECTION('center_axis',(0.99026806874157,0.0894587448987839,-0.106612780622095));
#60999=DIRECTION('ref_axis',(0.,0.766044443118978,0.642787609686539));
#61000=DIRECTION('center_axis',(-0.99026806874157,-0.0894587448987839,0.106612780622095));
#61001=DIRECTION('ref_axis',(-0.139173100960065,0.636532044855303,-0.758589351257639));
#61002=DIRECTION('',(0.137998583506848,-0.531847935749546,0.835520295497991));
#61003=DIRECTION('center_axis',(0.0617712249622996,0.846570802931135,0.528679668032723));
#61004=DIRECTION('ref_axis',(-0.998052578482889,0.0477845394804615,0.0400959894540314));
#61005=DIRECTION('center_axis',(-0.0617712249622996,-0.846570802931135,
-0.528679668032723));
#61006=DIRECTION('ref_axis',(-0.998090334472114,0.0523937700909925,0.0327196743412163));
#61007=DIRECTION('',(-0.0161503784824054,-0.528774052761765,0.848608959651484));
#61008=DIRECTION('center_axis',(-0.284551435696759,0.816055565222214,0.50307434332588));
#61009=DIRECTION('ref_axis',(-0.957826285221151,-0.220121250980087,-0.184703660511673));
#61010=DIRECTION('center_axis',(0.284551435696759,-0.816055565222214,-0.50307434332588));
#61011=DIRECTION('ref_axis',(0.958660774436356,0.242223097976277,0.149323442110948));
#61012=DIRECTION('',(-0.0552259184163639,-0.537850200094025,0.841229612052433));
#61013=DIRECTION('center_axis',(-0.491310548314114,0.748098746816874,0.446051802065978));
#61014=DIRECTION('ref_axis',(-0.868243142124459,-0.380064476743201,-0.318911962258806));
#61015=DIRECTION('center_axis',(0.491310548314114,-0.748098746816874,-0.446051802065978));
#61016=DIRECTION('ref_axis',(0.870984468928858,0.421992375987731,0.25161178329511));
#61017=DIRECTION('',(-0.0570786439550532,-0.538677468419953,0.840576357876501));
#61018=DIRECTION('center_axis',(-0.313150259135956,0.809119792515883,0.497254539006069));
#61019=DIRECTION('ref_axis',(-0.948683298050513,-0.242244522917128,-0.203267289834478));
#61020=DIRECTION('center_axis',(0.313150259135956,-0.809119792515883,-0.497254539006069));
#61021=DIRECTION('ref_axis',(0.949703593340092,0.266794897350299,0.163962091791853));
#61022=DIRECTION('',(-0.0225789275220273,-0.529784168481124,0.847831897759644));
#61023=DIRECTION('center_axis',(0.,0.848048096156426,0.529919264233205));
#61024=DIRECTION('ref_axis',(-1.,0.,0.));
#61025=DIRECTION('',(-1.,0.,0.));
#61026=DIRECTION('',(0.0225789275220281,-0.529784168481124,0.847831897759644));
#61027=DIRECTION('center_axis',(0.313150259135957,0.809119792515883,0.497254539006068));
#61028=DIRECTION('ref_axis',(-0.948683298050513,0.242244522917128,0.203267289834479));
#61029=DIRECTION('center_axis',(-0.313150259135957,-0.809119792515883,-0.497254539006068));
#61030=DIRECTION('ref_axis',(-0.949703593340092,0.2667948973503,0.163962091791853));
#61031=DIRECTION('',(0.0570786439550534,-0.538677468419953,0.840576357876501));
#61032=DIRECTION('center_axis',(0.491310548314113,0.748098746816875,0.446051802065978));
#61033=DIRECTION('ref_axis',(-0.86824314212446,0.3800644767432,0.318911962258805));
#61034=DIRECTION('center_axis',(-0.491310548314113,-0.748098746816875,-0.446051802065978));
#61035=DIRECTION('ref_axis',(-0.870984468928858,0.421992375987729,0.25161178329511));
#61036=DIRECTION('',(0.0552259184163649,-0.537850200094026,0.841229612052432));
#61037=DIRECTION('center_axis',(0.284551435696759,0.816055565222214,0.50307434332588));
#61038=DIRECTION('ref_axis',(-0.957826285221151,0.220121250980087,0.184703660511672));
#61039=DIRECTION('center_axis',(-0.284551435696759,-0.816055565222214,-0.50307434332588));
#61040=DIRECTION('ref_axis',(-0.958660774436356,0.242223097976277,0.149323442110947));
#61041=DIRECTION('',(0.0161503784824051,-0.528774052761765,0.848608959651484));
#61042=DIRECTION('center_axis',(-0.0617712249622997,0.846570802931135,0.528679668032723));
#61043=DIRECTION('ref_axis',(-0.998052578482889,-0.0477845394804615,-0.0400959894540315));
#61044=DIRECTION('center_axis',(0.0617712249622997,-0.846570802931135,-0.528679668032723));
#61045=DIRECTION('ref_axis',(0.998090334472114,0.0523937700909926,0.0327196743412163));
#61046=DIRECTION('',(-0.137998583506848,-0.531847935749546,0.835520295497991));
#61047=DIRECTION('center_axis',(-0.99026806874157,0.0894587448987841,-0.106612780622095));
#61048=DIRECTION('ref_axis',(0.,-0.766044443118978,-0.642787609686539));
#61049=DIRECTION('center_axis',(0.99026806874157,-0.0894587448987841,0.106612780622095));
#61050=DIRECTION('ref_axis',(0.139173100960066,0.636532044855299,-0.758589351257642));
#61051=DIRECTION('',(-0.137844537491629,-0.524860590029465,0.839952525157012));
#61052=DIRECTION('center_axis',(0.,0.848048096156426,0.529919264233205));
#61053=DIRECTION('ref_axis',(-1.,0.,0.));
#61054=DIRECTION('',(-1.,0.,0.));
#61055=DIRECTION('center_axis',(0.,-0.642787609686539,0.766044443118978));
#61056=DIRECTION('ref_axis',(1.,0.,0.));
#61057=DIRECTION('center_axis',(1.,0.,0.));
#61058=DIRECTION('ref_axis',(0.,1.,0.));
#61059=DIRECTION('center_axis',(1.,0.,0.));
#61060=DIRECTION('ref_axis',(0.,0.,-1.));
#61061=DIRECTION('center_axis',(0.64930555798837,0.577927816349714,0.494370034948177));
#61062=DIRECTION('ref_axis',(-0.760527640763576,0.49340973708095,0.422071722564183));
#61063=DIRECTION('',(1.,0.,0.));
#61064=DIRECTION('center_axis',(-0.99026806874157,-0.0695865504800327,0.120527440954873));
#61065=DIRECTION('ref_axis',(-0.139173100960065,0.495134034370783,-0.857597304086756));
#61066=DIRECTION('center_axis',(-0.0617712249622996,0.786340650163727,0.61469724065327));
#61067=DIRECTION('ref_axis',(0.998090334472114,0.0486661612888524,0.0380432514219071));
#61068=DIRECTION('center_axis',(0.284551435696759,0.751842689509058,0.594779833782804));
#61069=DIRECTION('ref_axis',(-0.958660774436356,0.223163315348643,0.176543632679541));
#61070=DIRECTION('center_axis',(0.491310548314114,0.675016427497717,0.550424170729724));
#61071=DIRECTION('ref_axis',(-0.870984468928858,0.380767628982861,0.310486823558562));
#61072=DIRECTION('center_axis',(0.313150259135956,0.744001688360219,0.590252829658806));
#61073=DIRECTION('ref_axis',(-0.949703593340092,0.245323196775732,0.194626858168784));
#61074=DIRECTION('',(1.,0.,0.));
#61075=DIRECTION('center_axis',(-0.313150259135957,0.744001688360219,0.590252829658806));
#61076=DIRECTION('ref_axis',(0.949703593340092,0.245323196775733,0.194626858168784));
#61077=DIRECTION('center_axis',(-0.491310548314113,0.675016427497717,0.550424170729724));
#61078=DIRECTION('ref_axis',(0.870984468928858,0.38076762898286,0.310486823558561));
#61079=DIRECTION('center_axis',(-0.284551435696759,0.751842689509058,0.594779833782804));
#61080=DIRECTION('ref_axis',(0.958660774436356,0.223163315348643,0.176543632679541));
#61081=DIRECTION('center_axis',(0.0617712249622997,0.786340650163727,0.61469724065327));
#61082=DIRECTION('ref_axis',(-0.998090334472114,0.0486661612888524,0.0380432514219071));
#61083=DIRECTION('center_axis',(0.99026806874157,-0.0695865504800328,0.120527440954873));
#61084=DIRECTION('ref_axis',(0.139173100960066,0.495134034370784,-0.857597304086755));
#61085=DIRECTION('',(1.,0.,0.));
#61086=DIRECTION('center_axis',(0.,-0.788010753606722,-0.615661475325658));
#61087=DIRECTION('ref_axis',(1.,0.,0.));
#61088=DIRECTION('',(-0.137844537491629,-0.609784295472661,0.780488306432985));
#61089=DIRECTION('center_axis',(-0.99026806874157,0.0695865504800328,-0.120527440954873));
#61090=DIRECTION('ref_axis',(0.,-0.866025403784439,-0.5));
#61091=DIRECTION('',(-0.137998583506848,-0.603229548983802,0.785538351821795));
#61092=DIRECTION('center_axis',(-0.0617712249622997,-0.786340650163727,
-0.61469724065327));
#61093=DIRECTION('ref_axis',(0.998052578482889,-0.0540211804549215,-0.0311891430775903));
#61094=DIRECTION('',(0.0161503784824051,-0.616580200004832,0.787126433450736));
#61095=DIRECTION('center_axis',(0.284551435696759,-0.751842689509058,-0.594779833782804));
#61096=DIRECTION('ref_axis',(0.957826285221151,0.248850568624199,0.143673942783173));
#61097=DIRECTION('',(0.0552259184163645,-0.606541656308365,0.79313133660055));
#61098=DIRECTION('center_axis',(0.491310548314113,-0.675016427497717,-0.550424170729724));
#61099=DIRECTION('ref_axis',(0.86824314212446,0.429668924423658,0.248069469178416));
#61100=DIRECTION('',(0.057078643955053,-0.605644855748342,0.793685288454953));
#61101=DIRECTION('center_axis',(0.313150259135957,-0.744001688360219,-0.590252829658806));
#61102=DIRECTION('ref_axis',(0.948683298050513,0.273861278752585,0.15811388300842));
#61103=DIRECTION('',(0.0225789275220278,-0.615504520756066,0.787809860918738));
#61104=DIRECTION('center_axis',(0.,-0.788010753606722,-0.615661475325658));
#61105=DIRECTION('ref_axis',(1.,0.,0.));
#61106=DIRECTION('',(-0.0225789275220274,-0.615504520756066,0.787809860918738));
#61107=DIRECTION('center_axis',(-0.313150259135956,-0.744001688360219,-0.590252829658806));
#61108=DIRECTION('ref_axis',(0.948683298050513,-0.273861278752584,-0.158113883008419));
#61109=DIRECTION('',(-0.0570786439550527,-0.605644855748342,0.793685288454953));
#61110=DIRECTION('center_axis',(-0.491310548314114,-0.675016427497717,-0.550424170729724));
#61111=DIRECTION('ref_axis',(0.868243142124459,-0.429668924423659,-0.248069469178417));
#61112=DIRECTION('',(-0.0552259184163635,-0.606541656308365,0.79313133660055));
#61113=DIRECTION('center_axis',(-0.284551435696759,-0.751842689509058,-0.594779833782804));
#61114=DIRECTION('ref_axis',(0.957826285221151,-0.248850568624199,-0.143673942783173));
#61115=DIRECTION('',(-0.0161503784824052,-0.616580200004832,0.787126433450736));
#61116=DIRECTION('center_axis',(0.0617712249622996,-0.786340650163727,-0.61469724065327));
#61117=DIRECTION('ref_axis',(0.998052578482889,0.0540211804549215,0.0311891430775902));
#61118=DIRECTION('',(0.137998583506848,-0.603229548983803,0.785538351821795));
#61119=DIRECTION('center_axis',(0.99026806874157,0.0695865504800327,-0.120527440954873));
#61120=DIRECTION('ref_axis',(0.,0.866025403784439,0.5));
#61121=DIRECTION('',(0.137844537491629,-0.609784295472661,0.780488306432985));
#61122=DIRECTION('center_axis',(0.,-0.788010753606722,-0.615661475325658));
#61123=DIRECTION('ref_axis',(1.,0.,0.));
#61124=DIRECTION('',(-0.0519254248777279,-0.614830926556977,0.786947699660121));
#61125=DIRECTION('center_axis',(-0.64930555798837,-0.577927816349714,-0.494370034948177));
#61126=DIRECTION('ref_axis',(0.755033118392644,-0.567841300538901,-0.327843327723121));
#61127=DIRECTION('center_axis',(0.,0.927183854566788,0.374606593415912));
#61128=DIRECTION('ref_axis',(-1.,0.,0.));
#61129=DIRECTION('',(-1.,0.,0.));
#61130=DIRECTION('',(0.137844537491629,-0.371030552991328,0.918332843924614));
#61131=DIRECTION('center_axis',(0.99026806874157,0.0695865504800327,-0.120527440954873));
#61132=DIRECTION('ref_axis',(0.,0.866025403784439,0.5));
#61133=DIRECTION('center_axis',(-0.99026806874157,-0.0695865504800327,0.120527440954873));
#61134=DIRECTION('ref_axis',(-0.139173100960065,0.495134034370783,-0.857597304086756));
#61135=DIRECTION('',(0.137998583506848,-0.378681393832731,0.9151812896443));
#61136=DIRECTION('center_axis',(0.0617712249622996,0.925513751123792,0.373642358743524));
#61137=DIRECTION('ref_axis',(-0.998052578482889,0.0540211804549215,0.0311891430775902));
#61138=DIRECTION('center_axis',(-0.0617712249622996,-0.925513751123792,
-0.373642358743524));
#61139=DIRECTION('ref_axis',(-0.998090334472114,0.0572795028183562,0.0231245062698634));
#61140=DIRECTION('',(-0.0161503784824054,-0.373381387356162,0.927537333400043));
#61141=DIRECTION('center_axis',(-0.284551435696759,0.891015790469123,0.353724951873058));
#61142=DIRECTION('ref_axis',(-0.957826285221151,-0.248850568624199,-0.143673942783173));
#61143=DIRECTION('center_axis',(0.284551435696759,-0.891015790469123,-0.353724951873058));
#61144=DIRECTION('ref_axis',(0.958660774436356,0.264472928451193,0.104993283944912));
#61145=DIRECTION('',(-0.0552259184163638,-0.3836010578794,0.921846151116809));
#61146=DIRECTION('center_axis',(-0.491310548314114,0.814189528457782,0.309369288819977));
#61147=DIRECTION('ref_axis',(-0.868243142124459,-0.429668924423659,-0.248069469178417));
#61148=DIRECTION('center_axis',(0.491310548314114,-0.814189528457782,-0.309369288819977));
#61149=DIRECTION('ref_axis',(0.870984468928858,0.459273291233482,0.174511027858645));
#61150=DIRECTION('',(-0.0570786439550532,-0.384529194537798,0.921346474976903));
#61151=DIRECTION('center_axis',(-0.313150259135956,0.883174789320284,0.34919794774906));
#61152=DIRECTION('ref_axis',(-0.948683298050513,-0.273861278752584,-0.158113883008419));
#61153=DIRECTION('center_axis',(0.313150259135956,-0.883174789320284,-0.34919794774906));
#61154=DIRECTION('ref_axis',(0.949703593340092,0.291213401820784,0.115142691461001));
#61155=DIRECTION('',(-0.0225789275220273,-0.374511092529479,0.926947481578288));
#61156=DIRECTION('center_axis',(0.,0.927183854566788,0.374606593415912));
#61157=DIRECTION('ref_axis',(-1.,0.,0.));
#61158=DIRECTION('',(-1.,0.,0.));
#61159=DIRECTION('',(0.0225789275220281,-0.374511092529479,0.926947481578288));
#61160=DIRECTION('center_axis',(0.313150259135957,0.883174789320284,0.349197947749059));
#61161=DIRECTION('ref_axis',(-0.948683298050513,0.273861278752585,0.15811388300842));
#61162=DIRECTION('center_axis',(-0.313150259135957,-0.883174789320284,-0.349197947749059));
#61163=DIRECTION('ref_axis',(-0.949703593340092,0.291213401820785,0.115142691461001));
#61164=DIRECTION('',(0.0570786439550533,-0.384529194537798,0.921346474976903));
#61165=DIRECTION('center_axis',(0.491310548314113,0.814189528457783,0.309369288819977));
#61166=DIRECTION('ref_axis',(-0.86824314212446,0.429668924423658,0.248069469178416));
#61167=DIRECTION('center_axis',(-0.491310548314113,-0.814189528457783,-0.309369288819977));
#61168=DIRECTION('ref_axis',(-0.870984468928858,0.459273291233481,0.174511027858644));
#61169=DIRECTION('',(0.0552259184163649,-0.3836010578794,0.921846151116809));
#61170=DIRECTION('center_axis',(0.284551435696759,0.891015790469123,0.353724951873058));
#61171=DIRECTION('ref_axis',(-0.957826285221151,0.248850568624199,0.143673942783173));
#61172=DIRECTION('center_axis',(-0.284551435696759,-0.891015790469123,-0.353724951873058));
#61173=DIRECTION('ref_axis',(-0.958660774436356,0.264472928451193,0.104993283944912));
#61174=DIRECTION('',(0.016150378482405,-0.373381387356162,0.927537333400043));
#61175=DIRECTION('center_axis',(-0.0617712249622997,0.925513751123792,0.373642358743524));
#61176=DIRECTION('ref_axis',(-0.998052578482889,-0.0540211804549215,-0.0311891430775903));
#61177=DIRECTION('center_axis',(0.0617712249622997,-0.925513751123792,-0.373642358743524));
#61178=DIRECTION('ref_axis',(0.998090334472114,0.0572795028183563,0.0231245062698634));
#61179=DIRECTION('',(-0.137998583506848,-0.378681393832731,0.9151812896443));
#61180=DIRECTION('center_axis',(-0.99026806874157,0.0695865504800328,-0.120527440954873));
#61181=DIRECTION('ref_axis',(0.,-0.866025403784439,-0.5));
#61182=DIRECTION('center_axis',(0.99026806874157,-0.0695865504800328,0.120527440954873));
#61183=DIRECTION('ref_axis',(0.139173100960066,0.495134034370784,-0.857597304086755));
#61184=DIRECTION('',(-0.137844537491629,-0.371030552991328,0.918332843924614));
#61185=DIRECTION('center_axis',(0.,0.927183854566788,0.374606593415912));
#61186=DIRECTION('ref_axis',(-1.,0.,0.));
#61187=DIRECTION('',(-1.,0.,0.));
#61188=DIRECTION('center_axis',(0.,-0.5,0.866025403784439));
#61189=DIRECTION('ref_axis',(1.,0.,0.));
#61190=DIRECTION('center_axis',(1.,0.,0.));
#61191=DIRECTION('ref_axis',(0.,1.,0.));
#61192=DIRECTION('center_axis',(1.,0.,0.));
#61193=DIRECTION('ref_axis',(0.,0.,-1.));
#61194=DIRECTION('center_axis',(0.649305557988371,0.654994249884502,0.386503331141725));
#61195=DIRECTION('ref_axis',(-0.760527640763576,0.559205719957048,0.329979803021199));
#61196=DIRECTION('',(1.,0.,0.));
#61197=DIRECTION('center_axis',(-0.99026806874157,-0.0476000039374393,0.130779935984066));
#61198=DIRECTION('ref_axis',(-0.139173100960065,0.338691626801824,-0.930547596796367));
#61199=DIRECTION('center_axis',(-0.0617712249622996,0.881135424446229,0.468811987424192));
#61200=DIRECTION('ref_axis',(0.998090334472114,0.0545329542285434,0.0290144987282327));
#61201=DIRECTION('center_axis',(0.284551435696759,0.843702943923494,0.455187678719166));
#61202=DIRECTION('ref_axis',(-0.958660774436356,0.250429443236754,0.135109635175349));
#61203=DIRECTION('center_axis',(0.491310548314114,0.760341565401402,0.424846618249727));
#61204=DIRECTION('ref_axis',(-0.870984468928858,0.428898384218936,0.239650226161174));
#61205=DIRECTION('center_axis',(0.313150259135956,0.835194959184317,0.452091025520515));
#61206=DIRECTION('ref_axis',(-0.949703593340092,0.27539278542453,0.149070112809494));
#61207=DIRECTION('',(1.,0.,0.));
#61208=DIRECTION('center_axis',(-0.313150259135957,0.835194959184317,0.452091025520515));
#61209=DIRECTION('ref_axis',(0.949703593340092,0.275392785424531,0.149070112809494));
#61210=DIRECTION('center_axis',(-0.491310548314113,0.760341565401403,0.424846618249727));
#61211=DIRECTION('ref_axis',(0.870984468928858,0.428898384218935,0.239650226161173));
#61212=DIRECTION('center_axis',(-0.284551435696759,0.843702943923494,0.455187678719166));
#61213=DIRECTION('ref_axis',(0.958660774436356,0.250429443236754,0.135109635175349));
#61214=DIRECTION('center_axis',(0.0617712249622997,0.881135424446229,0.468811987424191));
#61215=DIRECTION('ref_axis',(-0.998090334472114,0.0545329542285435,0.0290144987282327));
#61216=DIRECTION('center_axis',(0.99026806874157,-0.0476000039374394,0.130779935984066));
#61217=DIRECTION('ref_axis',(0.139173100960066,0.338691626801825,-0.930547596796366));
#61218=DIRECTION('',(1.,0.,0.));
#61219=DIRECTION('center_axis',(0.,-0.882947592858927,-0.469471562785891));
#61220=DIRECTION('ref_axis',(1.,0.,0.));
#61221=DIRECTION('',(-0.137844537491629,-0.464989929744128,0.874518866989312));
#61222=DIRECTION('center_axis',(-0.99026806874157,0.0476000039374394,-0.130779935984066));
#61223=DIRECTION('ref_axis',(0.,-0.939692620785908,-0.342020143325669));
#61224=DIRECTION('',(-0.137998583506848,-0.457657833403968,0.878353971058417));
#61225=DIRECTION('center_axis',(-0.0617712249622997,-0.881135424446229,
-0.468811987424191));
#61226=DIRECTION('ref_axis',(0.998052578482889,-0.058616415197295,-0.0213346303712044));
#61227=DIRECTION('',(0.0161503784824051,-0.470529890556386,0.882236242379483));
#61228=DIRECTION('center_axis',(0.284551435696759,-0.843702943923494,-0.455187678719166));
#61229=DIRECTION('ref_axis',(0.957826285221151,0.270018687665128,0.0982787650057293));
#61230=DIRECTION('',(0.0552259184163645,-0.459601114406122,0.886406742738186));
#61231=DIRECTION('center_axis',(0.491310548314113,-0.760341565401403,-0.424846618249727));
#61232=DIRECTION('ref_axis',(0.86824314212446,0.46621809925847,0.169689510806249));
#61233=DIRECTION('',(0.057078643955053,-0.458621745531673,0.886796551036219));
#61234=DIRECTION('center_axis',(0.313150259135957,-0.835194959184317,-0.452091025520515));
#61235=DIRECTION('ref_axis',(0.948683298050513,0.297156898213637,0.108156265856636));
#61236=DIRECTION('',(0.0225789275220278,-0.469351877358061,0.88272249730729));
#61237=DIRECTION('center_axis',(0.,-0.882947592858927,-0.469471562785891));
#61238=DIRECTION('ref_axis',(1.,0.,0.));
#61239=DIRECTION('',(-0.0225789275220274,-0.469351877358061,0.88272249730729));
#61240=DIRECTION('center_axis',(-0.313150259135956,-0.835194959184317,-0.452091025520515));
#61241=DIRECTION('ref_axis',(0.948683298050514,-0.297156898213636,-0.108156265856635));
#61242=DIRECTION('',(-0.0570786439550527,-0.458621745531673,0.886796551036219));
#61243=DIRECTION('center_axis',(-0.491310548314114,-0.760341565401402,-0.424846618249727));
#61244=DIRECTION('ref_axis',(0.868243142124459,-0.466218099258471,-0.169689510806249));
#61245=DIRECTION('',(-0.0552259184163635,-0.459601114406122,0.886406742738186));
#61246=DIRECTION('center_axis',(-0.284551435696759,-0.843702943923494,-0.455187678719166));
#61247=DIRECTION('ref_axis',(0.957826285221151,-0.270018687665129,-0.0982787650057295));
#61248=DIRECTION('',(-0.0161503784824052,-0.470529890556386,0.882236242379483));
#61249=DIRECTION('center_axis',(0.0617712249622996,-0.881135424446229,-0.468811987424192));
#61250=DIRECTION('ref_axis',(0.998052578482889,0.0586164151972949,0.0213346303712044));
#61251=DIRECTION('',(0.137998583506848,-0.457657833403968,0.878353971058417));
#61252=DIRECTION('center_axis',(0.99026806874157,0.0476000039374393,-0.130779935984066));
#61253=DIRECTION('ref_axis',(0.,0.939692620785908,0.342020143325669));
#61254=DIRECTION('',(0.137844537491629,-0.464989929744127,0.874518866989312));
#61255=DIRECTION('center_axis',(0.,-0.882947592858927,-0.469471562785891));
#61256=DIRECTION('ref_axis',(1.,0.,0.));
#61257=DIRECTION('',(-0.0519254248777279,-0.468838229299828,0.881756465810299));
#61258=DIRECTION('center_axis',(-0.649305557988371,-0.654994249884502,-0.386503331141725));
#61259=DIRECTION('ref_axis',(0.755033118392644,-0.616143911670627,-0.224258043872452));
#61260=DIRECTION('center_axis',(0.,0.978147600733806,0.207911690817759));
#61261=DIRECTION('ref_axis',(-1.,0.,0.));
#61262=DIRECTION('',(-1.,0.,0.));
#61263=DIRECTION('',(0.137844537491629,-0.205926940351068,0.968810083928407));
#61264=DIRECTION('center_axis',(0.99026806874157,0.0476000039374393,-0.130779935984066));
#61265=DIRECTION('ref_axis',(0.,0.939692620785908,0.342020143325669));
#61266=DIRECTION('center_axis',(-0.99026806874157,-0.0476000039374393,0.130779935984066));
#61267=DIRECTION('ref_axis',(-0.139173100960065,0.338691626801824,-0.930547596796367));
#61268=DIRECTION('',(0.137998583506848,-0.214008809386339,0.967034963408845));
#61269=DIRECTION('center_axis',(0.0617712249622996,0.976335432321108,0.20725211545606));
#61270=DIRECTION('ref_axis',(-0.998052578482889,0.0586164151972949,0.0213346303712044));
#61271=DIRECTION('center_axis',(-0.0617712249622996,-0.976335432321108,
-0.20725211545606));
#61272=DIRECTION('ref_axis',(-0.998090334472114,0.0604248268374111,0.0128267117770656));
#61273=DIRECTION('',(-0.0161503784824054,-0.206643717435842,0.978282954629779));
#61274=DIRECTION('center_axis',(-0.284551435696759,0.938902951798373,0.193627806751035));
#61275=DIRECTION('ref_axis',(-0.957826285221151,-0.270018687665129,-0.0982787650057295));
#61276=DIRECTION('center_axis',(0.284551435696759,-0.938902951798373,-0.193627806751035));
#61277=DIRECTION('ref_axis',(0.958660774436356,0.278686882824878,0.0574729579753755));
#61278=DIRECTION('',(-0.0552259184163638,-0.21769639163261,0.974452861356161));
#61279=DIRECTION('center_axis',(-0.491310548314114,0.855541573276281,0.163286746281596));
#61280=DIRECTION('ref_axis',(-0.868243142124459,-0.466218099258471,-0.169689510806249));
#61281=DIRECTION('center_axis',(0.491310548314114,-0.855541573276281,-0.163286746281596));
#61282=DIRECTION('ref_axis',(0.870984468928858,0.482599419928604,0.0921078431475351));
#61283=DIRECTION('',(-0.0570786439550532,-0.218697195660774,0.974121945658943));
#61284=DIRECTION('center_axis',(-0.313150259135956,0.930394967059196,0.190531153552383));
#61285=DIRECTION('ref_axis',(-0.948683298050514,-0.297156898213636,-0.108156265856635));
#61286=DIRECTION('center_axis',(0.313150259135956,-0.930394967059196,-0.190531153552383));
#61287=DIRECTION('ref_axis',(0.949703593340092,0.306783534438035,0.0628247387151196));
#61288=DIRECTION('',(-0.0225789275220273,-0.207858686543083,0.977898235227234));
#61289=DIRECTION('center_axis',(0.,0.978147600733806,0.207911690817759));
#61290=DIRECTION('ref_axis',(-1.,0.,0.));
#61291=DIRECTION('',(-1.,0.,0.));
#61292=DIRECTION('',(0.0225789275220281,-0.207858686543083,0.977898235227234));
#61293=DIRECTION('center_axis',(0.313150259135957,0.930394967059195,0.190531153552383));
#61294=DIRECTION('ref_axis',(-0.948683298050513,0.297156898213637,0.108156265856636));
#61295=DIRECTION('center_axis',(-0.313150259135957,-0.930394967059195,-0.190531153552383));
#61296=DIRECTION('ref_axis',(-0.949703593340092,0.306783534438037,0.0628247387151197));
#61297=DIRECTION('',(0.0570786439550534,-0.218697195660774,0.974121945658943));
#61298=DIRECTION('center_axis',(0.491310548314113,0.855541573276282,0.163286746281596));
#61299=DIRECTION('ref_axis',(-0.86824314212446,0.46621809925847,0.169689510806249));
#61300=DIRECTION('center_axis',(-0.491310548314113,-0.855541573276282,-0.163286746281596));
#61301=DIRECTION('ref_axis',(-0.870984468928858,0.482599419928602,0.0921078431475348));
#61302=DIRECTION('',(0.0552259184163649,-0.21769639163261,0.974452861356161));
#61303=DIRECTION('center_axis',(0.284551435696759,0.938902951798373,0.193627806751035));
#61304=DIRECTION('ref_axis',(-0.957826285221151,0.270018687665128,0.0982787650057293));
#61305=DIRECTION('center_axis',(-0.284551435696759,-0.938902951798373,-0.193627806751035));
#61306=DIRECTION('ref_axis',(-0.958660774436356,0.278686882824878,0.0574729579753754));
#61307=DIRECTION('',(0.0161503784824051,-0.206643717435842,0.978282954629779));
#61308=DIRECTION('center_axis',(-0.0617712249622997,0.976335432321108,0.20725211545606));
#61309=DIRECTION('ref_axis',(-0.998052578482889,-0.058616415197295,-0.0213346303712044));
#61310=DIRECTION('center_axis',(0.0617712249622997,-0.976335432321108,-0.20725211545606));
#61311=DIRECTION('ref_axis',(0.998090334472114,0.0604248268374111,0.0128267117770656));
#61312=DIRECTION('',(-0.137998583506848,-0.214008809386339,0.967034963408845));
#61313=DIRECTION('center_axis',(-0.99026806874157,0.0476000039374394,-0.130779935984066));
#61314=DIRECTION('ref_axis',(0.,-0.939692620785908,-0.342020143325669));
#61315=DIRECTION('center_axis',(0.99026806874157,-0.0476000039374394,0.130779935984066));
#61316=DIRECTION('ref_axis',(0.139173100960066,0.338691626801825,-0.930547596796366));
#61317=DIRECTION('',(-0.137844537491629,-0.205926940351068,0.968810083928407));
#61318=DIRECTION('center_axis',(0.,0.978147600733806,0.207911690817759));
#61319=DIRECTION('ref_axis',(-1.,0.,0.));
#61320=DIRECTION('',(-1.,0.,0.));
#61321=DIRECTION('center_axis',(0.,-0.342020143325669,0.939692620785908));
#61322=DIRECTION('ref_axis',(1.,0.,0.));
#61323=DIRECTION('center_axis',(1.,0.,0.));
#61324=DIRECTION('ref_axis',(0.,1.,0.));
#61325=DIRECTION('center_axis',(1.,0.,0.));
#61326=DIRECTION('ref_axis',(0.,0.,-1.));
#61327=DIRECTION('center_axis',(0.64930555798837,0.712159014579631,0.266892919198654));
#61328=DIRECTION('ref_axis',(-0.760527640763576,0.608010520003998,0.227861614141253));
#61329=DIRECTION('',(1.,0.,0.));
#61330=DIRECTION('center_axis',(-0.99026806874157,-0.0241671553619711,0.137058748836223));
#61331=DIRECTION('ref_axis',(-0.139173100960065,0.171958245538723,-0.975223671657125));
#61332=DIRECTION('center_axis',(-0.0617712249622996,0.949157344732972,0.308682119187541));
#61333=DIRECTION('ref_axis',(0.998090334472114,0.0587427909490065,0.0191041551727457));
#61334=DIRECTION('center_axis',(0.284551435696759,0.909927711321104,0.301764876373726));
#61335=DIRECTION('ref_axis',(-0.958660774436356,0.27008639921553,0.0895703997751286));
#61336=DIRECTION('center_axis',(0.491310548314114,0.822564109591763,0.286360316256974));
#61337=DIRECTION('ref_axis',(-0.870984468928858,0.463997279083573,0.161531977910744));
#61338=DIRECTION('center_axis',(0.313150259135956,0.901011253802641,0.30019266434088));
#61339=DIRECTION('ref_axis',(-0.949703593340092,0.297094703643677,0.0989839475056044));
#61340=DIRECTION('',(1.,0.,0.));
#61341=DIRECTION('center_axis',(-0.313150259135957,0.901011253802641,0.30019266434088));
#61342=DIRECTION('ref_axis',(0.949703593340092,0.297094703643678,0.0989839475056048));
#61343=DIRECTION('center_axis',(-0.491310548314113,0.822564109591764,0.286360316256975));
#61344=DIRECTION('ref_axis',(0.870984468928858,0.463997279083571,0.161531977910744));
#61345=DIRECTION('center_axis',(-0.284551435696759,0.909927711321105,0.301764876373726));
#61346=DIRECTION('ref_axis',(0.958660774436356,0.270086399215529,0.0895703997751284));
#61347=DIRECTION('center_axis',(0.0617712249622997,0.949157344732972,0.308682119187541));
#61348=DIRECTION('ref_axis',(-0.998090334472114,0.0587427909490066,0.0191041551727457));
#61349=DIRECTION('center_axis',(0.99026806874157,-0.0241671553619711,0.137058748836224));
#61350=DIRECTION('ref_axis',(0.139173100960066,0.171958245538724,-0.975223671657125));
#61351=DIRECTION('',(1.,0.,0.));
#61352=DIRECTION('center_axis',(0.,-0.951056516295154,-0.309016994374948));
#61353=DIRECTION('ref_axis',(1.,0.,0.));
#61354=DIRECTION('',(-0.137844537491629,-0.306067080296576,0.941977614300068));
#61355=DIRECTION('center_axis',(-0.99026806874157,0.0241671553619711,-0.137058748836224));
#61356=DIRECTION('ref_axis',(0.,-0.984807753012208,-0.17364817766693));
#61357=DIRECTION('',(-0.137998583506848,-0.298180416142191,0.944481249352984));
#61358=DIRECTION('center_axis',(-0.0617712249622997,-0.949157344732972,
-0.308682119187541));
#61359=DIRECTION('ref_axis',(0.998052578482889,-0.0614306198252359,-0.0108318757168334));
#61360=DIRECTION('',(0.0161503784824051,-0.310182768482997,0.950539749516609));
#61361=DIRECTION('center_axis',(0.284551435696759,-0.909927711321105,-0.301764876373726));
#61362=DIRECTION('ref_axis',(0.957826285221151,0.282982425517402,0.0498974366850415));
#61363=DIRECTION('',(0.0552259184163645,-0.298695825212034,0.952749128541176));
#61364=DIRECTION('center_axis',(0.491310548314113,-0.822564109591764,-0.286360316256975));
#61365=DIRECTION('ref_axis',(0.86824314212446,0.488601473065054,0.0861536225152694));
#61366=DIRECTION('',(0.057078643955053,-0.297663645650825,0.952962949154956));
#61367=DIRECTION('center_axis',(0.313150259135957,-0.901011253802641,-0.30019266434088));
#61368=DIRECTION('ref_axis',(0.948683298050513,0.311423555691114,0.0549123752965087));
#61369=DIRECTION('',(0.0225789275220278,-0.30893821467004,0.950814057294297));
#61370=DIRECTION('center_axis',(0.,-0.951056516295154,-0.309016994374947));
#61371=DIRECTION('ref_axis',(1.,0.,0.));
#61372=DIRECTION('',(-0.0225789275220274,-0.30893821467004,0.950814057294297));
#61373=DIRECTION('center_axis',(-0.313150259135956,-0.901011253802641,-0.30019266434088));
#61374=DIRECTION('ref_axis',(0.948683298050514,-0.311423555691113,-0.0549123752965085));
#61375=DIRECTION('',(-0.0570786439550527,-0.297663645650826,0.952962949154956));
#61376=DIRECTION('center_axis',(-0.491310548314114,-0.822564109591763,-0.286360316256974));
#61377=DIRECTION('ref_axis',(0.868243142124459,-0.488601473065055,-0.0861536225152696));
#61378=DIRECTION('',(-0.0552259184163635,-0.298695825212034,0.952749128541176));
#61379=DIRECTION('center_axis',(-0.284551435696759,-0.909927711321104,-0.301764876373726));
#61380=DIRECTION('ref_axis',(0.957826285221151,-0.282982425517402,-0.0498974366850416));
#61381=DIRECTION('',(-0.0161503784824052,-0.310182768482997,0.950539749516609));
#61382=DIRECTION('center_axis',(0.0617712249622996,-0.949157344732972,-0.308682119187541));
#61383=DIRECTION('ref_axis',(0.998052578482889,0.0614306198252359,0.0108318757168334));
#61384=DIRECTION('',(0.137998583506848,-0.298180416142191,0.944481249352984));
#61385=DIRECTION('center_axis',(0.99026806874157,0.0241671553619711,-0.137058748836223));
#61386=DIRECTION('ref_axis',(0.,0.984807753012208,0.17364817766693));
#61387=DIRECTION('',(0.137844537491629,-0.306067080296576,0.941977614300068));
#61388=DIRECTION('center_axis',(0.,-0.951056516295154,-0.309016994374947));
#61389=DIRECTION('ref_axis',(1.,0.,0.));
#61390=DIRECTION('',(-0.0519254248777279,-0.308600119688995,0.949773507937132));
#61391=DIRECTION('center_axis',(-0.64930555798837,-0.712159014579631,-0.266892919198654));
#61392=DIRECTION('ref_axis',(0.755033118392644,-0.645725301830105,-0.113858792838765));
#61393=DIRECTION('center_axis',(0.,0.999390827019096,0.034899496702501));
#61394=DIRECTION('ref_axis',(-1.,0.,0.));
#61395=DIRECTION('',(-1.,0.,0.));
#61396=DIRECTION('',(0.137844537491629,-0.0345663418323003,0.989850519773593));
#61397=DIRECTION('center_axis',(0.99026806874157,0.0241671553619711,-0.137058748836223));
#61398=DIRECTION('ref_axis',(0.,0.984807753012208,0.17364817766693));
#61399=DIRECTION('center_axis',(-0.99026806874157,-0.0241671553619711,0.137058748836223));
#61400=DIRECTION('ref_axis',(-0.139173100960065,0.171958245538723,-0.975223671657125));
#61401=DIRECTION('',(0.137998583506848,-0.0428336755604258,0.989505769153514));
#61402=DIRECTION('center_axis',(0.0617712249622996,0.997491655456914,0.0345646215150941));
#61403=DIRECTION('ref_axis',(-0.998052578482889,0.0614306198252359,0.0108318757168334));
#61404=DIRECTION('center_axis',(-0.0617712249622996,-0.997491655456914,
-0.0345646215150941));
#61405=DIRECTION('ref_axis',(-0.998090334472114,0.061734173069449,0.0021391841375509));
#61406=DIRECTION('',(-0.0161503784824054,-0.0336272827279996,0.999303943318151));
#61407=DIRECTION('center_axis',(-0.284551435696759,0.958262022045047,0.0276473787012795));
#61408=DIRECTION('ref_axis',(-0.957826285221151,-0.282982425517402,-0.0498974366850416));
#61409=DIRECTION('center_axis',(0.284551435696759,-0.958262022045047,-0.0276473787012795));
#61410=DIRECTION('ref_axis',(0.958660774436356,0.284433077286297,0.00820634526047707));
#61411=DIRECTION('',(-0.0552259184163638,-0.045177130685753,0.997451314500147));
#61412=DIRECTION('center_axis',(-0.491310548314114,0.870898420315705,0.0122428185845279));
#61413=DIRECTION('ref_axis',(-0.868243142124459,-0.488601473065055,-0.0861536225152696));
#61414=DIRECTION('center_axis',(0.491310548314114,-0.870898420315705,-0.0122428185845279));
#61415=DIRECTION('ref_axis',(0.870984468928858,0.491262009456284,0.00690600823120527));
#61416=DIRECTION('',(-0.0570786439550532,-0.0462201931597182,0.997299213951626));
#61417=DIRECTION('center_axis',(-0.313150259135956,0.949345564526583,0.0260751666684337));
#61418=DIRECTION('ref_axis',(-0.948683298050514,-0.311423555691113,-0.0549123752965085));
#61419=DIRECTION('center_axis',(0.313150259135956,-0.949345564526583,-0.0260751666684337));
#61420=DIRECTION('ref_axis',(0.949703593340092,0.313032204601347,0.00859788807423115));
#61421=DIRECTION('',(-0.0225789275220273,-0.0348905995476465,0.999136045839184));
#61422=DIRECTION('center_axis',(0.,0.999390827019096,0.034899496702501));
#61423=DIRECTION('ref_axis',(-1.,0.,0.));
#61424=DIRECTION('',(-1.,0.,0.));
#61425=DIRECTION('',(0.0225789275220281,-0.0348905995476465,0.999136045839184));
#61426=DIRECTION('center_axis',(0.313150259135957,0.949345564526583,0.0260751666684334));
#61427=DIRECTION('ref_axis',(-0.948683298050513,0.311423555691114,0.0549123752965087));
#61428=DIRECTION('center_axis',(-0.313150259135957,-0.949345564526583,-0.0260751666684334));
#61429=DIRECTION('ref_axis',(-0.949703593340092,0.313032204601348,0.0085978880742311));
#61430=DIRECTION('',(0.0570786439550533,-0.0462201931597181,0.997299213951626));
#61431=DIRECTION('center_axis',(0.491310548314113,0.870898420315706,0.0122428185845278));
#61432=DIRECTION('ref_axis',(-0.86824314212446,0.488601473065054,0.0861536225152694));
#61433=DIRECTION('center_axis',(-0.491310548314113,-0.870898420315706,-0.0122428185845278));
#61434=DIRECTION('ref_axis',(-0.870984468928858,0.491262009456283,0.0069060082312052));
#61435=DIRECTION('',(0.0552259184163649,-0.0451771306857534,0.997451314500147));
#61436=DIRECTION('center_axis',(0.284551435696759,0.958262022045047,0.0276473787012796));
#61437=DIRECTION('ref_axis',(-0.957826285221151,0.282982425517402,0.0498974366850415));
#61438=DIRECTION('center_axis',(-0.284551435696759,-0.958262022045047,-0.0276473787012796));
#61439=DIRECTION('ref_axis',(-0.958660774436356,0.284433077286297,0.00820634526047709));
#61440=DIRECTION('',(0.016150378482405,-0.0336272827279996,0.999303943318151));
#61441=DIRECTION('center_axis',(-0.0617712249622997,0.997491655456914,0.0345646215150941));
#61442=DIRECTION('ref_axis',(-0.998052578482889,-0.0614306198252359,-0.0108318757168334));
#61443=DIRECTION('center_axis',(0.0617712249622997,-0.997491655456914,-0.0345646215150941));
#61444=DIRECTION('ref_axis',(0.998090334472114,0.061734173069449,0.0021391841375509));
#61445=DIRECTION('',(-0.137998583506848,-0.0428336755604258,0.989505769153514));
#61446=DIRECTION('center_axis',(-0.99026806874157,0.0241671553619711,-0.137058748836224));
#61447=DIRECTION('ref_axis',(0.,-0.984807753012208,-0.17364817766693));
#61448=DIRECTION('center_axis',(0.99026806874157,-0.0241671553619711,0.137058748836224));
#61449=DIRECTION('ref_axis',(0.139173100960066,0.171958245538724,-0.975223671657125));
#61450=DIRECTION('',(-0.137844537491629,-0.0345663418323003,0.989850519773593));
#61451=DIRECTION('center_axis',(0.,0.999390827019096,0.0348994967025009));
#61452=DIRECTION('ref_axis',(-1.,0.,0.));
#61453=DIRECTION('',(-1.,0.,0.));
#61454=DIRECTION('center_axis',(0.,-0.17364817766693,0.984807753012208));
#61455=DIRECTION('ref_axis',(1.,0.,0.));
#61456=DIRECTION('center_axis',(1.,0.,0.));
#61457=DIRECTION('ref_axis',(0.,1.,0.));
#61458=DIRECTION('center_axis',(1.,0.,0.));
#61459=DIRECTION('ref_axis',(0.,0.,-1.));
#61460=DIRECTION('center_axis',(0.649305557988371,0.747685187986609,0.139173100960065));
#61461=DIRECTION('ref_axis',(-0.760527640763576,0.638341228068795,0.118819965419165));
#61462=DIRECTION('',(1.,0.,0.));
#61463=DIRECTION('center_axis',(-0.99026806874157,8.52189463090778E-18,
0.139173100960065));
#61464=DIRECTION('ref_axis',(0.139173100960065,0.,0.99026806874157));
#61465=DIRECTION('center_axis',(-0.0617712249622996,0.988339599396795,0.139173100960065));
#61466=DIRECTION('ref_axis',(0.998090334472114,0.0611677576917705,0.00861334152950385));
#61467=DIRECTION('center_axis',(0.284551435696759,0.948504785655862,0.139173100960065));
#61468=DIRECTION('ref_axis',(-0.958660774436356,0.281536916624453,0.0413096131025498));
#61469=DIRECTION('center_axis',(0.491310548314114,0.859793459549701,0.139173100960065));
#61470=DIRECTION('ref_axis',(-0.870984468928858,0.484997851417207,0.0785056622506209));
#61471=DIRECTION('center_axis',(0.313150259135956,0.939450777407866,0.139173100960065));
#61472=DIRECTION('ref_axis',(-0.949703593340092,0.309769549629784,0.0458902050450515));
#61473=DIRECTION('',(1.,0.,0.));
#61474=DIRECTION('center_axis',(-0.313150259135957,0.939450777407865,0.139173100960065));
#61475=DIRECTION('ref_axis',(0.949703593340092,0.309769549629785,0.0458902050450517));
#61476=DIRECTION('center_axis',(-0.491310548314113,0.859793459549702,0.139173100960066));
#61477=DIRECTION('ref_axis',(0.870984468928858,0.484997851417206,0.0785056622506207));
#61478=DIRECTION('center_axis',(-0.284551435696759,0.948504785655862,0.139173100960065));
#61479=DIRECTION('ref_axis',(0.958660774436356,0.281536916624453,0.0413096131025497));
#61480=DIRECTION('center_axis',(0.0617712249622997,0.988339599396795,0.139173100960065));
#61481=DIRECTION('ref_axis',(-0.998090334472114,0.0611677576917706,0.00861334152950385));
#61482=DIRECTION('center_axis',(0.99026806874157,8.5218946309078E-18,0.139173100960066));
#61483=DIRECTION('ref_axis',(-0.139173100960066,0.,0.99026806874157));
#61484=DIRECTION('',(1.,0.,0.));
#61485=DIRECTION('center_axis',(0.,-0.99026806874157,-0.139173100960066));
#61486=DIRECTION('ref_axis',(1.,0.,0.));
#61487=DIRECTION('',(-0.137844537491629,-0.137844537491629,0.980814848463989));
#61488=DIRECTION('center_axis',(-0.99026806874157,-8.5218946309078E-18,
-0.139173100960066));
#61489=DIRECTION('ref_axis',(0.,-1.,6.12323399573677E-17));
#61490=DIRECTION('',(-0.137998583506848,-0.129642937822505,0.981910942816534));
#61491=DIRECTION('center_axis',(-0.0617712249622997,-0.988339599396795,
-0.139173100960065));
#61492=DIRECTION('ref_axis',(0.998052578482889,-0.0623782861551806,3.81956842381198E-18));
#61493=DIRECTION('',(0.0161503784824051,-0.140410899949307,0.989961587360995));
#61494=DIRECTION('center_axis',(0.284551435696759,-0.948504785655862,-0.139173100960065));
#61495=DIRECTION('ref_axis',(0.957826285221151,0.287347885566345,-1.75949834150292E-17));
#61496=DIRECTION('',(0.0552259184163645,-0.128714814516259,0.990142714187765));
#61497=DIRECTION('center_axis',(0.491310548314113,-0.859793459549702,-0.139173100960066));
#61498=DIRECTION('ref_axis',(0.86824314212446,0.496138938356832,-3.0379748139553E-17));
#61499=DIRECTION('',(0.057078643955053,-0.12766118652195,0.99017405028614));
#61500=DIRECTION('center_axis',(0.313150259135957,-0.939450777407865,-0.139173100960065));
#61501=DIRECTION('ref_axis',(0.948683298050513,0.31622776601684,-1.9363366072702E-17));
#61502=DIRECTION('',(0.0225789275220278,-0.13913762065955,0.990015613285545));
#61503=DIRECTION('center_axis',(0.,-0.99026806874157,-0.139173100960065));
#61504=DIRECTION('ref_axis',(1.,0.,0.));
#61505=DIRECTION('',(-0.0225789275220274,-0.13913762065955,0.990015613285545));
#61506=DIRECTION('center_axis',(-0.313150259135956,-0.939450777407866,-0.139173100960065));
#61507=DIRECTION('ref_axis',(0.948683298050514,-0.316227766016839,1.9363366072702E-17));
#61508=DIRECTION('',(-0.0570786439550527,-0.12766118652195,0.99017405028614));
#61509=DIRECTION('center_axis',(-0.491310548314114,-0.859793459549701,-0.139173100960065));
#61510=DIRECTION('ref_axis',(0.868243142124459,-0.496138938356833,3.03797481395531E-17));
#61511=DIRECTION('',(-0.0552259184163635,-0.128714814516259,0.990142714187765));
#61512=DIRECTION('center_axis',(-0.284551435696759,-0.948504785655862,-0.139173100960065));
#61513=DIRECTION('ref_axis',(0.957826285221151,-0.287347885566346,1.75949834150293E-17));
#61514=DIRECTION('',(-0.0161503784824052,-0.140410899949307,0.989961587360995));
#61515=DIRECTION('center_axis',(0.0617712249622996,-0.988339599396795,-0.139173100960065));
#61516=DIRECTION('ref_axis',(0.998052578482889,0.0623782861551805,-3.81956842381197E-18));
#61517=DIRECTION('',(0.137998583506848,-0.129642937822505,0.981910942816534));
#61518=DIRECTION('center_axis',(0.99026806874157,-8.52189463090778E-18,
-0.139173100960065));
#61519=DIRECTION('ref_axis',(0.,1.,-6.12323399573677E-17));
#61520=DIRECTION('',(0.137844537491629,-0.137844537491629,0.980814848463989));
#61521=DIRECTION('center_axis',(0.,-0.99026806874157,-0.139173100960065));
#61522=DIRECTION('ref_axis',(1.,0.,0.));
#61523=DIRECTION('',(-0.051925424877728,-0.138985351600607,0.98893216263388));
#61524=DIRECTION('center_axis',(-0.649305557988371,-0.747685187986609,-0.139173100960065));
#61525=DIRECTION('ref_axis',(0.755033118392644,-0.655686655446243,4.01492281917938E-17));
#61526=DIRECTION('center_axis',(0.,0.99026806874157,-0.139173100960065));
#61527=DIRECTION('ref_axis',(-1.,0.,0.));
#61528=DIRECTION('',(-1.,0.,0.));
#61529=DIRECTION('',(0.137844537491629,0.137844537491629,0.980814848463989));
#61530=DIRECTION('center_axis',(0.99026806874157,-8.52189463090778E-18,
-0.139173100960065));
#61531=DIRECTION('ref_axis',(0.,1.,-6.12323399573677E-17));
#61532=DIRECTION('center_axis',(-0.99026806874157,8.52189463090778E-18,
0.139173100960065));
#61533=DIRECTION('ref_axis',(0.139173100960065,0.,0.99026806874157));
#61534=DIRECTION('',(0.137998583506848,0.129642937822505,0.981910942816534));
#61535=DIRECTION('center_axis',(0.0617712249622996,0.988339599396795,-0.139173100960065));
#61536=DIRECTION('ref_axis',(-0.998052578482889,0.0623782861551805,-3.81956842381197E-18));
#61537=DIRECTION('center_axis',(-0.0617712249622996,-0.988339599396795,
0.139173100960065));
#61538=DIRECTION('ref_axis',(-0.998090334472114,0.0611677576917705,-0.00861334152950385));
#61539=DIRECTION('',(-0.0161503784824054,0.140410899949307,0.989961587360995));
#61540=DIRECTION('center_axis',(-0.284551435696759,0.948504785655862,-0.139173100960066));
#61541=DIRECTION('ref_axis',(-0.957826285221151,-0.287347885566346,1.75949834150293E-17));
#61542=DIRECTION('center_axis',(0.284551435696759,-0.948504785655862,0.139173100960066));
#61543=DIRECTION('ref_axis',(0.958660774436356,0.281536916624453,-0.0413096131025498));
#61544=DIRECTION('',(-0.0552259184163638,0.12871481451626,0.990142714187765));
#61545=DIRECTION('center_axis',(-0.491310548314114,0.859793459549701,-0.139173100960066));
#61546=DIRECTION('ref_axis',(-0.868243142124459,-0.496138938356833,3.03797481395531E-17));
#61547=DIRECTION('center_axis',(0.491310548314114,-0.859793459549701,0.139173100960066));
#61548=DIRECTION('ref_axis',(0.870984468928858,0.484997851417207,-0.0785056622506209));
#61549=DIRECTION('',(-0.0570786439550532,0.12766118652195,0.99017405028614));
#61550=DIRECTION('center_axis',(-0.313150259135956,0.939450777407866,-0.139173100960065));
#61551=DIRECTION('ref_axis',(-0.948683298050514,-0.316227766016839,1.9363366072702E-17));
#61552=DIRECTION('center_axis',(0.313150259135956,-0.939450777407866,0.139173100960065));
#61553=DIRECTION('ref_axis',(0.949703593340092,0.309769549629784,-0.0458902050450515));
#61554=DIRECTION('',(-0.0225789275220273,0.139137620659551,0.990015613285545));
#61555=DIRECTION('center_axis',(0.,0.99026806874157,-0.139173100960065));
#61556=DIRECTION('ref_axis',(-1.,0.,0.));
#61557=DIRECTION('',(-1.,0.,0.));
#61558=DIRECTION('',(0.0225789275220281,0.139137620659551,0.990015613285545));
#61559=DIRECTION('center_axis',(0.313150259135957,0.939450777407865,-0.139173100960066));
#61560=DIRECTION('ref_axis',(-0.948683298050513,0.31622776601684,-1.9363366072702E-17));
#61561=DIRECTION('center_axis',(-0.313150259135957,-0.939450777407865,0.139173100960066));
#61562=DIRECTION('ref_axis',(-0.949703593340092,0.309769549629785,-0.0458902050450517));
#61563=DIRECTION('',(0.0570786439550534,0.12766118652195,0.99017405028614));
#61564=DIRECTION('center_axis',(0.491310548314113,0.859793459549702,-0.139173100960066));
#61565=DIRECTION('ref_axis',(-0.86824314212446,0.496138938356832,-3.0379748139553E-17));
#61566=DIRECTION('center_axis',(-0.491310548314113,-0.859793459549702,0.139173100960066));
#61567=DIRECTION('ref_axis',(-0.870984468928858,0.484997851417206,-0.0785056622506208));
#61568=DIRECTION('',(0.0552259184163649,0.128714814516259,0.990142714187765));
#61569=DIRECTION('center_axis',(0.284551435696759,0.948504785655862,-0.139173100960065));
#61570=DIRECTION('ref_axis',(-0.957826285221151,0.287347885566345,-1.75949834150292E-17));
#61571=DIRECTION('center_axis',(-0.284551435696759,-0.948504785655862,0.139173100960065));
#61572=DIRECTION('ref_axis',(-0.958660774436356,0.281536916624453,-0.0413096131025497));
#61573=DIRECTION('',(0.0161503784824051,0.140410899949307,0.989961587360995));
#61574=DIRECTION('center_axis',(-0.0617712249622997,0.988339599396795,-0.139173100960066));
#61575=DIRECTION('ref_axis',(-0.998052578482889,-0.0623782861551806,3.81956842381198E-18));
#61576=DIRECTION('center_axis',(0.0617712249622997,-0.988339599396795,0.139173100960066));
#61577=DIRECTION('ref_axis',(0.998090334472114,0.0611677576917706,-0.00861334152950386));
#61578=DIRECTION('',(-0.137998583506848,0.129642937822505,0.981910942816533));
#61579=DIRECTION('center_axis',(-0.99026806874157,-8.5218946309078E-18,
-0.139173100960066));
#61580=DIRECTION('ref_axis',(0.,-1.,6.12323399573677E-17));
#61581=DIRECTION('center_axis',(0.99026806874157,8.5218946309078E-18,0.139173100960066));
#61582=DIRECTION('ref_axis',(-0.139173100960066,0.,0.99026806874157));
#61583=DIRECTION('',(-0.137844537491629,0.137844537491629,0.980814848463989));
#61584=DIRECTION('center_axis',(0.,0.99026806874157,-0.139173100960066));
#61585=DIRECTION('ref_axis',(-1.,0.,0.));
#61586=DIRECTION('',(-1.,0.,0.));
#61587=DIRECTION('center_axis',(0.,6.12323399573677E-17,1.));
#61588=DIRECTION('ref_axis',(1.,0.,0.));
#61589=DIRECTION('center_axis',(1.,0.,0.));
#61590=DIRECTION('ref_axis',(0.,1.,0.));
#61591=DIRECTION('center_axis',(1.,0.,0.));
#61592=DIRECTION('ref_axis',(0.,0.,-1.));
#61593=DIRECTION('center_axis',(0.64930555798837,0.760493325303574,0.00722457847379229));
#61594=DIRECTION('ref_axis',(-0.760527640763576,0.649276260934969,0.00616803217361924));
#61595=DIRECTION('',(1.,0.,0.));
#61596=DIRECTION('center_axis',(-0.99026806874157,0.0241671553619711,0.137058748836223));
#61597=DIRECTION('ref_axis',(0.139173100960065,0.171958245538723,0.975223671657125));
#61598=DIRECTION('center_axis',(-0.0617712249622996,0.997491655456914,-0.0345646215150942));
#61599=DIRECTION('ref_axis',(0.998090334472114,0.061734173069449,-0.0021391841375509));
#61600=DIRECTION('center_axis',(0.284551435696759,0.958262022045047,-0.0276473787012796));
#61601=DIRECTION('ref_axis',(-0.958660774436356,0.284433077286297,-0.00820634526047711));
#61602=DIRECTION('center_axis',(0.491310548314114,0.870898420315705,-0.0122428185845281));
#61603=DIRECTION('ref_axis',(-0.870984468928858,0.491262009456284,-0.00690600823120538));
#61604=DIRECTION('center_axis',(0.313150259135956,0.949345564526583,-0.0260751666684337));
#61605=DIRECTION('ref_axis',(-0.949703593340092,0.313032204601347,-0.00859788807423117));
#61606=DIRECTION('',(1.,0.,0.));
#61607=DIRECTION('center_axis',(-0.313150259135957,0.949345564526583,-0.0260751666684336));
#61608=DIRECTION('ref_axis',(0.949703593340092,0.313032204601348,-0.00859788807423114));
#61609=DIRECTION('center_axis',(-0.491310548314113,0.870898420315706,-0.0122428185845281));
#61610=DIRECTION('ref_axis',(0.870984468928858,0.491262009456283,-0.00690600823120532));
#61611=DIRECTION('center_axis',(-0.284551435696759,0.958262022045047,-0.0276473787012797));
#61612=DIRECTION('ref_axis',(0.958660774436356,0.284433077286297,-0.00820634526047713));
#61613=DIRECTION('center_axis',(0.0617712249622997,0.997491655456914,-0.0345646215150942));
#61614=DIRECTION('ref_axis',(-0.998090334472114,0.061734173069449,-0.00213918413755091));
#61615=DIRECTION('center_axis',(0.99026806874157,0.0241671553619711,0.137058748836224));
#61616=DIRECTION('ref_axis',(-0.139173100960066,0.171958245538724,0.975223671657125));
#61617=DIRECTION('',(1.,0.,0.));
#61618=DIRECTION('center_axis',(0.,-0.999390827019096,0.0348994967025009));
#61619=DIRECTION('ref_axis',(1.,0.,0.));
#61620=DIRECTION('',(-0.137844537491629,0.0345663418323002,0.989850519773593));
#61621=DIRECTION('center_axis',(-0.99026806874157,-0.0241671553619711,-0.137058748836224));
#61622=DIRECTION('ref_axis',(0.,-0.984807753012208,0.17364817766693));
#61623=DIRECTION('',(-0.137998583506848,0.0428336755604259,0.989505769153514));
#61624=DIRECTION('center_axis',(-0.0617712249622997,-0.997491655456914,
0.0345646215150942));
#61625=DIRECTION('ref_axis',(0.998052578482889,-0.0614306198252359,0.0108318757168334));
#61626=DIRECTION('',(0.0161503784824051,0.0336272827279997,0.999303943318151));
#61627=DIRECTION('center_axis',(0.284551435696759,-0.958262022045047,0.0276473787012797));
#61628=DIRECTION('ref_axis',(0.957826285221151,0.282982425517402,-0.0498974366850415));
#61629=DIRECTION('',(0.0552259184163645,0.0451771306857535,0.997451314500147));
#61630=DIRECTION('center_axis',(0.491310548314113,-0.870898420315706,0.0122428185845281));
#61631=DIRECTION('ref_axis',(0.86824314212446,0.488601473065054,-0.0861536225152694));
#61632=DIRECTION('',(0.057078643955053,0.0462201931597181,0.997299213951626));
#61633=DIRECTION('center_axis',(0.313150259135957,-0.949345564526583,0.0260751666684336));
#61634=DIRECTION('ref_axis',(0.948683298050513,0.311423555691114,-0.0549123752965087));
#61635=DIRECTION('',(0.0225789275220278,0.0348905995476465,0.999136045839184));
#61636=DIRECTION('center_axis',(0.,-0.999390827019096,0.034899496702501));
#61637=DIRECTION('ref_axis',(1.,0.,0.));
#61638=DIRECTION('',(-0.0225789275220274,0.0348905995476465,0.999136045839184));
#61639=DIRECTION('center_axis',(-0.313150259135956,-0.949345564526583,0.0260751666684337));
#61640=DIRECTION('ref_axis',(0.948683298050514,-0.311423555691113,0.0549123752965085));
#61641=DIRECTION('',(-0.0570786439550527,0.0462201931597181,0.997299213951626));
#61642=DIRECTION('center_axis',(-0.491310548314114,-0.870898420315705,0.0122428185845281));
#61643=DIRECTION('ref_axis',(0.868243142124459,-0.488601473065055,0.0861536225152696));
#61644=DIRECTION('',(-0.0552259184163635,0.045177130685753,0.997451314500147));
#61645=DIRECTION('center_axis',(-0.284551435696759,-0.958262022045047,0.0276473787012796));
#61646=DIRECTION('ref_axis',(0.957826285221151,-0.282982425517402,0.0498974366850416));
#61647=DIRECTION('',(-0.0161503784824052,0.0336272827279996,0.999303943318151));
#61648=DIRECTION('center_axis',(0.0617712249622996,-0.997491655456914,0.0345646215150942));
#61649=DIRECTION('ref_axis',(0.998052578482889,0.0614306198252359,-0.0108318757168334));
#61650=DIRECTION('',(0.137998583506848,0.0428336755604258,0.989505769153514));
#61651=DIRECTION('center_axis',(0.99026806874157,-0.0241671553619711,-0.137058748836223));
#61652=DIRECTION('ref_axis',(0.,0.984807753012208,-0.17364817766693));
#61653=DIRECTION('',(0.137844537491629,0.0345663418323004,0.989850519773593));
#61654=DIRECTION('center_axis',(0.,-0.999390827019096,0.034899496702501));
#61655=DIRECTION('ref_axis',(1.,0.,0.));
#61656=DIRECTION('',(-0.051925424877728,0.0348524160661846,0.998042613992818));
#61657=DIRECTION('center_axis',(-0.64930555798837,-0.760493325303574,-0.00722457847379229));
#61658=DIRECTION('ref_axis',(0.755033118392644,-0.645725301830105,0.113858792838765));
#61659=DIRECTION('center_axis',(0.,0.951056516295154,-0.309016994374948));
#61660=DIRECTION('ref_axis',(-1.,0.,0.));
#61661=DIRECTION('',(-1.,0.,0.));
#61662=DIRECTION('',(0.137844537491629,0.306067080296576,0.941977614300068));
#61663=DIRECTION('center_axis',(0.99026806874157,-0.0241671553619711,-0.137058748836223));
#61664=DIRECTION('ref_axis',(0.,0.984807753012208,-0.17364817766693));
#61665=DIRECTION('center_axis',(-0.99026806874157,0.0241671553619711,0.137058748836223));
#61666=DIRECTION('ref_axis',(0.139173100960065,0.171958245538723,0.975223671657125));
#61667=DIRECTION('',(0.137998583506848,0.298180416142191,0.944481249352984));
#61668=DIRECTION('center_axis',(0.0617712249622996,0.949157344732972,-0.308682119187541));
#61669=DIRECTION('ref_axis',(-0.998052578482889,0.0614306198252359,-0.0108318757168334));
#61670=DIRECTION('center_axis',(-0.0617712249622996,-0.949157344732972,
0.308682119187541));
#61671=DIRECTION('ref_axis',(-0.998090334472114,0.0587427909490065,-0.0191041551727457));
#61672=DIRECTION('',(-0.0161503784824054,0.310182768482997,0.950539749516609));
#61673=DIRECTION('center_axis',(-0.284551435696759,0.909927711321104,-0.301764876373726));
#61674=DIRECTION('ref_axis',(-0.957826285221151,-0.282982425517402,0.0498974366850416));
#61675=DIRECTION('center_axis',(0.284551435696759,-0.909927711321104,0.301764876373726));
#61676=DIRECTION('ref_axis',(0.958660774436356,0.27008639921553,-0.0895703997751286));
#61677=DIRECTION('',(-0.0552259184163638,0.298695825212034,0.952749128541176));
#61678=DIRECTION('center_axis',(-0.491310548314114,0.822564109591763,-0.286360316256975));
#61679=DIRECTION('ref_axis',(-0.868243142124459,-0.488601473065055,0.0861536225152696));
#61680=DIRECTION('center_axis',(0.491310548314114,-0.822564109591763,0.286360316256975));
#61681=DIRECTION('ref_axis',(0.870984468928858,0.463997279083572,-0.161531977910744));
#61682=DIRECTION('',(-0.0570786439550532,0.297663645650825,0.952962949154956));
#61683=DIRECTION('center_axis',(-0.313150259135956,0.901011253802641,-0.30019266434088));
#61684=DIRECTION('ref_axis',(-0.948683298050514,-0.311423555691113,0.0549123752965085));
#61685=DIRECTION('center_axis',(0.313150259135956,-0.901011253802641,0.30019266434088));
#61686=DIRECTION('ref_axis',(0.949703593340092,0.297094703643677,-0.0989839475056044));
#61687=DIRECTION('',(-0.0225789275220273,0.30893821467004,0.950814057294297));
#61688=DIRECTION('center_axis',(0.,0.951056516295154,-0.309016994374948));
#61689=DIRECTION('ref_axis',(-1.,0.,0.));
#61690=DIRECTION('',(-1.,0.,0.));
#61691=DIRECTION('',(0.0225789275220281,0.30893821467004,0.950814057294297));
#61692=DIRECTION('center_axis',(0.313150259135957,0.901011253802641,-0.30019266434088));
#61693=DIRECTION('ref_axis',(-0.948683298050513,0.311423555691114,-0.0549123752965087));
#61694=DIRECTION('center_axis',(-0.313150259135957,-0.901011253802641,0.30019266434088));
#61695=DIRECTION('ref_axis',(-0.949703593340092,0.297094703643678,-0.0989839475056049));
#61696=DIRECTION('',(0.0570786439550533,0.297663645650825,0.952962949154956));
#61697=DIRECTION('center_axis',(0.491310548314113,0.822564109591764,-0.286360316256975));
#61698=DIRECTION('ref_axis',(-0.86824314212446,0.488601473065054,-0.0861536225152694));
#61699=DIRECTION('center_axis',(-0.491310548314113,-0.822564109591764,0.286360316256975));
#61700=DIRECTION('ref_axis',(-0.870984468928858,0.463997279083571,-0.161531977910744));
#61701=DIRECTION('',(0.0552259184163649,0.298695825212034,0.952749128541176));
#61702=DIRECTION('center_axis',(0.284551435696759,0.909927711321105,-0.301764876373726));
#61703=DIRECTION('ref_axis',(-0.957826285221151,0.282982425517402,-0.0498974366850415));
#61704=DIRECTION('center_axis',(-0.284551435696759,-0.909927711321105,0.301764876373726));
#61705=DIRECTION('ref_axis',(-0.958660774436356,0.270086399215529,-0.0895703997751284));
#61706=DIRECTION('',(0.0161503784824051,0.310182768482997,0.950539749516609));
#61707=DIRECTION('center_axis',(-0.0617712249622997,0.949157344732972,-0.308682119187541));
#61708=DIRECTION('ref_axis',(-0.998052578482889,-0.0614306198252359,0.0108318757168334));
#61709=DIRECTION('center_axis',(0.0617712249622997,-0.949157344732972,0.308682119187541));
#61710=DIRECTION('ref_axis',(0.998090334472114,0.0587427909490065,-0.0191041551727457));
#61711=DIRECTION('',(-0.137998583506848,0.298180416142191,0.944481249352984));
#61712=DIRECTION('center_axis',(-0.99026806874157,-0.0241671553619711,-0.137058748836224));
#61713=DIRECTION('ref_axis',(0.,-0.984807753012208,0.17364817766693));
#61714=DIRECTION('center_axis',(0.99026806874157,0.0241671553619711,0.137058748836224));
#61715=DIRECTION('ref_axis',(-0.139173100960066,0.171958245538724,0.975223671657125));
#61716=DIRECTION('',(-0.137844537491629,0.306067080296576,0.941977614300068));
#61717=DIRECTION('center_axis',(0.,0.951056516295154,-0.309016994374948));
#61718=DIRECTION('ref_axis',(-1.,0.,0.));
#61719=DIRECTION('',(-1.,0.,0.));
#61720=DIRECTION('center_axis',(0.,0.17364817766693,0.984807753012208));
#61721=DIRECTION('ref_axis',(1.,0.,0.));
#61722=DIRECTION('center_axis',(1.,0.,0.));
#61723=DIRECTION('ref_axis',(0.,1.,0.));
#61724=DIRECTION('center_axis',(1.,0.,0.));
#61725=DIRECTION('ref_axis',(0.,0.,-1.));
#61726=DIRECTION('center_axis',(0.64930555798837,0.75019425775938,-0.124943459173594));
#61727=DIRECTION('ref_axis',(-0.760527640763576,0.640483363162275,-0.106671313608347));
#61728=DIRECTION('',(1.,0.,0.));
#61729=DIRECTION('center_axis',(-0.99026806874157,0.0476000039374394,0.130779935984066));
#61730=DIRECTION('ref_axis',(0.139173100960065,0.338691626801824,0.930547596796367));
#61731=DIRECTION('center_axis',(-0.0617712249622996,0.976335432321108,-0.20725211545606));
#61732=DIRECTION('ref_axis',(0.998090334472114,0.0604248268374111,-0.0128267117770656));
#61733=DIRECTION('center_axis',(0.284551435696759,0.938902951798373,-0.193627806751035));
#61734=DIRECTION('ref_axis',(-0.958660774436356,0.278686882824878,-0.0574729579753755));
#61735=DIRECTION('center_axis',(0.491310548314114,0.855541573276281,-0.163286746281596));
#61736=DIRECTION('ref_axis',(-0.870984468928858,0.482599419928604,-0.0921078431475353));
#61737=DIRECTION('center_axis',(0.313150259135956,0.930394967059196,-0.190531153552384));
#61738=DIRECTION('ref_axis',(-0.949703593340092,0.306783534438036,-0.0628247387151196));
#61739=DIRECTION('',(1.,0.,0.));
#61740=DIRECTION('center_axis',(-0.313150259135957,0.930394967059195,-0.190531153552383));
#61741=DIRECTION('ref_axis',(0.949703593340092,0.306783534438036,-0.0628247387151197));
#61742=DIRECTION('center_axis',(-0.491310548314113,0.855541573276282,-0.163286746281596));
#61743=DIRECTION('ref_axis',(0.870984468928858,0.482599419928602,-0.092107843147535));
#61744=DIRECTION('center_axis',(-0.284551435696759,0.938902951798373,-0.193627806751035));
#61745=DIRECTION('ref_axis',(0.958660774436356,0.278686882824878,-0.0574729579753754));
#61746=DIRECTION('center_axis',(0.0617712249622997,0.976335432321108,-0.20725211545606));
#61747=DIRECTION('ref_axis',(-0.998090334472114,0.0604248268374112,-0.0128267117770656));
#61748=DIRECTION('center_axis',(0.99026806874157,0.0476000039374395,0.130779935984066));
#61749=DIRECTION('ref_axis',(-0.139173100960066,0.338691626801825,0.930547596796366));
#61750=DIRECTION('',(1.,0.,0.));
#61751=DIRECTION('center_axis',(0.,-0.978147600733806,0.207911690817759));
#61752=DIRECTION('ref_axis',(1.,0.,0.));
#61753=DIRECTION('',(-0.137844537491629,0.205926940351068,0.968810083928407));
#61754=DIRECTION('center_axis',(-0.99026806874157,-0.0476000039374395,-0.130779935984066));
#61755=DIRECTION('ref_axis',(0.,-0.939692620785908,0.342020143325669));
#61756=DIRECTION('',(-0.137998583506848,0.214008809386339,0.967034963408844));
#61757=DIRECTION('center_axis',(-0.0617712249622997,-0.976335432321108,
0.20725211545606));
#61758=DIRECTION('ref_axis',(0.998052578482889,-0.058616415197295,0.0213346303712044));
#61759=DIRECTION('',(0.0161503784824051,0.206643717435842,0.978282954629779));
#61760=DIRECTION('center_axis',(0.284551435696759,-0.938902951798373,0.193627806751035));
#61761=DIRECTION('ref_axis',(0.957826285221151,0.270018687665128,-0.0982787650057293));
#61762=DIRECTION('',(0.0552259184163645,0.217696391632611,0.974452861356161));
#61763=DIRECTION('center_axis',(0.491310548314113,-0.855541573276282,0.163286746281596));
#61764=DIRECTION('ref_axis',(0.86824314212446,0.46621809925847,-0.169689510806249));
#61765=DIRECTION('',(0.057078643955053,0.218697195660774,0.974121945658943));
#61766=DIRECTION('center_axis',(0.313150259135957,-0.930394967059195,0.190531153552383));
#61767=DIRECTION('ref_axis',(0.948683298050513,0.297156898213637,-0.108156265856636));
#61768=DIRECTION('',(0.0225789275220278,0.207858686543084,0.977898235227234));
#61769=DIRECTION('center_axis',(0.,-0.978147600733806,0.207911690817759));
#61770=DIRECTION('ref_axis',(1.,0.,0.));
#61771=DIRECTION('',(-0.0225789275220274,0.207858686543084,0.977898235227234));
#61772=DIRECTION('center_axis',(-0.313150259135956,-0.930394967059196,0.190531153552384));
#61773=DIRECTION('ref_axis',(0.948683298050514,-0.297156898213636,0.108156265856635));
#61774=DIRECTION('',(-0.0570786439550527,0.218697195660774,0.974121945658943));
#61775=DIRECTION('center_axis',(-0.491310548314114,-0.855541573276281,0.163286746281596));
#61776=DIRECTION('ref_axis',(0.868243142124459,-0.466218099258471,0.169689510806249));
#61777=DIRECTION('',(-0.0552259184163635,0.21769639163261,0.974452861356161));
#61778=DIRECTION('center_axis',(-0.284551435696759,-0.938902951798373,0.193627806751035));
#61779=DIRECTION('ref_axis',(0.957826285221151,-0.270018687665129,0.0982787650057295));
#61780=DIRECTION('',(-0.0161503784824052,0.206643717435842,0.978282954629779));
#61781=DIRECTION('center_axis',(0.0617712249622996,-0.976335432321108,0.20725211545606));
#61782=DIRECTION('ref_axis',(0.998052578482889,0.0586164151972949,-0.0213346303712044));
#61783=DIRECTION('',(0.137998583506848,0.214008809386339,0.967034963408845));
#61784=DIRECTION('center_axis',(0.99026806874157,-0.0476000039374394,-0.130779935984066));
#61785=DIRECTION('ref_axis',(0.,0.939692620785908,-0.342020143325669));
#61786=DIRECTION('',(0.137844537491629,0.205926940351068,0.968810083928407));
#61787=DIRECTION('center_axis',(0.,-0.978147600733806,0.207911690817759));
#61788=DIRECTION('ref_axis',(1.,0.,0.));
#61789=DIRECTION('',(-0.0519254248777279,0.207631210706978,0.976828045559515));
#61790=DIRECTION('center_axis',(-0.64930555798837,-0.75019425775938,0.124943459173594));
#61791=DIRECTION('ref_axis',(0.755033118392644,-0.616143911670627,0.224258043872453));
#61792=DIRECTION('center_axis',(0.,0.882947592858927,-0.469471562785891));
#61793=DIRECTION('ref_axis',(-1.,0.,0.));
#61794=DIRECTION('',(-1.,0.,0.));
#61795=DIRECTION('',(0.137844537491629,0.464989929744128,0.874518866989312));
#61796=DIRECTION('center_axis',(0.99026806874157,-0.0476000039374394,-0.130779935984066));
#61797=DIRECTION('ref_axis',(0.,0.939692620785908,-0.342020143325669));
#61798=DIRECTION('center_axis',(-0.99026806874157,0.0476000039374394,0.130779935984066));
#61799=DIRECTION('ref_axis',(0.139173100960065,0.338691626801824,0.930547596796367));
#61800=DIRECTION('',(0.137998583506848,0.457657833403968,0.878353971058417));
#61801=DIRECTION('center_axis',(0.0617712249622996,0.881135424446229,-0.468811987424192));
#61802=DIRECTION('ref_axis',(-0.998052578482889,0.0586164151972949,-0.0213346303712044));
#61803=DIRECTION('center_axis',(-0.0617712249622996,-0.881135424446229,
0.468811987424192));
#61804=DIRECTION('ref_axis',(-0.998090334472114,0.0545329542285434,-0.0290144987282327));
#61805=DIRECTION('',(-0.0161503784824054,0.470529890556386,0.882236242379483));
#61806=DIRECTION('center_axis',(-0.284551435696759,0.843702943923494,-0.455187678719166));
#61807=DIRECTION('ref_axis',(-0.957826285221151,-0.270018687665129,0.0982787650057295));
#61808=DIRECTION('center_axis',(0.284551435696759,-0.843702943923494,0.455187678719166));
#61809=DIRECTION('ref_axis',(0.958660774436356,0.250429443236754,-0.135109635175349));
#61810=DIRECTION('',(-0.0552259184163638,0.459601114406122,0.886406742738186));
#61811=DIRECTION('center_axis',(-0.491310548314114,0.760341565401402,-0.424846618249727));
#61812=DIRECTION('ref_axis',(-0.868243142124459,-0.466218099258471,0.169689510806249));
#61813=DIRECTION('center_axis',(0.491310548314114,-0.760341565401402,0.424846618249727));
#61814=DIRECTION('ref_axis',(0.870984468928858,0.428898384218936,-0.239650226161174));
#61815=DIRECTION('',(-0.0570786439550532,0.458621745531673,0.886796551036219));
#61816=DIRECTION('center_axis',(-0.313150259135956,0.835194959184317,-0.452091025520515));
#61817=DIRECTION('ref_axis',(-0.948683298050514,-0.297156898213636,0.108156265856635));
#61818=DIRECTION('center_axis',(0.313150259135956,-0.835194959184317,0.452091025520515));
#61819=DIRECTION('ref_axis',(0.949703593340092,0.27539278542453,-0.149070112809494));
#61820=DIRECTION('',(-0.0225789275220273,0.469351877358061,0.88272249730729));
#61821=DIRECTION('center_axis',(0.,0.882947592858927,-0.469471562785891));
#61822=DIRECTION('ref_axis',(-1.,0.,0.));
#61823=DIRECTION('',(-1.,0.,0.));
#61824=DIRECTION('',(0.0225789275220281,0.469351877358061,0.88272249730729));
#61825=DIRECTION('center_axis',(0.313150259135957,0.835194959184317,-0.452091025520515));
#61826=DIRECTION('ref_axis',(-0.948683298050513,0.297156898213637,-0.108156265856636));
#61827=DIRECTION('center_axis',(-0.313150259135957,-0.835194959184317,0.452091025520515));
#61828=DIRECTION('ref_axis',(-0.949703593340092,0.275392785424531,-0.149070112809494));
#61829=DIRECTION('',(0.0570786439550534,0.458621745531673,0.886796551036219));
#61830=DIRECTION('center_axis',(0.491310548314113,0.760341565401403,-0.424846618249728));
#61831=DIRECTION('ref_axis',(-0.86824314212446,0.46621809925847,-0.169689510806249));
#61832=DIRECTION('center_axis',(-0.491310548314113,-0.760341565401403,0.424846618249728));
#61833=DIRECTION('ref_axis',(-0.870984468928858,0.428898384218935,-0.239650226161173));
#61834=DIRECTION('',(0.0552259184163649,0.459601114406122,0.886406742738186));
#61835=DIRECTION('center_axis',(0.284551435696759,0.843702943923494,-0.455187678719166));
#61836=DIRECTION('ref_axis',(-0.957826285221151,0.270018687665128,-0.0982787650057293));
#61837=DIRECTION('center_axis',(-0.284551435696759,-0.843702943923494,0.455187678719166));
#61838=DIRECTION('ref_axis',(-0.958660774436356,0.250429443236754,-0.135109635175349));
#61839=DIRECTION('',(0.0161503784824051,0.470529890556386,0.882236242379483));
#61840=DIRECTION('center_axis',(-0.0617712249622997,0.881135424446229,-0.468811987424192));
#61841=DIRECTION('ref_axis',(-0.998052578482889,-0.058616415197295,0.0213346303712044));
#61842=DIRECTION('center_axis',(0.0617712249622997,-0.881135424446229,0.468811987424192));
#61843=DIRECTION('ref_axis',(0.998090334472114,0.0545329542285434,-0.0290144987282327));
#61844=DIRECTION('',(-0.137998583506848,0.457657833403968,0.878353971058417));
#61845=DIRECTION('center_axis',(-0.99026806874157,-0.0476000039374395,-0.130779935984066));
#61846=DIRECTION('ref_axis',(0.,-0.939692620785908,0.342020143325669));
#61847=DIRECTION('center_axis',(0.99026806874157,0.0476000039374395,0.130779935984066));
#61848=DIRECTION('ref_axis',(-0.139173100960066,0.338691626801825,0.930547596796366));
#61849=DIRECTION('',(-0.137844537491629,0.464989929744128,0.874518866989312));
#61850=DIRECTION('center_axis',(0.,0.882947592858927,-0.469471562785891));
#61851=DIRECTION('ref_axis',(-1.,0.,0.));
#61852=DIRECTION('',(-1.,0.,0.));
#61853=DIRECTION('center_axis',(0.,0.342020143325669,0.939692620785908));
#61854=DIRECTION('ref_axis',(1.,0.,0.));
#61855=DIRECTION('center_axis',(1.,0.,0.));
#61856=DIRECTION('ref_axis',(0.,1.,0.));
#61857=DIRECTION('center_axis',(1.,0.,0.));
#61858=DIRECTION('ref_axis',(0.,0.,-1.));
#61859=DIRECTION('center_axis',(0.649305557988371,0.717100917309779,-0.253315153038431));
#61860=DIRECTION('ref_axis',(-0.760527640763576,0.612229702500115,-0.216269505504612));
#61861=DIRECTION('',(1.,0.,0.));
#61862=DIRECTION('center_axis',(-0.99026806874157,0.0695865504800327,0.120527440954873));
#61863=DIRECTION('ref_axis',(0.139173100960065,0.495134034370783,0.857597304086756));
#61864=DIRECTION('center_axis',(-0.0617712249622996,0.925513751123792,-0.373642358743524));
#61865=DIRECTION('ref_axis',(0.998090334472114,0.0572795028183562,-0.0231245062698634));
#61866=DIRECTION('center_axis',(0.284551435696759,0.891015790469123,-0.353724951873058));
#61867=DIRECTION('ref_axis',(-0.958660774436356,0.264472928451193,-0.104993283944912));
#61868=DIRECTION('center_axis',(0.491310548314114,0.814189528457782,-0.309369288819978));
#61869=DIRECTION('ref_axis',(-0.870984468928858,0.459273291233482,-0.174511027858645));
#61870=DIRECTION('center_axis',(0.313150259135956,0.883174789320284,-0.34919794774906));
#61871=DIRECTION('ref_axis',(-0.949703593340092,0.291213401820784,-0.115142691461001));
#61872=DIRECTION('',(1.,0.,0.));
#61873=DIRECTION('center_axis',(-0.313150259135957,0.883174789320284,-0.34919794774906));
#61874=DIRECTION('ref_axis',(0.949703593340092,0.291213401820784,-0.115142691461001));
#61875=DIRECTION('center_axis',(-0.491310548314113,0.814189528457783,-0.309369288819978));
#61876=DIRECTION('ref_axis',(0.870984468928858,0.459273291233481,-0.174511027858644));
#61877=DIRECTION('center_axis',(-0.284551435696759,0.891015790469123,-0.353724951873058));
#61878=DIRECTION('ref_axis',(0.958660774436356,0.264472928451193,-0.104993283944912));
#61879=DIRECTION('center_axis',(0.0617712249622997,0.925513751123792,-0.373642358743524));
#61880=DIRECTION('ref_axis',(-0.998090334472114,0.0572795028183562,-0.0231245062698635));
#61881=DIRECTION('center_axis',(0.99026806874157,0.0695865504800329,0.120527440954873));
#61882=DIRECTION('ref_axis',(-0.139173100960066,0.495134034370784,0.857597304086755));
#61883=DIRECTION('',(1.,0.,0.));
#61884=DIRECTION('center_axis',(0.,-0.927183854566788,0.374606593415912));
#61885=DIRECTION('ref_axis',(1.,0.,0.));
#61886=DIRECTION('',(-0.137844537491629,0.371030552991328,0.918332843924613));
#61887=DIRECTION('center_axis',(-0.99026806874157,-0.0695865504800329,-0.120527440954873));
#61888=DIRECTION('ref_axis',(0.,-0.866025403784439,0.5));
#61889=DIRECTION('',(-0.137998583506848,0.378681393832731,0.9151812896443));
#61890=DIRECTION('center_axis',(-0.0617712249622997,-0.925513751123792,
0.373642358743524));
#61891=DIRECTION('ref_axis',(0.998052578482889,-0.0540211804549215,0.0311891430775903));
#61892=DIRECTION('',(0.0161503784824051,0.373381387356163,0.927537333400043));
#61893=DIRECTION('center_axis',(0.284551435696759,-0.891015790469123,0.353724951873058));
#61894=DIRECTION('ref_axis',(0.957826285221151,0.248850568624199,-0.143673942783173));
#61895=DIRECTION('',(0.0552259184163645,0.3836010578794,0.921846151116809));
#61896=DIRECTION('center_axis',(0.491310548314113,-0.814189528457783,0.309369288819978));
#61897=DIRECTION('ref_axis',(0.86824314212446,0.429668924423658,-0.248069469178416));
#61898=DIRECTION('',(0.057078643955053,0.384529194537798,0.921346474976903));
#61899=DIRECTION('center_axis',(0.313150259135957,-0.883174789320284,0.34919794774906));
#61900=DIRECTION('ref_axis',(0.948683298050513,0.273861278752585,-0.15811388300842));
#61901=DIRECTION('',(0.0225789275220278,0.374511092529479,0.926947481578288));
#61902=DIRECTION('center_axis',(0.,-0.927183854566787,0.374606593415912));
#61903=DIRECTION('ref_axis',(1.,0.,0.));
#61904=DIRECTION('',(-0.0225789275220274,0.374511092529479,0.926947481578288));
#61905=DIRECTION('center_axis',(-0.313150259135956,-0.883174789320284,0.34919794774906));
#61906=DIRECTION('ref_axis',(0.948683298050514,-0.273861278752584,0.158113883008419));
#61907=DIRECTION('',(-0.0570786439550527,0.384529194537798,0.921346474976903));
#61908=DIRECTION('center_axis',(-0.491310548314114,-0.814189528457782,0.309369288819978));
#61909=DIRECTION('ref_axis',(0.868243142124459,-0.429668924423659,0.248069469178417));
#61910=DIRECTION('',(-0.0552259184163635,0.3836010578794,0.921846151116809));
#61911=DIRECTION('center_axis',(-0.284551435696759,-0.891015790469123,0.353724951873058));
#61912=DIRECTION('ref_axis',(0.957826285221151,-0.248850568624199,0.143673942783173));
#61913=DIRECTION('',(-0.0161503784824052,0.373381387356163,0.927537333400043));
#61914=DIRECTION('center_axis',(0.0617712249622996,-0.925513751123792,0.373642358743524));
#61915=DIRECTION('ref_axis',(0.998052578482889,0.0540211804549215,-0.0311891430775903));
#61916=DIRECTION('',(0.137998583506848,0.378681393832731,0.9151812896443));
#61917=DIRECTION('center_axis',(0.99026806874157,-0.0695865504800327,-0.120527440954873));
#61918=DIRECTION('ref_axis',(0.,0.866025403784439,-0.5));
#61919=DIRECTION('',(0.137844537491629,0.371030552991328,0.918332843924613));
#61920=DIRECTION('center_axis',(0.,-0.927183854566787,0.374606593415912));
#61921=DIRECTION('ref_axis',(1.,0.,0.));
#61922=DIRECTION('',(-0.0519254248777279,0.374101236076903,0.925933051260727));
#61923=DIRECTION('center_axis',(-0.649305557988371,-0.717100917309779,0.253315153038431));
#61924=DIRECTION('ref_axis',(0.755033118392644,-0.567841300538901,0.327843327723122));
#61925=DIRECTION('center_axis',(0.,0.788010753606722,-0.615661475325658));
#61926=DIRECTION('ref_axis',(-1.,0.,0.));
#61927=DIRECTION('',(-1.,0.,0.));
#61928=DIRECTION('',(0.137844537491629,0.609784295472662,0.780488306432985));
#61929=DIRECTION('center_axis',(0.99026806874157,-0.0695865504800327,-0.120527440954873));
#61930=DIRECTION('ref_axis',(0.,0.866025403784439,-0.5));
#61931=DIRECTION('center_axis',(-0.99026806874157,0.0695865504800327,0.120527440954873));
#61932=DIRECTION('ref_axis',(0.139173100960065,0.495134034370783,0.857597304086756));
#61933=DIRECTION('',(0.137998583506848,0.603229548983803,0.785538351821795));
#61934=DIRECTION('center_axis',(0.0617712249622996,0.786340650163727,-0.61469724065327));
#61935=DIRECTION('ref_axis',(-0.998052578482889,0.0540211804549215,-0.0311891430775903));
#61936=DIRECTION('center_axis',(-0.0617712249622996,-0.786340650163727,
0.61469724065327));
#61937=DIRECTION('ref_axis',(-0.998090334472114,0.0486661612888524,-0.0380432514219071));
#61938=DIRECTION('',(-0.0161503784824054,0.616580200004832,0.787126433450736));
#61939=DIRECTION('center_axis',(-0.284551435696759,0.751842689509057,-0.594779833782804));
#61940=DIRECTION('ref_axis',(-0.957826285221151,-0.248850568624199,0.143673942783173));
#61941=DIRECTION('center_axis',(0.284551435696759,-0.751842689509057,0.594779833782804));
#61942=DIRECTION('ref_axis',(0.958660774436356,0.223163315348643,-0.176543632679541));
#61943=DIRECTION('',(-0.0552259184163638,0.606541656308365,0.793131336600549));
#61944=DIRECTION('center_axis',(-0.491310548314114,0.675016427497717,-0.550424170729724));
#61945=DIRECTION('ref_axis',(-0.868243142124459,-0.429668924423659,0.248069469178417));
#61946=DIRECTION('center_axis',(0.491310548314114,-0.675016427497717,0.550424170729724));
#61947=DIRECTION('ref_axis',(0.870984468928858,0.380767628982861,-0.310486823558562));
#61948=DIRECTION('',(-0.0570786439550532,0.605644855748342,0.793685288454953));
#61949=DIRECTION('center_axis',(-0.313150259135956,0.744001688360219,-0.590252829658806));
#61950=DIRECTION('ref_axis',(-0.948683298050514,-0.273861278752584,0.158113883008419));
#61951=DIRECTION('center_axis',(0.313150259135956,-0.744001688360219,0.590252829658806));
#61952=DIRECTION('ref_axis',(0.949703593340092,0.245323196775732,-0.194626858168784));
#61953=DIRECTION('',(-0.0225789275220273,0.615504520756066,0.787809860918738));
#61954=DIRECTION('center_axis',(0.,0.788010753606722,-0.615661475325658));
#61955=DIRECTION('ref_axis',(-1.,0.,0.));
#61956=DIRECTION('',(-1.,0.,0.));
#61957=DIRECTION('',(0.0225789275220281,0.615504520756066,0.787809860918738));
#61958=DIRECTION('center_axis',(0.313150259135957,0.744001688360218,-0.590252829658806));
#61959=DIRECTION('ref_axis',(-0.948683298050513,0.273861278752585,-0.15811388300842));
#61960=DIRECTION('center_axis',(-0.313150259135957,-0.744001688360218,0.590252829658806));
#61961=DIRECTION('ref_axis',(-0.949703593340092,0.245323196775733,-0.194626858168784));
#61962=DIRECTION('',(0.0570786439550533,0.605644855748342,0.793685288454953));
#61963=DIRECTION('center_axis',(0.491310548314113,0.675016427497717,-0.550424170729724));
#61964=DIRECTION('ref_axis',(-0.86824314212446,0.429668924423658,-0.248069469178416));
#61965=DIRECTION('center_axis',(-0.491310548314113,-0.675016427497717,0.550424170729724));
#61966=DIRECTION('ref_axis',(-0.870984468928858,0.38076762898286,-0.310486823558561));
#61967=DIRECTION('',(0.0552259184163649,0.606541656308365,0.79313133660055));
#61968=DIRECTION('center_axis',(0.284551435696759,0.751842689509058,-0.594779833782804));
#61969=DIRECTION('ref_axis',(-0.957826285221151,0.248850568624199,-0.143673942783173));
#61970=DIRECTION('center_axis',(-0.284551435696759,-0.751842689509058,0.594779833782804));
#61971=DIRECTION('ref_axis',(-0.958660774436356,0.223163315348643,-0.176543632679541));
#61972=DIRECTION('',(0.0161503784824051,0.616580200004832,0.787126433450736));
#61973=DIRECTION('center_axis',(-0.0617712249622997,0.786340650163727,-0.614697240653271));
#61974=DIRECTION('ref_axis',(-0.998052578482889,-0.0540211804549215,0.0311891430775903));
#61975=DIRECTION('center_axis',(0.0617712249622997,-0.786340650163727,0.614697240653271));
#61976=DIRECTION('ref_axis',(0.998090334472114,0.0486661612888524,-0.0380432514219071));
#61977=DIRECTION('',(-0.137998583506848,0.603229548983803,0.785538351821795));
#61978=DIRECTION('center_axis',(-0.99026806874157,-0.0695865504800329,-0.120527440954873));
#61979=DIRECTION('ref_axis',(0.,-0.866025403784439,0.5));
#61980=DIRECTION('center_axis',(0.99026806874157,0.0695865504800329,0.120527440954873));
#61981=DIRECTION('ref_axis',(-0.139173100960066,0.495134034370784,0.857597304086755));
#61982=DIRECTION('',(-0.137844537491629,0.609784295472662,0.780488306432985));
#61983=DIRECTION('center_axis',(0.,0.788010753606722,-0.615661475325658));
#61984=DIRECTION('ref_axis',(-1.,0.,0.));
#61985=DIRECTION('',(-1.,0.,0.));
#61986=DIRECTION('center_axis',(0.,0.5,0.866025403784439));
#61987=DIRECTION('ref_axis',(1.,0.,0.));
#61988=DIRECTION('center_axis',(1.,0.,0.));
#61989=DIRECTION('ref_axis',(0.,1.,0.));
#61990=DIRECTION('center_axis',(1.,0.,0.));
#61991=DIRECTION('ref_axis',(0.,0.,-1.));
#61992=DIRECTION('center_axis',(0.64930555798837,0.662218828358294,-0.373989994161848));
#61993=DIRECTION('ref_axis',(-0.760527640763576,0.565373752130667,-0.31929645791377));
#61994=DIRECTION('',(1.,0.,0.));
#61995=DIRECTION('center_axis',(-0.99026806874157,0.0894587448987838,0.106612780622095));
#61996=DIRECTION('ref_axis',(0.139173100960065,0.636532044855299,0.758589351257642));
#61997=DIRECTION('center_axis',(-0.0617712249622996,0.846570802931135,-0.528679668032723));
#61998=DIRECTION('ref_axis',(0.998090334472114,0.0523937700909925,-0.0327196743412163));
#61999=DIRECTION('center_axis',(0.284551435696759,0.816055565222214,-0.50307434332588));
#62000=DIRECTION('ref_axis',(-0.958660774436356,0.242223097976277,-0.149323442110948));
#62001=DIRECTION('center_axis',(0.491310548314114,0.748098746816874,-0.446051802065978));
#62002=DIRECTION('ref_axis',(-0.870984468928858,0.42199237598773,-0.25161178329511));
#62003=DIRECTION('center_axis',(0.313150259135956,0.809119792515883,-0.497254539006068));
#62004=DIRECTION('ref_axis',(-0.949703593340092,0.266794897350299,-0.163962091791853));
#62005=DIRECTION('',(1.,0.,0.));
#62006=DIRECTION('center_axis',(-0.313150259135957,0.809119792515883,-0.497254539006068));
#62007=DIRECTION('ref_axis',(0.949703593340092,0.2667948973503,-0.163962091791853));
#62008=DIRECTION('center_axis',(-0.491310548314113,0.748098746816875,-0.446051802065978));
#62009=DIRECTION('ref_axis',(0.870984468928858,0.421992375987729,-0.25161178329511));
#62010=DIRECTION('center_axis',(-0.284551435696759,0.816055565222214,-0.503074343325881));
#62011=DIRECTION('ref_axis',(0.958660774436356,0.242223097976277,-0.149323442110948));
#62012=DIRECTION('center_axis',(0.0617712249622997,0.846570802931135,-0.528679668032723));
#62013=DIRECTION('ref_axis',(-0.998090334472114,0.0523937700909926,-0.0327196743412163));
#62014=DIRECTION('center_axis',(0.99026806874157,0.0894587448987841,0.106612780622095));
#62015=DIRECTION('ref_axis',(-0.139173100960066,0.636532044855299,0.758589351257642));
#62016=DIRECTION('',(1.,0.,0.));
#62017=DIRECTION('center_axis',(0.,-0.848048096156426,0.529919264233205));
#62018=DIRECTION('ref_axis',(1.,0.,0.));
#62019=DIRECTION('',(-0.137844537491629,0.524860590029465,0.839952525157012));
#62020=DIRECTION('center_axis',(-0.99026806874157,-0.0894587448987841,-0.106612780622095));
#62021=DIRECTION('ref_axis',(0.,-0.766044443118978,0.642787609686539));
#62022=DIRECTION('',(-0.137998583506848,0.531847935749546,0.835520295497991));
#62023=DIRECTION('center_axis',(-0.0617712249622997,-0.846570802931135,
0.528679668032723));
#62024=DIRECTION('ref_axis',(0.998052578482889,-0.0477845394804615,0.0400959894540315));
#62025=DIRECTION('',(0.0161503784824051,0.528774052761765,0.848608959651484));
#62026=DIRECTION('center_axis',(0.284551435696759,-0.816055565222214,0.503074343325881));
#62027=DIRECTION('ref_axis',(0.957826285221151,0.220121250980087,-0.184703660511672));
#62028=DIRECTION('',(0.0552259184163645,0.537850200094026,0.841229612052432));
#62029=DIRECTION('center_axis',(0.491310548314113,-0.748098746816875,0.446051802065978));
#62030=DIRECTION('ref_axis',(0.86824314212446,0.3800644767432,-0.318911962258805));
#62031=DIRECTION('',(0.057078643955053,0.538677468419953,0.840576357876501));
#62032=DIRECTION('center_axis',(0.313150259135957,-0.809119792515883,0.497254539006068));
#62033=DIRECTION('ref_axis',(0.948683298050513,0.242244522917128,-0.203267289834479));
#62034=DIRECTION('',(0.0225789275220278,0.529784168481124,0.847831897759644));
#62035=DIRECTION('center_axis',(0.,-0.848048096156426,0.529919264233205));
#62036=DIRECTION('ref_axis',(1.,0.,0.));
#62037=DIRECTION('',(-0.0225789275220274,0.529784168481124,0.847831897759644));
#62038=DIRECTION('center_axis',(-0.313150259135956,-0.809119792515883,0.497254539006068));
#62039=DIRECTION('ref_axis',(0.948683298050513,-0.242244522917128,0.203267289834478));
#62040=DIRECTION('',(-0.0570786439550527,0.538677468419953,0.840576357876501));
#62041=DIRECTION('center_axis',(-0.491310548314114,-0.748098746816874,0.446051802065978));
#62042=DIRECTION('ref_axis',(0.868243142124459,-0.380064476743201,0.318911962258806));
#62043=DIRECTION('',(-0.0552259184163635,0.537850200094025,0.841229612052433));
#62044=DIRECTION('center_axis',(-0.284551435696759,-0.816055565222214,0.50307434332588));
#62045=DIRECTION('ref_axis',(0.957826285221151,-0.220121250980087,0.184703660511673));
#62046=DIRECTION('',(-0.0161503784824052,0.528774052761765,0.848608959651484));
#62047=DIRECTION('center_axis',(0.0617712249622996,-0.846570802931135,0.528679668032723));
#62048=DIRECTION('ref_axis',(0.998052578482889,0.0477845394804615,-0.0400959894540314));
#62049=DIRECTION('',(0.137998583506848,0.531847935749546,0.835520295497991));
#62050=DIRECTION('center_axis',(0.99026806874157,-0.0894587448987838,-0.106612780622095));
#62051=DIRECTION('ref_axis',(0.,0.766044443118978,-0.642787609686539));
#62052=DIRECTION('',(0.137844537491629,0.524860590029465,0.839952525157012));
#62053=DIRECTION('center_axis',(0.,-0.848048096156426,0.529919264233205));
#62054=DIRECTION('ref_axis',(1.,0.,0.));
#62055=DIRECTION('',(-0.051925424877728,0.52920438469299,0.846904049744115));
#62056=DIRECTION('center_axis',(-0.64930555798837,-0.662218828358294,0.373989994161848));
#62057=DIRECTION('ref_axis',(0.755033118392644,-0.502285118831862,0.421467257957652));
#62058=DIRECTION('center_axis',(0.,0.669130606358858,-0.743144825477394));
#62059=DIRECTION('ref_axis',(-1.,0.,0.));
#62060=DIRECTION('',(-1.,0.,0.));
#62061=DIRECTION('',(0.137844537491629,0.736050673949001,0.662743003631831));
#62062=DIRECTION('center_axis',(0.99026806874157,-0.0894587448987839,-0.106612780622095));
#62063=DIRECTION('ref_axis',(0.,0.766044443118978,-0.642787609686539));
#62064=DIRECTION('center_axis',(-0.99026806874157,0.0894587448987839,0.106612780622095));
#62065=DIRECTION('ref_axis',(0.139173100960065,0.636532044855303,0.758589351257639));
#62066=DIRECTION('',(0.137998583506848,0.730472439966645,0.668854547266653));
#62067=DIRECTION('center_axis',(0.0617712249622996,0.667653313133567,-0.741905229276912));
#62068=DIRECTION('ref_axis',(-0.998052578482889,0.0477845394804615,-0.0400959894540314));
#62069=DIRECTION('center_axis',(-0.0617712249622996,-0.667653313133567,
0.741905229276912));
#62070=DIRECTION('ref_axis',(-0.998090334472114,0.0413206716646654,-0.045916079171941));
#62071=DIRECTION('',(-0.0161503784824054,0.743896032080767,0.668100186146782));
#62072=DIRECTION('center_axis',(-0.284551435696759,0.637138075424646,-0.71629990457007));
#62073=DIRECTION('ref_axis',(-0.957826285221151,-0.220121250980087,0.184703660511673));
#62074=DIRECTION('center_axis',(0.284551435696759,-0.637138075424646,0.71629990457007));
#62075=DIRECTION('ref_axis',(0.958660774436356,0.18911648304975,-0.212613441240154));
#62076=DIRECTION('',(-0.0552259184163638,0.735052736908566,0.675757036144127));
#62077=DIRECTION('center_axis',(-0.491310548314114,0.569181257019307,-0.659277363310167));
#62078=DIRECTION('ref_axis',(-0.868243142124459,-0.380064476743201,0.318911962258806));
#62079=DIRECTION('center_axis',(0.491310548314114,-0.569181257019307,0.659277363310167));
#62080=DIRECTION('ref_axis',(0.870984468928858,0.32106744201786,-0.371889435936037));
#62081=DIRECTION('',(-0.0570786439550532,0.734265753494182,0.676458300008118));
#62082=DIRECTION('center_axis',(-0.313150259135956,0.630202302718316,-0.710480100250258));
#62083=DIRECTION('ref_axis',(-0.948683298050513,-0.242244522917128,0.203267289834478));
#62084=DIRECTION('center_axis',(0.313150259135956,-0.630202302718316,0.710480100250258));
#62085=DIRECTION('ref_axis',(0.949703593340092,0.207799586932431,-0.234269964928557));
#62086=DIRECTION('',(-0.0225789275220273,0.742955370751214,0.668960020557194));
#62087=DIRECTION('center_axis',(0.,0.669130606358858,-0.743144825477394));
#62088=DIRECTION('ref_axis',(-1.,0.,0.));
#62089=DIRECTION('',(-1.,0.,0.));
#62090=DIRECTION('',(0.0225789275220281,0.742955370751214,0.668960020557194));
#62091=DIRECTION('center_axis',(0.313150259135957,0.630202302718315,-0.710480100250258));
#62092=DIRECTION('ref_axis',(-0.948683298050513,0.242244522917128,-0.203267289834479));
#62093=DIRECTION('center_axis',(-0.313150259135957,-0.630202302718315,0.710480100250258));
#62094=DIRECTION('ref_axis',(-0.949703593340092,0.207799586932432,-0.234269964928558));
#62095=DIRECTION('',(0.0570786439550534,0.734265753494182,0.676458300008118));
#62096=DIRECTION('center_axis',(0.491310548314113,0.569181257019307,-0.659277363310168));
#62097=DIRECTION('ref_axis',(-0.86824314212446,0.3800644767432,-0.318911962258805));
#62098=DIRECTION('center_axis',(-0.491310548314113,-0.569181257019307,0.659277363310168));
#62099=DIRECTION('ref_axis',(-0.870984468928858,0.321067442017859,-0.371889435936036));
#62100=DIRECTION('',(0.0552259184163649,0.735052736908566,0.675757036144127));
#62101=DIRECTION('center_axis',(0.284551435696759,0.637138075424647,-0.71629990457007));
#62102=DIRECTION('ref_axis',(-0.957826285221151,0.220121250980087,-0.184703660511672));
#62103=DIRECTION('center_axis',(-0.284551435696759,-0.637138075424647,0.71629990457007));
#62104=DIRECTION('ref_axis',(-0.958660774436356,0.189116483049749,-0.212613441240154));
#62105=DIRECTION('',(0.016150378482405,0.743896032080767,0.668100186146782));
#62106=DIRECTION('center_axis',(-0.0617712249622997,0.667653313133567,-0.741905229276912));
#62107=DIRECTION('ref_axis',(-0.998052578482889,-0.0477845394804615,0.0400959894540315));
#62108=DIRECTION('center_axis',(0.0617712249622997,-0.667653313133567,0.741905229276912));
#62109=DIRECTION('ref_axis',(0.998090334472114,0.0413206716646654,-0.045916079171941));
#62110=DIRECTION('',(-0.137998583506848,0.730472439966645,0.668854547266653));
#62111=DIRECTION('center_axis',(-0.99026806874157,-0.0894587448987841,-0.106612780622095));
#62112=DIRECTION('ref_axis',(0.,-0.766044443118978,0.642787609686539));
#62113=DIRECTION('center_axis',(0.99026806874157,0.0894587448987841,0.106612780622095));
#62114=DIRECTION('ref_axis',(-0.139173100960066,0.636532044855299,0.758589351257642));
#62115=DIRECTION('',(-0.137844537491629,0.736050673949001,0.662743003631831));
#62116=DIRECTION('center_axis',(0.,0.669130606358858,-0.743144825477394));
#62117=DIRECTION('ref_axis',(-1.,0.,0.));
#62118=DIRECTION('',(-1.,0.,0.));
#62119=DIRECTION('center_axis',(0.,0.642787609686539,0.766044443118978));
#62120=DIRECTION('ref_axis',(1.,0.,0.));
#62121=DIRECTION('center_axis',(1.,0.,0.));
#62122=DIRECTION('ref_axis',(0.,1.,0.));
#62123=DIRECTION('center_axis',(1.,0.,0.));
#62124=DIRECTION('ref_axis',(0.,0.,-1.));
#62125=DIRECTION('center_axis',(0.64930555798837,0.587215555406038,-0.483301338560726));
#62126=DIRECTION('ref_axis',(-0.760527640763576,0.501339206395651,-0.412621749021023));
#62127=DIRECTION('',(1.,0.,0.));
#62128=DIRECTION('center_axis',(-0.99026806874157,0.106612780622095,0.0894587448987838));
#62129=DIRECTION('ref_axis',(0.139173100960065,0.758589351257642,0.636532044855299));
#62130=DIRECTION('center_axis',(-0.0617712249622996,0.741905229276912,-0.667653313133568));
#62131=DIRECTION('ref_axis',(0.998090334472114,0.045916079171941,-0.0413206716646654));
#62132=DIRECTION('center_axis',(0.284551435696759,0.71629990457007,-0.637138075424647));
#62133=DIRECTION('ref_axis',(-0.958660774436356,0.212613441240154,-0.18911648304975));
#62134=DIRECTION('center_axis',(0.491310548314114,0.659277363310167,-0.569181257019307));
#62135=DIRECTION('ref_axis',(-0.870984468928858,0.371889435936037,-0.32106744201786));
#62136=DIRECTION('center_axis',(0.313150259135956,0.710480100250258,-0.630202302718316));
#62137=DIRECTION('ref_axis',(-0.949703593340092,0.234269964928557,-0.207799586932431));
#62138=DIRECTION('',(1.,0.,0.));
#62139=DIRECTION('center_axis',(-0.313150259135957,0.710480100250258,-0.630202302718315));
#62140=DIRECTION('ref_axis',(0.949703593340092,0.234269964928558,-0.207799586932432));
#62141=DIRECTION('center_axis',(-0.491310548314113,0.659277363310168,-0.569181257019307));
#62142=DIRECTION('ref_axis',(0.870984468928858,0.371889435936036,-0.321067442017859));
#62143=DIRECTION('center_axis',(-0.284551435696759,0.71629990457007,-0.637138075424647));
#62144=DIRECTION('ref_axis',(0.958660774436356,0.212613441240154,-0.189116483049749));
#62145=DIRECTION('center_axis',(0.0617712249622997,0.741905229276912,-0.667653313133568));
#62146=DIRECTION('ref_axis',(-0.998090334472114,0.045916079171941,-0.0413206716646654));
#62147=DIRECTION('center_axis',(0.99026806874157,0.106612780622095,0.0894587448987841));
#62148=DIRECTION('ref_axis',(-0.139173100960066,0.758589351257642,0.636532044855299));
#62149=DIRECTION('',(1.,0.,0.));
#62150=DIRECTION('center_axis',(0.,-0.743144825477394,0.669130606358858));
#62151=DIRECTION('ref_axis',(1.,0.,0.));
#62152=DIRECTION('',(-0.137844537491629,0.662743003631831,0.736050673949001));
#62153=DIRECTION('center_axis',(-0.99026806874157,-0.106612780622095,-0.0894587448987841));
#62154=DIRECTION('ref_axis',(0.,-0.642787609686539,0.766044443118978));
#62155=DIRECTION('',(-0.137998583506848,0.668854547266653,0.730472439966645));
#62156=DIRECTION('center_axis',(-0.0617712249622997,-0.741905229276912,
0.667653313133568));
#62157=DIRECTION('ref_axis',(0.998052578482889,-0.0400959894540315,0.0477845394804616));
#62158=DIRECTION('',(0.0161503784824051,0.668100186146782,0.743896032080767));
#62159=DIRECTION('center_axis',(0.284551435696759,-0.71629990457007,0.637138075424647));
#62160=DIRECTION('ref_axis',(0.957826285221151,0.184703660511672,-0.220121250980087));
#62161=DIRECTION('',(0.0552259184163645,0.675757036144128,0.735052736908566));
#62162=DIRECTION('center_axis',(0.491310548314113,-0.659277363310168,0.569181257019307));
#62163=DIRECTION('ref_axis',(0.86824314212446,0.318911962258805,-0.3800644767432));
#62164=DIRECTION('',(0.057078643955053,0.676458300008118,0.734265753494182));
#62165=DIRECTION('center_axis',(0.313150259135957,-0.710480100250258,0.630202302718315));
#62166=DIRECTION('ref_axis',(0.948683298050513,0.203267289834479,-0.242244522917128));
#62167=DIRECTION('',(0.0225789275220278,0.668960020557194,0.742955370751214));
#62168=DIRECTION('center_axis',(0.,-0.743144825477394,0.669130606358858));
#62169=DIRECTION('ref_axis',(1.,0.,0.));
#62170=DIRECTION('',(-0.0225789275220274,0.668960020557194,0.742955370751214));
#62171=DIRECTION('center_axis',(-0.313150259135956,-0.710480100250258,0.630202302718316));
#62172=DIRECTION('ref_axis',(0.948683298050514,-0.203267289834478,0.242244522917128));
#62173=DIRECTION('',(-0.0570786439550527,0.676458300008118,0.734265753494182));
#62174=DIRECTION('center_axis',(-0.491310548314114,-0.659277363310167,0.569181257019307));
#62175=DIRECTION('ref_axis',(0.868243142124459,-0.318911962258806,0.380064476743201));
#62176=DIRECTION('',(-0.0552259184163635,0.675757036144127,0.735052736908566));
#62177=DIRECTION('center_axis',(-0.284551435696759,-0.71629990457007,0.637138075424647));
#62178=DIRECTION('ref_axis',(0.957826285221151,-0.184703660511673,0.220121250980087));
#62179=DIRECTION('',(-0.0161503784824052,0.668100186146782,0.743896032080767));
#62180=DIRECTION('center_axis',(0.0617712249622996,-0.741905229276912,0.667653313133568));
#62181=DIRECTION('ref_axis',(0.998052578482889,0.0400959894540314,-0.0477845394804615));
#62182=DIRECTION('',(0.137998583506848,0.668854547266653,0.730472439966645));
#62183=DIRECTION('center_axis',(0.99026806874157,-0.106612780622095,-0.0894587448987838));
#62184=DIRECTION('ref_axis',(0.,0.642787609686539,-0.766044443118978));
#62185=DIRECTION('',(0.137844537491629,0.662743003631831,0.736050673949001));
#62186=DIRECTION('center_axis',(0.,-0.743144825477394,0.669130606358858));
#62187=DIRECTION('ref_axis',(1.,0.,0.));
#62188=DIRECTION('',(-0.0519254248777279,0.66822792587052,0.742142297230154));
#62189=DIRECTION('center_axis',(-0.64930555798837,-0.587215555406038,0.483301338560726));
#62190=DIRECTION('ref_axis',(0.755033118392644,-0.421467257957652,0.502285118831862));
#62191=DIRECTION('center_axis',(0.,0.529919264233205,-0.848048096156426));
#62192=DIRECTION('ref_axis',(-1.,0.,0.));
#62193=DIRECTION('',(-1.,0.,0.));
#62194=DIRECTION('',(0.137844537491629,0.839952525157012,0.524860590029465));
#62195=DIRECTION('center_axis',(0.99026806874157,-0.106612780622095,-0.0894587448987839));
#62196=DIRECTION('ref_axis',(0.,0.642787609686539,-0.766044443118978));
#62197=DIRECTION('center_axis',(-0.99026806874157,0.106612780622095,0.0894587448987839));
#62198=DIRECTION('ref_axis',(0.139173100960065,0.758589351257639,0.636532044855303));
#62199=DIRECTION('',(0.137998583506848,0.835520295497991,0.531847935749546));
#62200=DIRECTION('center_axis',(0.0617712249622996,0.528679668032723,-0.846570802931135));
#62201=DIRECTION('ref_axis',(-0.998052578482889,0.0400959894540314,-0.0477845394804615));
#62202=DIRECTION('center_axis',(-0.0617712249622996,-0.528679668032723,
0.846570802931135));
#62203=DIRECTION('ref_axis',(-0.998090334472114,0.0327196743412163,-0.0523937700909925));
#62204=DIRECTION('',(-0.0161503784824054,0.848608959651484,0.528774052761765));
#62205=DIRECTION('center_axis',(-0.284551435696759,0.50307434332588,-0.816055565222214));
#62206=DIRECTION('ref_axis',(-0.957826285221151,-0.184703660511673,0.220121250980087));
#62207=DIRECTION('center_axis',(0.284551435696759,-0.50307434332588,0.816055565222214));
#62208=DIRECTION('ref_axis',(0.958660774436356,0.149323442110948,-0.242223097976277));
#62209=DIRECTION('',(-0.0552259184163638,0.841229612052433,0.537850200094025));
#62210=DIRECTION('center_axis',(-0.491310548314114,0.446051802065978,-0.748098746816874));
#62211=DIRECTION('ref_axis',(-0.868243142124459,-0.318911962258806,0.380064476743201));
#62212=DIRECTION('center_axis',(0.491310548314114,-0.446051802065978,0.748098746816874));
#62213=DIRECTION('ref_axis',(0.870984468928858,0.25161178329511,-0.421992375987731));
#62214=DIRECTION('',(-0.0570786439550532,0.840576357876501,0.538677468419953));
#62215=DIRECTION('center_axis',(-0.313150259135956,0.497254539006068,-0.809119792515883));
#62216=DIRECTION('ref_axis',(-0.948683298050514,-0.203267289834478,0.242244522917128));
#62217=DIRECTION('center_axis',(0.313150259135956,-0.497254539006068,0.809119792515883));
#62218=DIRECTION('ref_axis',(0.949703593340092,0.163962091791853,-0.266794897350299));
#62219=DIRECTION('',(-0.0225789275220273,0.847831897759644,0.529784168481124));
#62220=DIRECTION('center_axis',(0.,0.529919264233205,-0.848048096156426));
#62221=DIRECTION('ref_axis',(-1.,0.,0.));
#62222=DIRECTION('',(-1.,0.,0.));
#62223=DIRECTION('',(0.0225789275220281,0.847831897759644,0.529784168481124));
#62224=DIRECTION('center_axis',(0.313150259135957,0.497254539006068,-0.809119792515883));
#62225=DIRECTION('ref_axis',(-0.948683298050513,0.203267289834479,-0.242244522917128));
#62226=DIRECTION('center_axis',(-0.313150259135957,-0.497254539006068,0.809119792515883));
#62227=DIRECTION('ref_axis',(-0.949703593340092,0.163962091791853,-0.2667948973503));
#62228=DIRECTION('',(0.0570786439550534,0.840576357876501,0.538677468419953));
#62229=DIRECTION('center_axis',(0.491310548314113,0.446051802065978,-0.748098746816875));
#62230=DIRECTION('ref_axis',(-0.86824314212446,0.318911962258805,-0.3800644767432));
#62231=DIRECTION('center_axis',(-0.491310548314113,-0.446051802065978,0.748098746816875));
#62232=DIRECTION('ref_axis',(-0.870984468928858,0.25161178329511,-0.421992375987729));
#62233=DIRECTION('',(0.0552259184163649,0.841229612052432,0.537850200094026));
#62234=DIRECTION('center_axis',(0.284551435696759,0.50307434332588,-0.816055565222214));
#62235=DIRECTION('ref_axis',(-0.957826285221151,0.184703660511672,-0.220121250980087));
#62236=DIRECTION('center_axis',(-0.284551435696759,-0.50307434332588,0.816055565222214));
#62237=DIRECTION('ref_axis',(-0.958660774436356,0.149323442110947,-0.242223097976277));
#62238=DIRECTION('',(0.0161503784824051,0.848608959651484,0.528774052761765));
#62239=DIRECTION('center_axis',(-0.0617712249622997,0.528679668032723,-0.846570802931135));
#62240=DIRECTION('ref_axis',(-0.998052578482889,-0.0400959894540315,0.0477845394804616));
#62241=DIRECTION('center_axis',(0.0617712249622997,-0.528679668032723,0.846570802931135));
#62242=DIRECTION('ref_axis',(0.998090334472114,0.0327196743412163,-0.0523937700909926));
#62243=DIRECTION('',(-0.137998583506848,0.835520295497991,0.531847935749546));
#62244=DIRECTION('center_axis',(-0.99026806874157,-0.106612780622095,-0.0894587448987841));
#62245=DIRECTION('ref_axis',(0.,-0.642787609686539,0.766044443118978));
#62246=DIRECTION('center_axis',(0.99026806874157,0.106612780622095,0.0894587448987841));
#62247=DIRECTION('ref_axis',(-0.139173100960066,0.758589351257642,0.636532044855299));
#62248=DIRECTION('',(-0.137844537491629,0.839952525157012,0.524860590029465));
#62249=DIRECTION('center_axis',(0.,0.529919264233205,-0.848048096156426));
#62250=DIRECTION('ref_axis',(-1.,0.,0.));
#62251=DIRECTION('',(-1.,0.,0.));
#62252=DIRECTION('center_axis',(0.,0.766044443118978,0.642787609686539));
#62253=DIRECTION('ref_axis',(1.,0.,0.));
#62254=DIRECTION('center_axis',(1.,0.,0.));
#62255=DIRECTION('ref_axis',(0.,1.,0.));
#62256=DIRECTION('center_axis',(1.,0.,0.));
#62257=DIRECTION('ref_axis',(0.,0.,-1.));
#62258=DIRECTION('center_axis',(0.64930555798837,0.494370034948177,-0.577927816349714));
#62259=DIRECTION('ref_axis',(-0.760527640763576,0.422071722564183,-0.49340973708095));
#62260=DIRECTION('',(1.,0.,0.));
#62261=DIRECTION('center_axis',(-0.99026806874157,0.120527440954873,0.0695865504800327));
#62262=DIRECTION('ref_axis',(0.139173100960065,0.857597304086756,0.495134034370783));
#62263=DIRECTION('center_axis',(-0.0617712249622996,0.61469724065327,-0.786340650163727));
#62264=DIRECTION('ref_axis',(0.998090334472114,0.0380432514219071,-0.0486661612888524));
#62265=DIRECTION('center_axis',(0.284551435696759,0.594779833782804,-0.751842689509058));
#62266=DIRECTION('ref_axis',(-0.958660774436356,0.176543632679541,-0.223163315348643));
#62267=DIRECTION('center_axis',(0.491310548314114,0.550424170729724,-0.675016427497717));
#62268=DIRECTION('ref_axis',(-0.870984468928858,0.310486823558562,-0.380767628982861));
#62269=DIRECTION('center_axis',(0.313150259135956,0.590252829658806,-0.744001688360219));
#62270=DIRECTION('ref_axis',(-0.949703593340092,0.194626858168784,-0.245323196775732));
#62271=DIRECTION('',(1.,0.,0.));
#62272=DIRECTION('center_axis',(-0.313150259135957,0.590252829658806,-0.744001688360219));
#62273=DIRECTION('ref_axis',(0.949703593340092,0.194626858168784,-0.245323196775733));
#62274=DIRECTION('center_axis',(-0.491310548314113,0.550424170729724,-0.675016427497717));
#62275=DIRECTION('ref_axis',(0.870984468928858,0.310486823558561,-0.38076762898286));
#62276=DIRECTION('center_axis',(-0.284551435696759,0.594779833782804,-0.751842689509058));
#62277=DIRECTION('ref_axis',(0.958660774436356,0.176543632679541,-0.223163315348643));
#62278=DIRECTION('center_axis',(0.0617712249622997,0.61469724065327,-0.786340650163727));
#62279=DIRECTION('ref_axis',(-0.998090334472114,0.0380432514219071,-0.0486661612888524));
#62280=DIRECTION('center_axis',(0.99026806874157,0.120527440954873,0.0695865504800329));
#62281=DIRECTION('ref_axis',(-0.139173100960066,0.857597304086755,0.495134034370784));
#62282=DIRECTION('',(1.,0.,0.));
#62283=DIRECTION('center_axis',(0.,-0.615661475325658,0.788010753606722));
#62284=DIRECTION('ref_axis',(1.,0.,0.));
#62285=DIRECTION('',(-0.137844537491629,0.780488306432985,0.609784295472662));
#62286=DIRECTION('center_axis',(-0.99026806874157,-0.120527440954873,-0.0695865504800329));
#62287=DIRECTION('ref_axis',(0.,-0.5,0.866025403784439));
#62288=DIRECTION('',(-0.137998583506848,0.785538351821795,0.603229548983802));
#62289=DIRECTION('center_axis',(-0.0617712249622997,-0.61469724065327,0.786340650163727));
#62290=DIRECTION('ref_axis',(0.998052578482889,-0.0311891430775903,0.0540211804549215));
#62291=DIRECTION('',(0.0161503784824051,0.787126433450736,0.616580200004832));
#62292=DIRECTION('center_axis',(0.284551435696759,-0.594779833782804,0.751842689509058));
#62293=DIRECTION('ref_axis',(0.957826285221151,0.143673942783173,-0.248850568624199));
#62294=DIRECTION('',(0.0552259184163645,0.79313133660055,0.606541656308365));
#62295=DIRECTION('center_axis',(0.491310548314113,-0.550424170729724,0.675016427497717));
#62296=DIRECTION('ref_axis',(0.86824314212446,0.248069469178416,-0.429668924423658));
#62297=DIRECTION('',(0.057078643955053,0.793685288454953,0.605644855748342));
#62298=DIRECTION('center_axis',(0.313150259135957,-0.590252829658806,0.744001688360219));
#62299=DIRECTION('ref_axis',(0.948683298050513,0.15811388300842,-0.273861278752585));
#62300=DIRECTION('',(0.0225789275220278,0.787809860918738,0.615504520756066));
#62301=DIRECTION('center_axis',(0.,-0.615661475325658,0.788010753606722));
#62302=DIRECTION('ref_axis',(1.,0.,0.));
#62303=DIRECTION('',(-0.0225789275220274,0.787809860918738,0.615504520756066));
#62304=DIRECTION('center_axis',(-0.313150259135956,-0.590252829658806,0.744001688360219));
#62305=DIRECTION('ref_axis',(0.948683298050514,-0.158113883008419,0.273861278752584));
#62306=DIRECTION('',(-0.0570786439550527,0.793685288454953,0.605644855748342));
#62307=DIRECTION('center_axis',(-0.491310548314114,-0.550424170729724,0.675016427497717));
#62308=DIRECTION('ref_axis',(0.868243142124459,-0.248069469178417,0.429668924423659));
#62309=DIRECTION('',(-0.0552259184163635,0.793131336600549,0.606541656308365));
#62310=DIRECTION('center_axis',(-0.284551435696759,-0.594779833782804,0.751842689509058));
#62311=DIRECTION('ref_axis',(0.957826285221151,-0.143673942783173,0.248850568624199));
#62312=DIRECTION('',(-0.0161503784824052,0.787126433450736,0.616580200004832));
#62313=DIRECTION('center_axis',(0.0617712249622996,-0.61469724065327,0.786340650163727));
#62314=DIRECTION('ref_axis',(0.998052578482889,0.0311891430775903,-0.0540211804549215));
#62315=DIRECTION('',(0.137998583506848,0.785538351821795,0.603229548983803));
#62316=DIRECTION('center_axis',(0.99026806874157,-0.120527440954873,-0.0695865504800327));
#62317=DIRECTION('ref_axis',(0.,0.5,-0.866025403784439));
#62318=DIRECTION('',(0.137844537491629,0.780488306432985,0.609784295472661));
#62319=DIRECTION('center_axis',(0.,-0.615661475325658,0.788010753606722));
#62320=DIRECTION('ref_axis',(1.,0.,0.));
#62321=DIRECTION('',(-0.0519254248777279,0.786947699660121,0.614830926556978));
#62322=DIRECTION('center_axis',(-0.64930555798837,-0.494370034948177,0.577927816349714));
#62323=DIRECTION('ref_axis',(0.755033118392644,-0.327843327723121,0.567841300538901));
#62324=DIRECTION('center_axis',(0.,0.374606593415912,-0.927183854566788));
#62325=DIRECTION('ref_axis',(-1.,0.,0.));
#62326=DIRECTION('',(-1.,0.,0.));
#62327=DIRECTION('',(0.137844537491629,0.918332843924614,0.371030552991328));
#62328=DIRECTION('center_axis',(0.99026806874157,-0.120527440954873,-0.0695865504800327));
#62329=DIRECTION('ref_axis',(0.,0.5,-0.866025403784439));
#62330=DIRECTION('center_axis',(-0.99026806874157,0.120527440954873,0.0695865504800327));
#62331=DIRECTION('ref_axis',(0.139173100960065,0.857597304086756,0.495134034370783));
#62332=DIRECTION('',(0.137998583506848,0.9151812896443,0.378681393832731));
#62333=DIRECTION('center_axis',(0.0617712249622996,0.373642358743524,-0.925513751123792));
#62334=DIRECTION('ref_axis',(-0.998052578482889,0.0311891430775903,-0.0540211804549215));
#62335=DIRECTION('center_axis',(-0.0617712249622996,-0.373642358743524,
0.925513751123792));
#62336=DIRECTION('ref_axis',(-0.998090334472114,0.0231245062698634,-0.0572795028183562));
#62337=DIRECTION('',(-0.0161503784824054,0.927537333400043,0.373381387356162));
#62338=DIRECTION('center_axis',(-0.284551435696759,0.353724951873058,-0.891015790469123));
#62339=DIRECTION('ref_axis',(-0.957826285221151,-0.143673942783173,0.248850568624199));
#62340=DIRECTION('center_axis',(0.284551435696759,-0.353724951873058,0.891015790469123));
#62341=DIRECTION('ref_axis',(0.958660774436356,0.104993283944912,-0.264472928451193));
#62342=DIRECTION('',(-0.0552259184163638,0.921846151116809,0.3836010578794));
#62343=DIRECTION('center_axis',(-0.491310548314114,0.309369288819977,-0.814189528457782));
#62344=DIRECTION('ref_axis',(-0.868243142124459,-0.248069469178417,0.429668924423659));
#62345=DIRECTION('center_axis',(0.491310548314114,-0.309369288819977,0.814189528457782));
#62346=DIRECTION('ref_axis',(0.870984468928858,0.174511027858645,-0.459273291233482));
#62347=DIRECTION('',(-0.0570786439550532,0.921346474976903,0.384529194537798));
#62348=DIRECTION('center_axis',(-0.313150259135956,0.34919794774906,-0.883174789320284));
#62349=DIRECTION('ref_axis',(-0.948683298050514,-0.158113883008419,0.273861278752584));
#62350=DIRECTION('center_axis',(0.313150259135956,-0.34919794774906,0.883174789320284));
#62351=DIRECTION('ref_axis',(0.949703593340092,0.115142691461001,-0.291213401820783));
#62352=DIRECTION('',(-0.0225789275220273,0.926947481578288,0.374511092529479));
#62353=DIRECTION('center_axis',(0.,0.374606593415912,-0.927183854566788));
#62354=DIRECTION('ref_axis',(-1.,0.,0.));
#62355=DIRECTION('',(-1.,0.,0.));
#62356=DIRECTION('',(0.0225789275220281,0.926947481578288,0.374511092529479));
#62357=DIRECTION('center_axis',(0.313150259135957,0.349197947749059,-0.883174789320284));
#62358=DIRECTION('ref_axis',(-0.948683298050513,0.15811388300842,-0.273861278752585));
#62359=DIRECTION('center_axis',(-0.313150259135957,-0.349197947749059,0.883174789320284));
#62360=DIRECTION('ref_axis',(-0.949703593340092,0.115142691461001,-0.291213401820784));
#62361=DIRECTION('',(0.0570786439550534,0.921346474976903,0.384529194537798));
#62362=DIRECTION('center_axis',(0.491310548314113,0.309369288819978,-0.814189528457783));
#62363=DIRECTION('ref_axis',(-0.86824314212446,0.248069469178416,-0.429668924423658));
#62364=DIRECTION('center_axis',(-0.491310548314113,-0.309369288819978,0.814189528457783));
#62365=DIRECTION('ref_axis',(-0.870984468928858,0.174511027858644,-0.459273291233481));
#62366=DIRECTION('',(0.0552259184163649,0.921846151116809,0.3836010578794));
#62367=DIRECTION('center_axis',(0.284551435696759,0.353724951873058,-0.891015790469123));
#62368=DIRECTION('ref_axis',(-0.957826285221151,0.143673942783173,-0.248850568624199));
#62369=DIRECTION('center_axis',(-0.284551435696759,-0.353724951873058,0.891015790469123));
#62370=DIRECTION('ref_axis',(-0.958660774436356,0.104993283944912,-0.264472928451193));
#62371=DIRECTION('',(0.0161503784824051,0.927537333400043,0.373381387356162));
#62372=DIRECTION('center_axis',(-0.0617712249622997,0.373642358743524,-0.925513751123792));
#62373=DIRECTION('ref_axis',(-0.998052578482889,-0.0311891430775903,0.0540211804549215));
#62374=DIRECTION('center_axis',(0.0617712249622997,-0.373642358743524,0.925513751123792));
#62375=DIRECTION('ref_axis',(0.998090334472114,0.0231245062698634,-0.0572795028183563));
#62376=DIRECTION('',(-0.137998583506848,0.9151812896443,0.378681393832731));
#62377=DIRECTION('center_axis',(-0.99026806874157,-0.120527440954873,-0.0695865504800329));
#62378=DIRECTION('ref_axis',(0.,-0.5,0.866025403784439));
#62379=DIRECTION('center_axis',(0.99026806874157,0.120527440954873,0.0695865504800329));
#62380=DIRECTION('ref_axis',(-0.139173100960066,0.857597304086755,0.495134034370784));
#62381=DIRECTION('',(-0.137844537491629,0.918332843924613,0.371030552991328));
#62382=DIRECTION('center_axis',(0.,0.374606593415912,-0.927183854566787));
#62383=DIRECTION('ref_axis',(-1.,0.,0.));
#62384=DIRECTION('',(-1.,0.,0.));
#62385=DIRECTION('center_axis',(0.,0.866025403784439,0.5));
#62386=DIRECTION('ref_axis',(1.,0.,0.));
#62387=DIRECTION('center_axis',(1.,0.,0.));
#62388=DIRECTION('ref_axis',(0.,1.,0.));
#62389=DIRECTION('center_axis',(1.,0.,0.));
#62390=DIRECTION('ref_axis',(0.,0.,-1.));
#62391=DIRECTION('center_axis',(0.64930555798837,0.386503331141725,-0.654994249884502));
#62392=DIRECTION('ref_axis',(-0.760527640763576,0.329979803021199,-0.559205719957048));
#62393=DIRECTION('',(1.,0.,0.));
#62394=DIRECTION('center_axis',(-0.99026806874157,0.130779935984066,0.0476000039374393));
#62395=DIRECTION('ref_axis',(0.139173100960065,0.930547596796367,0.338691626801823));
#62396=DIRECTION('center_axis',(-0.0617712249622996,0.468811987424192,-0.881135424446229));
#62397=DIRECTION('ref_axis',(0.998090334472114,0.0290144987282327,-0.0545329542285434));
#62398=DIRECTION('center_axis',(0.284551435696759,0.455187678719166,-0.843702943923494));
#62399=DIRECTION('ref_axis',(-0.958660774436356,0.135109635175349,-0.250429443236754));
#62400=DIRECTION('center_axis',(0.491310548314114,0.424846618249727,-0.760341565401402));
#62401=DIRECTION('ref_axis',(-0.870984468928858,0.239650226161174,-0.428898384218936));
#62402=DIRECTION('center_axis',(0.313150259135956,0.452091025520515,-0.835194959184317));
#62403=DIRECTION('ref_axis',(-0.949703593340092,0.149070112809494,-0.27539278542453));
#62404=DIRECTION('',(1.,0.,0.));
#62405=DIRECTION('center_axis',(-0.313150259135957,0.452091025520515,-0.835194959184317));
#62406=DIRECTION('ref_axis',(0.949703593340092,0.149070112809494,-0.275392785424531));
#62407=DIRECTION('center_axis',(-0.491310548314113,0.424846618249727,-0.760341565401403));
#62408=DIRECTION('ref_axis',(0.870984468928858,0.239650226161173,-0.428898384218935));
#62409=DIRECTION('center_axis',(-0.284551435696759,0.455187678719166,-0.843702943923494));
#62410=DIRECTION('ref_axis',(0.958660774436356,0.135109635175349,-0.250429443236754));
#62411=DIRECTION('center_axis',(0.0617712249622997,0.468811987424191,-0.881135424446229));
#62412=DIRECTION('ref_axis',(-0.998090334472114,0.0290144987282327,-0.0545329542285435));
#62413=DIRECTION('center_axis',(0.99026806874157,0.130779935984066,0.0476000039374394));
#62414=DIRECTION('ref_axis',(-0.139173100960066,0.930547596796366,0.338691626801825));
#62415=DIRECTION('',(1.,0.,0.));
#62416=DIRECTION('center_axis',(0.,-0.469471562785891,0.882947592858927));
#62417=DIRECTION('ref_axis',(1.,0.,0.));
#62418=DIRECTION('',(-0.137844537491629,0.874518866989312,0.464989929744128));
#62419=DIRECTION('center_axis',(-0.99026806874157,-0.130779935984066,-0.0476000039374394));
#62420=DIRECTION('ref_axis',(0.,-0.342020143325669,0.939692620785908));
#62421=DIRECTION('',(-0.137998583506848,0.878353971058417,0.457657833403968));
#62422=DIRECTION('center_axis',(-0.0617712249622997,-0.468811987424191,
0.881135424446229));
#62423=DIRECTION('ref_axis',(0.998052578482889,-0.0213346303712044,0.058616415197295));
#62424=DIRECTION('',(0.0161503784824051,0.882236242379483,0.470529890556386));
#62425=DIRECTION('center_axis',(0.284551435696759,-0.455187678719166,0.843702943923494));
#62426=DIRECTION('ref_axis',(0.957826285221151,0.0982787650057293,-0.270018687665128));
#62427=DIRECTION('',(0.0552259184163645,0.886406742738186,0.459601114406122));
#62428=DIRECTION('center_axis',(0.491310548314113,-0.424846618249727,0.760341565401403));
#62429=DIRECTION('ref_axis',(0.86824314212446,0.169689510806249,-0.46621809925847));
#62430=DIRECTION('',(0.057078643955053,0.886796551036219,0.458621745531673));
#62431=DIRECTION('center_axis',(0.313150259135957,-0.452091025520515,0.835194959184317));
#62432=DIRECTION('ref_axis',(0.948683298050513,0.108156265856636,-0.297156898213637));
#62433=DIRECTION('',(0.0225789275220278,0.88272249730729,0.469351877358061));
#62434=DIRECTION('center_axis',(0.,-0.469471562785891,0.882947592858927));
#62435=DIRECTION('ref_axis',(1.,0.,0.));
#62436=DIRECTION('',(-0.0225789275220274,0.88272249730729,0.469351877358061));
#62437=DIRECTION('center_axis',(-0.313150259135956,-0.452091025520515,0.835194959184317));
#62438=DIRECTION('ref_axis',(0.948683298050514,-0.108156265856635,0.297156898213636));
#62439=DIRECTION('',(-0.0570786439550527,0.886796551036219,0.458621745531673));
#62440=DIRECTION('center_axis',(-0.491310548314114,-0.424846618249727,0.760341565401402));
#62441=DIRECTION('ref_axis',(0.868243142124459,-0.169689510806249,0.466218099258471));
#62442=DIRECTION('',(-0.0552259184163635,0.886406742738186,0.459601114406122));
#62443=DIRECTION('center_axis',(-0.284551435696759,-0.455187678719166,0.843702943923494));
#62444=DIRECTION('ref_axis',(0.957826285221151,-0.0982787650057295,0.270018687665129));
#62445=DIRECTION('',(-0.0161503784824052,0.882236242379483,0.470529890556386));
#62446=DIRECTION('center_axis',(0.0617712249622996,-0.468811987424192,0.881135424446229));
#62447=DIRECTION('ref_axis',(0.998052578482889,0.0213346303712044,-0.0586164151972949));
#62448=DIRECTION('',(0.137998583506848,0.878353971058417,0.457657833403968));
#62449=DIRECTION('center_axis',(0.99026806874157,-0.130779935984066,-0.0476000039374393));
#62450=DIRECTION('ref_axis',(0.,0.342020143325669,-0.939692620785908));
#62451=DIRECTION('',(0.137844537491629,0.874518866989312,0.464989929744127));
#62452=DIRECTION('center_axis',(0.,-0.469471562785891,0.882947592858927));
#62453=DIRECTION('ref_axis',(1.,0.,0.));
#62454=DIRECTION('',(-0.0519254248777279,0.881756465810299,0.468838229299828));
#62455=DIRECTION('center_axis',(-0.64930555798837,-0.386503331141725,0.654994249884502));
#62456=DIRECTION('ref_axis',(0.755033118392644,-0.224258043872452,0.616143911670627));
#62457=DIRECTION('center_axis',(0.,0.207911690817759,-0.978147600733806));
#62458=DIRECTION('ref_axis',(-1.,0.,0.));
#62459=DIRECTION('',(-1.,0.,0.));
#62460=DIRECTION('',(0.137844537491629,0.968810083928407,0.205926940351068));
#62461=DIRECTION('center_axis',(0.99026806874157,-0.130779935984066,-0.0476000039374393));
#62462=DIRECTION('ref_axis',(0.,0.342020143325669,-0.939692620785908));
#62463=DIRECTION('center_axis',(-0.99026806874157,0.130779935984066,0.0476000039374393));
#62464=DIRECTION('ref_axis',(0.139173100960065,0.930547596796367,0.338691626801824));
#62465=DIRECTION('',(0.137998583506848,0.967034963408845,0.214008809386339));
#62466=DIRECTION('center_axis',(0.0617712249622996,0.20725211545606,-0.976335432321108));
#62467=DIRECTION('ref_axis',(-0.998052578482889,0.0213346303712044,-0.0586164151972949));
#62468=DIRECTION('center_axis',(-0.0617712249622996,-0.20725211545606,0.976335432321108));
#62469=DIRECTION('ref_axis',(-0.998090334472114,0.0128267117770656,-0.0604248268374111));
#62470=DIRECTION('',(-0.0161503784824054,0.978282954629779,0.206643717435842));
#62471=DIRECTION('center_axis',(-0.284551435696759,0.193627806751035,-0.938902951798373));
#62472=DIRECTION('ref_axis',(-0.957826285221151,-0.0982787650057295,0.270018687665129));
#62473=DIRECTION('center_axis',(0.284551435696759,-0.193627806751035,0.938902951798373));
#62474=DIRECTION('ref_axis',(0.958660774436356,0.0574729579753755,-0.278686882824878));
#62475=DIRECTION('',(-0.0552259184163638,0.974452861356161,0.21769639163261));
#62476=DIRECTION('center_axis',(-0.491310548314114,0.163286746281596,-0.855541573276281));
#62477=DIRECTION('ref_axis',(-0.868243142124459,-0.169689510806249,0.466218099258471));
#62478=DIRECTION('center_axis',(0.491310548314114,-0.163286746281596,0.855541573276281));
#62479=DIRECTION('ref_axis',(0.870984468928858,0.0921078431475352,-0.482599419928604));
#62480=DIRECTION('',(-0.0570786439550532,0.974121945658943,0.218697195660774));
#62481=DIRECTION('center_axis',(-0.313150259135956,0.190531153552383,-0.930394967059196));
#62482=DIRECTION('ref_axis',(-0.948683298050514,-0.108156265856635,0.297156898213636));
#62483=DIRECTION('center_axis',(0.313150259135956,-0.190531153552383,0.930394967059196));
#62484=DIRECTION('ref_axis',(0.949703593340092,0.0628247387151196,-0.306783534438035));
#62485=DIRECTION('',(-0.0225789275220273,0.977898235227234,0.207858686543083));
#62486=DIRECTION('center_axis',(0.,0.207911690817759,-0.978147600733806));
#62487=DIRECTION('ref_axis',(-1.,0.,0.));
#62488=DIRECTION('',(-1.,0.,0.));
#62489=DIRECTION('',(0.0225789275220281,0.977898235227234,0.207858686543083));
#62490=DIRECTION('center_axis',(0.313150259135957,0.190531153552383,-0.930394967059195));
#62491=DIRECTION('ref_axis',(-0.948683298050513,0.108156265856636,-0.297156898213637));
#62492=DIRECTION('center_axis',(-0.313150259135957,-0.190531153552383,0.930394967059195));
#62493=DIRECTION('ref_axis',(-0.949703593340092,0.0628247387151197,-0.306783534438037));
#62494=DIRECTION('',(0.0570786439550534,0.974121945658943,0.218697195660774));
#62495=DIRECTION('center_axis',(0.491310548314113,0.163286746281596,-0.855541573276282));
#62496=DIRECTION('ref_axis',(-0.86824314212446,0.169689510806249,-0.46621809925847));
#62497=DIRECTION('center_axis',(-0.491310548314113,-0.163286746281596,0.855541573276282));
#62498=DIRECTION('ref_axis',(-0.870984468928858,0.0921078431475348,-0.482599419928602));
#62499=DIRECTION('',(0.0552259184163649,0.974452861356161,0.21769639163261));
#62500=DIRECTION('center_axis',(0.284551435696759,0.193627806751035,-0.938902951798373));
#62501=DIRECTION('ref_axis',(-0.957826285221151,0.0982787650057293,-0.270018687665128));
#62502=DIRECTION('center_axis',(-0.284551435696759,-0.193627806751035,0.938902951798373));
#62503=DIRECTION('ref_axis',(-0.958660774436356,0.0574729579753754,-0.278686882824878));
#62504=DIRECTION('',(0.0161503784824051,0.978282954629779,0.206643717435842));
#62505=DIRECTION('center_axis',(-0.0617712249622997,0.20725211545606,-0.976335432321108));
#62506=DIRECTION('ref_axis',(-0.998052578482889,-0.0213346303712044,0.058616415197295));
#62507=DIRECTION('center_axis',(0.0617712249622997,-0.20725211545606,0.976335432321108));
#62508=DIRECTION('ref_axis',(0.998090334472114,0.0128267117770656,-0.0604248268374111));
#62509=DIRECTION('',(-0.137998583506848,0.967034963408845,0.214008809386339));
#62510=DIRECTION('center_axis',(-0.99026806874157,-0.130779935984066,-0.0476000039374394));
#62511=DIRECTION('ref_axis',(0.,-0.342020143325669,0.939692620785908));
#62512=DIRECTION('center_axis',(0.99026806874157,0.130779935984066,0.0476000039374394));
#62513=DIRECTION('ref_axis',(-0.139173100960066,0.930547596796366,0.338691626801825));
#62514=DIRECTION('',(-0.137844537491629,0.968810083928407,0.205926940351068));
#62515=DIRECTION('center_axis',(0.,0.207911690817759,-0.978147600733806));
#62516=DIRECTION('ref_axis',(-1.,0.,0.));
#62517=DIRECTION('',(-1.,0.,0.));
#62518=DIRECTION('center_axis',(0.,0.939692620785908,0.342020143325669));
#62519=DIRECTION('ref_axis',(1.,0.,0.));
#62520=DIRECTION('center_axis',(1.,0.,0.));
#62521=DIRECTION('ref_axis',(0.,1.,0.));
#62522=DIRECTION('center_axis',(1.,0.,0.));
#62523=DIRECTION('ref_axis',(0.,0.,-1.));
#62524=DIRECTION('center_axis',(0.64930555798837,0.266892919198654,-0.712159014579631));
#62525=DIRECTION('ref_axis',(-0.760527640763576,0.227861614141253,-0.608010520003998));
#62526=DIRECTION('',(1.,0.,0.));
#62527=DIRECTION('center_axis',(-0.99026806874157,0.137058748836223,0.0241671553619711));
#62528=DIRECTION('ref_axis',(0.139173100960065,0.975223671657125,0.171958245538723));
#62529=DIRECTION('center_axis',(-0.0617712249622996,0.308682119187541,-0.949157344732972));
#62530=DIRECTION('ref_axis',(0.998090334472114,0.0191041551727457,-0.0587427909490065));
#62531=DIRECTION('center_axis',(0.284551435696759,0.301764876373726,-0.909927711321104));
#62532=DIRECTION('ref_axis',(-0.958660774436356,0.0895703997751286,-0.27008639921553));
#62533=DIRECTION('center_axis',(0.491310548314114,0.286360316256974,-0.822564109591763));
#62534=DIRECTION('ref_axis',(-0.870984468928858,0.161531977910744,-0.463997279083573));
#62535=DIRECTION('center_axis',(0.313150259135956,0.30019266434088,-0.901011253802641));
#62536=DIRECTION('ref_axis',(-0.949703593340092,0.0989839475056044,-0.297094703643677));
#62537=DIRECTION('',(1.,0.,0.));
#62538=DIRECTION('center_axis',(-0.313150259135957,0.30019266434088,-0.901011253802641));
#62539=DIRECTION('ref_axis',(0.949703593340092,0.0989839475056049,-0.297094703643678));
#62540=DIRECTION('center_axis',(-0.491310548314113,0.286360316256975,-0.822564109591764));
#62541=DIRECTION('ref_axis',(0.870984468928858,0.161531977910744,-0.463997279083571));
#62542=DIRECTION('center_axis',(-0.284551435696759,0.301764876373726,-0.909927711321105));
#62543=DIRECTION('ref_axis',(0.958660774436356,0.0895703997751284,-0.270086399215529));
#62544=DIRECTION('center_axis',(0.0617712249622997,0.308682119187541,-0.949157344732972));
#62545=DIRECTION('ref_axis',(-0.998090334472114,0.0191041551727457,-0.0587427909490066));
#62546=DIRECTION('center_axis',(0.99026806874157,0.137058748836224,0.0241671553619711));
#62547=DIRECTION('ref_axis',(-0.139173100960066,0.975223671657125,0.171958245538724));
#62548=DIRECTION('',(1.,0.,0.));
#62549=DIRECTION('center_axis',(0.,-0.309016994374948,0.951056516295154));
#62550=DIRECTION('ref_axis',(1.,0.,0.));
#62551=DIRECTION('',(-0.137844537491629,0.941977614300068,0.306067080296576));
#62552=DIRECTION('center_axis',(-0.99026806874157,-0.137058748836224,-0.0241671553619711));
#62553=DIRECTION('ref_axis',(0.,-0.17364817766693,0.984807753012208));
#62554=DIRECTION('',(-0.137998583506848,0.944481249352984,0.298180416142191));
#62555=DIRECTION('center_axis',(-0.0617712249622997,-0.308682119187541,
0.949157344732972));
#62556=DIRECTION('ref_axis',(0.998052578482889,-0.0108318757168334,0.0614306198252359));
#62557=DIRECTION('',(0.0161503784824051,0.950539749516609,0.310182768482997));
#62558=DIRECTION('center_axis',(0.284551435696759,-0.301764876373726,0.909927711321105));
#62559=DIRECTION('ref_axis',(0.957826285221151,0.0498974366850415,-0.282982425517402));
#62560=DIRECTION('',(0.0552259184163645,0.952749128541176,0.298695825212034));
#62561=DIRECTION('center_axis',(0.491310548314113,-0.286360316256975,0.822564109591764));
#62562=DIRECTION('ref_axis',(0.86824314212446,0.0861536225152694,-0.488601473065054));
#62563=DIRECTION('',(0.057078643955053,0.952962949154956,0.297663645650825));
#62564=DIRECTION('center_axis',(0.313150259135957,-0.30019266434088,0.901011253802641));
#62565=DIRECTION('ref_axis',(0.948683298050513,0.0549123752965087,-0.311423555691114));
#62566=DIRECTION('',(0.0225789275220278,0.950814057294297,0.30893821467004));
#62567=DIRECTION('center_axis',(0.,-0.309016994374947,0.951056516295154));
#62568=DIRECTION('ref_axis',(1.,0.,0.));
#62569=DIRECTION('',(-0.0225789275220274,0.950814057294297,0.30893821467004));
#62570=DIRECTION('center_axis',(-0.313150259135956,-0.30019266434088,0.901011253802641));
#62571=DIRECTION('ref_axis',(0.948683298050514,-0.0549123752965085,0.311423555691113));
#62572=DIRECTION('',(-0.0570786439550527,0.952962949154956,0.297663645650826));
#62573=DIRECTION('center_axis',(-0.491310548314114,-0.286360316256974,0.822564109591763));
#62574=DIRECTION('ref_axis',(0.868243142124459,-0.0861536225152696,0.488601473065055));
#62575=DIRECTION('',(-0.0552259184163635,0.952749128541176,0.298695825212034));
#62576=DIRECTION('center_axis',(-0.284551435696759,-0.301764876373726,0.909927711321104));
#62577=DIRECTION('ref_axis',(0.957826285221151,-0.0498974366850416,0.282982425517402));
#62578=DIRECTION('',(-0.0161503784824052,0.950539749516609,0.310182768482997));
#62579=DIRECTION('center_axis',(0.0617712249622996,-0.308682119187541,0.949157344732972));
#62580=DIRECTION('ref_axis',(0.998052578482889,0.0108318757168334,-0.0614306198252359));
#62581=DIRECTION('',(0.137998583506848,0.944481249352984,0.298180416142191));
#62582=DIRECTION('center_axis',(0.99026806874157,-0.137058748836223,-0.0241671553619711));
#62583=DIRECTION('ref_axis',(0.,0.17364817766693,-0.984807753012208));
#62584=DIRECTION('',(0.137844537491629,0.941977614300068,0.306067080296576));
#62585=DIRECTION('center_axis',(0.,-0.309016994374948,0.951056516295154));
#62586=DIRECTION('ref_axis',(1.,0.,0.));
#62587=DIRECTION('',(-0.0519254248777279,0.949773507937132,0.308600119688995));
#62588=DIRECTION('center_axis',(-0.64930555798837,-0.266892919198654,0.712159014579631));
#62589=DIRECTION('ref_axis',(0.755033118392644,-0.113858792838765,0.645725301830105));
#62590=DIRECTION('center_axis',(0.,0.034899496702501,-0.999390827019096));
#62591=DIRECTION('ref_axis',(-1.,0.,0.));
#62592=DIRECTION('',(-1.,0.,0.));
#62593=DIRECTION('',(0.137844537491629,0.989850519773593,0.0345663418323004));
#62594=DIRECTION('center_axis',(0.99026806874157,-0.137058748836223,-0.0241671553619711));
#62595=DIRECTION('ref_axis',(0.,0.17364817766693,-0.984807753012208));
#62596=DIRECTION('center_axis',(-0.99026806874157,0.137058748836223,0.0241671553619711));
#62597=DIRECTION('ref_axis',(0.139173100960065,0.975223671657125,0.171958245538723));
#62598=DIRECTION('',(0.137998583506848,0.989505769153514,0.0428336755604258));
#62599=DIRECTION('center_axis',(0.0617712249622996,0.0345646215150941,-0.997491655456914));
#62600=DIRECTION('ref_axis',(-0.998052578482889,0.0108318757168334,-0.0614306198252359));
#62601=DIRECTION('center_axis',(-0.0617712249622996,-0.0345646215150941,
0.997491655456914));
#62602=DIRECTION('ref_axis',(-0.998090334472114,0.0021391841375509,-0.061734173069449));
#62603=DIRECTION('',(-0.0161503784824054,0.999303943318151,0.0336272827279996));
#62604=DIRECTION('center_axis',(-0.284551435696759,0.0276473787012795,-0.958262022045047));
#62605=DIRECTION('ref_axis',(-0.957826285221151,-0.0498974366850416,0.282982425517402));
#62606=DIRECTION('center_axis',(0.284551435696759,-0.0276473787012795,0.958262022045047));
#62607=DIRECTION('ref_axis',(0.958660774436356,0.00820634526047709,-0.284433077286297));
#62608=DIRECTION('',(-0.0552259184163638,0.997451314500147,0.045177130685753));
#62609=DIRECTION('center_axis',(-0.491310548314114,0.0122428185845279,-0.870898420315705));
#62610=DIRECTION('ref_axis',(-0.868243142124459,-0.0861536225152696,0.488601473065055));
#62611=DIRECTION('center_axis',(0.491310548314114,-0.0122428185845279,0.870898420315705));
#62612=DIRECTION('ref_axis',(0.870984468928858,0.00690600823120529,-0.491262009456284));
#62613=DIRECTION('',(-0.0570786439550532,0.997299213951626,0.0462201931597183));
#62614=DIRECTION('center_axis',(-0.313150259135956,0.0260751666684337,-0.949345564526583));
#62615=DIRECTION('ref_axis',(-0.948683298050514,-0.0549123752965085,0.311423555691113));
#62616=DIRECTION('center_axis',(0.313150259135956,-0.0260751666684337,0.949345564526583));
#62617=DIRECTION('ref_axis',(0.949703593340092,0.00859788807423116,-0.313032204601347));
#62618=DIRECTION('',(-0.0225789275220273,0.999136045839184,0.0348905995476465));
#62619=DIRECTION('center_axis',(0.,0.034899496702501,-0.999390827019096));
#62620=DIRECTION('ref_axis',(-1.,0.,0.));
#62621=DIRECTION('',(-1.,0.,0.));
#62622=DIRECTION('',(0.0225789275220281,0.999136045839184,0.0348905995476465));
#62623=DIRECTION('center_axis',(0.313150259135957,0.0260751666684335,-0.949345564526583));
#62624=DIRECTION('ref_axis',(-0.948683298050513,0.0549123752965087,-0.311423555691114));
#62625=DIRECTION('center_axis',(-0.313150259135957,-0.0260751666684335,
0.949345564526583));
#62626=DIRECTION('ref_axis',(-0.949703593340092,0.00859788807423112,-0.313032204601348));
#62627=DIRECTION('',(0.0570786439550533,0.997299213951626,0.0462201931597181));
#62628=DIRECTION('center_axis',(0.491310548314113,0.0122428185845279,-0.870898420315706));
#62629=DIRECTION('ref_axis',(-0.86824314212446,0.0861536225152694,-0.488601473065054));
#62630=DIRECTION('center_axis',(-0.491310548314113,-0.0122428185845279,
0.870898420315706));
#62631=DIRECTION('ref_axis',(-0.870984468928858,0.00690600823120516,-0.491262009456283));
#62632=DIRECTION('',(0.0552259184163649,0.997451314500147,0.0451771306857534));
#62633=DIRECTION('center_axis',(0.284551435696759,0.0276473787012796,-0.958262022045047));
#62634=DIRECTION('ref_axis',(-0.957826285221151,0.0498974366850415,-0.282982425517402));
#62635=DIRECTION('center_axis',(-0.284551435696759,-0.0276473787012796,
0.958262022045047));
#62636=DIRECTION('ref_axis',(-0.958660774436356,0.00820634526047708,-0.284433077286297));
#62637=DIRECTION('',(0.016150378482405,0.999303943318151,0.0336272827279996));
#62638=DIRECTION('center_axis',(-0.0617712249622997,0.0345646215150941,
-0.997491655456914));
#62639=DIRECTION('ref_axis',(-0.998052578482889,-0.0108318757168334,0.0614306198252359));
#62640=DIRECTION('center_axis',(0.0617712249622997,-0.0345646215150941,
0.997491655456914));
#62641=DIRECTION('ref_axis',(0.998090334472114,0.0021391841375509,-0.061734173069449));
#62642=DIRECTION('',(-0.137998583506848,0.989505769153514,0.0428336755604258));
#62643=DIRECTION('center_axis',(-0.99026806874157,-0.137058748836224,-0.0241671553619711));
#62644=DIRECTION('ref_axis',(0.,-0.17364817766693,0.984807753012208));
#62645=DIRECTION('center_axis',(0.99026806874157,0.137058748836224,0.0241671553619711));
#62646=DIRECTION('ref_axis',(-0.139173100960066,0.975223671657125,0.171958245538724));
#62647=DIRECTION('',(-0.137844537491629,0.989850519773593,0.0345663418323003));
#62648=DIRECTION('center_axis',(0.,0.0348994967025009,-0.999390827019096));
#62649=DIRECTION('ref_axis',(-1.,0.,0.));
#62650=DIRECTION('',(-1.,0.,0.));
#62651=DIRECTION('center_axis',(0.,0.984807753012208,0.17364817766693));
#62652=DIRECTION('ref_axis',(1.,0.,0.));
#62653=DIRECTION('center_axis',(1.,0.,0.));
#62654=DIRECTION('ref_axis',(0.,1.,0.));
#62655=DIRECTION('center_axis',(1.,0.,0.));
#62656=DIRECTION('ref_axis',(0.,0.,-1.));
#62657=DIRECTION('center_axis',(0.649305557988371,0.139173100960065,-0.747685187986609));
#62658=DIRECTION('ref_axis',(-0.760527640763576,0.118819965419165,-0.638341228068795));
#62659=DIRECTION('',(1.,0.,0.));
#62660=DIRECTION('center_axis',(-0.99026806874157,0.139173100960065,0.));
#62661=DIRECTION('ref_axis',(0.139173100960065,0.99026806874157,0.));
#62662=DIRECTION('center_axis',(-0.0617712249622996,0.139173100960065,-0.988339599396795));
#62663=DIRECTION('ref_axis',(0.998090334472114,0.00861334152950385,-0.0611677576917705));
#62664=DIRECTION('center_axis',(0.284551435696759,0.139173100960065,-0.948504785655862));
#62665=DIRECTION('ref_axis',(-0.958660774436356,0.0413096131025498,-0.281536916624453));
#62666=DIRECTION('center_axis',(0.491310548314114,0.139173100960065,-0.859793459549701));
#62667=DIRECTION('ref_axis',(-0.870984468928858,0.0785056622506209,-0.484997851417207));
#62668=DIRECTION('center_axis',(0.313150259135956,0.139173100960065,-0.939450777407866));
#62669=DIRECTION('ref_axis',(-0.949703593340092,0.0458902050450515,-0.309769549629784));
#62670=DIRECTION('',(1.,0.,0.));
#62671=DIRECTION('center_axis',(-0.313150259135957,0.139173100960066,-0.939450777407865));
#62672=DIRECTION('ref_axis',(0.949703593340092,0.0458902050450517,-0.309769549629785));
#62673=DIRECTION('center_axis',(-0.491310548314113,0.139173100960066,-0.859793459549702));
#62674=DIRECTION('ref_axis',(0.870984468928858,0.0785056622506207,-0.484997851417206));
#62675=DIRECTION('center_axis',(-0.284551435696759,0.139173100960065,-0.948504785655862));
#62676=DIRECTION('ref_axis',(0.958660774436356,0.0413096131025497,-0.281536916624453));
#62677=DIRECTION('center_axis',(0.0617712249622997,0.139173100960065,-0.988339599396795));
#62678=DIRECTION('ref_axis',(-0.998090334472114,0.00861334152950385,-0.0611677576917706));
#62679=DIRECTION('center_axis',(0.99026806874157,0.139173100960066,0.));
#62680=DIRECTION('ref_axis',(-0.139173100960066,0.99026806874157,0.));
#62681=DIRECTION('',(1.,0.,0.));
#62682=DIRECTION('center_axis',(0.,-0.139173100960065,-0.99026806874157));
#62683=DIRECTION('ref_axis',(-1.,0.,0.));
#62684=DIRECTION('',(-1.,0.,0.));
#62685=DIRECTION('',(0.137844537491629,0.980814848463989,-0.137844537491629));
#62686=DIRECTION('center_axis',(0.99026806874157,-0.139173100960065,0.));
#62687=DIRECTION('ref_axis',(0.,0.,-1.));
#62688=DIRECTION('center_axis',(-0.99026806874157,0.139173100960065,0.));
#62689=DIRECTION('ref_axis',(0.139173100960065,0.99026806874157,0.));
#62690=DIRECTION('',(0.137998583506848,0.981910942816534,-0.129642937822505));
#62691=DIRECTION('center_axis',(0.0617712249622996,-0.139173100960065,-0.988339599396795));
#62692=DIRECTION('ref_axis',(-0.998052578482889,0.,-0.0623782861551805));
#62693=DIRECTION('center_axis',(-0.0617712249622996,0.139173100960065,0.988339599396795));
#62694=DIRECTION('ref_axis',(0.998090334472114,0.00861334152950385,0.0611677576917705));
#62695=DIRECTION('',(-0.0161503784824054,0.989961587360995,-0.140410899949307));
#62696=DIRECTION('center_axis',(-0.284551435696759,-0.139173100960066,-0.948504785655862));
#62697=DIRECTION('ref_axis',(-0.957826285221151,0.,0.287347885566346));
#62698=DIRECTION('center_axis',(0.284551435696759,0.139173100960066,0.948504785655862));
#62699=DIRECTION('ref_axis',(-0.958660774436356,0.0413096131025498,0.281536916624453));
#62700=DIRECTION('',(-0.0552259184163638,0.990142714187765,-0.128714814516259));
#62701=DIRECTION('center_axis',(-0.491310548314114,-0.139173100960065,-0.859793459549701));
#62702=DIRECTION('ref_axis',(-0.868243142124459,0.,0.496138938356833));
#62703=DIRECTION('center_axis',(0.491310548314114,0.139173100960065,0.859793459549701));
#62704=DIRECTION('ref_axis',(-0.870984468928858,0.0785056622506209,0.484997851417207));
#62705=DIRECTION('',(-0.0570786439550532,0.99017405028614,-0.12766118652195));
#62706=DIRECTION('center_axis',(-0.313150259135956,-0.139173100960065,-0.939450777407866));
#62707=DIRECTION('ref_axis',(-0.948683298050514,0.,0.316227766016839));
#62708=DIRECTION('center_axis',(0.313150259135956,0.139173100960065,0.939450777407866));
#62709=DIRECTION('ref_axis',(-0.949703593340092,0.0458902050450514,0.309769549629784));
#62710=DIRECTION('',(-0.0225789275220273,0.990015613285545,-0.13913762065955));
#62711=DIRECTION('center_axis',(0.,-0.139173100960065,-0.99026806874157));
#62712=DIRECTION('ref_axis',(-1.,0.,0.));
#62713=DIRECTION('',(-1.,0.,0.));
#62714=DIRECTION('',(0.0225789275220281,0.990015613285545,-0.13913762065955));
#62715=DIRECTION('center_axis',(0.313150259135957,-0.139173100960066,-0.939450777407865));
#62716=DIRECTION('ref_axis',(-0.948683298050513,0.,-0.31622776601684));
#62717=DIRECTION('center_axis',(-0.313150259135957,0.139173100960066,0.939450777407865));
#62718=DIRECTION('ref_axis',(0.949703593340092,0.0458902050450518,0.309769549629785));
#62719=DIRECTION('',(0.0570786439550534,0.99017405028614,-0.12766118652195));
#62720=DIRECTION('center_axis',(0.491310548314113,-0.139173100960066,-0.859793459549702));
#62721=DIRECTION('ref_axis',(-0.86824314212446,0.,-0.496138938356832));
#62722=DIRECTION('center_axis',(-0.491310548314113,0.139173100960066,0.859793459549702));
#62723=DIRECTION('ref_axis',(0.870984468928858,0.0785056622506208,0.484997851417206));
#62724=DIRECTION('',(0.0552259184163649,0.990142714187765,-0.128714814516259));
#62725=DIRECTION('center_axis',(0.284551435696759,-0.139173100960065,-0.948504785655862));
#62726=DIRECTION('ref_axis',(-0.957826285221151,0.,-0.287347885566345));
#62727=DIRECTION('center_axis',(-0.284551435696759,0.139173100960065,0.948504785655862));
#62728=DIRECTION('ref_axis',(0.958660774436356,0.0413096131025497,0.281536916624453));
#62729=DIRECTION('',(0.0161503784824051,0.989961587360995,-0.140410899949307));
#62730=DIRECTION('center_axis',(-0.0617712249622997,-0.139173100960065,
-0.988339599396795));
#62731=DIRECTION('ref_axis',(-0.998052578482889,0.,0.0623782861551806));
#62732=DIRECTION('center_axis',(0.0617712249622997,0.139173100960065,0.988339599396795));
#62733=DIRECTION('ref_axis',(-0.998090334472114,0.00861334152950385,0.0611677576917706));
#62734=DIRECTION('',(-0.137998583506848,0.981910942816533,-0.129642937822505));
#62735=DIRECTION('center_axis',(-0.99026806874157,-0.139173100960066,0.));
#62736=DIRECTION('ref_axis',(0.,0.,1.));
#62737=DIRECTION('center_axis',(0.99026806874157,0.139173100960066,0.));
#62738=DIRECTION('ref_axis',(-0.139173100960066,0.99026806874157,0.));
#62739=DIRECTION('',(-0.137844537491629,0.980814848463989,-0.137844537491629));
#62740=DIRECTION('center_axis',(0.,-0.139173100960065,-0.99026806874157));
#62741=DIRECTION('ref_axis',(-1.,0.,0.));
#62742=DIRECTION('',(-1.,0.,0.));
#62743=DIRECTION('',(0.0519254248777275,0.98893216263388,-0.138985351600607));
#62744=DIRECTION('center_axis',(0.649305557988371,-0.139173100960065,-0.747685187986609));
#62745=DIRECTION('ref_axis',(-0.755033118392643,0.,-0.655686655446243));
#62746=DIRECTION('center_axis',(-0.649305557988371,0.139173100960065,0.747685187986609));
#62747=DIRECTION('ref_axis',(0.760527640763576,0.118819965419165,0.638341228068795));
#62748=DIRECTION('center_axis',(0.,-0.139173100960066,0.99026806874157));
#62749=DIRECTION('ref_axis',(1.,0.,0.));
#62750=DIRECTION('',(-0.137844537491629,0.980814848463989,0.137844537491629));
#62751=DIRECTION('center_axis',(-0.99026806874157,-0.139173100960066,0.));
#62752=DIRECTION('ref_axis',(0.,0.,1.));
#62753=DIRECTION('',(-0.137998583506848,0.981910942816533,0.129642937822505));
#62754=DIRECTION('center_axis',(-0.0617712249622997,-0.139173100960065,
0.988339599396795));
#62755=DIRECTION('ref_axis',(0.998052578482889,0.,0.0623782861551806));
#62756=DIRECTION('',(0.0161503784824051,0.989961587360995,0.140410899949307));
#62757=DIRECTION('center_axis',(0.284551435696759,-0.139173100960065,0.948504785655862));
#62758=DIRECTION('ref_axis',(0.957826285221151,0.,-0.287347885566345));
#62759=DIRECTION('',(0.0552259184163645,0.990142714187765,0.128714814516259));
#62760=DIRECTION('center_axis',(0.491310548314113,-0.139173100960066,0.859793459549702));
#62761=DIRECTION('ref_axis',(0.86824314212446,0.,-0.496138938356832));
#62762=DIRECTION('',(0.057078643955053,0.99017405028614,0.12766118652195));
#62763=DIRECTION('center_axis',(0.313150259135957,-0.139173100960066,0.939450777407865));
#62764=DIRECTION('ref_axis',(0.948683298050513,0.,-0.31622776601684));
#62765=DIRECTION('',(0.0225789275220278,0.990015613285545,0.139137620659551));
#62766=DIRECTION('center_axis',(0.,-0.139173100960065,0.99026806874157));
#62767=DIRECTION('ref_axis',(1.,0.,0.));
#62768=DIRECTION('',(-0.0225789275220274,0.990015613285545,0.139137620659551));
#62769=DIRECTION('center_axis',(-0.313150259135956,-0.139173100960065,0.939450777407866));
#62770=DIRECTION('ref_axis',(0.948683298050514,0.,0.316227766016839));
#62771=DIRECTION('',(-0.0570786439550527,0.99017405028614,0.12766118652195));
#62772=DIRECTION('center_axis',(-0.491310548314114,-0.139173100960065,0.859793459549701));
#62773=DIRECTION('ref_axis',(0.868243142124459,0.,0.496138938356833));
#62774=DIRECTION('',(-0.0552259184163635,0.990142714187765,0.12871481451626));
#62775=DIRECTION('center_axis',(-0.284551435696759,-0.139173100960065,0.948504785655862));
#62776=DIRECTION('ref_axis',(0.957826285221151,0.,0.287347885566346));
#62777=DIRECTION('',(-0.0161503784824052,0.989961587360995,0.140410899949307));
#62778=DIRECTION('center_axis',(0.0617712249622996,-0.139173100960065,0.988339599396795));
#62779=DIRECTION('ref_axis',(0.998052578482889,0.,-0.0623782861551805));
#62780=DIRECTION('',(0.137998583506848,0.981910942816534,0.129642937822505));
#62781=DIRECTION('center_axis',(0.99026806874157,-0.139173100960065,0.));
#62782=DIRECTION('ref_axis',(0.,0.,-1.));
#62783=DIRECTION('',(0.137844537491629,0.980814848463989,0.137844537491629));
#62784=DIRECTION('center_axis',(0.,-0.139173100960065,0.99026806874157));
#62785=DIRECTION('ref_axis',(1.,0.,0.));
#62786=DIRECTION('',(-0.051925424877728,0.98893216263388,0.138985351600607));
#62787=DIRECTION('center_axis',(-0.649305557988371,-0.139173100960065,0.747685187986609));
#62788=DIRECTION('ref_axis',(0.755033118392644,0.,0.655686655446243));
#62789=DIRECTION('center_axis',(-1.,0.,0.));
#62790=DIRECTION('ref_axis',(0.,1.,0.));
#62791=DIRECTION('center_axis',(1.,0.,0.));
#62792=DIRECTION('ref_axis',(0.,0.,-1.));
#62793=DIRECTION('',(-0.707106781186545,-0.70710678118655,-8.65956056235497E-17));
#62794=DIRECTION('center_axis',(1.,0.,0.));
#62795=DIRECTION('ref_axis',(0.,0.,-1.));
#62796=DIRECTION('center_axis',(-1.,0.,-7.72527832197503E-15));
#62797=DIRECTION('ref_axis',(0.,-1.,-3.07881506165609E-17));
#62798=DIRECTION('center_axis',(-1.,0.,0.));
#62799=DIRECTION('ref_axis',(0.,-1.,0.));
#62800=DIRECTION('',(-0.57864046491405,0.815582744032788,-4.34516827576256E-15));
#62801=DIRECTION('center_axis',(1.,0.,0.));
#62802=DIRECTION('ref_axis',(0.,-1.,-6.12323399573677E-17));
#62803=DIRECTION('center_axis',(1.,0.,0.));
#62804=DIRECTION('ref_axis',(0.,-1.,-6.12323399573677E-17));
#62805=DIRECTION('center_axis',(-1.,0.,0.));
#62806=DIRECTION('ref_axis',(0.,1.,0.));
#62807=DIRECTION('',(-0.943858356366018,-0.330350424728106,-4.04562590240243E-17));
#62808=DIRECTION('center_axis',(-1.,0.,0.));
#62809=DIRECTION('ref_axis',(0.,-1.,3.06161699786838E-17));
#62810=DIRECTION('center_axis',(-1.,0.,0.));
#62811=DIRECTION('ref_axis',(0.,-1.,3.06161699786838E-17));
#62812=DIRECTION('center_axis',(1.,0.,0.));
#62813=DIRECTION('ref_axis',(0.,0.,-1.));
#62814=DIRECTION('center_axis',(1.,0.,0.));
#62815=DIRECTION('ref_axis',(0.,0.,-1.));
#62816=DIRECTION('center_axis',(0.,-1.,-1.22464679914735E-16));
#62817=DIRECTION('ref_axis',(0.,-1.22464679914735E-16,1.));
#62818=DIRECTION('center_axis',(1.,0.,0.));
#62819=DIRECTION('ref_axis',(0.,-1.,1.83697019872103E-16));
#62820=DIRECTION('center_axis',(1.,0.,0.));
#62821=DIRECTION('ref_axis',(0.,-1.,1.83697019872103E-16));
#62822=DIRECTION('center_axis',(1.,0.,0.));
#62823=DIRECTION('ref_axis',(0.,1.,0.));
#62824=DIRECTION('',(-1.,0.,0.));
#62825=DIRECTION('center_axis',(1.,0.,0.));
#62826=DIRECTION('ref_axis',(0.,0.,-1.));
#62827=DIRECTION('center_axis',(1.,0.,0.));
#62828=DIRECTION('ref_axis',(0.,0.,-1.));
#62829=DIRECTION('center_axis',(1.,0.,0.));
#62830=DIRECTION('ref_axis',(0.,-1.,1.83697019872103E-16));
#62831=DIRECTION('center_axis',(0.,-1.,-1.22464679914735E-16));
#62832=DIRECTION('ref_axis',(0.,-1.22464679914735E-16,1.));
#62833=DIRECTION('center_axis',(-1.,0.,0.));
#62834=DIRECTION('ref_axis',(0.,-1.,1.83697019872103E-16));
#62835=DIRECTION('center_axis',(1.,0.,0.));
#62836=DIRECTION('ref_axis',(0.,-1.,1.83697019872103E-16));
#62837=DIRECTION('center_axis',(1.,0.,0.));
#62838=DIRECTION('ref_axis',(0.,1.,0.));
#62839=DIRECTION('',(-1.,0.,0.));
#62840=DIRECTION('center_axis',(-1.,0.,0.));
#62841=DIRECTION('ref_axis',(0.,-1.,1.83697019872103E-16));
#62842=DIRECTION('center_axis',(-1.,0.,0.));
#62843=DIRECTION('ref_axis',(0.,-1.,1.83697019872103E-16));
#62844=DIRECTION('center_axis',(-1.,0.,0.));
#62845=DIRECTION('ref_axis',(0.,0.,1.));
#62846=DIRECTION('center_axis',(1.,0.,0.));
#62847=DIRECTION('ref_axis',(0.,0.,-1.));
#62848=DIRECTION('center_axis',(1.,0.,0.));
#62849=DIRECTION('ref_axis',(0.,0.,-1.));
#62850=DIRECTION('center_axis',(1.,0.,0.));
#62851=DIRECTION('ref_axis',(0.,-1.,1.83697019872103E-16));
#62852=DIRECTION('center_axis',(0.,-1.,-1.22464679914735E-16));
#62853=DIRECTION('ref_axis',(0.,-1.22464679914735E-16,1.));
#62854=DIRECTION('center_axis',(1.,0.,0.));
#62855=DIRECTION('ref_axis',(0.,0.,-1.));
#62856=DIRECTION('center_axis',(1.,0.,0.));
#62857=DIRECTION('ref_axis',(0.,0.,-1.));
#62858=DIRECTION('center_axis',(1.,0.,0.));
#62859=DIRECTION('ref_axis',(0.,1.,0.));
#62860=DIRECTION('center_axis',(-1.,0.,0.));
#62861=DIRECTION('ref_axis',(0.,0.,1.));
#62862=DIRECTION('center_axis',(1.,0.,0.));
#62863=DIRECTION('ref_axis',(0.,0.,-1.));
#62864=DIRECTION('center_axis',(1.,0.,0.));
#62865=DIRECTION('ref_axis',(0.,1.,0.));
#62866=DIRECTION('center_axis',(1.,0.,0.));
#62867=DIRECTION('ref_axis',(0.,0.,-1.));
#62868=DIRECTION('',(-0.707106781186551,0.707106781186544,8.65956056235489E-17));
#62869=DIRECTION('center_axis',(1.,0.,0.));
#62870=DIRECTION('ref_axis',(0.,1.,0.));
#62871=DIRECTION('center_axis',(1.,0.,0.));
#62872=DIRECTION('ref_axis',(0.,0.,-1.));
#62873=DIRECTION('',(-1.,0.,0.));
#62874=DIRECTION('center_axis',(-1.,0.,0.));
#62875=DIRECTION('ref_axis',(0.,1.,0.));
#62876=DIRECTION('',(-0.707106781186549,-0.707106781186546,-8.65956056235492E-17));
#62877=DIRECTION('center_axis',(1.,0.,0.));
#62878=DIRECTION('ref_axis',(0.,1.,0.));
#62879=DIRECTION('center_axis',(1.,0.,0.));
#62880=DIRECTION('ref_axis',(0.,0.,-1.));
#62881=DIRECTION('',(-1.,0.,0.));
#62882=DIRECTION('center_axis',(1.,0.,0.));
#62883=DIRECTION('ref_axis',(0.,1.,0.));
#62884=DIRECTION('',(-0.447213595499961,0.894427190999915,1.0953573965284E-16));
#62885=DIRECTION('axis',(0.,0.,1.));
#62886=DIRECTION('refdir',(1.,0.,0.));
#62887=DIRECTION('center_axis',(0.,0.90630778703665,-0.4226182617407));
#62888=DIRECTION('ref_axis',(0.,0.4226182617407,0.90630778703665));
#62889=DIRECTION('',(0.,-0.4226182617407,-0.90630778703665));
#62890=DIRECTION('',(1.,0.,0.));
#62891=DIRECTION('',(0.,0.4226182617407,0.90630778703665));
#62892=DIRECTION('',(-1.,0.,0.));
#62893=DIRECTION('center_axis',(0.,-0.90630778703665,0.4226182617407));
#62894=DIRECTION('ref_axis',(0.,-0.4226182617407,-0.90630778703665));
#62895=DIRECTION('',(1.,0.,0.));
#62896=DIRECTION('',(0.,-0.4226182617407,-0.90630778703665));
#62897=DIRECTION('',(1.,0.,0.));
#62898=DIRECTION('',(0.,0.4226182617407,0.90630778703665));
#62899=DIRECTION('center_axis',(0.,0.4226182617407,0.90630778703665));
#62900=DIRECTION('ref_axis',(0.,-0.906307787036649,0.4226182617407));
#62901=DIRECTION('',(0.,-0.906307787036649,0.4226182617407));
#62902=DIRECTION('',(0.,0.906307787036649,-0.4226182617407));
#62903=DIRECTION('center_axis',(1.,0.,0.));
#62904=DIRECTION('ref_axis',(0.,1.,0.));
#62905=DIRECTION('center_axis',(1.,0.,0.));
#62906=DIRECTION('ref_axis',(0.,0.,-1.));
#62907=DIRECTION('',(1.,0.,0.));
#62908=DIRECTION('center_axis',(1.,0.,0.));
#62909=DIRECTION('ref_axis',(0.,0.,-1.));
#62910=DIRECTION('center_axis',(-1.,0.,0.));
#62911=DIRECTION('ref_axis',(0.,-0.996194698091746,-0.0871557427476573));
#62912=DIRECTION('center_axis',(1.,0.,0.));
#62913=DIRECTION('ref_axis',(0.,0.,-1.));
#62914=DIRECTION('center_axis',(1.,0.,0.));
#62915=DIRECTION('ref_axis',(0.,0.,-1.));
#62916=DIRECTION('center_axis',(1.,0.,0.));
#62917=DIRECTION('ref_axis',(0.,0.,-1.));
#62918=DIRECTION('center_axis',(1.,0.,0.));
#62919=DIRECTION('ref_axis',(0.,0.,-1.));
#62920=DIRECTION('center_axis',(1.,0.,0.));
#62921=DIRECTION('ref_axis',(0.,0.,-1.));
#62922=DIRECTION('center_axis',(1.,0.,0.));
#62923=DIRECTION('ref_axis',(0.,0.,-1.));
#62924=DIRECTION('center_axis',(1.,0.,0.));
#62925=DIRECTION('ref_axis',(0.,0.,-1.));
#62926=DIRECTION('center_axis',(1.,0.,0.));
#62927=DIRECTION('ref_axis',(0.,0.,-1.));
#62928=DIRECTION('center_axis',(1.,0.,0.));
#62929=DIRECTION('ref_axis',(0.,0.,-1.));
#62930=DIRECTION('center_axis',(1.,0.,0.));
#62931=DIRECTION('ref_axis',(0.,0.,-1.));
#62932=DIRECTION('center_axis',(1.,0.,0.));
#62933=DIRECTION('ref_axis',(0.,0.,-1.));
#62934=DIRECTION('center_axis',(1.,0.,0.));
#62935=DIRECTION('ref_axis',(0.,0.,-1.));
#62936=DIRECTION('center_axis',(1.,0.,0.));
#62937=DIRECTION('ref_axis',(0.,0.,-1.));
#62938=DIRECTION('center_axis',(-1.,0.,0.));
#62939=DIRECTION('ref_axis',(0.,0.,1.));
#62940=DIRECTION('center_axis',(1.,0.,0.));
#62941=DIRECTION('ref_axis',(0.,0.,-1.));
#62942=DIRECTION('',(0.,0.573576436351046,-0.819152044288992));
#62943=DIRECTION('',(0.,0.819152044288992,0.573576436351046));
#62944=DIRECTION('',(0.,-0.573576436351046,0.819152044288992));
#62945=DIRECTION('center_axis',(1.,0.,0.));
#62946=DIRECTION('ref_axis',(0.,0.,-1.));
#62947=DIRECTION('',(0.,-0.996194698091746,-0.0871557427476583));
#62948=DIRECTION('',(0.,0.0871557427476578,-0.996194698091746));
#62949=DIRECTION('',(0.,0.996194698091746,0.0871557427476582));
#62950=DIRECTION('center_axis',(1.,0.,0.));
#62951=DIRECTION('ref_axis',(0.,0.,-1.));
#62952=DIRECTION('center_axis',(1.,0.,0.));
#62953=DIRECTION('ref_axis',(0.,0.,-1.));
#62954=DIRECTION('center_axis',(1.,0.,0.));
#62955=DIRECTION('ref_axis',(0.,-0.996194698091746,-0.0871557427476573));
#62956=DIRECTION('center_axis',(1.,0.,0.));
#62957=DIRECTION('ref_axis',(0.,0.,-1.));
#62958=DIRECTION('center_axis',(1.,0.,0.));
#62959=DIRECTION('ref_axis',(0.,0.,-1.));
#62960=DIRECTION('center_axis',(1.,0.,0.));
#62961=DIRECTION('ref_axis',(0.,0.,-1.));
#62962=DIRECTION('center_axis',(1.,0.,0.));
#62963=DIRECTION('ref_axis',(0.,0.,-1.));
#62964=DIRECTION('center_axis',(1.,0.,0.));
#62965=DIRECTION('ref_axis',(0.,0.,-1.));
#62966=DIRECTION('center_axis',(1.,0.,0.));
#62967=DIRECTION('ref_axis',(0.,0.,-1.));
#62968=DIRECTION('center_axis',(1.,0.,0.));
#62969=DIRECTION('ref_axis',(0.,0.,-1.));
#62970=DIRECTION('center_axis',(1.,0.,0.));
#62971=DIRECTION('ref_axis',(0.,0.,-1.));
#62972=DIRECTION('center_axis',(1.,0.,0.));
#62973=DIRECTION('ref_axis',(0.,0.,-1.));
#62974=DIRECTION('center_axis',(1.,0.,0.));
#62975=DIRECTION('ref_axis',(0.,0.,-1.));
#62976=DIRECTION('center_axis',(1.,0.,0.));
#62977=DIRECTION('ref_axis',(0.,0.,-1.));
#62978=DIRECTION('center_axis',(1.,0.,0.));
#62979=DIRECTION('ref_axis',(0.,0.,-1.));
#62980=DIRECTION('center_axis',(1.,0.,0.));
#62981=DIRECTION('ref_axis',(0.,1.,0.));
#62982=DIRECTION('center_axis',(1.,0.,0.));
#62983=DIRECTION('ref_axis',(0.,0.,-1.));
#62984=DIRECTION('center_axis',(1.,0.,0.));
#62985=DIRECTION('ref_axis',(0.,0.,-1.));
#62986=DIRECTION('center_axis',(1.,0.,0.));
#62987=DIRECTION('ref_axis',(0.,0.,-1.));
#62988=DIRECTION('center_axis',(1.,0.,0.));
#62989=DIRECTION('ref_axis',(0.,0.,-1.));
#62990=DIRECTION('center_axis',(1.,0.,0.));
#62991=DIRECTION('ref_axis',(0.,0.,-1.));
#62992=DIRECTION('center_axis',(1.,0.,0.));
#62993=DIRECTION('ref_axis',(0.,0.,-1.));
#62994=DIRECTION('center_axis',(1.,0.,0.));
#62995=DIRECTION('ref_axis',(0.,0.,-1.));
#62996=DIRECTION('center_axis',(1.,0.,0.));
#62997=DIRECTION('ref_axis',(0.,0.,-1.));
#62998=DIRECTION('center_axis',(1.,0.,0.));
#62999=DIRECTION('ref_axis',(0.,0.,-1.));
#63000=DIRECTION('center_axis',(1.,0.,0.));
#63001=DIRECTION('ref_axis',(0.,0.,-1.));
#63002=DIRECTION('center_axis',(1.,0.,0.));
#63003=DIRECTION('ref_axis',(0.,0.,-1.));
#63004=DIRECTION('center_axis',(0.,-0.819152044288992,-0.573576436351046));
#63005=DIRECTION('ref_axis',(0.,0.573576436351046,-0.819152044288992));
#63006=DIRECTION('',(0.,-0.573576436351046,0.819152044288992));
#63007=DIRECTION('',(1.,0.,0.));
#63008=DIRECTION('',(-1.,0.,0.));
#63009=DIRECTION('center_axis',(0.,0.819152044288992,0.573576436351046));
#63010=DIRECTION('ref_axis',(0.,-0.573576436351046,0.819152044288992));
#63011=DIRECTION('',(1.,0.,0.));
#63012=DIRECTION('',(1.,0.,0.));
#63013=DIRECTION('',(0.,0.573576436351046,-0.819152044288992));
#63014=DIRECTION('center_axis',(0.,0.573576436351046,-0.819152044288992));
#63015=DIRECTION('ref_axis',(0.,0.819152044288992,0.573576436351045));
#63016=DIRECTION('',(0.,-0.819152044288992,-0.573576436351046));
#63017=DIRECTION('center_axis',(-1.,0.,0.));
#63018=DIRECTION('ref_axis',(0.,1.,0.));
#63019=DIRECTION('center_axis',(1.,0.,0.));
#63020=DIRECTION('ref_axis',(0.,0.,-1.));
#63021=DIRECTION('center_axis',(1.,0.,0.));
#63022=DIRECTION('ref_axis',(0.,0.,-1.));
#63023=DIRECTION('center_axis',(1.,0.,0.));
#63024=DIRECTION('ref_axis',(0.,0.,-1.));
#63025=DIRECTION('center_axis',(1.,0.,0.));
#63026=DIRECTION('ref_axis',(0.,0.,-1.));
#63027=DIRECTION('center_axis',(1.,0.,0.));
#63028=DIRECTION('ref_axis',(0.,0.,-1.));
#63029=DIRECTION('center_axis',(1.,0.,0.));
#63030=DIRECTION('ref_axis',(0.,0.,-1.));
#63031=DIRECTION('center_axis',(1.,0.,0.));
#63032=DIRECTION('ref_axis',(0.,0.,-1.));
#63033=DIRECTION('center_axis',(1.,0.,0.));
#63034=DIRECTION('ref_axis',(0.,0.,-1.));
#63035=DIRECTION('center_axis',(1.,0.,0.));
#63036=DIRECTION('ref_axis',(0.,0.,-1.));
#63037=DIRECTION('center_axis',(1.,0.,0.));
#63038=DIRECTION('ref_axis',(0.,0.,-1.));
#63039=DIRECTION('center_axis',(1.,0.,0.));
#63040=DIRECTION('ref_axis',(0.,0.,-1.));
#63041=DIRECTION('center_axis',(1.,0.,0.));
#63042=DIRECTION('ref_axis',(0.,0.,-1.));
#63043=DIRECTION('center_axis',(1.,0.,0.));
#63044=DIRECTION('ref_axis',(0.,0.,-1.));
#63045=DIRECTION('center_axis',(-1.,0.,0.));
#63046=DIRECTION('ref_axis',(0.,1.,0.));
#63047=DIRECTION('center_axis',(1.,0.,0.));
#63048=DIRECTION('ref_axis',(0.,0.,-1.));
#63049=DIRECTION('center_axis',(1.,0.,0.));
#63050=DIRECTION('ref_axis',(0.,0.,-1.));
#63051=DIRECTION('center_axis',(1.,0.,0.));
#63052=DIRECTION('ref_axis',(0.,0.,-1.));
#63053=DIRECTION('center_axis',(1.,0.,0.));
#63054=DIRECTION('ref_axis',(0.,0.,-1.));
#63055=DIRECTION('center_axis',(1.,0.,0.));
#63056=DIRECTION('ref_axis',(0.,0.,-1.));
#63057=DIRECTION('center_axis',(1.,0.,0.));
#63058=DIRECTION('ref_axis',(0.,0.,-1.));
#63059=DIRECTION('center_axis',(1.,0.,0.));
#63060=DIRECTION('ref_axis',(0.,0.,-1.));
#63061=DIRECTION('center_axis',(1.,0.,0.));
#63062=DIRECTION('ref_axis',(0.,0.,-1.));
#63063=DIRECTION('center_axis',(1.,0.,0.));
#63064=DIRECTION('ref_axis',(0.,0.,-1.));
#63065=DIRECTION('center_axis',(1.,0.,0.));
#63066=DIRECTION('ref_axis',(0.,0.,-1.));
#63067=DIRECTION('center_axis',(1.,0.,0.));
#63068=DIRECTION('ref_axis',(0.,0.,-1.));
#63069=DIRECTION('center_axis',(1.,0.,0.));
#63070=DIRECTION('ref_axis',(0.,0.,-1.));
#63071=DIRECTION('center_axis',(1.,0.,0.));
#63072=DIRECTION('ref_axis',(0.,1.,0.));
#63073=DIRECTION('',(1.,0.,0.));
#63074=DIRECTION('center_axis',(1.,0.,0.));
#63075=DIRECTION('ref_axis',(0.,1.,0.));
#63076=DIRECTION('center_axis',(1.,0.,0.));
#63077=DIRECTION('ref_axis',(0.,0.,-1.));
#63078=DIRECTION('center_axis',(1.,0.,0.));
#63079=DIRECTION('ref_axis',(0.,0.,-1.));
#63080=DIRECTION('center_axis',(1.,0.,0.));
#63081=DIRECTION('ref_axis',(0.,0.,-1.));
#63082=DIRECTION('center_axis',(1.,0.,0.));
#63083=DIRECTION('ref_axis',(0.,0.,-1.));
#63084=DIRECTION('center_axis',(1.,0.,0.));
#63085=DIRECTION('ref_axis',(0.,0.,-1.));
#63086=DIRECTION('center_axis',(1.,0.,0.));
#63087=DIRECTION('ref_axis',(0.,0.,-1.));
#63088=DIRECTION('center_axis',(1.,0.,0.));
#63089=DIRECTION('ref_axis',(0.,0.,-1.));
#63090=DIRECTION('center_axis',(1.,0.,0.));
#63091=DIRECTION('ref_axis',(0.,0.,-1.));
#63092=DIRECTION('center_axis',(1.,0.,0.));
#63093=DIRECTION('ref_axis',(0.,0.,-1.));
#63094=DIRECTION('center_axis',(1.,0.,0.));
#63095=DIRECTION('ref_axis',(0.,0.,-1.));
#63096=DIRECTION('center_axis',(1.,0.,0.));
#63097=DIRECTION('ref_axis',(0.,0.,-1.));
#63098=DIRECTION('center_axis',(1.,0.,0.));
#63099=DIRECTION('ref_axis',(0.,0.,-1.));
#63100=DIRECTION('center_axis',(0.,-0.0871557427476583,0.996194698091746));
#63101=DIRECTION('ref_axis',(0.,-0.996194698091746,-0.0871557427476583));
#63102=DIRECTION('',(0.,0.996194698091746,0.0871557427476583));
#63103=DIRECTION('',(1.,0.,0.));
#63104=DIRECTION('',(-1.,0.,0.));
#63105=DIRECTION('center_axis',(0.,0.0871557427476582,-0.996194698091746));
#63106=DIRECTION('ref_axis',(0.,0.996194698091746,0.0871557427476582));
#63107=DIRECTION('',(1.,0.,0.));
#63108=DIRECTION('',(1.,0.,0.));
#63109=DIRECTION('',(0.,-0.996194698091746,-0.0871557427476582));
#63110=DIRECTION('center_axis',(0.,-0.996194698091746,-0.0871557427476578));
#63111=DIRECTION('ref_axis',(0.,0.0871557427476578,-0.996194698091746));
#63112=DIRECTION('',(0.,-0.0871557427476578,0.996194698091746));
#63113=DIRECTION('center_axis',(1.,0.,0.));
#63114=DIRECTION('ref_axis',(0.,1.,0.));
#63115=DIRECTION('',(1.,0.,0.));
#63116=DIRECTION('center_axis',(-1.,0.,0.));
#63117=DIRECTION('ref_axis',(0.,1.,0.));
#63118=DIRECTION('center_axis',(1.,0.,0.));
#63119=DIRECTION('ref_axis',(0.,1.,0.));
#63120=DIRECTION('center_axis',(-1.,0.,0.));
#63121=DIRECTION('ref_axis',(0.,1.,0.));
#63122=DIRECTION('center_axis',(1.,0.,0.));
#63123=DIRECTION('ref_axis',(0.,1.,0.));
#63124=DIRECTION('center_axis',(-1.,0.,0.));
#63125=DIRECTION('ref_axis',(0.,1.,0.));
#63126=DIRECTION('center_axis',(1.,0.,0.));
#63127=DIRECTION('ref_axis',(0.,1.,0.));
#63128=DIRECTION('center_axis',(-1.,0.,0.));
#63129=DIRECTION('ref_axis',(0.,1.,0.));
#63130=DIRECTION('center_axis',(1.,0.,0.));
#63131=DIRECTION('ref_axis',(0.,1.,0.));
#63132=DIRECTION('center_axis',(-1.,0.,0.));
#63133=DIRECTION('ref_axis',(0.,1.,0.));
#63134=DIRECTION('center_axis',(1.,0.,0.));
#63135=DIRECTION('ref_axis',(0.,1.,0.));
#63136=DIRECTION('center_axis',(-1.,0.,0.));
#63137=DIRECTION('ref_axis',(0.,1.,0.));
#63138=DIRECTION('center_axis',(1.,0.,0.));
#63139=DIRECTION('ref_axis',(0.,1.,0.));
#63140=DIRECTION('center_axis',(-1.,0.,0.));
#63141=DIRECTION('ref_axis',(0.,1.,0.));
#63142=DIRECTION('center_axis',(1.,0.,0.));
#63143=DIRECTION('ref_axis',(0.,1.,0.));
#63144=DIRECTION('center_axis',(-1.,0.,0.));
#63145=DIRECTION('ref_axis',(0.,1.,0.));
#63146=DIRECTION('center_axis',(1.,0.,0.));
#63147=DIRECTION('ref_axis',(0.,1.,0.));
#63148=DIRECTION('center_axis',(-1.,0.,0.));
#63149=DIRECTION('ref_axis',(0.,1.,0.));
#63150=DIRECTION('center_axis',(1.,0.,0.));
#63151=DIRECTION('ref_axis',(0.,1.,0.));
#63152=DIRECTION('center_axis',(-1.,0.,0.));
#63153=DIRECTION('ref_axis',(0.,1.,0.));
#63154=DIRECTION('center_axis',(1.,0.,0.));
#63155=DIRECTION('ref_axis',(0.,1.,0.));
#63156=DIRECTION('center_axis',(-1.,0.,0.));
#63157=DIRECTION('ref_axis',(0.,1.,0.));
#63158=DIRECTION('center_axis',(1.,0.,0.));
#63159=DIRECTION('ref_axis',(0.,1.,0.));
#63160=DIRECTION('center_axis',(-1.,0.,0.));
#63161=DIRECTION('ref_axis',(0.,1.,0.));
#63162=DIRECTION('center_axis',(1.,0.,0.));
#63163=DIRECTION('ref_axis',(0.,1.,0.));
#63164=DIRECTION('center_axis',(-1.,0.,0.));
#63165=DIRECTION('ref_axis',(0.,1.,0.));
#63166=DIRECTION('center_axis',(1.,0.,0.));
#63167=DIRECTION('ref_axis',(0.,1.,0.));
#63168=DIRECTION('center_axis',(-1.,0.,0.));
#63169=DIRECTION('ref_axis',(0.,1.,0.));
#63170=DIRECTION('center_axis',(1.,0.,0.));
#63171=DIRECTION('ref_axis',(0.,1.,0.));
#63172=DIRECTION('center_axis',(-1.,0.,0.));
#63173=DIRECTION('ref_axis',(0.,1.,0.));
#63174=DIRECTION('center_axis',(1.,0.,0.));
#63175=DIRECTION('ref_axis',(0.,1.,0.));
#63176=DIRECTION('center_axis',(-1.,0.,0.));
#63177=DIRECTION('ref_axis',(0.,1.,0.));
#63178=DIRECTION('center_axis',(1.,0.,0.));
#63179=DIRECTION('ref_axis',(0.,1.,0.));
#63180=DIRECTION('center_axis',(-1.,0.,0.));
#63181=DIRECTION('ref_axis',(0.,1.,0.));
#63182=DIRECTION('center_axis',(1.,0.,0.));
#63183=DIRECTION('ref_axis',(0.,1.,0.));
#63184=DIRECTION('center_axis',(-1.,0.,0.));
#63185=DIRECTION('ref_axis',(0.,1.,0.));
#63186=DIRECTION('center_axis',(1.,0.,0.));
#63187=DIRECTION('ref_axis',(0.,1.,0.));
#63188=DIRECTION('center_axis',(-1.,0.,0.));
#63189=DIRECTION('ref_axis',(0.,1.,0.));
#63190=DIRECTION('center_axis',(1.,0.,0.));
#63191=DIRECTION('ref_axis',(0.,1.,0.));
#63192=DIRECTION('center_axis',(-1.,0.,0.));
#63193=DIRECTION('ref_axis',(0.,1.,0.));
#63194=DIRECTION('center_axis',(1.,0.,0.));
#63195=DIRECTION('ref_axis',(0.,1.,0.));
#63196=DIRECTION('center_axis',(-1.,0.,0.));
#63197=DIRECTION('ref_axis',(0.,1.,0.));
#63198=DIRECTION('center_axis',(1.,0.,0.));
#63199=DIRECTION('ref_axis',(0.,1.,0.));
#63200=DIRECTION('center_axis',(-1.,0.,0.));
#63201=DIRECTION('ref_axis',(0.,1.,0.));
#63202=DIRECTION('center_axis',(1.,0.,0.));
#63203=DIRECTION('ref_axis',(0.,1.,0.));
#63204=DIRECTION('center_axis',(-1.,0.,0.));
#63205=DIRECTION('ref_axis',(0.,1.,0.));
#63206=DIRECTION('center_axis',(1.,0.,0.));
#63207=DIRECTION('ref_axis',(0.,1.,0.));
#63208=DIRECTION('center_axis',(-1.,0.,0.));
#63209=DIRECTION('ref_axis',(0.,1.,0.));
#63210=DIRECTION('center_axis',(1.,0.,0.));
#63211=DIRECTION('ref_axis',(0.,1.,0.));
#63212=DIRECTION('center_axis',(-1.,0.,0.));
#63213=DIRECTION('ref_axis',(0.,1.,0.));
#63214=DIRECTION('center_axis',(1.,0.,0.));
#63215=DIRECTION('ref_axis',(0.,1.,0.));
#63216=DIRECTION('center_axis',(-1.,0.,0.));
#63217=DIRECTION('ref_axis',(0.,1.,0.));
#63218=DIRECTION('center_axis',(1.,0.,0.));
#63219=DIRECTION('ref_axis',(0.,1.,0.));
#63220=DIRECTION('center_axis',(-1.,0.,0.));
#63221=DIRECTION('ref_axis',(0.,1.,0.));
#63222=DIRECTION('center_axis',(1.,0.,0.));
#63223=DIRECTION('ref_axis',(0.,1.,0.));
#63224=DIRECTION('center_axis',(-1.,0.,0.));
#63225=DIRECTION('ref_axis',(0.,1.,0.));
#63226=DIRECTION('center_axis',(1.,0.,0.));
#63227=DIRECTION('ref_axis',(0.,1.,0.));
#63228=DIRECTION('center_axis',(-1.,0.,0.));
#63229=DIRECTION('ref_axis',(0.,1.,0.));
#63230=DIRECTION('center_axis',(1.,0.,0.));
#63231=DIRECTION('ref_axis',(0.,1.,0.));
#63232=DIRECTION('center_axis',(-1.,0.,0.));
#63233=DIRECTION('ref_axis',(0.,1.,0.));
#63234=DIRECTION('center_axis',(1.,0.,0.));
#63235=DIRECTION('ref_axis',(0.,1.,0.));
#63236=DIRECTION('center_axis',(-1.,0.,0.));
#63237=DIRECTION('ref_axis',(0.,1.,0.));
#63238=DIRECTION('center_axis',(1.,0.,0.));
#63239=DIRECTION('ref_axis',(0.,1.,0.));
#63240=DIRECTION('center_axis',(-1.,0.,0.));
#63241=DIRECTION('ref_axis',(0.,1.,0.));
#63242=DIRECTION('center_axis',(1.,0.,0.));
#63243=DIRECTION('ref_axis',(0.,1.,0.));
#63244=DIRECTION('center_axis',(-1.,0.,0.));
#63245=DIRECTION('ref_axis',(0.,1.,0.));
#63246=DIRECTION('center_axis',(1.,0.,0.));
#63247=DIRECTION('ref_axis',(0.,1.,0.));
#63248=DIRECTION('center_axis',(0.,0.139173100960065,0.99026806874157));
#63249=DIRECTION('ref_axis',(0.,-0.99026806874157,0.139173100960065));
#63250=DIRECTION('',(1.,0.,0.));
#63251=DIRECTION('',(0.,-0.99026806874157,0.139173100960065));
#63252=DIRECTION('',(1.,0.,0.));
#63253=DIRECTION('',(-1.,0.,0.));
#63254=DIRECTION('',(1.,0.,0.));
#63255=DIRECTION('',(0.,-0.99026806874157,0.139173100960065));
#63256=DIRECTION('center_axis',(0.,0.996194698091746,-0.0871557427476593));
#63257=DIRECTION('ref_axis',(0.,0.0871557427476593,0.996194698091746));
#63258=DIRECTION('',(1.,0.,0.));
#63259=DIRECTION('center_axis',(0.,0.309016994374948,0.951056516295153));
#63260=DIRECTION('ref_axis',(0.,-0.951056516295153,0.309016994374948));
#63261=DIRECTION('',(1.,0.,0.));
#63262=DIRECTION('',(0.,-0.951056516295153,0.309016994374948));
#63263=DIRECTION('',(1.,0.,0.));
#63264=DIRECTION('',(-1.,0.,0.));
#63265=DIRECTION('',(1.,0.,0.));
#63266=DIRECTION('',(0.,-0.951056516295153,0.309016994374948));
#63267=DIRECTION('center_axis',(0.,0.965925826289068,-0.258819045102523));
#63268=DIRECTION('ref_axis',(0.,0.258819045102523,0.965925826289068));
#63269=DIRECTION('',(1.,0.,0.));
#63270=DIRECTION('center_axis',(0.,0.469471562785891,0.882947592858927));
#63271=DIRECTION('ref_axis',(0.,-0.882947592858927,0.469471562785891));
#63272=DIRECTION('',(1.,0.,0.));
#63273=DIRECTION('',(0.,-0.882947592858927,0.469471562785891));
#63274=DIRECTION('',(1.,0.,0.));
#63275=DIRECTION('',(-1.,0.,0.));
#63276=DIRECTION('',(1.,0.,0.));
#63277=DIRECTION('',(0.,-0.882947592858927,0.469471562785891));
#63278=DIRECTION('center_axis',(0.,0.906307787036649,-0.422618261740701));
#63279=DIRECTION('ref_axis',(0.,0.422618261740701,0.906307787036649));
#63280=DIRECTION('',(1.,0.,0.));
#63281=DIRECTION('center_axis',(0.,0.615661475325659,0.788010753606722));
#63282=DIRECTION('ref_axis',(0.,-0.788010753606722,0.615661475325659));
#63283=DIRECTION('',(1.,0.,0.));
#63284=DIRECTION('',(0.,-0.788010753606722,0.615661475325659));
#63285=DIRECTION('',(1.,0.,0.));
#63286=DIRECTION('',(-1.,0.,0.));
#63287=DIRECTION('',(1.,0.,0.));
#63288=DIRECTION('',(0.,-0.788010753606722,0.615661475325659));
#63289=DIRECTION('center_axis',(0.,0.819152044288991,-0.573576436351047));
#63290=DIRECTION('ref_axis',(0.,0.573576436351047,0.819152044288991));
#63291=DIRECTION('',(1.,0.,0.));
#63292=DIRECTION('center_axis',(0.,0.743144825477394,0.669130606358858));
#63293=DIRECTION('ref_axis',(0.,-0.669130606358858,0.743144825477394));
#63294=DIRECTION('',(1.,0.,0.));
#63295=DIRECTION('',(0.,-0.669130606358858,0.743144825477394));
#63296=DIRECTION('',(1.,0.,0.));
#63297=DIRECTION('',(-1.,0.,0.));
#63298=DIRECTION('',(1.,0.,0.));
#63299=DIRECTION('',(0.,-0.669130606358858,0.743144825477394));
#63300=DIRECTION('center_axis',(0.,0.707106781186547,-0.707106781186548));
#63301=DIRECTION('ref_axis',(0.,0.707106781186548,0.707106781186547));
#63302=DIRECTION('',(1.,0.,0.));
#63303=DIRECTION('center_axis',(0.,0.848048096156426,0.529919264233205));
#63304=DIRECTION('ref_axis',(0.,-0.529919264233205,0.848048096156426));
#63305=DIRECTION('',(1.,0.,0.));
#63306=DIRECTION('',(0.,-0.529919264233205,0.848048096156426));
#63307=DIRECTION('',(1.,0.,0.));
#63308=DIRECTION('',(-1.,0.,0.));
#63309=DIRECTION('',(1.,0.,0.));
#63310=DIRECTION('',(0.,-0.529919264233205,0.848048096156426));
#63311=DIRECTION('center_axis',(0.,0.573576436351045,-0.819152044288992));
#63312=DIRECTION('ref_axis',(0.,0.819152044288992,0.573576436351045));
#63313=DIRECTION('',(1.,0.,0.));
#63314=DIRECTION('center_axis',(0.,0.927183854566788,0.374606593415912));
#63315=DIRECTION('ref_axis',(0.,-0.374606593415912,0.927183854566788));
#63316=DIRECTION('',(1.,0.,0.));
#63317=DIRECTION('',(0.,-0.374606593415912,0.927183854566788));
#63318=DIRECTION('',(1.,0.,0.));
#63319=DIRECTION('',(-1.,0.,0.));
#63320=DIRECTION('',(1.,0.,0.));
#63321=DIRECTION('',(0.,-0.374606593415912,0.927183854566788));
#63322=DIRECTION('center_axis',(0.,0.422618261740698,-0.906307787036651));
#63323=DIRECTION('ref_axis',(0.,0.906307787036651,0.422618261740698));
#63324=DIRECTION('',(1.,0.,0.));
#63325=DIRECTION('center_axis',(0.,0.978147600733806,0.207911690817759));
#63326=DIRECTION('ref_axis',(0.,-0.207911690817759,0.978147600733806));
#63327=DIRECTION('',(1.,0.,0.));
#63328=DIRECTION('',(0.,-0.207911690817759,0.978147600733806));
#63329=DIRECTION('',(1.,0.,0.));
#63330=DIRECTION('',(-1.,0.,0.));
#63331=DIRECTION('',(1.,0.,0.));
#63332=DIRECTION('',(0.,-0.207911690817759,0.978147600733806));
#63333=DIRECTION('center_axis',(0.,0.258819045102519,-0.965925826289069));
#63334=DIRECTION('ref_axis',(0.,0.965925826289069,0.258819045102519));
#63335=DIRECTION('',(1.,0.,0.));
#63336=DIRECTION('center_axis',(0.,0.999390827019096,0.0348994967025009));
#63337=DIRECTION('ref_axis',(0.,-0.0348994967025009,0.999390827019096));
#63338=DIRECTION('',(1.,0.,0.));
#63339=DIRECTION('',(0.,-0.0348994967025009,0.999390827019096));
#63340=DIRECTION('',(1.,0.,0.));
#63341=DIRECTION('',(-1.,0.,0.));
#63342=DIRECTION('',(1.,0.,0.));
#63343=DIRECTION('',(0.,-0.0348994967025009,0.999390827019096));
#63344=DIRECTION('center_axis',(0.,0.0871557427476569,-0.996194698091746));
#63345=DIRECTION('ref_axis',(0.,0.996194698091746,0.0871557427476569));
#63346=DIRECTION('',(1.,0.,0.));
#63347=DIRECTION('center_axis',(0.,0.99026806874157,-0.139173100960065));
#63348=DIRECTION('ref_axis',(0.,0.139173100960065,0.99026806874157));
#63349=DIRECTION('',(1.,0.,0.));
#63350=DIRECTION('',(0.,0.139173100960065,0.99026806874157));
#63351=DIRECTION('',(1.,0.,0.));
#63352=DIRECTION('',(-1.,0.,0.));
#63353=DIRECTION('',(1.,0.,0.));
#63354=DIRECTION('',(0.,0.139173100960065,0.99026806874157));
#63355=DIRECTION('center_axis',(0.,-0.0871557427476592,-0.996194698091746));
#63356=DIRECTION('ref_axis',(0.,0.996194698091746,-0.0871557427476592));
#63357=DIRECTION('',(1.,0.,0.));
#63358=DIRECTION('center_axis',(0.,0.951056516295153,-0.309016994374948));
#63359=DIRECTION('ref_axis',(0.,0.309016994374948,0.951056516295153));
#63360=DIRECTION('',(1.,0.,0.));
#63361=DIRECTION('',(0.,0.309016994374948,0.951056516295153));
#63362=DIRECTION('',(1.,0.,0.));
#63363=DIRECTION('',(-1.,0.,0.));
#63364=DIRECTION('',(1.,0.,0.));
#63365=DIRECTION('',(0.,0.309016994374948,0.951056516295153));
#63366=DIRECTION('center_axis',(0.,-0.258819045102522,-0.965925826289068));
#63367=DIRECTION('ref_axis',(0.,0.965925826289068,-0.258819045102522));
#63368=DIRECTION('',(1.,0.,0.));
#63369=DIRECTION('center_axis',(0.,0.788010753606722,-0.615661475325658));
#63370=DIRECTION('ref_axis',(0.,0.615661475325658,0.788010753606722));
#63371=DIRECTION('',(1.,0.,0.));
#63372=DIRECTION('',(0.,0.615661475325658,0.788010753606722));
#63373=DIRECTION('',(1.,0.,0.));
#63374=DIRECTION('',(-1.,0.,0.));
#63375=DIRECTION('',(1.,0.,0.));
#63376=DIRECTION('',(0.,0.615661475325658,0.788010753606722));
#63377=DIRECTION('center_axis',(0.,-0.573576436351047,-0.819152044288991));
#63378=DIRECTION('ref_axis',(0.,0.819152044288991,-0.573576436351047));
#63379=DIRECTION('',(1.,0.,0.));
#63380=DIRECTION('center_axis',(0.,0.669130606358858,-0.743144825477394));
#63381=DIRECTION('ref_axis',(0.,0.743144825477394,0.669130606358858));
#63382=DIRECTION('',(1.,0.,0.));
#63383=DIRECTION('',(0.,0.743144825477394,0.669130606358858));
#63384=DIRECTION('',(1.,0.,0.));
#63385=DIRECTION('',(-1.,0.,0.));
#63386=DIRECTION('',(1.,0.,0.));
#63387=DIRECTION('',(0.,0.743144825477394,0.669130606358858));
#63388=DIRECTION('center_axis',(0.,-0.707106781186548,-0.707106781186547));
#63389=DIRECTION('ref_axis',(0.,0.707106781186547,-0.707106781186548));
#63390=DIRECTION('',(1.,0.,0.));
#63391=DIRECTION('center_axis',(0.,0.529919264233205,-0.848048096156426));
#63392=DIRECTION('ref_axis',(0.,0.848048096156426,0.529919264233205));
#63393=DIRECTION('',(1.,0.,0.));
#63394=DIRECTION('',(0.,0.848048096156426,0.529919264233205));
#63395=DIRECTION('',(1.,0.,0.));
#63396=DIRECTION('',(-1.,0.,0.));
#63397=DIRECTION('',(1.,0.,0.));
#63398=DIRECTION('',(0.,0.848048096156426,0.529919264233205));
#63399=DIRECTION('center_axis',(0.,-0.819152044288993,-0.573576436351045));
#63400=DIRECTION('ref_axis',(0.,0.573576436351045,-0.819152044288993));
#63401=DIRECTION('',(1.,0.,0.));
#63402=DIRECTION('center_axis',(0.,0.374606593415912,-0.927183854566787));
#63403=DIRECTION('ref_axis',(0.,0.927183854566787,0.374606593415912));
#63404=DIRECTION('',(1.,0.,0.));
#63405=DIRECTION('',(0.,0.927183854566787,0.374606593415912));
#63406=DIRECTION('',(1.,0.,0.));
#63407=DIRECTION('',(-1.,0.,0.));
#63408=DIRECTION('',(1.,0.,0.));
#63409=DIRECTION('',(0.,0.927183854566787,0.374606593415912));
#63410=DIRECTION('center_axis',(0.,-0.90630778703665,-0.422618261740698));
#63411=DIRECTION('ref_axis',(0.,0.422618261740698,-0.90630778703665));
#63412=DIRECTION('',(1.,0.,0.));
#63413=DIRECTION('center_axis',(0.,0.207911690817759,-0.978147600733806));
#63414=DIRECTION('ref_axis',(0.,0.978147600733806,0.207911690817759));
#63415=DIRECTION('',(1.,0.,0.));
#63416=DIRECTION('',(0.,0.978147600733806,0.207911690817759));
#63417=DIRECTION('',(1.,0.,0.));
#63418=DIRECTION('',(-1.,0.,0.));
#63419=DIRECTION('',(1.,0.,0.));
#63420=DIRECTION('',(0.,0.978147600733806,0.207911690817759));
#63421=DIRECTION('center_axis',(0.,-0.965925826289069,-0.258819045102519));
#63422=DIRECTION('ref_axis',(0.,0.258819045102519,-0.965925826289069));
#63423=DIRECTION('',(1.,0.,0.));
#63424=DIRECTION('center_axis',(0.,0.0348994967025009,-0.999390827019096));
#63425=DIRECTION('ref_axis',(0.,0.999390827019096,0.0348994967025009));
#63426=DIRECTION('',(1.,0.,0.));
#63427=DIRECTION('',(0.,0.999390827019096,0.0348994967025009));
#63428=DIRECTION('',(1.,0.,0.));
#63429=DIRECTION('',(-1.,0.,0.));
#63430=DIRECTION('',(1.,0.,0.));
#63431=DIRECTION('',(0.,0.999390827019096,0.0348994967025009));
#63432=DIRECTION('center_axis',(0.,-0.996194698091746,-0.087155742747657));
#63433=DIRECTION('ref_axis',(0.,0.087155742747657,-0.996194698091746));
#63434=DIRECTION('',(1.,0.,0.));
#63435=DIRECTION('center_axis',(0.,-0.139173100960066,-0.99026806874157));
#63436=DIRECTION('ref_axis',(0.,0.99026806874157,-0.139173100960066));
#63437=DIRECTION('',(1.,0.,0.));
#63438=DIRECTION('',(0.,0.99026806874157,-0.139173100960066));
#63439=DIRECTION('',(1.,0.,0.));
#63440=DIRECTION('',(-1.,0.,0.));
#63441=DIRECTION('',(1.,0.,0.));
#63442=DIRECTION('',(0.,0.99026806874157,-0.139173100960066));
#63443=DIRECTION('center_axis',(0.,-0.996194698091745,0.0871557427476596));
#63444=DIRECTION('ref_axis',(0.,-0.0871557427476596,-0.996194698091745));
#63445=DIRECTION('',(1.,0.,0.));
#63446=DIRECTION('center_axis',(0.,-0.309016994374948,-0.951056516295154));
#63447=DIRECTION('ref_axis',(0.,0.951056516295154,-0.309016994374948));
#63448=DIRECTION('',(1.,0.,0.));
#63449=DIRECTION('',(0.,0.951056516295154,-0.309016994374948));
#63450=DIRECTION('',(1.,0.,0.));
#63451=DIRECTION('',(-1.,0.,0.));
#63452=DIRECTION('',(1.,0.,0.));
#63453=DIRECTION('',(0.,0.951056516295154,-0.309016994374948));
#63454=DIRECTION('center_axis',(0.,-0.965925826289068,0.258819045102522));
#63455=DIRECTION('ref_axis',(0.,-0.258819045102522,-0.965925826289068));
#63456=DIRECTION('',(1.,0.,0.));
#63457=DIRECTION('center_axis',(0.,-0.469471562785891,-0.882947592858927));
#63458=DIRECTION('ref_axis',(0.,0.882947592858927,-0.469471562785891));
#63459=DIRECTION('',(1.,0.,0.));
#63460=DIRECTION('',(0.,0.882947592858927,-0.469471562785891));
#63461=DIRECTION('',(1.,0.,0.));
#63462=DIRECTION('',(-1.,0.,0.));
#63463=DIRECTION('',(1.,0.,0.));
#63464=DIRECTION('',(0.,0.882947592858927,-0.469471562785891));
#63465=DIRECTION('center_axis',(0.,-0.90630778703665,0.4226182617407));
#63466=DIRECTION('ref_axis',(0.,-0.4226182617407,-0.906307787036649));
#63467=DIRECTION('',(1.,0.,0.));
#63468=DIRECTION('center_axis',(0.,-0.615661475325658,-0.788010753606722));
#63469=DIRECTION('ref_axis',(0.,0.788010753606722,-0.615661475325658));
#63470=DIRECTION('',(1.,0.,0.));
#63471=DIRECTION('',(0.,0.788010753606722,-0.615661475325658));
#63472=DIRECTION('',(1.,0.,0.));
#63473=DIRECTION('',(-1.,0.,0.));
#63474=DIRECTION('',(1.,0.,0.));
#63475=DIRECTION('',(0.,0.788010753606722,-0.615661475325658));
#63476=DIRECTION('center_axis',(0.,-0.819152044288991,0.573576436351047));
#63477=DIRECTION('ref_axis',(0.,-0.573576436351047,-0.819152044288991));
#63478=DIRECTION('',(1.,0.,0.));
#63479=DIRECTION('center_axis',(0.,-0.743144825477394,-0.669130606358858));
#63480=DIRECTION('ref_axis',(0.,0.669130606358858,-0.743144825477394));
#63481=DIRECTION('',(1.,0.,0.));
#63482=DIRECTION('',(0.,0.669130606358858,-0.743144825477394));
#63483=DIRECTION('',(1.,0.,0.));
#63484=DIRECTION('',(-1.,0.,0.));
#63485=DIRECTION('',(1.,0.,0.));
#63486=DIRECTION('',(0.,0.669130606358858,-0.743144825477394));
#63487=DIRECTION('center_axis',(0.,-0.707106781186547,0.707106781186548));
#63488=DIRECTION('ref_axis',(0.,-0.707106781186548,-0.707106781186547));
#63489=DIRECTION('',(1.,0.,0.));
#63490=DIRECTION('center_axis',(0.,-0.927183854566787,-0.374606593415912));
#63491=DIRECTION('ref_axis',(0.,0.374606593415912,-0.927183854566787));
#63492=DIRECTION('',(1.,0.,0.));
#63493=DIRECTION('',(0.,0.374606593415912,-0.927183854566787));
#63494=DIRECTION('',(1.,0.,0.));
#63495=DIRECTION('',(-1.,0.,0.));
#63496=DIRECTION('',(1.,0.,0.));
#63497=DIRECTION('',(0.,0.374606593415912,-0.927183854566787));
#63498=DIRECTION('center_axis',(0.,-0.422618261740698,0.90630778703665));
#63499=DIRECTION('ref_axis',(0.,-0.90630778703665,-0.422618261740698));
#63500=DIRECTION('',(1.,0.,0.));
#63501=DIRECTION('center_axis',(0.,-0.978147600733806,-0.207911690817759));
#63502=DIRECTION('ref_axis',(0.,0.207911690817759,-0.978147600733806));
#63503=DIRECTION('',(1.,0.,0.));
#63504=DIRECTION('',(0.,0.207911690817759,-0.978147600733806));
#63505=DIRECTION('',(1.,0.,0.));
#63506=DIRECTION('',(-1.,0.,0.));
#63507=DIRECTION('',(1.,0.,0.));
#63508=DIRECTION('',(0.,0.207911690817759,-0.978147600733806));
#63509=DIRECTION('center_axis',(0.,-0.25881904510252,0.965925826289069));
#63510=DIRECTION('ref_axis',(0.,-0.965925826289069,-0.25881904510252));
#63511=DIRECTION('',(1.,0.,0.));
#63512=DIRECTION('center_axis',(0.,-0.999390827019096,-0.034899496702501));
#63513=DIRECTION('ref_axis',(0.,0.034899496702501,-0.999390827019096));
#63514=DIRECTION('',(1.,0.,0.));
#63515=DIRECTION('',(0.,0.034899496702501,-0.999390827019096));
#63516=DIRECTION('',(1.,0.,0.));
#63517=DIRECTION('',(-1.,0.,0.));
#63518=DIRECTION('',(1.,0.,0.));
#63519=DIRECTION('',(0.,0.034899496702501,-0.999390827019096));
#63520=DIRECTION('center_axis',(0.,-0.0871557427476571,0.996194698091746));
#63521=DIRECTION('ref_axis',(0.,-0.996194698091746,-0.0871557427476571));
#63522=DIRECTION('',(1.,0.,0.));
#63523=DIRECTION('center_axis',(0.,-0.99026806874157,0.139173100960065));
#63524=DIRECTION('ref_axis',(0.,-0.139173100960065,-0.99026806874157));
#63525=DIRECTION('',(1.,0.,0.));
#63526=DIRECTION('',(0.,-0.139173100960065,-0.99026806874157));
#63527=DIRECTION('',(1.,0.,0.));
#63528=DIRECTION('',(-1.,0.,0.));
#63529=DIRECTION('',(1.,0.,0.));
#63530=DIRECTION('',(0.,-0.139173100960065,-0.99026806874157));
#63531=DIRECTION('center_axis',(0.,0.0871557427476593,0.996194698091746));
#63532=DIRECTION('ref_axis',(0.,-0.996194698091746,0.0871557427476593));
#63533=DIRECTION('',(1.,0.,0.));
#63534=DIRECTION('center_axis',(0.,-0.951056516295154,0.309016994374948));
#63535=DIRECTION('ref_axis',(0.,-0.309016994374948,-0.951056516295154));
#63536=DIRECTION('',(1.,0.,0.));
#63537=DIRECTION('',(0.,-0.309016994374948,-0.951056516295154));
#63538=DIRECTION('',(1.,0.,0.));
#63539=DIRECTION('',(-1.,0.,0.));
#63540=DIRECTION('',(1.,0.,0.));
#63541=DIRECTION('',(0.,-0.309016994374948,-0.951056516295154));
#63542=DIRECTION('center_axis',(0.,0.258819045102522,0.965925826289068));
#63543=DIRECTION('ref_axis',(0.,-0.965925826289068,0.258819045102522));
#63544=DIRECTION('',(1.,0.,0.));
#63545=DIRECTION('center_axis',(0.,-0.882947592858927,0.469471562785891));
#63546=DIRECTION('ref_axis',(0.,-0.469471562785891,-0.882947592858927));
#63547=DIRECTION('',(1.,0.,0.));
#63548=DIRECTION('',(0.,-0.469471562785891,-0.882947592858927));
#63549=DIRECTION('',(1.,0.,0.));
#63550=DIRECTION('',(-1.,0.,0.));
#63551=DIRECTION('',(1.,0.,0.));
#63552=DIRECTION('',(0.,-0.469471562785891,-0.882947592858927));
#63553=DIRECTION('center_axis',(0.,0.422618261740701,0.906307787036649));
#63554=DIRECTION('ref_axis',(0.,-0.906307787036649,0.4226182617407));
#63555=DIRECTION('',(1.,0.,0.));
#63556=DIRECTION('center_axis',(0.,-0.788010753606722,0.615661475325658));
#63557=DIRECTION('ref_axis',(0.,-0.615661475325658,-0.788010753606722));
#63558=DIRECTION('',(1.,0.,0.));
#63559=DIRECTION('',(0.,-0.615661475325658,-0.788010753606722));
#63560=DIRECTION('',(1.,0.,0.));
#63561=DIRECTION('',(-1.,0.,0.));
#63562=DIRECTION('',(1.,0.,0.));
#63563=DIRECTION('',(0.,-0.615661475325658,-0.788010753606722));
#63564=DIRECTION('center_axis',(0.,0.573576436351047,0.819152044288991));
#63565=DIRECTION('ref_axis',(0.,-0.819152044288991,0.573576436351047));
#63566=DIRECTION('',(1.,0.,0.));
#63567=DIRECTION('center_axis',(0.,-0.669130606358858,0.743144825477394));
#63568=DIRECTION('ref_axis',(0.,-0.743144825477394,-0.669130606358858));
#63569=DIRECTION('',(1.,0.,0.));
#63570=DIRECTION('',(0.,-0.743144825477394,-0.669130606358858));
#63571=DIRECTION('',(1.,0.,0.));
#63572=DIRECTION('',(-1.,0.,0.));
#63573=DIRECTION('',(1.,0.,0.));
#63574=DIRECTION('',(0.,-0.743144825477394,-0.669130606358858));
#63575=DIRECTION('center_axis',(0.,0.707106781186548,0.707106781186547));
#63576=DIRECTION('ref_axis',(0.,-0.707106781186547,0.707106781186548));
#63577=DIRECTION('',(1.,0.,0.));
#63578=DIRECTION('center_axis',(0.,-0.529919264233205,0.848048096156426));
#63579=DIRECTION('ref_axis',(0.,-0.848048096156426,-0.529919264233205));
#63580=DIRECTION('',(1.,0.,0.));
#63581=DIRECTION('',(0.,-0.848048096156426,-0.529919264233205));
#63582=DIRECTION('',(1.,0.,0.));
#63583=DIRECTION('',(-1.,0.,0.));
#63584=DIRECTION('',(1.,0.,0.));
#63585=DIRECTION('',(0.,-0.848048096156426,-0.529919264233205));
#63586=DIRECTION('center_axis',(0.,0.819152044288993,0.573576436351045));
#63587=DIRECTION('ref_axis',(0.,-0.573576436351045,0.819152044288992));
#63588=DIRECTION('',(1.,0.,0.));
#63589=DIRECTION('center_axis',(0.,-0.374606593415912,0.927183854566787));
#63590=DIRECTION('ref_axis',(0.,-0.927183854566787,-0.374606593415912));
#63591=DIRECTION('',(1.,0.,0.));
#63592=DIRECTION('',(0.,-0.927183854566787,-0.374606593415912));
#63593=DIRECTION('',(1.,0.,0.));
#63594=DIRECTION('',(-1.,0.,0.));
#63595=DIRECTION('',(1.,0.,0.));
#63596=DIRECTION('',(0.,-0.927183854566787,-0.374606593415912));
#63597=DIRECTION('center_axis',(0.,0.90630778703665,0.422618261740698));
#63598=DIRECTION('ref_axis',(0.,-0.422618261740698,0.90630778703665));
#63599=DIRECTION('',(1.,0.,0.));
#63600=DIRECTION('center_axis',(0.,-0.207911690817759,0.978147600733806));
#63601=DIRECTION('ref_axis',(0.,-0.978147600733806,-0.207911690817759));
#63602=DIRECTION('',(1.,0.,0.));
#63603=DIRECTION('',(0.,-0.978147600733806,-0.207911690817759));
#63604=DIRECTION('',(1.,0.,0.));
#63605=DIRECTION('',(-1.,0.,0.));
#63606=DIRECTION('',(1.,0.,0.));
#63607=DIRECTION('',(0.,-0.978147600733806,-0.207911690817759));
#63608=DIRECTION('center_axis',(0.,0.965925826289069,0.25881904510252));
#63609=DIRECTION('ref_axis',(0.,-0.25881904510252,0.965925826289069));
#63610=DIRECTION('',(1.,0.,0.));
#63611=DIRECTION('center_axis',(1.,0.,0.));
#63612=DIRECTION('ref_axis',(0.,1.,0.));
#63613=DIRECTION('center_axis',(-1.,0.,0.));
#63614=DIRECTION('ref_axis',(0.,1.,0.));
#63615=DIRECTION('center_axis',(1.,0.,0.));
#63616=DIRECTION('ref_axis',(0.,1.,0.));
#63617=DIRECTION('center_axis',(-1.,0.,0.));
#63618=DIRECTION('ref_axis',(0.,1.,0.));
#63619=DIRECTION('center_axis',(1.,0.,0.));
#63620=DIRECTION('ref_axis',(0.,1.,0.));
#63621=DIRECTION('center_axis',(-1.,0.,0.));
#63622=DIRECTION('ref_axis',(0.,1.,0.));
#63623=DIRECTION('center_axis',(1.,0.,0.));
#63624=DIRECTION('ref_axis',(0.,1.,0.));
#63625=DIRECTION('center_axis',(-1.,0.,0.));
#63626=DIRECTION('ref_axis',(0.,1.,0.));
#63627=DIRECTION('center_axis',(1.,0.,0.));
#63628=DIRECTION('ref_axis',(0.,1.,0.));
#63629=DIRECTION('center_axis',(-1.,0.,0.));
#63630=DIRECTION('ref_axis',(0.,1.,0.));
#63631=DIRECTION('center_axis',(1.,0.,0.));
#63632=DIRECTION('ref_axis',(0.,1.,0.));
#63633=DIRECTION('center_axis',(-1.,0.,0.));
#63634=DIRECTION('ref_axis',(0.,1.,0.));
#63635=DIRECTION('center_axis',(1.,0.,0.));
#63636=DIRECTION('ref_axis',(0.,1.,0.));
#63637=DIRECTION('center_axis',(-1.,0.,0.));
#63638=DIRECTION('ref_axis',(0.,1.,0.));
#63639=DIRECTION('center_axis',(1.,0.,0.));
#63640=DIRECTION('ref_axis',(0.,1.,0.));
#63641=DIRECTION('center_axis',(-1.,0.,0.));
#63642=DIRECTION('ref_axis',(0.,1.,0.));
#63643=DIRECTION('center_axis',(1.,0.,0.));
#63644=DIRECTION('ref_axis',(0.,1.,0.));
#63645=DIRECTION('center_axis',(-1.,0.,0.));
#63646=DIRECTION('ref_axis',(0.,1.,0.));
#63647=DIRECTION('center_axis',(1.,0.,0.));
#63648=DIRECTION('ref_axis',(0.,1.,0.));
#63649=DIRECTION('center_axis',(-1.,0.,0.));
#63650=DIRECTION('ref_axis',(0.,1.,0.));
#63651=DIRECTION('center_axis',(1.,0.,0.));
#63652=DIRECTION('ref_axis',(0.,1.,0.));
#63653=DIRECTION('center_axis',(-1.,0.,0.));
#63654=DIRECTION('ref_axis',(0.,1.,0.));
#63655=DIRECTION('center_axis',(1.,0.,0.));
#63656=DIRECTION('ref_axis',(0.,1.,0.));
#63657=DIRECTION('center_axis',(-1.,0.,0.));
#63658=DIRECTION('ref_axis',(0.,1.,0.));
#63659=DIRECTION('center_axis',(1.,0.,0.));
#63660=DIRECTION('ref_axis',(0.,1.,0.));
#63661=DIRECTION('center_axis',(-1.,0.,0.));
#63662=DIRECTION('ref_axis',(0.,1.,0.));
#63663=DIRECTION('center_axis',(1.,0.,0.));
#63664=DIRECTION('ref_axis',(0.,1.,0.));
#63665=DIRECTION('center_axis',(-1.,0.,0.));
#63666=DIRECTION('ref_axis',(0.,1.,0.));
#63667=DIRECTION('center_axis',(1.,0.,0.));
#63668=DIRECTION('ref_axis',(0.,1.,0.));
#63669=DIRECTION('center_axis',(-1.,0.,0.));
#63670=DIRECTION('ref_axis',(0.,1.,0.));
#63671=DIRECTION('center_axis',(1.,0.,0.));
#63672=DIRECTION('ref_axis',(0.,1.,0.));
#63673=DIRECTION('center_axis',(-1.,0.,0.));
#63674=DIRECTION('ref_axis',(0.,1.,0.));
#63675=DIRECTION('center_axis',(1.,0.,0.));
#63676=DIRECTION('ref_axis',(0.,1.,0.));
#63677=DIRECTION('center_axis',(-1.,0.,0.));
#63678=DIRECTION('ref_axis',(0.,1.,0.));
#63679=DIRECTION('center_axis',(1.,0.,0.));
#63680=DIRECTION('ref_axis',(0.,1.,0.));
#63681=DIRECTION('center_axis',(-1.,0.,0.));
#63682=DIRECTION('ref_axis',(0.,1.,0.));
#63683=DIRECTION('center_axis',(1.,0.,0.));
#63684=DIRECTION('ref_axis',(0.,1.,0.));
#63685=DIRECTION('center_axis',(-1.,0.,0.));
#63686=DIRECTION('ref_axis',(0.,1.,0.));
#63687=DIRECTION('center_axis',(1.,0.,0.));
#63688=DIRECTION('ref_axis',(0.,1.,0.));
#63689=DIRECTION('center_axis',(-1.,0.,0.));
#63690=DIRECTION('ref_axis',(0.,1.,0.));
#63691=DIRECTION('center_axis',(1.,0.,0.));
#63692=DIRECTION('ref_axis',(0.,1.,0.));
#63693=DIRECTION('center_axis',(-1.,0.,0.));
#63694=DIRECTION('ref_axis',(0.,1.,0.));
#63695=DIRECTION('center_axis',(1.,0.,0.));
#63696=DIRECTION('ref_axis',(0.,1.,0.));
#63697=DIRECTION('center_axis',(-1.,0.,0.));
#63698=DIRECTION('ref_axis',(0.,1.,0.));
#63699=DIRECTION('center_axis',(1.,0.,0.));
#63700=DIRECTION('ref_axis',(0.,1.,0.));
#63701=DIRECTION('center_axis',(-1.,0.,0.));
#63702=DIRECTION('ref_axis',(0.,1.,0.));
#63703=DIRECTION('center_axis',(1.,0.,0.));
#63704=DIRECTION('ref_axis',(0.,1.,0.));
#63705=DIRECTION('center_axis',(-1.,0.,0.));
#63706=DIRECTION('ref_axis',(0.,1.,0.));
#63707=DIRECTION('center_axis',(1.,0.,0.));
#63708=DIRECTION('ref_axis',(0.,1.,0.));
#63709=DIRECTION('center_axis',(-1.,0.,0.));
#63710=DIRECTION('ref_axis',(0.,1.,0.));
#63711=DIRECTION('center_axis',(1.,0.,0.));
#63712=DIRECTION('ref_axis',(0.,1.,0.));
#63713=DIRECTION('center_axis',(-1.,0.,0.));
#63714=DIRECTION('ref_axis',(0.,1.,0.));
#63715=DIRECTION('center_axis',(1.,0.,0.));
#63716=DIRECTION('ref_axis',(0.,1.,0.));
#63717=DIRECTION('center_axis',(-1.,0.,0.));
#63718=DIRECTION('ref_axis',(0.,1.,0.));
#63719=DIRECTION('center_axis',(1.,0.,0.));
#63720=DIRECTION('ref_axis',(0.,1.,0.));
#63721=DIRECTION('center_axis',(-1.,0.,0.));
#63722=DIRECTION('ref_axis',(0.,1.,0.));
#63723=DIRECTION('center_axis',(1.,0.,0.));
#63724=DIRECTION('ref_axis',(0.,1.,0.));
#63725=DIRECTION('center_axis',(-1.,0.,0.));
#63726=DIRECTION('ref_axis',(0.,1.,0.));
#63727=DIRECTION('center_axis',(1.,0.,0.));
#63728=DIRECTION('ref_axis',(0.,1.,0.));
#63729=DIRECTION('center_axis',(-1.,0.,0.));
#63730=DIRECTION('ref_axis',(0.,1.,0.));
#63731=DIRECTION('center_axis',(1.,0.,0.));
#63732=DIRECTION('ref_axis',(0.,1.,0.));
#63733=DIRECTION('center_axis',(-1.,0.,0.));
#63734=DIRECTION('ref_axis',(0.,1.,0.));
#63735=DIRECTION('center_axis',(1.,0.,0.));
#63736=DIRECTION('ref_axis',(0.,1.,0.));
#63737=DIRECTION('center_axis',(-1.,0.,0.));
#63738=DIRECTION('ref_axis',(0.,1.,0.));
#63739=DIRECTION('center_axis',(1.,0.,0.));
#63740=DIRECTION('ref_axis',(0.,1.,0.));
#63741=DIRECTION('center_axis',(-1.,0.,0.));
#63742=DIRECTION('ref_axis',(0.,1.,0.));
#63743=DIRECTION('center_axis',(0.,-0.0348994967025009,-0.999390827019096));
#63744=DIRECTION('ref_axis',(0.,0.999390827019096,-0.0348994967025009));
#63745=DIRECTION('',(0.,0.999390827019096,-0.0348994967025009));
#63746=DIRECTION('',(1.,0.,0.));
#63747=DIRECTION('',(1.,0.,0.));
#63748=DIRECTION('',(1.,0.,0.));
#63749=DIRECTION('',(0.,0.999390827019096,-0.0348994967025009));
#63750=DIRECTION('center_axis',(0.,-0.20791169081776,-0.978147600733805));
#63751=DIRECTION('ref_axis',(0.,0.978147600733805,-0.20791169081776));
#63752=DIRECTION('',(0.,0.978147600733805,-0.20791169081776));
#63753=DIRECTION('',(1.,0.,0.));
#63754=DIRECTION('',(1.,0.,0.));
#63755=DIRECTION('',(1.,0.,0.));
#63756=DIRECTION('',(0.,0.978147600733805,-0.20791169081776));
#63757=DIRECTION('center_axis',(0.,-0.374606593415912,-0.927183854566787));
#63758=DIRECTION('ref_axis',(0.,0.927183854566787,-0.374606593415912));
#63759=DIRECTION('',(0.,0.927183854566787,-0.374606593415912));
#63760=DIRECTION('',(1.,0.,0.));
#63761=DIRECTION('',(1.,0.,0.));
#63762=DIRECTION('',(1.,0.,0.));
#63763=DIRECTION('',(0.,0.927183854566787,-0.374606593415912));
#63764=DIRECTION('center_axis',(0.,-0.529919264233205,-0.848048096156426));
#63765=DIRECTION('ref_axis',(0.,0.848048096156426,-0.529919264233205));
#63766=DIRECTION('',(0.,0.848048096156426,-0.529919264233205));
#63767=DIRECTION('',(1.,0.,0.));
#63768=DIRECTION('',(1.,0.,0.));
#63769=DIRECTION('',(1.,0.,0.));
#63770=DIRECTION('',(0.,0.848048096156426,-0.529919264233205));
#63771=DIRECTION('center_axis',(0.,-0.669130606358858,-0.743144825477394));
#63772=DIRECTION('ref_axis',(0.,0.743144825477394,-0.669130606358858));
#63773=DIRECTION('',(0.,0.743144825477394,-0.669130606358858));
#63774=DIRECTION('',(1.,0.,0.));
#63775=DIRECTION('',(1.,0.,0.));
#63776=DIRECTION('',(1.,0.,0.));
#63777=DIRECTION('',(0.,0.743144825477394,-0.669130606358858));
#63778=DIRECTION('center_axis',(0.,-0.788010753606722,-0.615661475325659));
#63779=DIRECTION('ref_axis',(0.,0.615661475325658,-0.788010753606722));
#63780=DIRECTION('',(0.,0.615661475325658,-0.788010753606722));
#63781=DIRECTION('',(1.,0.,0.));
#63782=DIRECTION('',(1.,0.,0.));
#63783=DIRECTION('',(1.,0.,0.));
#63784=DIRECTION('',(0.,0.615661475325658,-0.788010753606722));
#63785=DIRECTION('center_axis',(0.,-0.882947592858927,-0.46947156278589));
#63786=DIRECTION('ref_axis',(0.,0.46947156278589,-0.882947592858927));
#63787=DIRECTION('',(0.,0.46947156278589,-0.882947592858927));
#63788=DIRECTION('',(1.,0.,0.));
#63789=DIRECTION('',(1.,0.,0.));
#63790=DIRECTION('',(1.,0.,0.));
#63791=DIRECTION('',(0.,0.46947156278589,-0.882947592858927));
#63792=DIRECTION('center_axis',(0.,-0.951056516295154,-0.309016994374947));
#63793=DIRECTION('ref_axis',(0.,0.309016994374947,-0.951056516295154));
#63794=DIRECTION('',(0.,0.309016994374947,-0.951056516295154));
#63795=DIRECTION('',(1.,0.,0.));
#63796=DIRECTION('',(1.,0.,0.));
#63797=DIRECTION('',(1.,0.,0.));
#63798=DIRECTION('',(0.,0.309016994374947,-0.951056516295154));
#63799=DIRECTION('center_axis',(0.,-0.99026806874157,-0.139173100960065));
#63800=DIRECTION('ref_axis',(0.,0.139173100960065,-0.99026806874157));
#63801=DIRECTION('',(0.,0.139173100960065,-0.99026806874157));
#63802=DIRECTION('',(1.,0.,0.));
#63803=DIRECTION('',(1.,0.,0.));
#63804=DIRECTION('',(1.,0.,0.));
#63805=DIRECTION('',(0.,0.139173100960065,-0.99026806874157));
#63806=DIRECTION('center_axis',(0.,-0.999390827019096,0.0348994967025009));
#63807=DIRECTION('ref_axis',(0.,-0.0348994967025009,-0.999390827019096));
#63808=DIRECTION('',(0.,-0.0348994967025009,-0.999390827019096));
#63809=DIRECTION('',(1.,0.,0.));
#63810=DIRECTION('',(1.,0.,0.));
#63811=DIRECTION('',(1.,0.,0.));
#63812=DIRECTION('',(0.,-0.0348994967025009,-0.999390827019096));
#63813=DIRECTION('center_axis',(0.,-0.978147600733806,0.20791169081776));
#63814=DIRECTION('ref_axis',(0.,-0.20791169081776,-0.978147600733805));
#63815=DIRECTION('',(0.,-0.20791169081776,-0.978147600733805));
#63816=DIRECTION('',(1.,0.,0.));
#63817=DIRECTION('',(1.,0.,0.));
#63818=DIRECTION('',(0.,-0.20791169081776,-0.978147600733805));
#63819=DIRECTION('center_axis',(0.,-0.848048096156426,0.529919264233205));
#63820=DIRECTION('ref_axis',(0.,-0.529919264233205,-0.848048096156426));
#63821=DIRECTION('',(0.,-0.529919264233205,-0.848048096156426));
#63822=DIRECTION('',(1.,0.,0.));
#63823=DIRECTION('',(1.,0.,0.));
#63824=DIRECTION('',(1.,0.,0.));
#63825=DIRECTION('',(0.,-0.529919264233205,-0.848048096156426));
#63826=DIRECTION('center_axis',(0.,-0.743144825477394,0.669130606358858));
#63827=DIRECTION('ref_axis',(0.,-0.669130606358858,-0.743144825477394));
#63828=DIRECTION('',(0.,-0.669130606358858,-0.743144825477394));
#63829=DIRECTION('',(1.,0.,0.));
#63830=DIRECTION('',(1.,0.,0.));
#63831=DIRECTION('',(1.,0.,0.));
#63832=DIRECTION('',(0.,-0.669130606358858,-0.743144825477394));
#63833=DIRECTION('center_axis',(0.,-0.615661475325658,0.788010753606722));
#63834=DIRECTION('ref_axis',(0.,-0.788010753606722,-0.615661475325658));
#63835=DIRECTION('',(0.,-0.788010753606722,-0.615661475325658));
#63836=DIRECTION('',(1.,0.,0.));
#63837=DIRECTION('',(1.,0.,0.));
#63838=DIRECTION('',(1.,0.,0.));
#63839=DIRECTION('',(0.,-0.788010753606722,-0.615661475325658));
#63840=DIRECTION('center_axis',(0.,-0.469471562785891,0.882947592858927));
#63841=DIRECTION('ref_axis',(0.,-0.882947592858927,-0.469471562785891));
#63842=DIRECTION('',(0.,-0.882947592858927,-0.469471562785891));
#63843=DIRECTION('',(1.,0.,0.));
#63844=DIRECTION('',(1.,0.,0.));
#63845=DIRECTION('',(1.,0.,0.));
#63846=DIRECTION('',(0.,-0.882947592858927,-0.469471562785891));
#63847=DIRECTION('center_axis',(0.,-0.309016994374947,0.951056516295154));
#63848=DIRECTION('ref_axis',(0.,-0.951056516295154,-0.309016994374947));
#63849=DIRECTION('',(0.,-0.951056516295154,-0.309016994374947));
#63850=DIRECTION('',(1.,0.,0.));
#63851=DIRECTION('',(1.,0.,0.));
#63852=DIRECTION('',(1.,0.,0.));
#63853=DIRECTION('',(0.,-0.951056516295154,-0.309016994374947));
#63854=DIRECTION('center_axis',(0.,-0.139173100960065,0.99026806874157));
#63855=DIRECTION('ref_axis',(0.,-0.99026806874157,-0.139173100960065));
#63856=DIRECTION('',(0.,-0.99026806874157,-0.139173100960065));
#63857=DIRECTION('',(1.,0.,0.));
#63858=DIRECTION('',(1.,0.,0.));
#63859=DIRECTION('',(1.,0.,0.));
#63860=DIRECTION('',(0.,-0.99026806874157,-0.139173100960065));
#63861=DIRECTION('center_axis',(0.,0.0348994967025012,0.999390827019096));
#63862=DIRECTION('ref_axis',(0.,-0.999390827019096,0.0348994967025012));
#63863=DIRECTION('',(0.,-0.999390827019096,0.0348994967025012));
#63864=DIRECTION('',(1.,0.,0.));
#63865=DIRECTION('',(1.,0.,0.));
#63866=DIRECTION('',(1.,0.,0.));
#63867=DIRECTION('',(0.,-0.999390827019096,0.0348994967025012));
#63868=DIRECTION('center_axis',(0.,0.207911690817759,0.978147600733806));
#63869=DIRECTION('ref_axis',(0.,-0.978147600733806,0.207911690817759));
#63870=DIRECTION('',(0.,-0.978147600733806,0.207911690817759));
#63871=DIRECTION('',(1.,0.,0.));
#63872=DIRECTION('',(1.,0.,0.));
#63873=DIRECTION('',(1.,0.,0.));
#63874=DIRECTION('',(0.,-0.978147600733806,0.207911690817759));
#63875=DIRECTION('center_axis',(0.,0.374606593415912,0.927183854566788));
#63876=DIRECTION('ref_axis',(0.,-0.927183854566787,0.374606593415912));
#63877=DIRECTION('',(0.,-0.927183854566787,0.374606593415912));
#63878=DIRECTION('',(1.,0.,0.));
#63879=DIRECTION('',(1.,0.,0.));
#63880=DIRECTION('',(1.,0.,0.));
#63881=DIRECTION('',(0.,-0.927183854566787,0.374606593415912));
#63882=DIRECTION('center_axis',(0.,0.529919264233205,0.848048096156426));
#63883=DIRECTION('ref_axis',(0.,-0.848048096156426,0.529919264233205));
#63884=DIRECTION('',(0.,-0.848048096156426,0.529919264233205));
#63885=DIRECTION('',(1.,0.,0.));
#63886=DIRECTION('',(1.,0.,0.));
#63887=DIRECTION('',(1.,0.,0.));
#63888=DIRECTION('',(0.,-0.848048096156426,0.529919264233205));
#63889=DIRECTION('center_axis',(0.,0.669130606358858,0.743144825477394));
#63890=DIRECTION('ref_axis',(0.,-0.743144825477394,0.669130606358858));
#63891=DIRECTION('',(0.,-0.743144825477394,0.669130606358858));
#63892=DIRECTION('',(1.,0.,0.));
#63893=DIRECTION('',(1.,0.,0.));
#63894=DIRECTION('',(0.,-0.743144825477394,0.669130606358858));
#63895=DIRECTION('center_axis',(0.,0.882947592858927,0.469471562785891));
#63896=DIRECTION('ref_axis',(0.,-0.469471562785891,0.882947592858927));
#63897=DIRECTION('',(0.,-0.469471562785891,0.882947592858927));
#63898=DIRECTION('',(1.,0.,0.));
#63899=DIRECTION('',(1.,0.,0.));
#63900=DIRECTION('',(1.,0.,0.));
#63901=DIRECTION('',(0.,-0.469471562785891,0.882947592858927));
#63902=DIRECTION('center_axis',(0.,0.951056516295154,0.309016994374948));
#63903=DIRECTION('ref_axis',(0.,-0.309016994374948,0.951056516295154));
#63904=DIRECTION('',(0.,-0.309016994374948,0.951056516295154));
#63905=DIRECTION('',(1.,0.,0.));
#63906=DIRECTION('',(1.,0.,0.));
#63907=DIRECTION('',(1.,0.,0.));
#63908=DIRECTION('',(0.,-0.309016994374948,0.951056516295154));
#63909=DIRECTION('center_axis',(0.,0.99026806874157,0.139173100960065));
#63910=DIRECTION('ref_axis',(0.,-0.139173100960065,0.99026806874157));
#63911=DIRECTION('',(0.,-0.139173100960065,0.99026806874157));
#63912=DIRECTION('',(1.,0.,0.));
#63913=DIRECTION('',(1.,0.,0.));
#63914=DIRECTION('',(1.,0.,0.));
#63915=DIRECTION('',(0.,-0.139173100960065,0.99026806874157));
#63916=DIRECTION('center_axis',(0.,0.999390827019096,-0.0348994967025009));
#63917=DIRECTION('ref_axis',(0.,0.0348994967025009,0.999390827019096));
#63918=DIRECTION('',(0.,0.0348994967025009,0.999390827019096));
#63919=DIRECTION('',(1.,0.,0.));
#63920=DIRECTION('',(1.,0.,0.));
#63921=DIRECTION('',(1.,0.,0.));
#63922=DIRECTION('',(0.,0.0348994967025009,0.999390827019096));
#63923=DIRECTION('center_axis',(0.,0.978147600733806,-0.207911690817759));
#63924=DIRECTION('ref_axis',(0.,0.207911690817759,0.978147600733806));
#63925=DIRECTION('',(0.,0.207911690817759,0.978147600733806));
#63926=DIRECTION('',(1.,0.,0.));
#63927=DIRECTION('',(1.,0.,0.));
#63928=DIRECTION('',(1.,0.,0.));
#63929=DIRECTION('',(0.,0.207911690817759,0.978147600733806));
#63930=DIRECTION('center_axis',(0.,0.927183854566787,-0.374606593415912));
#63931=DIRECTION('ref_axis',(0.,0.374606593415912,0.927183854566787));
#63932=DIRECTION('',(0.,0.374606593415912,0.927183854566787));
#63933=DIRECTION('',(1.,0.,0.));
#63934=DIRECTION('',(1.,0.,0.));
#63935=DIRECTION('',(1.,0.,0.));
#63936=DIRECTION('',(0.,0.374606593415912,0.927183854566787));
#63937=DIRECTION('center_axis',(0.,0.848048096156426,-0.529919264233205));
#63938=DIRECTION('ref_axis',(0.,0.529919264233205,0.848048096156426));
#63939=DIRECTION('',(0.,0.529919264233205,0.848048096156426));
#63940=DIRECTION('',(1.,0.,0.));
#63941=DIRECTION('',(1.,0.,0.));
#63942=DIRECTION('',(1.,0.,0.));
#63943=DIRECTION('',(0.,0.529919264233205,0.848048096156426));
#63944=DIRECTION('center_axis',(0.,0.743144825477394,-0.669130606358858));
#63945=DIRECTION('ref_axis',(0.,0.669130606358858,0.743144825477394));
#63946=DIRECTION('',(0.,0.669130606358858,0.743144825477394));
#63947=DIRECTION('',(1.,0.,0.));
#63948=DIRECTION('',(1.,0.,0.));
#63949=DIRECTION('',(1.,0.,0.));
#63950=DIRECTION('',(0.,0.669130606358858,0.743144825477394));
#63951=DIRECTION('center_axis',(0.,0.615661475325658,-0.788010753606722));
#63952=DIRECTION('ref_axis',(0.,0.788010753606722,0.615661475325658));
#63953=DIRECTION('',(0.,0.788010753606722,0.615661475325658));
#63954=DIRECTION('',(1.,0.,0.));
#63955=DIRECTION('',(1.,0.,0.));
#63956=DIRECTION('',(1.,0.,0.));
#63957=DIRECTION('',(0.,0.788010753606722,0.615661475325658));
#63958=DIRECTION('center_axis',(0.,0.469471562785891,-0.882947592858927));
#63959=DIRECTION('ref_axis',(0.,0.882947592858927,0.469471562785891));
#63960=DIRECTION('',(0.,0.882947592858927,0.469471562785891));
#63961=DIRECTION('',(1.,0.,0.));
#63962=DIRECTION('',(1.,0.,0.));
#63963=DIRECTION('',(1.,0.,0.));
#63964=DIRECTION('',(0.,0.882947592858927,0.469471562785891));
#63965=DIRECTION('center_axis',(0.,0.309016994374948,-0.951056516295154));
#63966=DIRECTION('ref_axis',(0.,0.951056516295154,0.309016994374948));
#63967=DIRECTION('',(0.,0.951056516295154,0.309016994374948));
#63968=DIRECTION('',(1.,0.,0.));
#63969=DIRECTION('',(1.,0.,0.));
#63970=DIRECTION('',(0.,0.951056516295154,0.309016994374948));
#63971=DIRECTION('center_axis',(0.,-0.996194698091746,0.0871557427476582));
#63972=DIRECTION('ref_axis',(0.,-0.0871557427476581,-0.996194698091746));
#63973=DIRECTION('',(0.,-0.0871557427476581,-0.996194698091746));
#63974=DIRECTION('center_axis',(0.,-0.996194698091746,0.0871557427476582));
#63975=DIRECTION('ref_axis',(0.,-0.0871557427476581,-0.996194698091746));
#63976=DIRECTION('',(0.,-0.0871557427476581,-0.996194698091746));
#63977=DIRECTION('center_axis',(1.,0.,0.));
#63978=DIRECTION('ref_axis',(0.,-0.17364817766693,-0.984807753012208));
#63979=DIRECTION('center_axis',(1.,0.,0.));
#63980=DIRECTION('ref_axis',(0.,-0.17364817766693,-0.984807753012208));
#63981=DIRECTION('center_axis',(1.,0.,0.));
#63982=DIRECTION('ref_axis',(0.,1.,0.));
#63983=DIRECTION('center_axis',(1.,0.,0.));
#63984=DIRECTION('ref_axis',(0.,1.,0.));
#63985=DIRECTION('center_axis',(0.,-0.965925826289068,0.258819045102521));
#63986=DIRECTION('ref_axis',(0.,-0.258819045102521,-0.965925826289068));
#63987=DIRECTION('',(0.,-0.258819045102521,-0.965925826289068));
#63988=DIRECTION('center_axis',(0.,-0.965925826289068,0.258819045102521));
#63989=DIRECTION('ref_axis',(0.,-0.258819045102521,-0.965925826289068));
#63990=DIRECTION('',(0.,-0.258819045102521,-0.965925826289068));
#63991=DIRECTION('center_axis',(1.,0.,0.));
#63992=DIRECTION('ref_axis',(0.,-0.342020143325669,-0.939692620785908));
#63993=DIRECTION('center_axis',(1.,0.,0.));
#63994=DIRECTION('ref_axis',(0.,-0.342020143325669,-0.939692620785908));
#63995=DIRECTION('center_axis',(1.,0.,0.));
#63996=DIRECTION('ref_axis',(0.,1.,0.));
#63997=DIRECTION('center_axis',(0.,-0.90630778703665,0.4226182617407));
#63998=DIRECTION('ref_axis',(0.,-0.4226182617407,-0.90630778703665));
#63999=DIRECTION('',(0.,-0.4226182617407,-0.90630778703665));
#64000=DIRECTION('center_axis',(0.,-0.90630778703665,0.4226182617407));
#64001=DIRECTION('ref_axis',(0.,-0.4226182617407,-0.90630778703665));
#64002=DIRECTION('',(0.,-0.4226182617407,-0.90630778703665));
#64003=DIRECTION('center_axis',(1.,0.,0.));
#64004=DIRECTION('ref_axis',(0.,-0.5,-0.866025403784438));
#64005=DIRECTION('center_axis',(1.,0.,0.));
#64006=DIRECTION('ref_axis',(0.,-0.5,-0.866025403784438));
#64007=DIRECTION('center_axis',(1.,0.,0.));
#64008=DIRECTION('ref_axis',(0.,1.,0.));
#64009=DIRECTION('center_axis',(0.,-0.819152044288992,0.573576436351046));
#64010=DIRECTION('ref_axis',(0.,-0.573576436351046,-0.819152044288992));
#64011=DIRECTION('',(0.,-0.573576436351046,-0.819152044288992));
#64012=DIRECTION('center_axis',(0.,-0.819152044288992,0.573576436351046));
#64013=DIRECTION('ref_axis',(0.,-0.573576436351046,-0.819152044288992));
#64014=DIRECTION('',(0.,-0.573576436351046,-0.819152044288992));
#64015=DIRECTION('center_axis',(1.,0.,0.));
#64016=DIRECTION('ref_axis',(0.,-0.64278760968654,-0.766044443118978));
#64017=DIRECTION('center_axis',(1.,0.,0.));
#64018=DIRECTION('ref_axis',(0.,-0.64278760968654,-0.766044443118978));
#64019=DIRECTION('center_axis',(1.,0.,0.));
#64020=DIRECTION('ref_axis',(0.,1.,0.));
#64021=DIRECTION('center_axis',(0.,-0.707106781186547,0.707106781186548));
#64022=DIRECTION('ref_axis',(0.,-0.707106781186548,-0.707106781186547));
#64023=DIRECTION('',(0.,-0.707106781186548,-0.707106781186547));
#64024=DIRECTION('center_axis',(0.,-0.707106781186547,0.707106781186548));
#64025=DIRECTION('ref_axis',(0.,-0.707106781186548,-0.707106781186547));
#64026=DIRECTION('',(0.,-0.707106781186548,-0.707106781186547));
#64027=DIRECTION('center_axis',(1.,0.,0.));
#64028=DIRECTION('ref_axis',(0.,-0.766044443118978,-0.642787609686539));
#64029=DIRECTION('center_axis',(1.,0.,0.));
#64030=DIRECTION('ref_axis',(0.,-0.766044443118978,-0.642787609686539));
#64031=DIRECTION('center_axis',(1.,0.,0.));
#64032=DIRECTION('ref_axis',(0.,1.,0.));
#64033=DIRECTION('center_axis',(0.,-0.573576436351046,0.819152044288992));
#64034=DIRECTION('ref_axis',(0.,-0.819152044288992,-0.573576436351046));
#64035=DIRECTION('',(0.,-0.819152044288992,-0.573576436351046));
#64036=DIRECTION('center_axis',(0.,-0.573576436351046,0.819152044288992));
#64037=DIRECTION('ref_axis',(0.,-0.819152044288992,-0.573576436351046));
#64038=DIRECTION('',(0.,-0.819152044288992,-0.573576436351046));
#64039=DIRECTION('center_axis',(1.,0.,0.));
#64040=DIRECTION('ref_axis',(0.,-0.866025403784439,-0.5));
#64041=DIRECTION('center_axis',(1.,0.,0.));
#64042=DIRECTION('ref_axis',(0.,-0.866025403784439,-0.5));
#64043=DIRECTION('center_axis',(1.,0.,0.));
#64044=DIRECTION('ref_axis',(0.,1.,0.));
#64045=DIRECTION('center_axis',(0.,-0.422618261740699,0.90630778703665));
#64046=DIRECTION('ref_axis',(0.,-0.90630778703665,-0.422618261740699));
#64047=DIRECTION('',(0.,-0.90630778703665,-0.422618261740699));
#64048=DIRECTION('center_axis',(0.,-0.422618261740699,0.90630778703665));
#64049=DIRECTION('ref_axis',(0.,-0.90630778703665,-0.422618261740699));
#64050=DIRECTION('',(0.,-0.90630778703665,-0.422618261740699));
#64051=DIRECTION('center_axis',(1.,0.,0.));
#64052=DIRECTION('ref_axis',(0.,-0.939692620785909,-0.342020143325668));
#64053=DIRECTION('center_axis',(1.,0.,0.));
#64054=DIRECTION('ref_axis',(0.,-0.939692620785909,-0.342020143325668));
#64055=DIRECTION('center_axis',(1.,0.,0.));
#64056=DIRECTION('ref_axis',(0.,1.,0.));
#64057=DIRECTION('center_axis',(0.,-0.25881904510252,0.965925826289068));
#64058=DIRECTION('ref_axis',(0.,-0.965925826289068,-0.25881904510252));
#64059=DIRECTION('',(0.,-0.965925826289068,-0.25881904510252));
#64060=DIRECTION('center_axis',(0.,-0.25881904510252,0.965925826289068));
#64061=DIRECTION('ref_axis',(0.,-0.965925826289068,-0.25881904510252));
#64062=DIRECTION('',(0.,-0.965925826289068,-0.25881904510252));
#64063=DIRECTION('center_axis',(1.,0.,0.));
#64064=DIRECTION('ref_axis',(0.,-0.984807753012208,-0.17364817766693));
#64065=DIRECTION('center_axis',(1.,0.,0.));
#64066=DIRECTION('ref_axis',(0.,-0.984807753012208,-0.17364817766693));
#64067=DIRECTION('center_axis',(1.,0.,0.));
#64068=DIRECTION('ref_axis',(0.,1.,0.));
#64069=DIRECTION('center_axis',(0.,-0.0871557427476581,0.996194698091746));
#64070=DIRECTION('ref_axis',(0.,-0.996194698091746,-0.0871557427476581));
#64071=DIRECTION('',(0.,-0.996194698091746,-0.0871557427476581));
#64072=DIRECTION('center_axis',(0.,-0.0871557427476581,0.996194698091746));
#64073=DIRECTION('ref_axis',(0.,-0.996194698091746,-0.0871557427476581));
#64074=DIRECTION('',(0.,-0.996194698091746,-0.0871557427476581));
#64075=DIRECTION('center_axis',(1.,0.,0.));
#64076=DIRECTION('ref_axis',(0.,-1.,1.83697019872103E-16));
#64077=DIRECTION('center_axis',(1.,0.,0.));
#64078=DIRECTION('ref_axis',(0.,-1.,1.83697019872103E-16));
#64079=DIRECTION('center_axis',(1.,0.,0.));
#64080=DIRECTION('ref_axis',(0.,1.,0.));
#64081=DIRECTION('center_axis',(0.,0.0871557427476581,0.996194698091746));
#64082=DIRECTION('ref_axis',(0.,-0.996194698091746,0.0871557427476581));
#64083=DIRECTION('',(0.,-0.996194698091746,0.0871557427476581));
#64084=DIRECTION('center_axis',(0.,0.0871557427476581,0.996194698091746));
#64085=DIRECTION('ref_axis',(0.,-0.996194698091746,0.0871557427476581));
#64086=DIRECTION('',(0.,-0.996194698091746,0.0871557427476581));
#64087=DIRECTION('center_axis',(1.,0.,0.));
#64088=DIRECTION('ref_axis',(0.,-0.984807753012208,0.17364817766693));
#64089=DIRECTION('center_axis',(1.,0.,0.));
#64090=DIRECTION('ref_axis',(0.,-0.984807753012208,0.17364817766693));
#64091=DIRECTION('center_axis',(1.,0.,0.));
#64092=DIRECTION('ref_axis',(0.,1.,0.));
#64093=DIRECTION('center_axis',(0.,0.258819045102521,0.965925826289068));
#64094=DIRECTION('ref_axis',(0.,-0.965925826289068,0.258819045102521));
#64095=DIRECTION('',(0.,-0.965925826289068,0.258819045102521));
#64096=DIRECTION('center_axis',(0.,0.258819045102521,0.965925826289068));
#64097=DIRECTION('ref_axis',(0.,-0.965925826289068,0.258819045102521));
#64098=DIRECTION('',(0.,-0.965925826289068,0.258819045102521));
#64099=DIRECTION('center_axis',(1.,0.,0.));
#64100=DIRECTION('ref_axis',(0.,-0.939692620785908,0.342020143325669));
#64101=DIRECTION('center_axis',(1.,0.,0.));
#64102=DIRECTION('ref_axis',(0.,-0.939692620785908,0.342020143325669));
#64103=DIRECTION('center_axis',(1.,0.,0.));
#64104=DIRECTION('ref_axis',(0.,1.,0.));
#64105=DIRECTION('center_axis',(0.,0.573576436351046,0.819152044288992));
#64106=DIRECTION('ref_axis',(0.,-0.819152044288992,0.573576436351046));
#64107=DIRECTION('',(0.,-0.819152044288992,0.573576436351046));
#64108=DIRECTION('center_axis',(0.,0.573576436351046,0.819152044288992));
#64109=DIRECTION('ref_axis',(0.,-0.819152044288992,0.573576436351046));
#64110=DIRECTION('',(0.,-0.819152044288992,0.573576436351046));
#64111=DIRECTION('center_axis',(1.,0.,0.));
#64112=DIRECTION('ref_axis',(0.,-0.766044443118978,0.642787609686539));
#64113=DIRECTION('center_axis',(1.,0.,0.));
#64114=DIRECTION('ref_axis',(0.,-0.766044443118978,0.642787609686539));
#64115=DIRECTION('center_axis',(1.,0.,0.));
#64116=DIRECTION('ref_axis',(0.,1.,0.));
#64117=DIRECTION('center_axis',(0.,0.707106781186547,0.707106781186548));
#64118=DIRECTION('ref_axis',(0.,-0.707106781186548,0.707106781186547));
#64119=DIRECTION('',(0.,-0.707106781186548,0.707106781186547));
#64120=DIRECTION('center_axis',(0.,0.707106781186547,0.707106781186548));
#64121=DIRECTION('ref_axis',(0.,-0.707106781186548,0.707106781186547));
#64122=DIRECTION('',(0.,-0.707106781186548,0.707106781186547));
#64123=DIRECTION('center_axis',(1.,0.,0.));
#64124=DIRECTION('ref_axis',(0.,-0.642787609686539,0.766044443118978));
#64125=DIRECTION('center_axis',(1.,0.,0.));
#64126=DIRECTION('ref_axis',(0.,-0.642787609686539,0.766044443118978));
#64127=DIRECTION('center_axis',(1.,0.,0.));
#64128=DIRECTION('ref_axis',(0.,1.,0.));
#64129=DIRECTION('center_axis',(0.,0.819152044288992,0.573576436351046));
#64130=DIRECTION('ref_axis',(0.,-0.573576436351046,0.819152044288992));
#64131=DIRECTION('',(0.,-0.573576436351046,0.819152044288992));
#64132=DIRECTION('center_axis',(0.,0.819152044288992,0.573576436351046));
#64133=DIRECTION('ref_axis',(0.,-0.573576436351046,0.819152044288992));
#64134=DIRECTION('',(0.,-0.573576436351046,0.819152044288992));
#64135=DIRECTION('center_axis',(1.,0.,0.));
#64136=DIRECTION('ref_axis',(0.,-0.5,0.866025403784439));
#64137=DIRECTION('center_axis',(1.,0.,0.));
#64138=DIRECTION('ref_axis',(0.,-0.5,0.866025403784439));
#64139=DIRECTION('center_axis',(1.,0.,0.));
#64140=DIRECTION('ref_axis',(0.,1.,0.));
#64141=DIRECTION('center_axis',(0.,0.90630778703665,0.422618261740699));
#64142=DIRECTION('ref_axis',(0.,-0.422618261740699,0.90630778703665));
#64143=DIRECTION('',(0.,-0.422618261740699,0.90630778703665));
#64144=DIRECTION('center_axis',(0.,0.90630778703665,0.422618261740699));
#64145=DIRECTION('ref_axis',(0.,-0.422618261740699,0.90630778703665));
#64146=DIRECTION('',(0.,-0.422618261740699,0.90630778703665));
#64147=DIRECTION('center_axis',(1.,0.,0.));
#64148=DIRECTION('ref_axis',(0.,-0.342020143325669,0.939692620785909));
#64149=DIRECTION('center_axis',(1.,0.,0.));
#64150=DIRECTION('ref_axis',(0.,-0.342020143325669,0.939692620785909));
#64151=DIRECTION('center_axis',(1.,0.,0.));
#64152=DIRECTION('ref_axis',(0.,1.,0.));
#64153=DIRECTION('center_axis',(0.,0.965925826289068,0.258819045102521));
#64154=DIRECTION('ref_axis',(0.,-0.25881904510252,0.965925826289068));
#64155=DIRECTION('',(0.,-0.25881904510252,0.965925826289068));
#64156=DIRECTION('center_axis',(0.,0.965925826289068,0.258819045102521));
#64157=DIRECTION('ref_axis',(0.,-0.25881904510252,0.965925826289068));
#64158=DIRECTION('',(0.,-0.25881904510252,0.965925826289068));
#64159=DIRECTION('center_axis',(1.,0.,0.));
#64160=DIRECTION('ref_axis',(0.,-0.17364817766693,0.984807753012208));
#64161=DIRECTION('center_axis',(1.,0.,0.));
#64162=DIRECTION('ref_axis',(0.,-0.17364817766693,0.984807753012208));
#64163=DIRECTION('center_axis',(1.,0.,0.));
#64164=DIRECTION('ref_axis',(0.,1.,0.));
#64165=DIRECTION('center_axis',(0.,0.996194698091746,0.0871557427476581));
#64166=DIRECTION('ref_axis',(0.,-0.0871557427476581,0.996194698091746));
#64167=DIRECTION('',(0.,-0.0871557427476581,0.996194698091746));
#64168=DIRECTION('center_axis',(0.,0.996194698091746,0.0871557427476581));
#64169=DIRECTION('ref_axis',(0.,-0.0871557427476581,0.996194698091746));
#64170=DIRECTION('',(0.,-0.0871557427476581,0.996194698091746));
#64171=DIRECTION('center_axis',(1.,0.,0.));
#64172=DIRECTION('ref_axis',(0.,1.22464679914735E-16,1.));
#64173=DIRECTION('center_axis',(1.,0.,0.));
#64174=DIRECTION('ref_axis',(0.,1.22464679914735E-16,1.));
#64175=DIRECTION('center_axis',(1.,0.,0.));
#64176=DIRECTION('ref_axis',(0.,-1.,-1.22464679914735E-16));
#64177=DIRECTION('center_axis',(0.,0.996194698091746,-0.0871557427476584));
#64178=DIRECTION('ref_axis',(0.,0.0871557427476584,0.996194698091746));
#64179=DIRECTION('',(0.,0.0871557427476584,0.996194698091746));
#64180=DIRECTION('center_axis',(0.,0.996194698091746,-0.0871557427476584));
#64181=DIRECTION('ref_axis',(0.,0.0871557427476584,0.996194698091746));
#64182=DIRECTION('',(0.,0.0871557427476584,0.996194698091746));
#64183=DIRECTION('center_axis',(1.,0.,0.));
#64184=DIRECTION('ref_axis',(0.,0.173648177666931,0.984807753012208));
#64185=DIRECTION('center_axis',(1.,0.,0.));
#64186=DIRECTION('ref_axis',(0.,0.173648177666931,0.984807753012208));
#64187=DIRECTION('center_axis',(1.,0.,0.));
#64188=DIRECTION('ref_axis',(0.,1.,0.));
#64189=DIRECTION('center_axis',(0.,0.965925826289068,-0.258819045102521));
#64190=DIRECTION('ref_axis',(0.,0.258819045102521,0.965925826289068));
#64191=DIRECTION('',(0.,0.258819045102521,0.965925826289068));
#64192=DIRECTION('center_axis',(0.,0.965925826289068,-0.258819045102521));
#64193=DIRECTION('ref_axis',(0.,0.258819045102521,0.965925826289068));
#64194=DIRECTION('',(0.,0.258819045102521,0.965925826289068));
#64195=DIRECTION('center_axis',(1.,0.,0.));
#64196=DIRECTION('ref_axis',(0.,0.342020143325669,0.939692620785908));
#64197=DIRECTION('center_axis',(1.,0.,0.));
#64198=DIRECTION('ref_axis',(0.,0.342020143325669,0.939692620785908));
#64199=DIRECTION('center_axis',(1.,0.,0.));
#64200=DIRECTION('ref_axis',(0.,1.,0.));
#64201=DIRECTION('center_axis',(0.,0.90630778703665,-0.422618261740699));
#64202=DIRECTION('ref_axis',(0.,0.422618261740699,0.90630778703665));
#64203=DIRECTION('',(0.,0.422618261740699,0.90630778703665));
#64204=DIRECTION('center_axis',(0.,0.90630778703665,-0.422618261740699));
#64205=DIRECTION('ref_axis',(0.,0.422618261740699,0.90630778703665));
#64206=DIRECTION('',(0.,0.422618261740699,0.90630778703665));
#64207=DIRECTION('center_axis',(1.,0.,0.));
#64208=DIRECTION('ref_axis',(0.,0.5,0.866025403784439));
#64209=DIRECTION('center_axis',(1.,0.,0.));
#64210=DIRECTION('ref_axis',(0.,0.5,0.866025403784439));
#64211=DIRECTION('center_axis',(1.,0.,0.));
#64212=DIRECTION('ref_axis',(0.,1.,0.));
#64213=DIRECTION('center_axis',(0.,0.819152044288992,-0.573576436351046));
#64214=DIRECTION('ref_axis',(0.,0.573576436351046,0.819152044288992));
#64215=DIRECTION('',(0.,0.573576436351046,0.819152044288992));
#64216=DIRECTION('center_axis',(0.,0.819152044288992,-0.573576436351046));
#64217=DIRECTION('ref_axis',(0.,0.573576436351046,0.819152044288992));
#64218=DIRECTION('',(0.,0.573576436351046,0.819152044288992));
#64219=DIRECTION('center_axis',(1.,0.,0.));
#64220=DIRECTION('ref_axis',(0.,0.642787609686539,0.766044443118978));
#64221=DIRECTION('center_axis',(1.,0.,0.));
#64222=DIRECTION('ref_axis',(0.,0.642787609686539,0.766044443118978));
#64223=DIRECTION('center_axis',(1.,0.,0.));
#64224=DIRECTION('ref_axis',(0.,1.,0.));
#64225=DIRECTION('center_axis',(0.,0.707106781186548,-0.707106781186547));
#64226=DIRECTION('ref_axis',(0.,0.707106781186547,0.707106781186548));
#64227=DIRECTION('',(0.,0.707106781186547,0.707106781186548));
#64228=DIRECTION('center_axis',(0.,0.707106781186548,-0.707106781186547));
#64229=DIRECTION('ref_axis',(0.,0.707106781186547,0.707106781186548));
#64230=DIRECTION('',(0.,0.707106781186547,0.707106781186548));
#64231=DIRECTION('center_axis',(1.,0.,0.));
#64232=DIRECTION('ref_axis',(0.,0.766044443118978,0.642787609686539));
#64233=DIRECTION('center_axis',(1.,0.,0.));
#64234=DIRECTION('ref_axis',(0.,0.766044443118978,0.642787609686539));
#64235=DIRECTION('center_axis',(1.,0.,0.));
#64236=DIRECTION('ref_axis',(0.,1.,0.));
#64237=DIRECTION('center_axis',(0.,0.422618261740699,-0.90630778703665));
#64238=DIRECTION('ref_axis',(0.,0.90630778703665,0.422618261740699));
#64239=DIRECTION('',(0.,0.90630778703665,0.422618261740699));
#64240=DIRECTION('center_axis',(0.,0.422618261740699,-0.90630778703665));
#64241=DIRECTION('ref_axis',(0.,0.90630778703665,0.422618261740699));
#64242=DIRECTION('',(0.,0.90630778703665,0.422618261740699));
#64243=DIRECTION('center_axis',(1.,0.,0.));
#64244=DIRECTION('ref_axis',(0.,0.939692620785908,0.342020143325669));
#64245=DIRECTION('center_axis',(1.,0.,0.));
#64246=DIRECTION('ref_axis',(0.,0.939692620785908,0.342020143325669));
#64247=DIRECTION('center_axis',(1.,0.,0.));
#64248=DIRECTION('ref_axis',(0.,1.,0.));
#64249=DIRECTION('center_axis',(0.,0.258819045102521,-0.965925826289068));
#64250=DIRECTION('ref_axis',(0.,0.965925826289068,0.258819045102521));
#64251=DIRECTION('',(0.,0.965925826289068,0.258819045102521));
#64252=DIRECTION('center_axis',(0.,0.258819045102521,-0.965925826289068));
#64253=DIRECTION('ref_axis',(0.,0.965925826289068,0.258819045102521));
#64254=DIRECTION('',(0.,0.965925826289068,0.258819045102521));
#64255=DIRECTION('center_axis',(1.,0.,0.));
#64256=DIRECTION('ref_axis',(0.,0.984807753012208,0.17364817766693));
#64257=DIRECTION('center_axis',(1.,0.,0.));
#64258=DIRECTION('ref_axis',(0.,0.984807753012208,0.17364817766693));
#64259=DIRECTION('center_axis',(1.,0.,0.));
#64260=DIRECTION('ref_axis',(0.,1.,0.));
#64261=DIRECTION('center_axis',(0.,0.0871557427476582,-0.996194698091746));
#64262=DIRECTION('ref_axis',(0.,0.996194698091746,0.0871557427476582));
#64263=DIRECTION('',(0.,0.996194698091746,0.0871557427476582));
#64264=DIRECTION('center_axis',(0.,0.0871557427476582,-0.996194698091746));
#64265=DIRECTION('ref_axis',(0.,0.996194698091746,0.0871557427476582));
#64266=DIRECTION('',(0.,0.996194698091746,0.0871557427476582));
#64267=DIRECTION('center_axis',(1.,0.,0.));
#64268=DIRECTION('ref_axis',(0.,1.,-6.12323399573677E-17));
#64269=DIRECTION('center_axis',(1.,0.,0.));
#64270=DIRECTION('ref_axis',(0.,1.,-6.12323399573677E-17));
#64271=DIRECTION('center_axis',(1.,0.,0.));
#64272=DIRECTION('ref_axis',(0.,1.,0.));
#64273=DIRECTION('center_axis',(0.,-0.0871557427476582,-0.996194698091746));
#64274=DIRECTION('ref_axis',(0.,0.996194698091746,-0.0871557427476582));
#64275=DIRECTION('',(0.,0.996194698091746,-0.0871557427476582));
#64276=DIRECTION('center_axis',(0.,-0.0871557427476582,-0.996194698091746));
#64277=DIRECTION('ref_axis',(0.,0.996194698091746,-0.0871557427476582));
#64278=DIRECTION('',(0.,0.996194698091746,-0.0871557427476582));
#64279=DIRECTION('center_axis',(1.,0.,0.));
#64280=DIRECTION('ref_axis',(0.,0.984807753012208,-0.17364817766693));
#64281=DIRECTION('center_axis',(1.,0.,0.));
#64282=DIRECTION('ref_axis',(0.,0.984807753012208,-0.17364817766693));
#64283=DIRECTION('center_axis',(1.,0.,0.));
#64284=DIRECTION('ref_axis',(0.,1.,0.));
#64285=DIRECTION('center_axis',(0.,-0.258819045102521,-0.965925826289068));
#64286=DIRECTION('ref_axis',(0.,0.965925826289068,-0.258819045102521));
#64287=DIRECTION('',(0.,0.965925826289068,-0.258819045102521));
#64288=DIRECTION('center_axis',(0.,-0.258819045102521,-0.965925826289068));
#64289=DIRECTION('ref_axis',(0.,0.965925826289068,-0.258819045102521));
#64290=DIRECTION('',(0.,0.965925826289068,-0.258819045102521));
#64291=DIRECTION('center_axis',(1.,0.,0.));
#64292=DIRECTION('ref_axis',(0.,0.939692620785908,-0.342020143325669));
#64293=DIRECTION('center_axis',(1.,0.,0.));
#64294=DIRECTION('ref_axis',(0.,0.939692620785908,-0.342020143325669));
#64295=DIRECTION('center_axis',(1.,0.,0.));
#64296=DIRECTION('ref_axis',(0.,1.,0.));
#64297=DIRECTION('center_axis',(0.,-0.422618261740699,-0.90630778703665));
#64298=DIRECTION('ref_axis',(0.,0.90630778703665,-0.422618261740699));
#64299=DIRECTION('',(0.,0.90630778703665,-0.422618261740699));
#64300=DIRECTION('center_axis',(0.,-0.422618261740699,-0.90630778703665));
#64301=DIRECTION('ref_axis',(0.,0.90630778703665,-0.422618261740699));
#64302=DIRECTION('',(0.,0.90630778703665,-0.422618261740699));
#64303=DIRECTION('center_axis',(1.,0.,0.));
#64304=DIRECTION('ref_axis',(0.,0.866025403784439,-0.5));
#64305=DIRECTION('center_axis',(1.,0.,0.));
#64306=DIRECTION('ref_axis',(0.,0.866025403784439,-0.5));
#64307=DIRECTION('center_axis',(1.,0.,0.));
#64308=DIRECTION('ref_axis',(0.,1.,0.));
#64309=DIRECTION('center_axis',(0.,-0.573576436351046,-0.819152044288992));
#64310=DIRECTION('ref_axis',(0.,0.819152044288992,-0.573576436351046));
#64311=DIRECTION('',(0.,0.819152044288992,-0.573576436351046));
#64312=DIRECTION('center_axis',(0.,-0.573576436351046,-0.819152044288992));
#64313=DIRECTION('ref_axis',(0.,0.819152044288992,-0.573576436351046));
#64314=DIRECTION('',(0.,0.819152044288992,-0.573576436351046));
#64315=DIRECTION('center_axis',(1.,0.,0.));
#64316=DIRECTION('ref_axis',(0.,0.766044443118978,-0.642787609686539));
#64317=DIRECTION('center_axis',(1.,0.,0.));
#64318=DIRECTION('ref_axis',(0.,0.766044443118978,-0.642787609686539));
#64319=DIRECTION('center_axis',(1.,0.,0.));
#64320=DIRECTION('ref_axis',(0.,1.,0.));
#64321=DIRECTION('center_axis',(0.,-0.707106781186547,-0.707106781186548));
#64322=DIRECTION('ref_axis',(0.,0.707106781186548,-0.707106781186547));
#64323=DIRECTION('',(0.,0.707106781186548,-0.707106781186547));
#64324=DIRECTION('center_axis',(0.,-0.707106781186547,-0.707106781186548));
#64325=DIRECTION('ref_axis',(0.,0.707106781186548,-0.707106781186547));
#64326=DIRECTION('',(0.,0.707106781186548,-0.707106781186547));
#64327=DIRECTION('center_axis',(1.,0.,0.));
#64328=DIRECTION('ref_axis',(0.,0.642787609686539,-0.766044443118978));
#64329=DIRECTION('center_axis',(1.,0.,0.));
#64330=DIRECTION('ref_axis',(0.,0.642787609686539,-0.766044443118978));
#64331=DIRECTION('center_axis',(1.,0.,0.));
#64332=DIRECTION('ref_axis',(0.,1.,0.));
#64333=DIRECTION('center_axis',(0.,-0.819152044288992,-0.573576436351046));
#64334=DIRECTION('ref_axis',(0.,0.573576436351046,-0.819152044288992));
#64335=DIRECTION('',(0.,0.573576436351046,-0.819152044288992));
#64336=DIRECTION('center_axis',(0.,-0.819152044288992,-0.573576436351046));
#64337=DIRECTION('ref_axis',(0.,0.573576436351046,-0.819152044288992));
#64338=DIRECTION('',(0.,0.573576436351046,-0.819152044288992));
#64339=DIRECTION('center_axis',(1.,0.,0.));
#64340=DIRECTION('ref_axis',(0.,0.5,-0.866025403784439));
#64341=DIRECTION('center_axis',(1.,0.,0.));
#64342=DIRECTION('ref_axis',(0.,0.5,-0.866025403784439));
#64343=DIRECTION('center_axis',(1.,0.,0.));
#64344=DIRECTION('ref_axis',(0.,1.,0.));
#64345=DIRECTION('center_axis',(0.,-0.90630778703665,-0.422618261740699));
#64346=DIRECTION('ref_axis',(0.,0.422618261740699,-0.90630778703665));
#64347=DIRECTION('',(0.,0.422618261740699,-0.90630778703665));
#64348=DIRECTION('center_axis',(0.,-0.90630778703665,-0.422618261740699));
#64349=DIRECTION('ref_axis',(0.,0.422618261740699,-0.90630778703665));
#64350=DIRECTION('',(0.,0.422618261740699,-0.90630778703665));
#64351=DIRECTION('center_axis',(1.,0.,0.));
#64352=DIRECTION('ref_axis',(0.,0.342020143325669,-0.939692620785908));
#64353=DIRECTION('center_axis',(1.,0.,0.));
#64354=DIRECTION('ref_axis',(0.,0.342020143325669,-0.939692620785908));
#64355=DIRECTION('center_axis',(1.,0.,0.));
#64356=DIRECTION('ref_axis',(0.,1.,0.));
#64357=DIRECTION('center_axis',(0.,-0.965925826289068,-0.258819045102521));
#64358=DIRECTION('ref_axis',(0.,0.258819045102521,-0.965925826289068));
#64359=DIRECTION('',(0.,0.258819045102521,-0.965925826289068));
#64360=DIRECTION('center_axis',(0.,-0.965925826289068,-0.258819045102521));
#64361=DIRECTION('ref_axis',(0.,0.258819045102521,-0.965925826289068));
#64362=DIRECTION('',(0.,0.258819045102521,-0.965925826289068));
#64363=DIRECTION('center_axis',(1.,0.,0.));
#64364=DIRECTION('ref_axis',(0.,0.17364817766693,-0.984807753012208));
#64365=DIRECTION('center_axis',(1.,0.,0.));
#64366=DIRECTION('ref_axis',(0.,0.17364817766693,-0.984807753012208));
#64367=DIRECTION('center_axis',(1.,0.,0.));
#64368=DIRECTION('ref_axis',(0.,0.,-1.));
#64369=DIRECTION('center_axis',(1.,0.,0.));
#64370=DIRECTION('ref_axis',(0.,-1.,1.83697019872103E-16));
#64371=DIRECTION('center_axis',(0.,-1.,-1.22464679914735E-16));
#64372=DIRECTION('ref_axis',(0.,-1.22464679914735E-16,1.));
#64373=DIRECTION('center_axis',(-1.,0.,0.));
#64374=DIRECTION('ref_axis',(0.,-1.,1.83697019872103E-16));
#64375=DIRECTION('center_axis',(1.,0.,0.));
#64376=DIRECTION('ref_axis',(0.,-1.,1.83697019872103E-16));
#64377=DIRECTION('center_axis',(1.,0.,0.));
#64378=DIRECTION('ref_axis',(0.,0.,-1.));
#64379=DIRECTION('center_axis',(1.,0.,0.));
#64380=DIRECTION('ref_axis',(0.,-1.,1.83697019872103E-16));
#64381=DIRECTION('center_axis',(1.,0.,0.));
#64382=DIRECTION('ref_axis',(0.,1.,0.));
#64383=DIRECTION('center_axis',(1.,0.,0.));
#64384=DIRECTION('ref_axis',(0.,0.,-1.));
#64385=DIRECTION('',(-1.,0.,0.));
#64386=DIRECTION('center_axis',(1.,0.,0.));
#64387=DIRECTION('ref_axis',(0.,0.,-1.));
#64388=DIRECTION('center_axis',(1.,0.,0.));
#64389=DIRECTION('ref_axis',(0.,-1.,1.83697019872103E-16));
#64390=DIRECTION('center_axis',(0.,-1.,-1.22464679914735E-16));
#64391=DIRECTION('ref_axis',(0.,-1.22464679914735E-16,1.));
#64392=DIRECTION('center_axis',(-1.,0.,0.));
#64393=DIRECTION('ref_axis',(0.,-1.,1.83697019872103E-16));
#64394=DIRECTION('center_axis',(-1.,0.,0.));
#64395=DIRECTION('ref_axis',(0.,-1.,1.83697019872103E-16));
#64396=DIRECTION('center_axis',(-1.,0.,0.));
#64397=DIRECTION('ref_axis',(0.,0.,1.));
#64398=DIRECTION('center_axis',(-1.,0.,0.));
#64399=DIRECTION('ref_axis',(0.,-1.,1.83697019872103E-16));
#64400=DIRECTION('center_axis',(1.,0.,0.));
#64401=DIRECTION('ref_axis',(0.,1.,0.));
#64402=DIRECTION('',(-1.,0.,0.));
#64403=DIRECTION('center_axis',(1.,0.,0.));
#64404=DIRECTION('ref_axis',(0.,0.,-1.));
#64405=DIRECTION('center_axis',(0.,-1.,-1.22464679914735E-16));
#64406=DIRECTION('ref_axis',(0.,-1.22464679914735E-16,1.));
#64407=DIRECTION('center_axis',(-1.,0.,0.));
#64408=DIRECTION('ref_axis',(0.,-1.,1.83697019872103E-16));
#64409=DIRECTION('center_axis',(-1.,0.,0.));
#64410=DIRECTION('ref_axis',(0.,-1.,1.83697019872103E-16));
#64411=DIRECTION('center_axis',(1.,0.,0.));
#64412=DIRECTION('ref_axis',(0.,1.,0.));
#64413=DIRECTION('center_axis',(1.,0.,0.));
#64414=DIRECTION('ref_axis',(0.,0.,-1.));
#64415=DIRECTION('',(-1.,0.,0.));
#64416=DIRECTION('center_axis',(1.,0.,0.));
#64417=DIRECTION('ref_axis',(0.,0.,-1.));
#64418=DIRECTION('center_axis',(1.,0.,0.));
#64419=DIRECTION('ref_axis',(0.,-1.,1.83697019872103E-16));
#64420=DIRECTION('center_axis',(0.,-1.,-1.22464679914735E-16));
#64421=DIRECTION('ref_axis',(0.,-1.22464679914735E-16,1.));
#64422=DIRECTION('center_axis',(1.,0.,0.));
#64423=DIRECTION('ref_axis',(0.,-1.,1.83697019872103E-16));
#64424=DIRECTION('center_axis',(1.,0.,0.));
#64425=DIRECTION('ref_axis',(0.,1.,0.));
#64426=DIRECTION('',(-1.,0.,0.));
#64427=DIRECTION('center_axis',(1.,0.,0.));
#64428=DIRECTION('ref_axis',(0.,0.,-1.));
#64429=DIRECTION('center_axis',(1.,0.,0.));
#64430=DIRECTION('ref_axis',(0.,1.,0.));
#64431=DIRECTION('center_axis',(1.,0.,0.));
#64432=DIRECTION('ref_axis',(0.,0.,-1.));
#64433=DIRECTION('',(-1.,0.,0.));
#64434=DIRECTION('center_axis',(1.,0.,0.));
#64435=DIRECTION('ref_axis',(0.,0.,-1.));
#64436=DIRECTION('center_axis',(-1.,0.,0.));
#64437=DIRECTION('ref_axis',(0.,1.,0.));
#64438=DIRECTION('',(-0.707106781186547,-0.707106781186548,-8.65956056235494E-17));
#64439=DIRECTION('center_axis',(1.,0.,0.));
#64440=DIRECTION('ref_axis',(0.,0.,-1.));
#64441=DIRECTION('center_axis',(-1.,0.,0.));
#64442=DIRECTION('ref_axis',(0.,0.,1.));
#64443=DIRECTION('center_axis',(1.,0.,0.));
#64444=DIRECTION('ref_axis',(0.,0.,-1.));
#64445=DIRECTION('center_axis',(1.,0.,0.));
#64446=DIRECTION('ref_axis',(0.,0.,-1.));
#64447=DIRECTION('center_axis',(1.,0.,0.));
#64448=DIRECTION('ref_axis',(0.,0.,-1.));
#64449=DIRECTION('center_axis',(1.,0.,0.));
#64450=DIRECTION('ref_axis',(0.,1.,0.));
#64451=DIRECTION('',(-0.707106781186548,0.707106781186548,8.65956056235493E-17));
#64452=DIRECTION('axis',(0.,0.,1.));
#64453=DIRECTION('refdir',(1.,0.,0.));
#64454=DIRECTION('center_axis',(1.,0.,0.));
#64455=DIRECTION('ref_axis',(0.,0.,-1.));
#64456=DIRECTION('center_axis',(1.,0.,0.));
#64457=DIRECTION('ref_axis',(0.,0.,-1.));
#64458=DIRECTION('',(-0.70710678118655,8.6595605623549E-17,-0.707106781186545));
#64459=DIRECTION('center_axis',(-1.,0.,0.));
#64460=DIRECTION('ref_axis',(0.,0.,-1.));
#64461=DIRECTION('center_axis',(1.,0.,0.));
#64462=DIRECTION('ref_axis',(0.,0.,-1.));
#64463=DIRECTION('center_axis',(1.,0.,0.));
#64464=DIRECTION('ref_axis',(0.,0.,-1.));
#64465=DIRECTION('center_axis',(1.,0.,0.));
#64466=DIRECTION('ref_axis',(0.,0.,-1.));
#64467=DIRECTION('center_axis',(-1.,0.,0.));
#64468=DIRECTION('ref_axis',(0.,0.,-1.));
#64469=DIRECTION('center_axis',(-1.,0.,0.));
#64470=DIRECTION('ref_axis',(0.,0.,-1.));
#64471=DIRECTION('center_axis',(-1.,0.,0.));
#64472=DIRECTION('ref_axis',(0.,0.,-1.));
#64473=DIRECTION('center_axis',(-1.,0.,0.));
#64474=DIRECTION('ref_axis',(0.,0.,-1.));
#64475=DIRECTION('center_axis',(1.,0.,0.));
#64476=DIRECTION('ref_axis',(0.,-1.,1.83697019872103E-16));
#64477=DIRECTION('center_axis',(1.,0.,0.));
#64478=DIRECTION('ref_axis',(0.,0.,-1.));
#64479=DIRECTION('center_axis',(1.,0.,0.));
#64480=DIRECTION('ref_axis',(0.,0.,-1.));
#64481=DIRECTION('',(1.,0.,0.));
#64482=DIRECTION('center_axis',(1.,0.,0.));
#64483=DIRECTION('ref_axis',(0.,0.,-1.));
#64484=DIRECTION('',(-0.70710678118655,8.6595605623549E-17,-0.707106781186545));
#64485=DIRECTION('center_axis',(-1.,0.,0.));
#64486=DIRECTION('ref_axis',(0.,0.,-1.));
#64487=DIRECTION('center_axis',(1.,0.,0.));
#64488=DIRECTION('ref_axis',(0.,0.,-1.));
#64489=DIRECTION('center_axis',(1.,0.,0.));
#64490=DIRECTION('ref_axis',(0.,0.,-1.));
#64491=DIRECTION('',(1.,0.,0.));
#64492=DIRECTION('center_axis',(1.,0.,0.));
#64493=DIRECTION('ref_axis',(0.,0.,-1.));
#64494=DIRECTION('center_axis',(1.,0.,0.));
#64495=DIRECTION('ref_axis',(0.,0.,-1.));
#64496=DIRECTION('',(1.,0.,0.));
#64497=DIRECTION('center_axis',(-1.,0.,0.));
#64498=DIRECTION('ref_axis',(0.,0.,-1.));
#64499=DIRECTION('center_axis',(1.,0.,0.));
#64500=DIRECTION('ref_axis',(0.,0.,-1.));
#64501=DIRECTION('center_axis',(1.,0.,0.));
#64502=DIRECTION('ref_axis',(0.,0.,-1.));
#64503=DIRECTION('',(1.,0.,0.));
#64504=DIRECTION('center_axis',(-1.,0.,0.));
#64505=DIRECTION('ref_axis',(0.,0.,-1.));
#64506=DIRECTION('center_axis',(1.,0.,0.));
#64507=DIRECTION('ref_axis',(0.,0.,-1.));
#64508=DIRECTION('center_axis',(1.,0.,0.));
#64509=DIRECTION('ref_axis',(0.,0.,-1.));
#64510=DIRECTION('',(1.,0.,0.));
#64511=DIRECTION('center_axis',(-1.,0.,0.));
#64512=DIRECTION('ref_axis',(0.,0.,-1.));
#64513=DIRECTION('center_axis',(1.,0.,0.));
#64514=DIRECTION('ref_axis',(0.,0.,-1.));
#64515=DIRECTION('center_axis',(1.,0.,0.));
#64516=DIRECTION('ref_axis',(0.,0.,-1.));
#64517=DIRECTION('',(1.,0.,0.));
#64518=DIRECTION('center_axis',(-1.,0.,0.));
#64519=DIRECTION('ref_axis',(0.,0.,-1.));
#64520=DIRECTION('center_axis',(1.,0.,0.));
#64521=DIRECTION('ref_axis',(0.,0.,-1.));
#64522=DIRECTION('center_axis',(1.,0.,0.));
#64523=DIRECTION('ref_axis',(0.,0.,-1.));
#64524=DIRECTION('',(1.,0.,0.));
#64525=DIRECTION('center_axis',(1.,0.,0.));
#64526=DIRECTION('ref_axis',(0.,0.,-1.));
#64527=DIRECTION('center_axis',(1.,0.,0.));
#64528=DIRECTION('ref_axis',(0.,0.,-1.));
#64529=DIRECTION('center_axis',(1.,0.,0.));
#64530=DIRECTION('ref_axis',(0.,0.,-1.));
#64531=DIRECTION('',(1.,0.,0.));
#64532=DIRECTION('center_axis',(1.,0.,0.));
#64533=DIRECTION('ref_axis',(0.,0.,-1.));
#64534=DIRECTION('center_axis',(1.,0.,0.));
#64535=DIRECTION('ref_axis',(0.,0.,-1.));
#64536=DIRECTION('center_axis',(1.,0.,0.));
#64537=DIRECTION('ref_axis',(0.,0.,-1.));
#64538=DIRECTION('',(1.,0.,0.));
#64539=DIRECTION('center_axis',(1.,0.,0.));
#64540=DIRECTION('ref_axis',(0.,0.,-1.));
#64541=DIRECTION('center_axis',(1.,0.,0.));
#64542=DIRECTION('ref_axis',(0.,0.,-1.));
#64543=DIRECTION('center_axis',(1.,0.,0.));
#64544=DIRECTION('ref_axis',(0.,0.,-1.));
#64545=DIRECTION('',(1.,0.,0.));
#64546=DIRECTION('center_axis',(1.,0.,0.));
#64547=DIRECTION('ref_axis',(0.,0.,-1.));
#64548=DIRECTION('center_axis',(1.,0.,0.));
#64549=DIRECTION('ref_axis',(0.,1.,0.));
#64550=DIRECTION('',(0.515038074910054,-0.857167300702112,-1.04972719113862E-16));
#64551=DIRECTION('center_axis',(1.,0.,0.));
#64552=DIRECTION('ref_axis',(0.,0.,-1.));
#64553=DIRECTION('center_axis',(1.,0.,0.));
#64554=DIRECTION('ref_axis',(0.,1.,0.));
#64555=DIRECTION('',(1.,0.,0.));
#64556=DIRECTION('center_axis',(1.,0.,0.));
#64557=DIRECTION('ref_axis',(0.,0.,-1.));
#64558=DIRECTION('center_axis',(1.,0.,0.));
#64559=DIRECTION('ref_axis',(0.,1.,0.));
#64560=DIRECTION('',(0.707106781186546,-0.707106781186549,-8.65956056235496E-17));
#64561=DIRECTION('center_axis',(-1.,0.,0.));
#64562=DIRECTION('ref_axis',(0.,1.,0.));
#64563=DIRECTION('center_axis',(1.,0.,0.));
#64564=DIRECTION('ref_axis',(0.,0.,-1.));
#64565=DIRECTION('center_axis',(0.,-1.,-1.22464679914735E-16));
#64566=DIRECTION('ref_axis',(0.,-1.22464679914735E-16,1.));
#64567=DIRECTION('center_axis',(-1.,0.,0.));
#64568=DIRECTION('ref_axis',(0.,-1.,1.83697019872103E-16));
#64569=DIRECTION('center_axis',(-1.,0.,0.));
#64570=DIRECTION('ref_axis',(0.,-1.,1.83697019872103E-16));
#64571=DIRECTION('center_axis',(1.,0.,0.));
#64572=DIRECTION('ref_axis',(0.,1.,0.));
#64573=DIRECTION('center_axis',(1.,0.,0.));
#64574=DIRECTION('ref_axis',(0.,0.,-1.));
#64575=DIRECTION('',(-1.,0.,0.));
#64576=DIRECTION('center_axis',(-1.,0.,0.));
#64577=DIRECTION('ref_axis',(0.,0.,1.));
#64578=DIRECTION('center_axis',(1.,0.,0.));
#64579=DIRECTION('ref_axis',(0.,0.,-1.));
#64580=DIRECTION('center_axis',(1.,0.,0.));
#64581=DIRECTION('ref_axis',(0.,1.,0.));
#64582=DIRECTION('center_axis',(1.,0.,0.));
#64583=DIRECTION('ref_axis',(0.,0.,-1.));
#64584=DIRECTION('',(-0.707106781186547,0.707106781186548,8.65956056235493E-17));
#64585=DIRECTION('center_axis',(1.,0.,0.));
#64586=DIRECTION('ref_axis',(0.,1.,0.));
#64587=DIRECTION('center_axis',(1.,0.,0.));
#64588=DIRECTION('ref_axis',(0.,0.,-1.));
#64589=DIRECTION('',(-1.,0.,0.));
#64590=DIRECTION('center_axis',(-1.,0.,0.));
#64591=DIRECTION('ref_axis',(0.,0.,1.));
#64592=DIRECTION('center_axis',(1.,0.,0.));
#64593=DIRECTION('ref_axis',(0.,0.,-1.));
#64594=DIRECTION('center_axis',(1.,0.,0.));
#64595=DIRECTION('ref_axis',(0.,1.,0.));
#64596=DIRECTION('center_axis',(1.,0.,0.));
#64597=DIRECTION('ref_axis',(0.,0.,-1.));
#64598=DIRECTION('',(-0.707106781186549,0.707106781186546,8.65956056235492E-17));
#64599=DIRECTION('center_axis',(1.,0.,0.));
#64600=DIRECTION('ref_axis',(0.,1.,0.));
#64601=DIRECTION('center_axis',(1.,0.,0.));
#64602=DIRECTION('ref_axis',(0.,0.,-1.));
#64603=DIRECTION('',(-1.,0.,0.));
#64604=DIRECTION('center_axis',(-1.,0.,0.));
#64605=DIRECTION('ref_axis',(0.,1.,0.));
#64606=DIRECTION('',(-0.707106781186548,-0.707106781186547,-8.65956056235492E-17));
#64607=DIRECTION('center_axis',(1.,0.,0.));
#64608=DIRECTION('ref_axis',(0.,0.,-1.));
#64609=DIRECTION('center_axis',(1.,0.,0.));
#64610=DIRECTION('ref_axis',(0.,0.,-1.));
#64611=DIRECTION('center_axis',(1.,0.,0.));
#64612=DIRECTION('ref_axis',(0.,1.,0.));
#64613=DIRECTION('center_axis',(1.,0.,0.));
#64614=DIRECTION('ref_axis',(0.,0.,-1.));
#64615=DIRECTION('',(-1.,0.,0.));
#64616=DIRECTION('center_axis',(-1.,0.,0.));
#64617=DIRECTION('ref_axis',(0.,1.,0.));
#64618=DIRECTION('center_axis',(1.,0.,0.));
#64619=DIRECTION('ref_axis',(0.,0.,-1.));
#64620=DIRECTION('',(-0.707106781186548,-0.707106781186547,-8.65956056235492E-17));
#64621=DIRECTION('center_axis',(1.,0.,0.));
#64622=DIRECTION('ref_axis',(0.,0.,-1.));
#64623=DIRECTION('axis',(0.,0.,1.));
#64624=DIRECTION('refdir',(1.,0.,0.));
#64625=DIRECTION('center_axis',(0.,1.,0.));
#64626=DIRECTION('ref_axis',(1.,0.,0.));
#64627=DIRECTION('',(1.,0.,0.));
#64628=DIRECTION('',(0.,0.,-1.));
#64629=DIRECTION('',(1.,0.,0.));
#64630=DIRECTION('',(0.,0.,-1.));
#64631=DIRECTION('center_axis',(1.,0.,0.));
#64632=DIRECTION('ref_axis',(0.,-1.,0.));
#64633=DIRECTION('',(0.,-1.,0.));
#64634=DIRECTION('',(0.,0.,-1.));
#64635=DIRECTION('',(0.,-1.,0.));
#64636=DIRECTION('center_axis',(0.,-1.,0.));
#64637=DIRECTION('ref_axis',(-1.,0.,0.));
#64638=DIRECTION('',(-1.,0.,0.));
#64639=DIRECTION('',(0.,0.,-1.));
#64640=DIRECTION('',(-1.,0.,0.));
#64641=DIRECTION('center_axis',(1.,0.,0.));
#64642=DIRECTION('ref_axis',(0.,-1.,0.));
#64643=DIRECTION('',(0.,-1.,0.));
#64644=DIRECTION('',(0.,0.,-1.));
#64645=DIRECTION('',(0.,-1.,0.));
#64646=DIRECTION('center_axis',(0.,1.,0.));
#64647=DIRECTION('ref_axis',(1.,0.,0.));
#64648=DIRECTION('',(1.,0.,0.));
#64649=DIRECTION('',(0.,0.,-1.));
#64650=DIRECTION('',(1.,0.,0.));
#64651=DIRECTION('center_axis',(1.,0.,0.));
#64652=DIRECTION('ref_axis',(0.,-1.,0.));
#64653=DIRECTION('',(0.,-1.,0.));
#64654=DIRECTION('',(0.,0.,-1.));
#64655=DIRECTION('',(0.,-1.,0.));
#64656=DIRECTION('center_axis',(0.,-1.,0.));
#64657=DIRECTION('ref_axis',(-1.,0.,0.));
#64658=DIRECTION('',(-1.,0.,0.));
#64659=DIRECTION('',(0.,0.,-1.));
#64660=DIRECTION('',(-1.,0.,0.));
#64661=DIRECTION('center_axis',(1.,0.,0.));
#64662=DIRECTION('ref_axis',(0.,-1.,0.));
#64663=DIRECTION('',(0.,-1.,0.));
#64664=DIRECTION('',(0.,0.,-1.));
#64665=DIRECTION('',(0.,-1.,0.));
#64666=DIRECTION('center_axis',(0.,1.,0.));
#64667=DIRECTION('ref_axis',(1.,0.,0.));
#64668=DIRECTION('',(1.,0.,0.));
#64669=DIRECTION('',(0.,0.,-1.));
#64670=DIRECTION('',(1.,0.,0.));
#64671=DIRECTION('center_axis',(-1.,0.,0.));
#64672=DIRECTION('ref_axis',(0.,1.,0.));
#64673=DIRECTION('',(0.,1.,0.));
#64674=DIRECTION('',(0.,0.,-1.));
#64675=DIRECTION('',(0.,1.,0.));
#64676=DIRECTION('center_axis',(0.,-1.,0.));
#64677=DIRECTION('ref_axis',(-1.,0.,0.));
#64678=DIRECTION('',(-1.,0.,0.));
#64679=DIRECTION('',(0.,0.,-1.));
#64680=DIRECTION('',(-1.,0.,0.));
#64681=DIRECTION('center_axis',(1.,0.,0.));
#64682=DIRECTION('ref_axis',(0.,-1.,0.));
#64683=DIRECTION('',(0.,-1.,0.));
#64684=DIRECTION('',(0.,-1.,0.));
#64685=DIRECTION('center_axis',(0.,0.,-1.));
#64686=DIRECTION('ref_axis',(-1.,0.,0.));
#64687=DIRECTION('center_axis',(0.,1.,0.));
#64688=DIRECTION('ref_axis',(1.,0.,0.));
#64689=DIRECTION('',(1.,0.,0.));
#64690=DIRECTION('',(0.,0.,-1.));
#64691=DIRECTION('',(1.,0.,0.));
#64692=DIRECTION('',(0.,0.,-1.));
#64693=DIRECTION('center_axis',(-1.,0.,0.));
#64694=DIRECTION('ref_axis',(0.,1.,0.));
#64695=DIRECTION('',(0.,1.,0.));
#64696=DIRECTION('',(0.,0.,-1.));
#64697=DIRECTION('',(0.,1.,0.));
#64698=DIRECTION('center_axis',(0.,-1.,0.));
#64699=DIRECTION('ref_axis',(-1.,0.,0.));
#64700=DIRECTION('',(-1.,0.,0.));
#64701=DIRECTION('',(0.,0.,-1.));
#64702=DIRECTION('',(-1.,0.,0.));
#64703=DIRECTION('center_axis',(1.,0.,0.));
#64704=DIRECTION('ref_axis',(0.,-1.,0.));
#64705=DIRECTION('',(0.,-1.,0.));
#64706=DIRECTION('',(0.,-1.,0.));
#64707=DIRECTION('center_axis',(0.,0.,-1.));
#64708=DIRECTION('ref_axis',(-1.,0.,0.));
#64709=DIRECTION('',(0.,0.,-1.));
#64710=DIRECTION('',(0.,0.,-1.));
#64711=DIRECTION('',(0.,0.,-1.));
#64712=DIRECTION('',(0.,0.,-1.));
#64713=DIRECTION('',(0.,0.,-1.));
#64714=DIRECTION('',(0.,0.,-1.));
#64715=DIRECTION('',(0.,0.,-1.));
#64716=DIRECTION('',(0.,0.,-1.));
#64717=DIRECTION('',(0.,0.,-1.));
#64718=DIRECTION('',(0.,0.,-1.));
#64719=DIRECTION('',(0.,0.,-1.));
#64720=DIRECTION('',(0.,0.,-1.));
#64721=DIRECTION('',(0.,0.,-1.));
#64722=DIRECTION('',(0.,0.,-1.));
#64723=DIRECTION('center_axis',(0.0750546489289138,-0.997179422006971,0.));
#64724=DIRECTION('ref_axis',(-0.997179422006971,-0.0750546489289138,0.));
#64725=DIRECTION('',(-0.997179422006971,-0.0750546489289138,0.));
#64726=DIRECTION('',(0.,0.,-1.));
#64727=DIRECTION('',(-0.997179422006971,-0.0750546489289138,0.));
#64728=DIRECTION('',(0.,0.,-1.));
#64729=DIRECTION('',(0.,0.,-1.));
#64730=DIRECTION('',(0.,0.,-1.));
#64731=DIRECTION('',(0.,0.,-1.));
#64732=DIRECTION('',(0.,0.,-1.));
#64733=DIRECTION('',(0.,0.,-1.));
#64734=DIRECTION('',(0.,0.,-1.));
#64735=DIRECTION('',(0.,0.,-1.));
#64736=DIRECTION('',(0.,0.,-1.));
#64737=DIRECTION('',(0.,0.,-1.));
#64738=DIRECTION('',(0.,0.,-1.));
#64739=DIRECTION('',(0.,0.,-1.));
#64740=DIRECTION('',(0.,0.,-1.));
#64741=DIRECTION('',(0.,0.,-1.));
#64742=DIRECTION('',(0.,0.,-1.));
#64743=DIRECTION('',(0.,0.,-1.));
#64744=DIRECTION('',(0.,0.,-1.));
#64745=DIRECTION('',(0.,0.,-1.));
#64746=DIRECTION('center_axis',(-0.0871014161005409,0.996199449564835,0.));
#64747=DIRECTION('ref_axis',(0.996199449564835,0.0871014161005409,0.));
#64748=DIRECTION('',(0.996199449564835,0.0871014161005409,0.));
#64749=DIRECTION('',(0.,0.,-1.));
#64750=DIRECTION('',(0.996199449564835,0.0871014161005409,0.));
#64751=DIRECTION('',(0.,0.,-1.));
#64752=DIRECTION('center_axis',(0.,0.,1.));
#64753=DIRECTION('ref_axis',(1.,0.,0.));
#64754=DIRECTION('',(0.,0.,-1.));
#64755=DIRECTION('',(0.,0.,-1.));
#64756=DIRECTION('',(0.,0.,-1.));
#64757=DIRECTION('',(0.,0.,-1.));
#64758=DIRECTION('',(0.,0.,-1.));
#64759=DIRECTION('',(0.,0.,-1.));
#64760=DIRECTION('',(0.,0.,-1.));
#64761=DIRECTION('',(0.,0.,-1.));
#64762=DIRECTION('',(0.,0.,-1.));
#64763=DIRECTION('center_axis',(0.229319053916465,-0.973351309400084,0.));
#64764=DIRECTION('ref_axis',(-0.973351309400084,-0.229319053916465,0.));
#64765=DIRECTION('',(-0.973351309400084,-0.229319053916465,0.));
#64766=DIRECTION('',(0.,0.,-1.));
#64767=DIRECTION('',(-0.973351309400084,-0.229319053916465,0.));
#64768=DIRECTION('',(0.,0.,-1.));
#64769=DIRECTION('',(0.,0.,-1.));
#64770=DIRECTION('',(0.,0.,-1.));
#64771=DIRECTION('',(0.,0.,-1.));
#64772=DIRECTION('',(0.,0.,-1.));
#64773=DIRECTION('',(0.,0.,-1.));
#64774=DIRECTION('',(0.,0.,-1.));
#64775=DIRECTION('',(0.,0.,-1.));
#64776=DIRECTION('',(0.,0.,-1.));
#64777=DIRECTION('',(0.,0.,-1.));
#64778=DIRECTION('center_axis',(0.244891010635767,0.969550613897899,0.));
#64779=DIRECTION('ref_axis',(0.969550613897899,-0.244891010635767,0.));
#64780=DIRECTION('',(0.969550613897899,-0.244891010635767,0.));
#64781=DIRECTION('',(0.,0.,-1.));
#64782=DIRECTION('',(0.969550613897899,-0.244891010635767,0.));
#64783=DIRECTION('',(0.,0.,-1.));
#64784=DIRECTION('center_axis',(0.,0.,1.));
#64785=DIRECTION('ref_axis',(1.,0.,0.));
#64786=DIRECTION('center_axis',(0.,1.,0.));
#64787=DIRECTION('ref_axis',(1.,0.,0.));
#64788=DIRECTION('',(1.,0.,0.));
#64789=DIRECTION('',(0.,0.,-1.));
#64790=DIRECTION('',(1.,0.,0.));
#64791=DIRECTION('',(0.,0.,-1.));
#64792=DIRECTION('center_axis',(1.,0.,0.));
#64793=DIRECTION('ref_axis',(0.,-1.,0.));
#64794=DIRECTION('',(0.,-1.,0.));
#64795=DIRECTION('',(0.,0.,-1.));
#64796=DIRECTION('',(0.,-1.,0.));
#64797=DIRECTION('center_axis',(0.,1.,0.));
#64798=DIRECTION('ref_axis',(1.,0.,0.));
#64799=DIRECTION('',(1.,0.,0.));
#64800=DIRECTION('',(0.,0.,-1.));
#64801=DIRECTION('',(1.,0.,0.));
#64802=DIRECTION('center_axis',(-1.,0.,0.));
#64803=DIRECTION('ref_axis',(0.,1.,0.));
#64804=DIRECTION('',(0.,1.,0.));
#64805=DIRECTION('',(0.,0.,-1.));
#64806=DIRECTION('',(0.,1.,0.));
#64807=DIRECTION('center_axis',(0.,-1.,0.));
#64808=DIRECTION('ref_axis',(-1.,0.,0.));
#64809=DIRECTION('',(-1.,0.,0.));
#64810=DIRECTION('',(0.,0.,-1.));
#64811=DIRECTION('',(-1.,0.,0.));
#64812=DIRECTION('center_axis',(1.,0.,0.));
#64813=DIRECTION('ref_axis',(0.,-1.,0.));
#64814=DIRECTION('',(0.,-1.,0.));
#64815=DIRECTION('',(0.,-1.,0.));
#64816=DIRECTION('center_axis',(0.,0.,-1.));
#64817=DIRECTION('ref_axis',(-1.,0.,0.));
#64818=DIRECTION('center_axis',(0.,-1.,0.));
#64819=DIRECTION('ref_axis',(-1.,0.,0.));
#64820=DIRECTION('',(-1.,0.,0.));
#64821=DIRECTION('',(0.,0.,-1.));
#64822=DIRECTION('',(-1.,0.,0.));
#64823=DIRECTION('',(0.,0.,-1.));
#64824=DIRECTION('center_axis',(1.,0.,0.));
#64825=DIRECTION('ref_axis',(0.,-1.,0.));
#64826=DIRECTION('',(0.,-1.,0.));
#64827=DIRECTION('',(0.,0.,-1.));
#64828=DIRECTION('',(0.,-1.,0.));
#64829=DIRECTION('center_axis',(0.,1.,0.));
#64830=DIRECTION('ref_axis',(1.,0.,0.));
#64831=DIRECTION('',(1.,0.,0.));
#64832=DIRECTION('',(0.,0.,-1.));
#64833=DIRECTION('',(1.,0.,0.));
#64834=DIRECTION('center_axis',(-1.,0.,0.));
#64835=DIRECTION('ref_axis',(0.,1.,0.));
#64836=DIRECTION('',(0.,1.,0.));
#64837=DIRECTION('',(0.,0.,-1.));
#64838=DIRECTION('',(0.,1.,0.));
#64839=DIRECTION('center_axis',(0.,-1.,0.));
#64840=DIRECTION('ref_axis',(-1.,0.,0.));
#64841=DIRECTION('',(-1.,0.,0.));
#64842=DIRECTION('',(0.,0.,-1.));
#64843=DIRECTION('',(-1.,0.,0.));
#64844=DIRECTION('center_axis',(-1.,0.,0.));
#64845=DIRECTION('ref_axis',(0.,1.,0.));
#64846=DIRECTION('',(0.,1.,0.));
#64847=DIRECTION('',(0.,0.,-1.));
#64848=DIRECTION('',(0.,1.,0.));
#64849=DIRECTION('center_axis',(0.,-1.,0.));
#64850=DIRECTION('ref_axis',(-1.,0.,0.));
#64851=DIRECTION('',(-1.,0.,0.));
#64852=DIRECTION('',(0.,0.,-1.));
#64853=DIRECTION('',(-1.,0.,0.));
#64854=DIRECTION('center_axis',(1.,0.,0.));
#64855=DIRECTION('ref_axis',(0.,-1.,0.));
#64856=DIRECTION('',(0.,-1.,0.));
#64857=DIRECTION('',(0.,-1.,0.));
#64858=DIRECTION('center_axis',(0.,0.,-1.));
#64859=DIRECTION('ref_axis',(-1.,0.,0.));
#64860=DIRECTION('',(0.,0.,-1.));
#64861=DIRECTION('',(0.,0.,-1.));
#64862=DIRECTION('',(0.,0.,-1.));
#64863=DIRECTION('',(0.,0.,-1.));
#64864=DIRECTION('',(0.,0.,-1.));
#64865=DIRECTION('center_axis',(1.,0.,0.));
#64866=DIRECTION('ref_axis',(0.,-1.,0.));
#64867=DIRECTION('',(0.,-1.,0.));
#64868=DIRECTION('',(0.,0.,-1.));
#64869=DIRECTION('',(0.,-1.,0.));
#64870=DIRECTION('center_axis',(0.,1.,0.));
#64871=DIRECTION('ref_axis',(1.,0.,0.));
#64872=DIRECTION('',(1.,0.,0.));
#64873=DIRECTION('',(0.,0.,-1.));
#64874=DIRECTION('',(1.,0.,0.));
#64875=DIRECTION('center_axis',(-1.,0.,0.));
#64876=DIRECTION('ref_axis',(0.,1.,0.));
#64877=DIRECTION('',(0.,1.,0.));
#64878=DIRECTION('',(0.,0.,-1.));
#64879=DIRECTION('',(0.,1.,0.));
#64880=DIRECTION('',(0.,0.,-1.));
#64881=DIRECTION('',(0.,0.,-1.));
#64882=DIRECTION('',(0.,0.,-1.));
#64883=DIRECTION('',(0.,0.,-1.));
#64884=DIRECTION('',(0.,0.,-1.));
#64885=DIRECTION('',(0.,0.,-1.));
#64886=DIRECTION('center_axis',(1.,0.,0.));
#64887=DIRECTION('ref_axis',(0.,-1.,0.));
#64888=DIRECTION('',(0.,-1.,0.));
#64889=DIRECTION('',(0.,0.,-1.));
#64890=DIRECTION('',(0.,-1.,0.));
#64891=DIRECTION('center_axis',(0.,1.,0.));
#64892=DIRECTION('ref_axis',(1.,0.,0.));
#64893=DIRECTION('',(1.,0.,0.));
#64894=DIRECTION('',(0.,0.,-1.));
#64895=DIRECTION('',(1.,0.,0.));
#64896=DIRECTION('center_axis',(-1.,0.,0.));
#64897=DIRECTION('ref_axis',(0.,1.,0.));
#64898=DIRECTION('',(0.,1.,0.));
#64899=DIRECTION('',(0.,0.,-1.));
#64900=DIRECTION('',(0.,1.,0.));
#64901=DIRECTION('center_axis',(0.,0.,1.));
#64902=DIRECTION('ref_axis',(1.,0.,0.));
#64903=DIRECTION('center_axis',(0.,-1.,0.));
#64904=DIRECTION('ref_axis',(-1.,0.,0.));
#64905=DIRECTION('',(-1.,0.,0.));
#64906=DIRECTION('',(0.,0.,-1.));
#64907=DIRECTION('',(-1.,0.,0.));
#64908=DIRECTION('',(0.,0.,-1.));
#64909=DIRECTION('',(0.,0.,-1.));
#64910=DIRECTION('',(0.,0.,-1.));
#64911=DIRECTION('',(0.,0.,-1.));
#64912=DIRECTION('',(0.,0.,-1.));
#64913=DIRECTION('center_axis',(-0.843774210720013,-0.536698314999981,0.));
#64914=DIRECTION('ref_axis',(-0.536698314999981,0.843774210720013,0.));
#64915=DIRECTION('',(-0.536698314999981,0.843774210720013,0.));
#64916=DIRECTION('',(0.,0.,-1.));
#64917=DIRECTION('',(-0.536698314999981,0.843774210720013,0.));
#64918=DIRECTION('center_axis',(0.,-1.,0.));
#64919=DIRECTION('ref_axis',(-1.,0.,0.));
#64920=DIRECTION('',(-1.,0.,0.));
#64921=DIRECTION('',(0.,0.,-1.));
#64922=DIRECTION('',(-1.,0.,0.));
#64923=DIRECTION('center_axis',(0.842616728563894,0.538513740534336,0.));
#64924=DIRECTION('ref_axis',(0.538513740534336,-0.842616728563894,0.));
#64925=DIRECTION('',(0.538513740534336,-0.842616728563894,0.));
#64926=DIRECTION('',(0.,0.,-1.));
#64927=DIRECTION('',(0.538513740534336,-0.842616728563894,0.));
#64928=DIRECTION('',(0.,0.,-1.));
#64929=DIRECTION('',(0.,0.,-1.));
#64930=DIRECTION('',(0.,0.,-1.));
#64931=DIRECTION('',(0.,0.,-1.));
#64932=DIRECTION('',(0.,0.,-1.));
#64933=DIRECTION('',(0.,0.,-1.));
#64934=DIRECTION('',(0.,0.,-1.));
#64935=DIRECTION('center_axis',(0.,1.,0.));
#64936=DIRECTION('ref_axis',(1.,0.,0.));
#64937=DIRECTION('',(1.,0.,0.));
#64938=DIRECTION('',(0.,0.,-1.));
#64939=DIRECTION('',(1.,0.,0.));
#64940=DIRECTION('center_axis',(-1.,0.,0.));
#64941=DIRECTION('ref_axis',(0.,1.,0.));
#64942=DIRECTION('',(0.,1.,0.));
#64943=DIRECTION('',(0.,0.,-1.));
#64944=DIRECTION('',(0.,1.,0.));
#64945=DIRECTION('center_axis',(0.,-1.,0.));
#64946=DIRECTION('ref_axis',(-1.,0.,0.));
#64947=DIRECTION('',(-1.,0.,0.));
#64948=DIRECTION('',(0.,0.,-1.));
#64949=DIRECTION('',(-1.,0.,0.));
#64950=DIRECTION('center_axis',(1.,0.,0.));
#64951=DIRECTION('ref_axis',(0.,-1.,0.));
#64952=DIRECTION('',(0.,-1.,0.));
#64953=DIRECTION('',(0.,-1.,0.));
#64954=DIRECTION('center_axis',(0.,0.,1.));
#64955=DIRECTION('ref_axis',(1.,0.,0.));
#64956=DIRECTION('center_axis',(0.,-1.,0.));
#64957=DIRECTION('ref_axis',(-1.,0.,0.));
#64958=DIRECTION('',(-1.,0.,0.));
#64959=DIRECTION('',(0.,0.,-1.));
#64960=DIRECTION('',(-1.,0.,0.));
#64961=DIRECTION('',(0.,0.,-1.));
#64962=DIRECTION('center_axis',(1.,0.,0.));
#64963=DIRECTION('ref_axis',(0.,-1.,0.));
#64964=DIRECTION('',(0.,-1.,0.));
#64965=DIRECTION('',(0.,0.,-1.));
#64966=DIRECTION('',(0.,-1.,0.));
#64967=DIRECTION('center_axis',(0.,1.,0.));
#64968=DIRECTION('ref_axis',(1.,0.,0.));
#64969=DIRECTION('',(1.,0.,0.));
#64970=DIRECTION('',(0.,0.,-1.));
#64971=DIRECTION('',(1.,0.,0.));
#64972=DIRECTION('center_axis',(-1.,0.,0.));
#64973=DIRECTION('ref_axis',(0.,1.,0.));
#64974=DIRECTION('',(0.,1.,0.));
#64975=DIRECTION('',(0.,0.,-1.));
#64976=DIRECTION('',(0.,1.,0.));
#64977=DIRECTION('center_axis',(0.,-1.,0.));
#64978=DIRECTION('ref_axis',(-1.,0.,0.));
#64979=DIRECTION('',(-1.,0.,0.));
#64980=DIRECTION('',(0.,0.,-1.));
#64981=DIRECTION('',(-1.,0.,0.));
#64982=DIRECTION('center_axis',(-1.,0.,0.));
#64983=DIRECTION('ref_axis',(0.,1.,0.));
#64984=DIRECTION('',(0.,1.,0.));
#64985=DIRECTION('',(0.,0.,-1.));
#64986=DIRECTION('',(0.,1.,0.));
#64987=DIRECTION('center_axis',(0.,-1.,0.));
#64988=DIRECTION('ref_axis',(-1.,0.,0.));
#64989=DIRECTION('',(-1.,0.,0.));
#64990=DIRECTION('',(0.,0.,-1.));
#64991=DIRECTION('',(-1.,0.,0.));
#64992=DIRECTION('center_axis',(1.,0.,0.));
#64993=DIRECTION('ref_axis',(0.,-1.,0.));
#64994=DIRECTION('',(0.,-1.,0.));
#64995=DIRECTION('',(0.,-1.,0.));
#64996=DIRECTION('center_axis',(0.,0.,-1.));
#64997=DIRECTION('ref_axis',(-1.,0.,0.));
#64998=DIRECTION('',(0.,0.,-1.));
#64999=DIRECTION('',(0.,0.,-1.));
#65000=DIRECTION('',(0.,0.,-1.));
#65001=DIRECTION('center_axis',(-1.,1.10046549710191E-14,0.));
#65002=DIRECTION('ref_axis',(1.10046549710191E-14,1.,0.));
#65003=DIRECTION('',(1.10046549710191E-14,1.,0.));
#65004=DIRECTION('',(0.,0.,-1.));
#65005=DIRECTION('',(1.10046549710191E-14,1.,0.));
#65006=DIRECTION('',(0.,0.,-1.));
#65007=DIRECTION('',(0.,0.,-1.));
#65008=DIRECTION('center_axis',(-1.,0.,0.));
#65009=DIRECTION('ref_axis',(0.,1.,0.));
#65010=DIRECTION('',(0.,1.,0.));
#65011=DIRECTION('',(0.,0.,-1.));
#65012=DIRECTION('',(0.,1.,0.));
#65013=DIRECTION('center_axis',(0.,-1.,0.));
#65014=DIRECTION('ref_axis',(-1.,0.,0.));
#65015=DIRECTION('',(-1.,0.,0.));
#65016=DIRECTION('',(0.,0.,-1.));
#65017=DIRECTION('',(-1.,0.,0.));
#65018=DIRECTION('center_axis',(1.,0.,0.));
#65019=DIRECTION('ref_axis',(0.,-1.,0.));
#65020=DIRECTION('',(0.,-1.,0.));
#65021=DIRECTION('',(0.,0.,-1.));
#65022=DIRECTION('',(0.,-1.,0.));
#65023=DIRECTION('center_axis',(0.,1.,0.));
#65024=DIRECTION('ref_axis',(1.,0.,0.));
#65025=DIRECTION('',(1.,0.,0.));
#65026=DIRECTION('',(1.,0.,0.));
#65027=DIRECTION('center_axis',(0.,0.,1.));
#65028=DIRECTION('ref_axis',(1.,0.,0.));
#65029=DIRECTION('',(0.,0.,-1.));
#65030=DIRECTION('',(0.,0.,-1.));
#65031=DIRECTION('',(0.,0.,-1.));
#65032=DIRECTION('',(0.,0.,-1.));
#65033=DIRECTION('',(0.,0.,-1.));
#65034=DIRECTION('',(0.,0.,-1.));
#65035=DIRECTION('',(0.,0.,-1.));
#65036=DIRECTION('',(0.,0.,-1.));
#65037=DIRECTION('',(0.,0.,-1.));
#65038=DIRECTION('',(0.,0.,-1.));
#65039=DIRECTION('',(0.,0.,-1.));
#65040=DIRECTION('',(0.,0.,-1.));
#65041=DIRECTION('center_axis',(0.,0.,1.));
#65042=DIRECTION('ref_axis',(1.,0.,0.));
#65043=DIRECTION('',(0.,0.,-1.));
#65044=DIRECTION('',(0.,0.,-1.));
#65045=DIRECTION('',(0.,0.,-1.));
#65046=DIRECTION('center_axis',(-1.,0.,0.));
#65047=DIRECTION('ref_axis',(0.,1.,0.));
#65048=DIRECTION('',(0.,1.,0.));
#65049=DIRECTION('',(0.,0.,-1.));
#65050=DIRECTION('',(0.,1.,0.));
#65051=DIRECTION('',(0.,0.,-1.));
#65052=DIRECTION('',(0.,0.,-1.));
#65053=DIRECTION('center_axis',(-1.,0.,0.));
#65054=DIRECTION('ref_axis',(0.,1.,0.));
#65055=DIRECTION('',(0.,1.,0.));
#65056=DIRECTION('',(0.,0.,-1.));
#65057=DIRECTION('',(0.,1.,0.));
#65058=DIRECTION('center_axis',(0.,-1.,0.));
#65059=DIRECTION('ref_axis',(-1.,0.,0.));
#65060=DIRECTION('',(-1.,0.,0.));
#65061=DIRECTION('',(0.,0.,-1.));
#65062=DIRECTION('',(-1.,0.,0.));
#65063=DIRECTION('center_axis',(1.,0.,0.));
#65064=DIRECTION('ref_axis',(0.,-1.,0.));
#65065=DIRECTION('',(0.,-1.,0.));
#65066=DIRECTION('',(0.,0.,-1.));
#65067=DIRECTION('',(0.,-1.,0.));
#65068=DIRECTION('center_axis',(0.,1.,0.));
#65069=DIRECTION('ref_axis',(1.,0.,0.));
#65070=DIRECTION('',(1.,0.,0.));
#65071=DIRECTION('',(1.,0.,0.));
#65072=DIRECTION('center_axis',(0.,0.,1.));
#65073=DIRECTION('ref_axis',(1.,0.,0.));
#65074=DIRECTION('center_axis',(0.,1.,0.));
#65075=DIRECTION('ref_axis',(1.,0.,0.));
#65076=DIRECTION('',(1.,0.,0.));
#65077=DIRECTION('',(0.,0.,-1.));
#65078=DIRECTION('',(1.,0.,0.));
#65079=DIRECTION('',(0.,0.,-1.));
#65080=DIRECTION('center_axis',(-1.,0.,0.));
#65081=DIRECTION('ref_axis',(0.,1.,0.));
#65082=DIRECTION('',(0.,1.,0.));
#65083=DIRECTION('',(0.,0.,-1.));
#65084=DIRECTION('',(0.,1.,0.));
#65085=DIRECTION('center_axis',(0.,-1.,0.));
#65086=DIRECTION('ref_axis',(-1.,0.,0.));
#65087=DIRECTION('',(-1.,0.,0.));
#65088=DIRECTION('',(0.,0.,-1.));
#65089=DIRECTION('',(-1.,0.,0.));
#65090=DIRECTION('center_axis',(1.,0.,0.));
#65091=DIRECTION('ref_axis',(0.,-1.,0.));
#65092=DIRECTION('',(0.,-1.,0.));
#65093=DIRECTION('',(0.,-1.,0.));
#65094=DIRECTION('center_axis',(0.,0.,-1.));
#65095=DIRECTION('ref_axis',(-1.,0.,0.));
#65096=DIRECTION('',(0.,0.,-1.));
#65097=DIRECTION('',(0.,0.,-1.));
#65098=DIRECTION('',(0.,0.,-1.));
#65099=DIRECTION('',(0.,0.,-1.));
#65100=DIRECTION('',(0.,0.,-1.));
#65101=DIRECTION('',(0.,0.,-1.));
#65102=DIRECTION('center_axis',(0.980484772608259,-0.196595042367124,0.));
#65103=DIRECTION('ref_axis',(-0.196595042367124,-0.980484772608259,0.));
#65104=DIRECTION('',(-0.196595042367124,-0.980484772608259,0.));
#65105=DIRECTION('',(0.,0.,-1.));
#65106=DIRECTION('',(-0.196595042367124,-0.980484772608259,0.));
#65107=DIRECTION('center_axis',(0.,-1.,0.));
#65108=DIRECTION('ref_axis',(-1.,0.,0.));
#65109=DIRECTION('',(-1.,0.,0.));
#65110=DIRECTION('',(0.,0.,-1.));
#65111=DIRECTION('',(-1.,0.,0.));
#65112=DIRECTION('center_axis',(1.,0.,0.));
#65113=DIRECTION('ref_axis',(0.,-1.,0.));
#65114=DIRECTION('',(0.,-1.,0.));
#65115=DIRECTION('',(0.,0.,-1.));
#65116=DIRECTION('',(0.,-1.,0.));
#65117=DIRECTION('center_axis',(0.,1.,0.));
#65118=DIRECTION('ref_axis',(1.,0.,0.));
#65119=DIRECTION('',(1.,0.,0.));
#65120=DIRECTION('',(0.,0.,-1.));
#65121=DIRECTION('',(1.,0.,0.));
#65122=DIRECTION('center_axis',(-0.982679625842875,0.185312581745834,0.));
#65123=DIRECTION('ref_axis',(0.185312581745834,0.982679625842876,0.));
#65124=DIRECTION('',(0.185312581745834,0.982679625842876,0.));
#65125=DIRECTION('',(0.,0.,-1.));
#65126=DIRECTION('',(0.185312581745834,0.982679625842876,0.));
#65127=DIRECTION('center_axis',(-0.129088850062387,-0.991633031312275,0.));
#65128=DIRECTION('ref_axis',(-0.991633031312275,0.129088850062387,0.));
#65129=DIRECTION('',(-0.991633031312275,0.129088850062387,0.));
#65130=DIRECTION('',(0.,0.,-1.));
#65131=DIRECTION('',(-0.991633031312275,0.129088850062387,0.));
#65132=DIRECTION('',(0.,0.,-1.));
#65133=DIRECTION('',(0.,0.,-1.));
#65134=DIRECTION('',(0.,0.,-1.));
#65135=DIRECTION('',(0.,0.,-1.));
#65136=DIRECTION('',(0.,0.,-1.));
#65137=DIRECTION('',(0.,0.,-1.));
#65138=DIRECTION('',(0.,0.,-1.));
#65139=DIRECTION('',(0.,0.,-1.));
#65140=DIRECTION('center_axis',(-0.0843535578886116,0.99643588718569,0.));
#65141=DIRECTION('ref_axis',(0.99643588718569,0.0843535578886116,0.));
#65142=DIRECTION('',(0.99643588718569,0.0843535578886116,0.));
#65143=DIRECTION('',(0.,0.,-1.));
#65144=DIRECTION('',(0.99643588718569,0.0843535578886116,0.));
#65145=DIRECTION('',(0.,0.,-1.));
#65146=DIRECTION('center_axis',(0.,0.,1.));
#65147=DIRECTION('ref_axis',(1.,0.,0.));
#65148=DIRECTION('',(0.,0.,-1.));
#65149=DIRECTION('',(0.,0.,-1.));
#65150=DIRECTION('',(0.,0.,-1.));
#65151=DIRECTION('',(0.,0.,-1.));
#65152=DIRECTION('',(0.,0.,-1.));
#65153=DIRECTION('',(0.,0.,-1.));
#65154=DIRECTION('',(0.,0.,-1.));
#65155=DIRECTION('',(0.,0.,-1.));
#65156=DIRECTION('',(0.,0.,-1.));
#65157=DIRECTION('',(0.,0.,-1.));
#65158=DIRECTION('',(0.,0.,-1.));
#65159=DIRECTION('center_axis',(0.,0.,1.));
#65160=DIRECTION('ref_axis',(1.,0.,0.));
#65161=DIRECTION('',(0.,0.,-1.));
#65162=DIRECTION('',(0.,0.,-1.));
#65163=DIRECTION('',(0.,0.,-1.));
#65164=DIRECTION('',(0.,0.,-1.));
#65165=DIRECTION('',(0.,0.,-1.));
#65166=DIRECTION('',(0.,0.,-1.));
#65167=DIRECTION('',(0.,0.,-1.));
#65168=DIRECTION('',(0.,0.,-1.));
#65169=DIRECTION('',(0.,0.,-1.));
#65170=DIRECTION('',(0.,0.,-1.));
#65171=DIRECTION('',(0.,0.,-1.));
#65172=DIRECTION('',(0.,0.,-1.));
#65173=DIRECTION('center_axis',(0.921250259693202,-0.388970383210866,0.));
#65174=DIRECTION('ref_axis',(-0.388970383210866,-0.921250259693202,0.));
#65175=DIRECTION('',(-0.388970383210866,-0.921250259693202,0.));
#65176=DIRECTION('',(0.,0.,-1.));
#65177=DIRECTION('',(-0.388970383210866,-0.921250259693202,0.));
#65178=DIRECTION('',(0.,0.,-1.));
#65179=DIRECTION('',(0.,0.,-1.));
#65180=DIRECTION('center_axis',(0.,0.,1.));
#65181=DIRECTION('ref_axis',(1.,0.,0.));
#65182=DIRECTION('center_axis',(0.,1.,0.));
#65183=DIRECTION('ref_axis',(1.,0.,0.));
#65184=DIRECTION('',(1.,0.,0.));
#65185=DIRECTION('',(0.,0.,-1.));
#65186=DIRECTION('',(1.,0.,0.));
#65187=DIRECTION('',(0.,0.,-1.));
#65188=DIRECTION('center_axis',(1.,0.,0.));
#65189=DIRECTION('ref_axis',(0.,-1.,0.));
#65190=DIRECTION('',(0.,-1.,0.));
#65191=DIRECTION('',(0.,0.,-1.));
#65192=DIRECTION('',(0.,-1.,0.));
#65193=DIRECTION('center_axis',(0.,-1.,0.));
#65194=DIRECTION('ref_axis',(-1.,0.,0.));
#65195=DIRECTION('',(-1.,0.,0.));
#65196=DIRECTION('',(0.,0.,-1.));
#65197=DIRECTION('',(-1.,0.,0.));
#65198=DIRECTION('center_axis',(1.,0.,0.));
#65199=DIRECTION('ref_axis',(0.,-1.,0.));
#65200=DIRECTION('',(0.,-1.,0.));
#65201=DIRECTION('',(0.,0.,-1.));
#65202=DIRECTION('',(0.,-1.,0.));
#65203=DIRECTION('center_axis',(0.,1.,0.));
#65204=DIRECTION('ref_axis',(1.,0.,0.));
#65205=DIRECTION('',(1.,0.,0.));
#65206=DIRECTION('',(0.,0.,-1.));
#65207=DIRECTION('',(1.,0.,0.));
#65208=DIRECTION('center_axis',(1.,0.,0.));
#65209=DIRECTION('ref_axis',(0.,-1.,0.));
#65210=DIRECTION('',(0.,-1.,0.));
#65211=DIRECTION('',(0.,0.,-1.));
#65212=DIRECTION('',(0.,-1.,0.));
#65213=DIRECTION('center_axis',(0.,-1.,0.));
#65214=DIRECTION('ref_axis',(-1.,0.,0.));
#65215=DIRECTION('',(-1.,0.,0.));
#65216=DIRECTION('',(0.,0.,-1.));
#65217=DIRECTION('',(-1.,0.,0.));
#65218=DIRECTION('center_axis',(1.,0.,0.));
#65219=DIRECTION('ref_axis',(0.,-1.,0.));
#65220=DIRECTION('',(0.,-1.,0.));
#65221=DIRECTION('',(0.,0.,-1.));
#65222=DIRECTION('',(0.,-1.,0.));
#65223=DIRECTION('center_axis',(0.,1.,0.));
#65224=DIRECTION('ref_axis',(1.,0.,0.));
#65225=DIRECTION('',(1.,0.,0.));
#65226=DIRECTION('',(0.,0.,-1.));
#65227=DIRECTION('',(1.,0.,0.));
#65228=DIRECTION('center_axis',(-1.,0.,0.));
#65229=DIRECTION('ref_axis',(0.,1.,0.));
#65230=DIRECTION('',(0.,1.,0.));
#65231=DIRECTION('',(0.,0.,-1.));
#65232=DIRECTION('',(0.,1.,0.));
#65233=DIRECTION('center_axis',(0.,-1.,0.));
#65234=DIRECTION('ref_axis',(-1.,0.,0.));
#65235=DIRECTION('',(-1.,0.,0.));
#65236=DIRECTION('',(0.,0.,-1.));
#65237=DIRECTION('',(-1.,0.,0.));
#65238=DIRECTION('center_axis',(1.,0.,0.));
#65239=DIRECTION('ref_axis',(0.,-1.,0.));
#65240=DIRECTION('',(0.,-1.,0.));
#65241=DIRECTION('',(0.,-1.,0.));
#65242=DIRECTION('center_axis',(0.,0.,-1.));
#65243=DIRECTION('ref_axis',(-1.,0.,0.));
#65244=DIRECTION('center_axis',(0.,1.,0.));
#65245=DIRECTION('ref_axis',(1.,0.,0.));
#65246=DIRECTION('',(1.,0.,0.));
#65247=DIRECTION('',(0.,0.,-1.));
#65248=DIRECTION('',(1.,0.,0.));
#65249=DIRECTION('',(0.,0.,-1.));
#65250=DIRECTION('center_axis',(-1.,0.,0.));
#65251=DIRECTION('ref_axis',(0.,1.,0.));
#65252=DIRECTION('',(0.,1.,0.));
#65253=DIRECTION('',(0.,0.,-1.));
#65254=DIRECTION('',(0.,1.,0.));
#65255=DIRECTION('center_axis',(0.,-1.,0.));
#65256=DIRECTION('ref_axis',(-1.,0.,0.));
#65257=DIRECTION('',(-1.,0.,0.));
#65258=DIRECTION('',(0.,0.,-1.));
#65259=DIRECTION('',(-1.,0.,0.));
#65260=DIRECTION('center_axis',(1.,0.,0.));
#65261=DIRECTION('ref_axis',(0.,-1.,0.));
#65262=DIRECTION('',(0.,-1.,0.));
#65263=DIRECTION('',(0.,-1.,0.));
#65264=DIRECTION('center_axis',(0.,0.,-1.));
#65265=DIRECTION('ref_axis',(-1.,0.,0.));
#65266=DIRECTION('',(0.,0.,-1.));
#65267=DIRECTION('',(0.,0.,-1.));
#65268=DIRECTION('',(0.,0.,-1.));
#65269=DIRECTION('',(0.,0.,-1.));
#65270=DIRECTION('',(0.,0.,-1.));
#65271=DIRECTION('',(0.,0.,-1.));
#65272=DIRECTION('',(0.,0.,-1.));
#65273=DIRECTION('',(0.,0.,-1.));
#65274=DIRECTION('',(0.,0.,-1.));
#65275=DIRECTION('',(0.,0.,-1.));
#65276=DIRECTION('',(0.,0.,-1.));
#65277=DIRECTION('center_axis',(0.,0.,1.));
#65278=DIRECTION('ref_axis',(1.,0.,0.));
#65279=DIRECTION('center_axis',(0.698096755785859,-0.716003435439565,0.));
#65280=DIRECTION('ref_axis',(-0.716003435439565,-0.698096755785859,0.));
#65281=DIRECTION('',(-0.716003435439565,-0.698096755785859,0.));
#65282=DIRECTION('',(0.,0.,-1.));
#65283=DIRECTION('',(-0.716003435439565,-0.698096755785859,0.));
#65284=DIRECTION('',(0.,0.,-1.));
#65285=DIRECTION('center_axis',(-0.817885251670677,-0.575381364922078,0.));
#65286=DIRECTION('ref_axis',(-0.575381364922078,0.817885251670677,0.));
#65287=DIRECTION('',(-0.575381364922078,0.817885251670677,0.));
#65288=DIRECTION('',(0.,0.,-1.));
#65289=DIRECTION('',(-0.575381364922078,0.817885251670677,0.));
#65290=DIRECTION('center_axis',(0.,-1.,0.));
#65291=DIRECTION('ref_axis',(-1.,0.,0.));
#65292=DIRECTION('',(-1.,0.,0.));
#65293=DIRECTION('',(0.,0.,-1.));
#65294=DIRECTION('',(-1.,0.,0.));
#65295=DIRECTION('center_axis',(0.8052872827866,0.592884805153729,0.));
#65296=DIRECTION('ref_axis',(0.592884805153729,-0.8052872827866,0.));
#65297=DIRECTION('',(0.592884805153729,-0.8052872827866,0.));
#65298=DIRECTION('',(0.,0.,-1.));
#65299=DIRECTION('',(0.592884805153729,-0.8052872827866,0.));
#65300=DIRECTION('center_axis',(0.694718635560915,-0.719281598127173,0.));
#65301=DIRECTION('ref_axis',(-0.719281598127173,-0.694718635560915,0.));
#65302=DIRECTION('',(-0.719281598127173,-0.694718635560915,0.));
#65303=DIRECTION('',(0.,0.,-1.));
#65304=DIRECTION('',(-0.719281598127173,-0.694718635560915,0.));
#65305=DIRECTION('center_axis',(0.,1.,0.));
#65306=DIRECTION('ref_axis',(1.,0.,0.));
#65307=DIRECTION('',(1.,0.,0.));
#65308=DIRECTION('',(0.,0.,-1.));
#65309=DIRECTION('',(1.,0.,0.));
#65310=DIRECTION('center_axis',(-0.706620509307552,0.707592718889854,0.));
#65311=DIRECTION('ref_axis',(0.707592718889854,0.706620509307552,0.));
#65312=DIRECTION('',(0.707592718889854,0.706620509307552,0.));
#65313=DIRECTION('',(0.,0.,-1.));
#65314=DIRECTION('',(0.707592718889854,0.706620509307552,0.));
#65315=DIRECTION('center_axis',(1.,0.,0.));
#65316=DIRECTION('ref_axis',(0.,-1.,0.));
#65317=DIRECTION('',(0.,-1.,0.));
#65318=DIRECTION('',(0.,0.,-1.));
#65319=DIRECTION('',(0.,-1.,0.));
#65320=DIRECTION('center_axis',(0.,1.,0.));
#65321=DIRECTION('ref_axis',(1.,0.,0.));
#65322=DIRECTION('',(1.,0.,0.));
#65323=DIRECTION('',(0.,0.,-1.));
#65324=DIRECTION('',(1.,0.,0.));
#65325=DIRECTION('center_axis',(-1.,0.,0.));
#65326=DIRECTION('ref_axis',(0.,1.,0.));
#65327=DIRECTION('',(0.,1.,0.));
#65328=DIRECTION('',(0.,0.,-1.));
#65329=DIRECTION('',(0.,1.,0.));
#65330=DIRECTION('center_axis',(0.,-1.,0.));
#65331=DIRECTION('ref_axis',(-1.,0.,0.));
#65332=DIRECTION('',(-1.,0.,0.));
#65333=DIRECTION('',(0.,0.,-1.));
#65334=DIRECTION('',(-1.,0.,0.));
#65335=DIRECTION('center_axis',(1.,0.,0.));
#65336=DIRECTION('ref_axis',(0.,-1.,0.));
#65337=DIRECTION('',(0.,-1.,0.));
#65338=DIRECTION('',(0.,-1.,0.));
#65339=DIRECTION('center_axis',(0.,0.,-1.));
#65340=DIRECTION('ref_axis',(-1.,0.,0.));
#65341=DIRECTION('center_axis',(0.,1.,0.));
#65342=DIRECTION('ref_axis',(1.,0.,0.));
#65343=DIRECTION('',(1.,0.,0.));
#65344=DIRECTION('',(0.,0.,-1.));
#65345=DIRECTION('',(1.,0.,0.));
#65346=DIRECTION('',(0.,0.,-1.));
#65347=DIRECTION('center_axis',(1.,0.,0.));
#65348=DIRECTION('ref_axis',(0.,-1.,0.));
#65349=DIRECTION('',(0.,-1.,0.));
#65350=DIRECTION('',(0.,0.,-1.));
#65351=DIRECTION('',(0.,-1.,0.));
#65352=DIRECTION('center_axis',(0.,1.,0.));
#65353=DIRECTION('ref_axis',(1.,0.,0.));
#65354=DIRECTION('',(1.,0.,0.));
#65355=DIRECTION('',(0.,0.,-1.));
#65356=DIRECTION('',(1.,0.,0.));
#65357=DIRECTION('center_axis',(-1.,0.,0.));
#65358=DIRECTION('ref_axis',(0.,1.,0.));
#65359=DIRECTION('',(0.,1.,0.));
#65360=DIRECTION('',(0.,0.,-1.));
#65361=DIRECTION('',(0.,1.,0.));
#65362=DIRECTION('center_axis',(0.,-1.,0.));
#65363=DIRECTION('ref_axis',(-1.,0.,0.));
#65364=DIRECTION('',(-1.,0.,0.));
#65365=DIRECTION('',(0.,0.,-1.));
#65366=DIRECTION('',(-1.,0.,0.));
#65367=DIRECTION('center_axis',(1.,0.,0.));
#65368=DIRECTION('ref_axis',(0.,-1.,0.));
#65369=DIRECTION('',(0.,-1.,0.));
#65370=DIRECTION('',(0.,-1.,0.));
#65371=DIRECTION('center_axis',(0.,0.,-1.));
#65372=DIRECTION('ref_axis',(-1.,0.,0.));
#65373=DIRECTION('',(0.,0.,-1.));
#65374=DIRECTION('',(0.,0.,-1.));
#65375=DIRECTION('',(0.,0.,-1.));
#65376=DIRECTION('',(0.,0.,-1.));
#65377=DIRECTION('',(0.,0.,-1.));
#65378=DIRECTION('',(0.,0.,-1.));
#65379=DIRECTION('',(0.,0.,-1.));
#65380=DIRECTION('',(0.,0.,-1.));
#65381=DIRECTION('',(0.,0.,-1.));
#65382=DIRECTION('center_axis',(0.,1.,0.));
#65383=DIRECTION('ref_axis',(1.,0.,0.));
#65384=DIRECTION('',(1.,0.,0.));
#65385=DIRECTION('',(0.,0.,-1.));
#65386=DIRECTION('',(1.,0.,0.));
#65387=DIRECTION('center_axis',(-1.,0.,0.));
#65388=DIRECTION('ref_axis',(0.,1.,0.));
#65389=DIRECTION('',(0.,1.,0.));
#65390=DIRECTION('',(0.,0.,-1.));
#65391=DIRECTION('',(0.,1.,0.));
#65392=DIRECTION('center_axis',(0.,-1.,0.));
#65393=DIRECTION('ref_axis',(-1.,0.,0.));
#65394=DIRECTION('',(-1.,0.,0.));
#65395=DIRECTION('',(0.,0.,-1.));
#65396=DIRECTION('',(-1.,0.,0.));
#65397=DIRECTION('center_axis',(0.,0.,1.));
#65398=DIRECTION('ref_axis',(1.,0.,0.));
#65399=DIRECTION('center_axis',(0.,-1.,0.));
#65400=DIRECTION('ref_axis',(-1.,0.,0.));
#65401=DIRECTION('',(-1.,0.,0.));
#65402=DIRECTION('',(0.,0.,-1.));
#65403=DIRECTION('',(-1.,0.,0.));
#65404=DIRECTION('',(0.,0.,-1.));
#65405=DIRECTION('',(0.,0.,-1.));
#65406=DIRECTION('',(0.,0.,-1.));
#65407=DIRECTION('',(0.,0.,-1.));
#65408=DIRECTION('',(0.,0.,-1.));
#65409=DIRECTION('center_axis',(-0.843779362263309,-0.536690215877393,0.));
#65410=DIRECTION('ref_axis',(-0.536690215877393,0.843779362263309,0.));
#65411=DIRECTION('',(-0.536690215877393,0.843779362263309,0.));
#65412=DIRECTION('',(0.,0.,-1.));
#65413=DIRECTION('',(-0.536690215877393,0.843779362263309,0.));
#65414=DIRECTION('center_axis',(0.,-1.,0.));
#65415=DIRECTION('ref_axis',(-1.,0.,0.));
#65416=DIRECTION('',(-1.,0.,0.));
#65417=DIRECTION('',(0.,0.,-1.));
#65418=DIRECTION('',(-1.,0.,0.));
#65419=DIRECTION('center_axis',(0.842613773269381,0.538518364679178,0.));
#65420=DIRECTION('ref_axis',(0.538518364679178,-0.842613773269381,0.));
#65421=DIRECTION('',(0.538518364679178,-0.842613773269381,0.));
#65422=DIRECTION('',(0.,0.,-1.));
#65423=DIRECTION('',(0.538518364679178,-0.842613773269381,0.));
#65424=DIRECTION('',(0.,0.,-1.));
#65425=DIRECTION('',(0.,0.,-1.));
#65426=DIRECTION('',(0.,0.,-1.));
#65427=DIRECTION('',(0.,0.,-1.));
#65428=DIRECTION('',(0.,0.,-1.));
#65429=DIRECTION('',(0.,0.,-1.));
#65430=DIRECTION('',(0.,0.,-1.));
#65431=DIRECTION('center_axis',(0.,1.,0.));
#65432=DIRECTION('ref_axis',(1.,0.,0.));
#65433=DIRECTION('',(1.,0.,0.));
#65434=DIRECTION('',(0.,0.,-1.));
#65435=DIRECTION('',(1.,0.,0.));
#65436=DIRECTION('center_axis',(-1.,0.,0.));
#65437=DIRECTION('ref_axis',(0.,1.,0.));
#65438=DIRECTION('',(0.,1.,0.));
#65439=DIRECTION('',(0.,0.,-1.));
#65440=DIRECTION('',(0.,1.,0.));
#65441=DIRECTION('center_axis',(0.,-1.,0.));
#65442=DIRECTION('ref_axis',(-1.,0.,0.));
#65443=DIRECTION('',(-1.,0.,0.));
#65444=DIRECTION('',(0.,0.,-1.));
#65445=DIRECTION('',(-1.,0.,0.));
#65446=DIRECTION('center_axis',(1.,0.,0.));
#65447=DIRECTION('ref_axis',(0.,-1.,0.));
#65448=DIRECTION('',(0.,-1.,0.));
#65449=DIRECTION('',(0.,-1.,0.));
#65450=DIRECTION('center_axis',(0.,0.,1.));
#65451=DIRECTION('ref_axis',(1.,0.,0.));
#65452=DIRECTION('center_axis',(0.,-1.,0.));
#65453=DIRECTION('ref_axis',(1.,0.,0.));
#65454=DIRECTION('',(-1.,0.,0.));
#65455=DIRECTION('',(0.,0.,1.));
#65456=DIRECTION('',(1.,0.,0.));
#65457=DIRECTION('',(0.,0.,1.));
#65458=DIRECTION('center_axis',(-1.,0.,0.));
#65459=DIRECTION('ref_axis',(0.,-1.,0.));
#65460=DIRECTION('',(0.,1.,0.));
#65461=DIRECTION('',(0.,-1.,0.));
#65462=DIRECTION('',(0.,0.,1.));
#65463=DIRECTION('center_axis',(0.,1.,0.));
#65464=DIRECTION('ref_axis',(-1.,0.,0.));
#65465=DIRECTION('',(1.,0.,0.));
#65466=DIRECTION('',(-1.,0.,0.));
#65467=DIRECTION('',(0.,0.,1.));
#65468=DIRECTION('center_axis',(1.,0.,0.));
#65469=DIRECTION('ref_axis',(0.,1.,0.));
#65470=DIRECTION('',(0.,-1.,0.));
#65471=DIRECTION('',(0.,1.,0.));
#65472=DIRECTION('center_axis',(0.,0.,1.));
#65473=DIRECTION('ref_axis',(1.,0.,0.));
#65474=DIRECTION('center_axis',(0.,0.,1.));
#65475=DIRECTION('ref_axis',(1.,0.,0.));
#65476=DIRECTION('center_axis',(0.,0.,1.));
#65477=DIRECTION('ref_axis',(1.,0.,0.));
#65478=DIRECTION('',(0.707106781186546,8.65956056235491E-17,-0.707106781186549));
#65479=DIRECTION('center_axis',(0.,0.,-1.));
#65480=DIRECTION('ref_axis',(1.,0.,0.));
#65481=DIRECTION('center_axis',(0.,0.,1.));
#65482=DIRECTION('ref_axis',(1.,0.,0.));
#65483=DIRECTION('center_axis',(0.,0.,1.));
#65484=DIRECTION('ref_axis',(1.,0.,0.));
#65485=DIRECTION('',(0.,0.,1.));
#65486=DIRECTION('center_axis',(0.,0.,1.));
#65487=DIRECTION('ref_axis',(1.,0.,0.));
#65488=DIRECTION('',(0.,1.,0.));
#65489=DIRECTION('center_axis',(0.,0.,-1.));
#65490=DIRECTION('ref_axis',(-1.,0.,0.));
#65491=DIRECTION('',(-1.,0.,0.));
#65492=DIRECTION('center_axis',(0.,0.,-1.));
#65493=DIRECTION('ref_axis',(0.,-1.,0.));
#65494=DIRECTION('',(0.,-1.,0.));
#65495=DIRECTION('center_axis',(0.,0.,-1.));
#65496=DIRECTION('ref_axis',(1.,0.,0.));
#65497=DIRECTION('',(1.,0.,0.));
#65498=DIRECTION('center_axis',(0.,0.,-1.));
#65499=DIRECTION('ref_axis',(0.,1.,0.));
#65500=DIRECTION('center_axis',(0.,0.,1.));
#65501=DIRECTION('ref_axis',(1.,0.,0.));
#65502=DIRECTION('center_axis',(0.,0.,-1.));
#65503=DIRECTION('ref_axis',(1.,0.,0.));
#65504=DIRECTION('center_axis',(0.,0.,-1.));
#65505=DIRECTION('ref_axis',(1.,0.,0.));
#65506=DIRECTION('center_axis',(0.,0.,-1.));
#65507=DIRECTION('ref_axis',(1.,0.,0.));
#65508=DIRECTION('center_axis',(0.,0.,-1.));
#65509=DIRECTION('ref_axis',(1.,0.,0.));
#65510=DIRECTION('center_axis',(0.,0.,-1.));
#65511=DIRECTION('ref_axis',(1.,0.,0.));
#65512=DIRECTION('center_axis',(0.,0.,-1.));
#65513=DIRECTION('ref_axis',(1.,0.,0.));
#65514=DIRECTION('center_axis',(0.,0.,-1.));
#65515=DIRECTION('ref_axis',(1.,0.,0.));
#65516=DIRECTION('center_axis',(0.,0.,1.));
#65517=DIRECTION('ref_axis',(1.,0.,0.));
#65518=DIRECTION('center_axis',(0.,0.,1.));
#65519=DIRECTION('ref_axis',(1.,0.,0.));
#65520=DIRECTION('center_axis',(0.,0.,-1.));
#65521=DIRECTION('ref_axis',(1.,0.,0.));
#65522=DIRECTION('center_axis',(0.,0.,-1.));
#65523=DIRECTION('ref_axis',(1.,0.,0.));
#65524=DIRECTION('',(0.707106781186546,-8.65956056235491E-17,0.707106781186549));
#65525=DIRECTION('center_axis',(0.,0.,1.));
#65526=DIRECTION('ref_axis',(1.,0.,0.));
#65527=DIRECTION('center_axis',(0.,0.,1.));
#65528=DIRECTION('ref_axis',(0.,-1.,0.));
#65529=DIRECTION('',(1.,0.,0.));
#65530=DIRECTION('center_axis',(0.,0.,1.));
#65531=DIRECTION('ref_axis',(-1.,0.,0.));
#65532=DIRECTION('',(0.,-1.,0.));
#65533=DIRECTION('center_axis',(0.,0.,1.));
#65534=DIRECTION('ref_axis',(0.,1.,0.));
#65535=DIRECTION('',(-1.,0.,0.));
#65536=DIRECTION('center_axis',(0.,0.,1.));
#65537=DIRECTION('ref_axis',(1.,0.,0.));
#65538=DIRECTION('',(0.,1.,0.));
#65539=DIRECTION('center_axis',(0.,0.,-1.));
#65540=DIRECTION('ref_axis',(1.,0.,0.));
#65541=DIRECTION('center_axis',(0.,0.,-1.));
#65542=DIRECTION('ref_axis',(1.,0.,0.));
#65543=DIRECTION('center_axis',(0.,0.,-1.));
#65544=DIRECTION('ref_axis',(1.,0.,0.));
#65545=DIRECTION('center_axis',(0.,0.,1.));
#65546=DIRECTION('ref_axis',(1.,0.,0.));
#65547=DIRECTION('',(0.707106781186546,8.65956056235491E-17,-0.707106781186549));
#65548=DIRECTION('center_axis',(0.,0.,-1.));
#65549=DIRECTION('ref_axis',(1.,0.,0.));
#65550=DIRECTION('center_axis',(0.,0.,1.));
#65551=DIRECTION('ref_axis',(1.,0.,0.));
#65552=DIRECTION('center_axis',(0.,0.,1.));
#65553=DIRECTION('ref_axis',(1.,0.,0.));
#65554=DIRECTION('',(0.,0.,1.));
#65555=DIRECTION('center_axis',(0.,0.,-1.));
#65556=DIRECTION('ref_axis',(1.,0.,0.));
#65557=DIRECTION('',(0.707106781186546,-8.65956056235491E-17,0.707106781186549));
#65558=DIRECTION('center_axis',(0.,0.,1.));
#65559=DIRECTION('ref_axis',(1.,0.,0.));
#65560=DIRECTION('',(0.707106781186546,8.65956056235491E-17,-0.707106781186549));
#65561=DIRECTION('center_axis',(0.,0.,-1.));
#65562=DIRECTION('ref_axis',(1.,0.,0.));
#65563=DIRECTION('center_axis',(0.,0.,1.));
#65564=DIRECTION('ref_axis',(1.,0.,0.));
#65565=DIRECTION('center_axis',(0.,0.,1.));
#65566=DIRECTION('ref_axis',(1.,0.,0.));
#65567=DIRECTION('',(0.,0.,1.));
#65568=DIRECTION('center_axis',(0.,0.,-1.));
#65569=DIRECTION('ref_axis',(1.,0.,0.));
#65570=DIRECTION('',(0.707106781186546,-8.65956056235491E-17,0.707106781186549));
#65571=DIRECTION('center_axis',(0.,0.,1.));
#65572=DIRECTION('ref_axis',(1.,0.,0.));
#65573=DIRECTION('',(0.707106781186546,8.65956056235491E-17,-0.707106781186549));
#65574=DIRECTION('center_axis',(0.,0.,-1.));
#65575=DIRECTION('ref_axis',(1.,0.,0.));
#65576=DIRECTION('center_axis',(0.,0.,1.));
#65577=DIRECTION('ref_axis',(1.,0.,0.));
#65578=DIRECTION('center_axis',(0.,0.,1.));
#65579=DIRECTION('ref_axis',(1.,0.,0.));
#65580=DIRECTION('',(0.,0.,1.));
#65581=DIRECTION('center_axis',(0.,0.,-1.));
#65582=DIRECTION('ref_axis',(1.,0.,0.));
#65583=DIRECTION('',(0.707106781186546,-8.65956056235491E-17,0.707106781186549));
#65584=DIRECTION('center_axis',(0.,0.,1.));
#65585=DIRECTION('ref_axis',(1.,0.,0.));
#65586=DIRECTION('center_axis',(0.,0.,-1.));
#65587=DIRECTION('ref_axis',(1.,0.,0.));
#65588=DIRECTION('',(0.857167300702112,-1.04972719113862E-16,-0.515038074910054));
#65589=DIRECTION('center_axis',(0.,0.,-1.));
#65590=DIRECTION('ref_axis',(1.,0.,0.));
#65591=DIRECTION('',(0.,0.,-1.));
#65592=DIRECTION('center_axis',(0.,0.,1.));
#65593=DIRECTION('ref_axis',(1.,0.,0.));
#65594=DIRECTION('center_axis',(0.,0.,-1.));
#65595=DIRECTION('ref_axis',(1.,0.,0.));
#65596=DIRECTION('',(0.857167300702112,-1.04972719113862E-16,-0.515038074910054));
#65597=DIRECTION('center_axis',(0.,0.,-1.));
#65598=DIRECTION('ref_axis',(1.,0.,0.));
#65599=DIRECTION('',(0.,0.,-1.));
#65600=DIRECTION('center_axis',(0.,0.,1.));
#65601=DIRECTION('ref_axis',(1.,0.,0.));
#65602=DIRECTION('center_axis',(0.,0.,-1.));
#65603=DIRECTION('ref_axis',(1.,0.,0.));
#65604=DIRECTION('',(0.857167300702112,-1.04972719113862E-16,-0.515038074910054));
#65605=DIRECTION('center_axis',(0.,0.,1.));
#65606=DIRECTION('ref_axis',(1.,0.,0.));
#65607=DIRECTION('',(0.707106781186548,-8.65956056235493E-17,-0.707106781186548));
#65608=DIRECTION('center_axis',(0.,0.,-1.));
#65609=DIRECTION('ref_axis',(1.,0.,0.));
#65610=DIRECTION('center_axis',(0.,0.,-1.));
#65611=DIRECTION('ref_axis',(1.,0.,0.));
#65612=DIRECTION('',(0.,0.,-1.));
#65613=DIRECTION('center_axis',(0.,0.,1.));
#65614=DIRECTION('ref_axis',(1.,0.,0.));
#65615=DIRECTION('center_axis',(0.,0.,-1.));
#65616=DIRECTION('ref_axis',(1.,0.,0.));
#65617=DIRECTION('',(0.857167300702112,-1.04972719113862E-16,-0.515038074910054));
#65618=DIRECTION('center_axis',(0.,0.,1.));
#65619=DIRECTION('ref_axis',(1.,0.,0.));
#65620=DIRECTION('',(0.707106781186548,-8.65956056235493E-17,-0.707106781186548));
#65621=DIRECTION('center_axis',(0.,0.,-1.));
#65622=DIRECTION('ref_axis',(1.,0.,0.));
#65623=DIRECTION('center_axis',(0.,0.,-1.));
#65624=DIRECTION('ref_axis',(1.,0.,0.));
#65625=DIRECTION('',(0.,0.,-1.));
#65626=DIRECTION('center_axis',(0.,0.,1.));
#65627=DIRECTION('ref_axis',(1.,0.,0.));
#65628=DIRECTION('center_axis',(0.,0.,-1.));
#65629=DIRECTION('ref_axis',(1.,0.,0.));
#65630=DIRECTION('',(0.857167300702112,-1.04972719113862E-16,-0.515038074910054));
#65631=DIRECTION('center_axis',(0.,0.,1.));
#65632=DIRECTION('ref_axis',(1.,0.,0.));
#65633=DIRECTION('',(0.707106781186548,-8.65956056235493E-17,-0.707106781186548));
#65634=DIRECTION('center_axis',(0.,0.,-1.));
#65635=DIRECTION('ref_axis',(1.,0.,0.));
#65636=DIRECTION('center_axis',(0.,0.,-1.));
#65637=DIRECTION('ref_axis',(1.,0.,0.));
#65638=DIRECTION('',(0.,0.,-1.));
#65639=DIRECTION('center_axis',(0.,0.,1.));
#65640=DIRECTION('ref_axis',(1.,0.,0.));
#65641=DIRECTION('center_axis',(0.,0.,-1.));
#65642=DIRECTION('ref_axis',(1.,0.,0.));
#65643=DIRECTION('',(0.857167300702112,-1.04972719113862E-16,-0.515038074910054));
#65644=DIRECTION('center_axis',(0.,0.,1.));
#65645=DIRECTION('ref_axis',(1.,0.,0.));
#65646=DIRECTION('',(0.707106781186548,-8.65956056235493E-17,-0.707106781186548));
#65647=DIRECTION('center_axis',(0.,0.,-1.));
#65648=DIRECTION('ref_axis',(1.,0.,0.));
#65649=DIRECTION('center_axis',(0.,0.,-1.));
#65650=DIRECTION('ref_axis',(1.,0.,0.));
#65651=DIRECTION('',(0.,0.,-1.));
#65652=DIRECTION('center_axis',(0.,0.,1.));
#65653=DIRECTION('ref_axis',(1.,0.,0.));
#65654=DIRECTION('center_axis',(0.,0.,1.));
#65655=DIRECTION('ref_axis',(1.,0.,0.));
#65656=DIRECTION('',(0.,0.,1.));
#65657=DIRECTION('center_axis',(0.,0.,1.));
#65658=DIRECTION('ref_axis',(1.,0.,0.));
#65659=DIRECTION('center_axis',(0.,0.,1.));
#65660=DIRECTION('ref_axis',(0.,-1.,0.));
#65661=DIRECTION('',(0.707106781186552,0.,0.707106781186543));
#65662=DIRECTION('center_axis',(0.,0.,-1.));
#65663=DIRECTION('ref_axis',(0.,-1.,0.));
#65664=DIRECTION('',(0.,0.707106781186546,-0.707106781186549));
#65665=DIRECTION('center_axis',(0.707106781186543,0.,-0.707106781186552));
#65666=DIRECTION('ref_axis',(-0.707106781186552,0.,-0.707106781186543));
#65667=DIRECTION('',(0.707106781186552,0.,0.707106781186543));
#65668=DIRECTION('',(0.,-1.,0.));
#65669=DIRECTION('center_axis',(0.,0.,1.));
#65670=DIRECTION('ref_axis',(1.,0.,0.));
#65671=DIRECTION('',(0.,0.707106781186546,0.707106781186549));
#65672=DIRECTION('center_axis',(0.,0.,-1.));
#65673=DIRECTION('ref_axis',(1.,0.,0.));
#65674=DIRECTION('center_axis',(0.,0.707106781186549,-0.707106781186546));
#65675=DIRECTION('ref_axis',(-1.,0.,0.));
#65676=DIRECTION('',(0.,0.707106781186546,0.707106781186549));
#65677=DIRECTION('',(1.,0.,0.));
#65678=DIRECTION('center_axis',(0.,0.,1.));
#65679=DIRECTION('ref_axis',(0.,1.,0.));
#65680=DIRECTION('',(-0.707106781186552,0.,0.707106781186543));
#65681=DIRECTION('center_axis',(0.,0.,-1.));
#65682=DIRECTION('ref_axis',(0.,1.,0.));
#65683=DIRECTION('center_axis',(-0.707106781186543,0.,-0.707106781186552));
#65684=DIRECTION('ref_axis',(-0.707106781186552,0.,0.707106781186543));
#65685=DIRECTION('',(-0.707106781186552,0.,0.707106781186543));
#65686=DIRECTION('',(0.,1.,0.));
#65687=DIRECTION('center_axis',(0.,0.,1.));
#65688=DIRECTION('ref_axis',(-1.,0.,0.));
#65689=DIRECTION('',(0.,-0.707106781186546,0.707106781186549));
#65690=DIRECTION('center_axis',(0.,0.,-1.));
#65691=DIRECTION('ref_axis',(-1.,0.,0.));
#65692=DIRECTION('center_axis',(0.,-0.707106781186549,-0.707106781186546));
#65693=DIRECTION('ref_axis',(-1.,0.,0.));
#65694=DIRECTION('',(-1.,0.,0.));
#65695=DIRECTION('center_axis',(-1.,0.,0.));
#65696=DIRECTION('ref_axis',(0.,-1.,0.));
#65697=DIRECTION('',(0.,0.,1.));
#65698=DIRECTION('',(0.,-1.,0.));
#65699=DIRECTION('',(0.,0.,1.));
#65700=DIRECTION('center_axis',(0.,0.,1.));
#65701=DIRECTION('ref_axis',(-1.,0.,0.));
#65702=DIRECTION('',(0.,0.,1.));
#65703=DIRECTION('center_axis',(0.,0.,1.));
#65704=DIRECTION('ref_axis',(-1.,0.,0.));
#65705=DIRECTION('center_axis',(0.,-1.,0.));
#65706=DIRECTION('ref_axis',(1.,0.,0.));
#65707=DIRECTION('',(0.,0.,1.));
#65708=DIRECTION('',(1.,0.,0.));
#65709=DIRECTION('center_axis',(0.,0.,1.));
#65710=DIRECTION('ref_axis',(0.,-1.,0.));
#65711=DIRECTION('',(0.,0.,1.));
#65712=DIRECTION('center_axis',(0.,0.,1.));
#65713=DIRECTION('ref_axis',(0.,-1.,0.));
#65714=DIRECTION('center_axis',(-0.707106781186549,0.,0.707106781186546));
#65715=DIRECTION('ref_axis',(0.707106781186546,0.,0.707106781186549));
#65716=DIRECTION('',(0.707106781186546,0.,0.707106781186549));
#65717=DIRECTION('',(-0.707106781186546,0.,-0.707106781186549));
#65718=DIRECTION('center_axis',(0.,0.,-1.));
#65719=DIRECTION('ref_axis',(-1.,0.,0.));
#65720=DIRECTION('',(0.,0.707106781186546,0.707106781186549));
#65721=DIRECTION('center_axis',(0.,-0.707106781186549,0.707106781186546));
#65722=DIRECTION('ref_axis',(1.,0.,0.));
#65723=DIRECTION('',(0.,0.707106781186546,0.707106781186549));
#65724=DIRECTION('center_axis',(0.,0.,-1.));
#65725=DIRECTION('ref_axis',(0.,-1.,0.));
#65726=DIRECTION('',(-0.707106781186546,0.,0.707106781186549));
#65727=DIRECTION('center_axis',(0.707106781186549,0.,0.707106781186546));
#65728=DIRECTION('ref_axis',(0.707106781186546,0.,-0.707106781186549));
#65729=DIRECTION('',(-0.707106781186546,0.,0.707106781186549));
#65730=DIRECTION('',(0.,1.,0.));
#65731=DIRECTION('center_axis',(0.,0.,-1.));
#65732=DIRECTION('ref_axis',(1.,0.,0.));
#65733=DIRECTION('',(0.,-0.707106781186546,0.707106781186549));
#65734=DIRECTION('center_axis',(0.,0.,1.));
#65735=DIRECTION('ref_axis',(1.,0.,0.));
#65736=DIRECTION('center_axis',(0.,0.707106781186549,0.707106781186546));
#65737=DIRECTION('ref_axis',(1.,0.,0.));
#65738=DIRECTION('',(0.,-0.707106781186546,0.707106781186549));
#65739=DIRECTION('',(-1.,0.,0.));
#65740=DIRECTION('center_axis',(0.,0.,-1.));
#65741=DIRECTION('ref_axis',(0.,1.,0.));
#65742=DIRECTION('center_axis',(0.,0.,1.));
#65743=DIRECTION('ref_axis',(0.,1.,0.));
#65744=DIRECTION('center_axis',(0.,0.,1.));
#65745=DIRECTION('ref_axis',(0.,1.,0.));
#65746=DIRECTION('',(0.,0.,1.));
#65747=DIRECTION('center_axis',(0.,1.,0.));
#65748=DIRECTION('ref_axis',(-1.,0.,0.));
#65749=DIRECTION('',(0.,0.,1.));
#65750=DIRECTION('center_axis',(0.,0.,1.));
#65751=DIRECTION('ref_axis',(1.,0.,0.));
#65752=DIRECTION('',(0.,0.,1.));
#65753=DIRECTION('center_axis',(1.,0.,0.));
#65754=DIRECTION('ref_axis',(0.,1.,0.));
#65755=DIRECTION('axis',(0.,0.,1.));
#65756=DIRECTION('refdir',(1.,0.,0.));
#65757=DIRECTION('center_axis',(1.,0.,0.));
#65758=DIRECTION('ref_axis',(0.,1.,0.));
#65759=DIRECTION('center_axis',(1.,0.,0.));
#65760=DIRECTION('ref_axis',(0.,0.,-1.));
#65761=DIRECTION('',(-1.,0.,0.));
#65762=DIRECTION('center_axis',(1.,0.,0.));
#65763=DIRECTION('ref_axis',(0.,0.,-1.));
#65764=DIRECTION('center_axis',(-1.,0.,0.));
#65765=DIRECTION('ref_axis',(0.,1.,0.));
#65766=DIRECTION('',(-0.707106781186548,-0.707106781186547,-8.65956056235493E-17));
#65767=DIRECTION('center_axis',(1.,0.,0.));
#65768=DIRECTION('ref_axis',(0.,0.,-1.));
#65769=DIRECTION('center_axis',(-1.,0.,0.));
#65770=DIRECTION('ref_axis',(0.,0.,1.));
#65771=DIRECTION('center_axis',(1.,0.,0.));
#65772=DIRECTION('ref_axis',(0.,0.,-1.));
#65773=DIRECTION('center_axis',(1.,0.,0.));
#65774=DIRECTION('ref_axis',(0.,1.,0.));
#65775=DIRECTION('center_axis',(1.,0.,0.));
#65776=DIRECTION('ref_axis',(0.,0.,-1.));
#65777=DIRECTION('',(-0.707106781186549,0.707106781186546,8.65956056235492E-17));
#65778=DIRECTION('center_axis',(1.,0.,0.));
#65779=DIRECTION('ref_axis',(0.,1.,0.));
#65780=DIRECTION('center_axis',(1.,0.,0.));
#65781=DIRECTION('ref_axis',(0.,0.,-1.));
#65782=DIRECTION('',(-1.,0.,0.));
#65783=DIRECTION('center_axis',(-1.,0.,0.));
#65784=DIRECTION('ref_axis',(0.,1.,0.));
#65785=DIRECTION('center_axis',(1.,0.,0.));
#65786=DIRECTION('ref_axis',(0.,0.,-1.));
#65787=DIRECTION('',(-0.707106781186549,-0.707106781186546,-8.65956056235492E-17));
#65788=DIRECTION('center_axis',(1.,0.,0.));
#65789=DIRECTION('ref_axis',(0.,0.,-1.));
#65790=DIRECTION('center_axis',(1.,0.,0.));
#65791=DIRECTION('ref_axis',(0.,0.,-1.));
#65792=DIRECTION('center_axis',(1.,0.,0.));
#65793=DIRECTION('ref_axis',(0.,1.,0.));
#65794=DIRECTION('',(-0.707106781186548,0.707106781186548,8.65956056235493E-17));
#65795=DIRECTION('axis',(0.,0.,1.));
#65796=DIRECTION('refdir',(1.,0.,0.));
#65797=DIRECTION('center_axis',(1.,0.,0.));
#65798=DIRECTION('ref_axis',(0.,1.,0.));
#65799=DIRECTION('',(-1.,0.,0.));
#65800=DIRECTION('center_axis',(1.,0.,0.));
#65801=DIRECTION('ref_axis',(0.,1.,0.));
#65802=DIRECTION('center_axis',(1.,0.,0.));
#65803=DIRECTION('ref_axis',(0.,1.,0.));
#65804=DIRECTION('',(-1.,0.,0.));
#65805=DIRECTION('center_axis',(1.,0.,0.));
#65806=DIRECTION('ref_axis',(0.,1.,0.));
#65807=DIRECTION('',(-1.,0.,0.));
#65808=DIRECTION('center_axis',(1.,0.,0.));
#65809=DIRECTION('ref_axis',(0.,1.,0.));
#65810=DIRECTION('',(-1.,0.,0.));
#65811=DIRECTION('center_axis',(1.,0.,0.));
#65812=DIRECTION('ref_axis',(0.,1.,0.));
#65813=DIRECTION('',(-1.,0.,0.));
#65814=DIRECTION('center_axis',(1.,0.,0.));
#65815=DIRECTION('ref_axis',(0.,1.,0.));
#65816=DIRECTION('',(-1.,0.,0.));
#65817=DIRECTION('center_axis',(1.,0.,0.));
#65818=DIRECTION('ref_axis',(0.,1.,0.));
#65819=DIRECTION('',(-1.,0.,0.));
#65820=DIRECTION('center_axis',(1.,0.,0.));
#65821=DIRECTION('ref_axis',(0.,1.,0.));
#65822=DIRECTION('',(-1.,0.,0.));
#65823=DIRECTION('center_axis',(1.,0.,0.));
#65824=DIRECTION('ref_axis',(0.,1.,0.));
#65825=DIRECTION('',(-1.,0.,0.));
#65826=DIRECTION('center_axis',(1.,0.,0.));
#65827=DIRECTION('ref_axis',(0.,1.,0.));
#65828=DIRECTION('',(-1.,0.,0.));
#65829=DIRECTION('center_axis',(1.,0.,0.));
#65830=DIRECTION('ref_axis',(0.,1.,0.));
#65831=DIRECTION('',(-1.,0.,0.));
#65832=DIRECTION('center_axis',(1.,0.,0.));
#65833=DIRECTION('ref_axis',(0.,1.,0.));
#65834=DIRECTION('',(-1.,0.,0.));
#65835=DIRECTION('center_axis',(1.,0.,0.));
#65836=DIRECTION('ref_axis',(0.,1.,0.));
#65837=DIRECTION('',(-1.,0.,0.));
#65838=DIRECTION('center_axis',(1.,0.,0.));
#65839=DIRECTION('ref_axis',(0.,1.,0.));
#65840=DIRECTION('',(-1.,0.,0.));
#65841=DIRECTION('center_axis',(1.,0.,0.));
#65842=DIRECTION('ref_axis',(0.,1.,0.));
#65843=DIRECTION('',(-1.,0.,0.));
#65844=DIRECTION('center_axis',(1.,0.,0.));
#65845=DIRECTION('ref_axis',(0.,1.,0.));
#65846=DIRECTION('',(-1.,0.,0.));
#65847=DIRECTION('center_axis',(1.,0.,0.));
#65848=DIRECTION('ref_axis',(0.,-0.915339016570139,-0.402684100436572));
#65849=DIRECTION('',(1.,0.,0.));
#65850=DIRECTION('center_axis',(1.,0.,0.));
#65851=DIRECTION('ref_axis',(0.,1.,9.48637278455213E-14));
#65852=DIRECTION('center_axis',(1.,0.,0.));
#65853=DIRECTION('ref_axis',(0.,1.,9.48637278455213E-14));
#65854=DIRECTION('',(1.,0.,0.));
#65855=DIRECTION('center_axis',(1.,0.,0.));
#65856=DIRECTION('ref_axis',(0.,1.,9.48637278455213E-14));
#65857=DIRECTION('center_axis',(1.,0.,0.));
#65858=DIRECTION('ref_axis',(0.,1.,9.48637278455213E-14));
#65859=DIRECTION('',(1.,0.,0.));
#65860=DIRECTION('center_axis',(1.,0.,0.));
#65861=DIRECTION('ref_axis',(0.,1.,9.48637278455213E-14));
#65862=DIRECTION('',(1.,0.,0.));
#65863=DIRECTION('center_axis',(1.,0.,0.));
#65864=DIRECTION('ref_axis',(0.,1.,9.48637278455213E-14));
#65865=DIRECTION('',(1.,0.,0.));
#65866=DIRECTION('center_axis',(1.,0.,0.));
#65867=DIRECTION('ref_axis',(0.,1.,9.48637278455213E-14));
#65868=DIRECTION('',(1.,0.,0.));
#65869=DIRECTION('center_axis',(1.,0.,0.));
#65870=DIRECTION('ref_axis',(0.,1.,9.48637278455213E-14));
#65871=DIRECTION('',(1.,0.,0.));
#65872=DIRECTION('center_axis',(1.,0.,0.));
#65873=DIRECTION('ref_axis',(0.,1.,9.48637278455213E-14));
#65874=DIRECTION('',(1.,0.,0.));
#65875=DIRECTION('center_axis',(1.,0.,0.));
#65876=DIRECTION('ref_axis',(0.,1.,9.48637278455213E-14));
#65877=DIRECTION('',(1.,0.,0.));
#65878=DIRECTION('center_axis',(1.,0.,0.));
#65879=DIRECTION('ref_axis',(0.,1.,9.48637278455213E-14));
#65880=DIRECTION('',(1.,0.,0.));
#65881=DIRECTION('center_axis',(1.,0.,0.));
#65882=DIRECTION('ref_axis',(0.,1.,9.48637278455213E-14));
#65883=DIRECTION('',(1.,0.,0.));
#65884=DIRECTION('center_axis',(1.,0.,0.));
#65885=DIRECTION('ref_axis',(0.,1.,9.48637278455213E-14));
#65886=DIRECTION('',(1.,0.,0.));
#65887=DIRECTION('center_axis',(1.,0.,0.));
#65888=DIRECTION('ref_axis',(0.,1.,9.48637278455213E-14));
#65889=DIRECTION('',(1.,0.,0.));
#65890=DIRECTION('center_axis',(1.,0.,0.));
#65891=DIRECTION('ref_axis',(0.,1.,9.48637278455213E-14));
#65892=DIRECTION('',(1.,0.,0.));
#65893=DIRECTION('center_axis',(1.,0.,0.));
#65894=DIRECTION('ref_axis',(0.,1.,9.48637278455213E-14));
#65895=DIRECTION('',(1.,0.,0.));
#65896=DIRECTION('center_axis',(1.,0.,0.));
#65897=DIRECTION('ref_axis',(0.,1.,9.48637278455213E-14));
#65898=DIRECTION('',(1.,0.,0.));
#65899=DIRECTION('center_axis',(1.,0.,0.));
#65900=DIRECTION('ref_axis',(0.,0.,-1.));
#65901=DIRECTION('center_axis',(1.,0.,0.));
#65902=DIRECTION('ref_axis',(0.,1.,0.));
#65903=DIRECTION('center_axis',(1.,0.,0.));
#65904=DIRECTION('ref_axis',(0.,1.,0.));
#65905=DIRECTION('center_axis',(1.,0.,0.));
#65906=DIRECTION('ref_axis',(0.,0.,-1.));
#65907=DIRECTION('center_axis',(1.,0.,0.));
#65908=DIRECTION('ref_axis',(0.,1.,0.));
#65909=DIRECTION('center_axis',(1.,0.,0.));
#65910=DIRECTION('ref_axis',(0.,1.,0.));
#65911=DIRECTION('center_axis',(-1.,0.,0.));
#65912=DIRECTION('ref_axis',(0.,1.,9.48637278455213E-14));
#65913=DIRECTION('center_axis',(1.,0.,0.));
#65914=DIRECTION('ref_axis',(0.,1.,9.48637278455213E-14));
#65915=DIRECTION('center_axis',(1.,0.,0.));
#65916=DIRECTION('ref_axis',(0.,0.,-1.));
#65917=DIRECTION('center_axis',(0.,-1.,-1.22464679914735E-16));
#65918=DIRECTION('ref_axis',(0.,-1.22464679914735E-16,1.));
#65919=DIRECTION('center_axis',(-1.,0.,0.));
#65920=DIRECTION('ref_axis',(0.,1.,0.));
#65921=DIRECTION('center_axis',(1.,0.,0.));
#65922=DIRECTION('ref_axis',(0.,1.,0.));
#65923=DIRECTION('center_axis',(1.,0.,0.));
#65924=DIRECTION('ref_axis',(0.,0.326715465838084,-0.945122745669685));
#65925=DIRECTION('center_axis',(-1.,0.,0.));
#65926=DIRECTION('ref_axis',(0.,0.,1.));
#65927=DIRECTION('center_axis',(1.,0.,0.));
#65928=DIRECTION('ref_axis',(0.,0.,-1.));
#65929=DIRECTION('center_axis',(0.,-0.601539426890005,-0.798843112192153));
#65930=DIRECTION('ref_axis',(0.,0.798843112192152,-0.601539426890005));
#65931=DIRECTION('',(1.,0.,0.));
#65932=DIRECTION('',(0.,-0.798843112192152,0.601539426890005));
#65933=DIRECTION('',(1.,0.,0.));
#65934=DIRECTION('',(0.,0.798843112192152,-0.601539426890005));
#65935=DIRECTION('center_axis',(1.,0.,0.));
#65936=DIRECTION('ref_axis',(0.,-0.17364817766693,-0.984807753012208));
#65937=DIRECTION('center_axis',(1.,0.,0.));
#65938=DIRECTION('ref_axis',(0.,0.,-1.));
#65939=DIRECTION('',(0.,-0.956405578693576,-0.292041724833639));
#65940=DIRECTION('center_axis',(0.,-0.292041724833639,0.956405578693576));
#65941=DIRECTION('ref_axis',(0.,-0.956405578693576,-0.292041724833639));
#65942=DIRECTION('',(-1.,0.,0.));
#65943=DIRECTION('',(0.,0.956405578693576,0.292041724833639));
#65944=DIRECTION('center_axis',(1.,0.,0.));
#65945=DIRECTION('ref_axis',(0.,-0.17364817766693,-0.984807753012208));
#65946=DIRECTION('center_axis',(-1.,0.,0.));
#65947=DIRECTION('ref_axis',(0.,1.,0.));
#65948=DIRECTION('center_axis',(0.,-0.731118342017745,-0.682250665052973));
#65949=DIRECTION('ref_axis',(0.,0.682250665052973,-0.731118342017745));
#65950=DIRECTION('',(1.,0.,0.));
#65951=DIRECTION('',(0.,-0.682250665052973,0.731118342017745));
#65952=DIRECTION('',(1.,0.,0.));
#65953=DIRECTION('',(0.,0.682250665052973,-0.731118342017745));
#65954=DIRECTION('center_axis',(1.,0.,0.));
#65955=DIRECTION('ref_axis',(0.,-0.342020143325669,-0.939692620785908));
#65956=DIRECTION('center_axis',(1.,0.,0.));
#65957=DIRECTION('ref_axis',(0.,0.,-1.));
#65958=DIRECTION('',(0.,-0.992588142241629,-0.1215268689686));
#65959=DIRECTION('center_axis',(0.,-0.1215268689686,0.992588142241629));
#65960=DIRECTION('ref_axis',(0.,-0.992588142241629,-0.1215268689686));
#65961=DIRECTION('',(-1.,0.,0.));
#65962=DIRECTION('',(0.,0.992588142241629,0.1215268689686));
#65963=DIRECTION('center_axis',(1.,0.,0.));
#65964=DIRECTION('ref_axis',(0.,-0.342020143325669,-0.939692620785908));
#65965=DIRECTION('center_axis',(-1.,0.,0.));
#65966=DIRECTION('ref_axis',(0.,1.,0.));
#65967=DIRECTION('center_axis',(0.,-0.838482596287006,-0.544928376691655));
#65968=DIRECTION('ref_axis',(0.,0.544928376691655,-0.838482596287006));
#65969=DIRECTION('',(1.,0.,0.));
#65970=DIRECTION('',(0.,-0.544928376691655,0.838482596287006));
#65971=DIRECTION('',(1.,0.,0.));
#65972=DIRECTION('',(0.,0.544928376691655,-0.838482596287006));
#65973=DIRECTION('center_axis',(1.,0.,0.));
#65974=DIRECTION('ref_axis',(0.,-0.5,-0.866025403784438));
#65975=DIRECTION('center_axis',(1.,0.,0.));
#65976=DIRECTION('ref_axis',(0.,0.,-1.));
#65977=DIRECTION('',(0.,-0.998611417361506,0.052680519314487));
#65978=DIRECTION('center_axis',(0.,0.052680519314487,0.998611417361506));
#65979=DIRECTION('ref_axis',(0.,-0.998611417361506,0.052680519314487));
#65980=DIRECTION('',(-1.,0.,0.));
#65981=DIRECTION('',(0.,0.998611417361506,-0.052680519314487));
#65982=DIRECTION('center_axis',(1.,0.,0.));
#65983=DIRECTION('ref_axis',(0.,-0.5,-0.866025403784438));
#65984=DIRECTION('center_axis',(-1.,0.,0.));
#65985=DIRECTION('ref_axis',(0.,1.,0.));
#65986=DIRECTION('center_axis',(0.,-0.920369981160753,-0.391048715351624));
#65987=DIRECTION('ref_axis',(0.,0.391048715351624,-0.920369981160753));
#65988=DIRECTION('',(1.,0.,0.));
#65989=DIRECTION('',(0.,-0.391048715351624,0.920369981160753));
#65990=DIRECTION('',(1.,0.,0.));
#65991=DIRECTION('',(0.,0.391048715351624,-0.920369981160753));
#65992=DIRECTION('center_axis',(1.,0.,0.));
#65993=DIRECTION('ref_axis',(0.,-0.64278760968654,-0.766044443118978));
#65994=DIRECTION('center_axis',(1.,0.,0.));
#65995=DIRECTION('ref_axis',(0.,0.,-1.));
#65996=DIRECTION('',(0.,-0.974292389886613,0.225287236675832));
#65997=DIRECTION('center_axis',(0.,0.225287236675832,0.974292389886613));
#65998=DIRECTION('ref_axis',(0.,-0.974292389886613,0.225287236675832));
#65999=DIRECTION('',(-1.,0.,0.));
#66000=DIRECTION('',(0.,0.974292389886613,-0.225287236675832));
#66001=DIRECTION('center_axis',(1.,0.,0.));
#66002=DIRECTION('ref_axis',(0.,-0.64278760968654,-0.766044443118978));
#66003=DIRECTION('center_axis',(-1.,0.,0.));
#66004=DIRECTION('ref_axis',(0.,1.,0.));
#66005=DIRECTION('center_axis',(0.,-0.974292389886613,-0.225287236675831));
#66006=DIRECTION('ref_axis',(0.,0.225287236675831,-0.974292389886613));
#66007=DIRECTION('',(1.,0.,0.));
#66008=DIRECTION('',(0.,-0.225287236675831,0.974292389886613));
#66009=DIRECTION('',(1.,0.,0.));
#66010=DIRECTION('',(0.,0.225287236675831,-0.974292389886613));
#66011=DIRECTION('center_axis',(1.,0.,0.));
#66012=DIRECTION('ref_axis',(0.,-0.766044443118978,-0.642787609686539));
#66013=DIRECTION('center_axis',(1.,0.,0.));
#66014=DIRECTION('ref_axis',(0.,0.,-1.));
#66015=DIRECTION('',(0.,-0.920369981160753,0.391048715351624));
#66016=DIRECTION('center_axis',(0.,0.391048715351624,0.920369981160753));
#66017=DIRECTION('ref_axis',(0.,-0.920369981160753,0.391048715351624));
#66018=DIRECTION('',(-1.,0.,0.));
#66019=DIRECTION('',(0.,0.920369981160753,-0.391048715351624));
#66020=DIRECTION('center_axis',(1.,0.,0.));
#66021=DIRECTION('ref_axis',(0.,-0.766044443118978,-0.642787609686539));
#66022=DIRECTION('center_axis',(-1.,0.,0.));
#66023=DIRECTION('ref_axis',(0.,1.,0.));
#66024=DIRECTION('center_axis',(0.,-0.998611417361506,-0.0526805193144866));
#66025=DIRECTION('ref_axis',(0.,0.0526805193144866,-0.998611417361506));
#66026=DIRECTION('',(1.,0.,0.));
#66027=DIRECTION('',(0.,-0.0526805193144866,0.998611417361506));
#66028=DIRECTION('',(1.,0.,0.));
#66029=DIRECTION('',(0.,0.0526805193144866,-0.998611417361506));
#66030=DIRECTION('center_axis',(1.,0.,0.));
#66031=DIRECTION('ref_axis',(0.,-0.866025403784439,-0.5));
#66032=DIRECTION('center_axis',(1.,0.,0.));
#66033=DIRECTION('ref_axis',(0.,0.,-1.));
#66034=DIRECTION('',(0.,-0.838482596287006,0.544928376691655));
#66035=DIRECTION('center_axis',(0.,0.544928376691655,0.838482596287006));
#66036=DIRECTION('ref_axis',(0.,-0.838482596287006,0.544928376691655));
#66037=DIRECTION('',(-1.,0.,0.));
#66038=DIRECTION('',(0.,0.838482596287006,-0.544928376691655));
#66039=DIRECTION('center_axis',(1.,0.,0.));
#66040=DIRECTION('ref_axis',(0.,-0.866025403784439,-0.5));
#66041=DIRECTION('center_axis',(-1.,0.,0.));
#66042=DIRECTION('ref_axis',(0.,1.,0.));
#66043=DIRECTION('center_axis',(0.,-0.992588142241629,0.121526868968601));
#66044=DIRECTION('ref_axis',(0.,-0.121526868968601,-0.992588142241629));
#66045=DIRECTION('',(1.,0.,0.));
#66046=DIRECTION('',(0.,0.121526868968601,0.992588142241629));
#66047=DIRECTION('',(1.,0.,0.));
#66048=DIRECTION('',(0.,-0.121526868968601,-0.992588142241629));
#66049=DIRECTION('center_axis',(1.,0.,0.));
#66050=DIRECTION('ref_axis',(0.,-0.939692620785909,-0.342020143325668));
#66051=DIRECTION('center_axis',(1.,0.,0.));
#66052=DIRECTION('ref_axis',(0.,0.,-1.));
#66053=DIRECTION('',(0.,-0.731118342017744,0.682250665052974));
#66054=DIRECTION('center_axis',(0.,0.682250665052974,0.731118342017744));
#66055=DIRECTION('ref_axis',(0.,-0.731118342017744,0.682250665052974));
#66056=DIRECTION('',(-1.,0.,0.));
#66057=DIRECTION('',(0.,0.731118342017744,-0.682250665052974));
#66058=DIRECTION('center_axis',(1.,0.,0.));
#66059=DIRECTION('ref_axis',(0.,-0.939692620785909,-0.342020143325668));
#66060=DIRECTION('center_axis',(-1.,0.,0.));
#66061=DIRECTION('ref_axis',(0.,1.,0.));
#66062=DIRECTION('center_axis',(0.,-0.956405578693575,0.292041724833639));
#66063=DIRECTION('ref_axis',(0.,-0.292041724833639,-0.956405578693575));
#66064=DIRECTION('',(1.,0.,0.));
#66065=DIRECTION('',(0.,0.292041724833639,0.956405578693575));
#66066=DIRECTION('',(1.,0.,0.));
#66067=DIRECTION('',(0.,-0.292041724833639,-0.956405578693575));
#66068=DIRECTION('center_axis',(1.,0.,0.));
#66069=DIRECTION('ref_axis',(0.,-0.984807753012208,-0.17364817766693));
#66070=DIRECTION('center_axis',(1.,0.,0.));
#66071=DIRECTION('ref_axis',(0.,0.,-1.));
#66072=DIRECTION('',(0.,-0.601539426890005,0.798843112192153));
#66073=DIRECTION('center_axis',(0.,0.798843112192153,0.601539426890005));
#66074=DIRECTION('ref_axis',(0.,-0.601539426890005,0.798843112192153));
#66075=DIRECTION('',(-1.,0.,0.));
#66076=DIRECTION('',(0.,0.601539426890005,-0.798843112192153));
#66077=DIRECTION('center_axis',(1.,0.,0.));
#66078=DIRECTION('ref_axis',(0.,-0.984807753012208,-0.17364817766693));
#66079=DIRECTION('center_axis',(-1.,0.,0.));
#66080=DIRECTION('ref_axis',(0.,1.,0.));
#66081=DIRECTION('center_axis',(0.,-0.891163115601492,0.453683040669851));
#66082=DIRECTION('ref_axis',(0.,-0.453683040669851,-0.891163115601492));
#66083=DIRECTION('',(1.,0.,0.));
#66084=DIRECTION('',(0.,0.453683040669851,0.891163115601492));
#66085=DIRECTION('',(1.,0.,0.));
#66086=DIRECTION('',(0.,-0.453683040669851,-0.891163115601492));
#66087=DIRECTION('center_axis',(1.,0.,0.));
#66088=DIRECTION('ref_axis',(0.,-1.,1.83697019872103E-16));
#66089=DIRECTION('center_axis',(1.,0.,0.));
#66090=DIRECTION('ref_axis',(0.,0.,-1.));
#66091=DIRECTION('',(0.,-0.453683040669851,0.891163115601492));
#66092=DIRECTION('center_axis',(0.,0.891163115601492,0.453683040669851));
#66093=DIRECTION('ref_axis',(0.,-0.453683040669851,0.891163115601492));
#66094=DIRECTION('',(-1.,0.,0.));
#66095=DIRECTION('',(0.,0.453683040669851,-0.891163115601492));
#66096=DIRECTION('center_axis',(1.,0.,0.));
#66097=DIRECTION('ref_axis',(0.,-1.,1.83697019872103E-16));
#66098=DIRECTION('center_axis',(-1.,0.,0.));
#66099=DIRECTION('ref_axis',(0.,1.,0.));
#66100=DIRECTION('center_axis',(0.,-0.798843112192153,0.601539426890005));
#66101=DIRECTION('ref_axis',(0.,-0.601539426890005,-0.798843112192153));
#66102=DIRECTION('',(1.,0.,0.));
#66103=DIRECTION('',(0.,0.601539426890005,0.798843112192153));
#66104=DIRECTION('',(1.,0.,0.));
#66105=DIRECTION('',(0.,-0.601539426890005,-0.798843112192153));
#66106=DIRECTION('center_axis',(1.,0.,0.));
#66107=DIRECTION('ref_axis',(0.,-0.984807753012208,0.17364817766693));
#66108=DIRECTION('center_axis',(1.,0.,0.));
#66109=DIRECTION('ref_axis',(0.,0.,-1.));
#66110=DIRECTION('',(0.,-0.292041724833639,0.956405578693576));
#66111=DIRECTION('center_axis',(0.,0.956405578693576,0.292041724833639));
#66112=DIRECTION('ref_axis',(0.,-0.292041724833639,0.956405578693576));
#66113=DIRECTION('',(-1.,0.,0.));
#66114=DIRECTION('',(0.,0.292041724833639,-0.956405578693576));
#66115=DIRECTION('center_axis',(1.,0.,0.));
#66116=DIRECTION('ref_axis',(0.,-0.984807753012208,0.17364817766693));
#66117=DIRECTION('center_axis',(-1.,0.,0.));
#66118=DIRECTION('ref_axis',(0.,1.,0.));
#66119=DIRECTION('center_axis',(0.,-0.682250665052973,0.731118342017745));
#66120=DIRECTION('ref_axis',(0.,-0.731118342017745,-0.682250665052973));
#66121=DIRECTION('',(1.,0.,0.));
#66122=DIRECTION('',(0.,0.731118342017745,0.682250665052973));
#66123=DIRECTION('',(1.,0.,0.));
#66124=DIRECTION('',(0.,-0.731118342017745,-0.682250665052973));
#66125=DIRECTION('center_axis',(1.,0.,0.));
#66126=DIRECTION('ref_axis',(0.,-0.939692620785908,0.342020143325669));
#66127=DIRECTION('center_axis',(1.,0.,0.));
#66128=DIRECTION('ref_axis',(0.,0.,-1.));
#66129=DIRECTION('',(0.,-0.1215268689686,0.992588142241629));
#66130=DIRECTION('center_axis',(0.,0.992588142241629,0.1215268689686));
#66131=DIRECTION('ref_axis',(0.,-0.1215268689686,0.992588142241629));
#66132=DIRECTION('',(-1.,0.,0.));
#66133=DIRECTION('',(0.,0.1215268689686,-0.992588142241629));
#66134=DIRECTION('center_axis',(1.,0.,0.));
#66135=DIRECTION('ref_axis',(0.,-0.939692620785908,0.342020143325669));
#66136=DIRECTION('center_axis',(-1.,0.,0.));
#66137=DIRECTION('ref_axis',(0.,1.,0.));
#66138=DIRECTION('center_axis',(0.,-0.544928376691655,0.838482596287006));
#66139=DIRECTION('ref_axis',(0.,-0.838482596287006,-0.544928376691655));
#66140=DIRECTION('',(1.,0.,0.));
#66141=DIRECTION('',(0.,0.838482596287006,0.544928376691655));
#66142=DIRECTION('',(1.,0.,0.));
#66143=DIRECTION('',(0.,-0.838482596287006,-0.544928376691655));
#66144=DIRECTION('center_axis',(1.,0.,0.));
#66145=DIRECTION('ref_axis',(0.,-0.866025403784438,0.5));
#66146=DIRECTION('center_axis',(1.,0.,0.));
#66147=DIRECTION('ref_axis',(0.,0.,-1.));
#66148=DIRECTION('',(0.,0.052680519314487,0.998611417361506));
#66149=DIRECTION('center_axis',(0.,0.998611417361506,-0.052680519314487));
#66150=DIRECTION('ref_axis',(0.,0.052680519314487,0.998611417361506));
#66151=DIRECTION('',(-1.,0.,0.));
#66152=DIRECTION('',(0.,-0.052680519314487,-0.998611417361506));
#66153=DIRECTION('center_axis',(1.,0.,0.));
#66154=DIRECTION('ref_axis',(0.,-0.866025403784438,0.5));
#66155=DIRECTION('center_axis',(-1.,0.,0.));
#66156=DIRECTION('ref_axis',(0.,1.,0.));
#66157=DIRECTION('center_axis',(0.,-0.391048715351624,0.920369981160753));
#66158=DIRECTION('ref_axis',(0.,-0.920369981160753,-0.391048715351624));
#66159=DIRECTION('',(1.,0.,0.));
#66160=DIRECTION('',(0.,0.920369981160753,0.391048715351624));
#66161=DIRECTION('',(1.,0.,0.));
#66162=DIRECTION('',(0.,-0.920369981160753,-0.391048715351624));
#66163=DIRECTION('center_axis',(1.,0.,0.));
#66164=DIRECTION('ref_axis',(0.,-0.766044443118978,0.642787609686539));
#66165=DIRECTION('center_axis',(1.,0.,0.));
#66166=DIRECTION('ref_axis',(0.,0.,-1.));
#66167=DIRECTION('',(0.,0.225287236675832,0.974292389886613));
#66168=DIRECTION('center_axis',(0.,0.974292389886613,-0.225287236675832));
#66169=DIRECTION('ref_axis',(0.,0.225287236675832,0.974292389886613));
#66170=DIRECTION('',(-1.,0.,0.));
#66171=DIRECTION('',(0.,-0.225287236675832,-0.974292389886613));
#66172=DIRECTION('center_axis',(1.,0.,0.));
#66173=DIRECTION('ref_axis',(0.,-0.766044443118978,0.642787609686539));
#66174=DIRECTION('center_axis',(-1.,0.,0.));
#66175=DIRECTION('ref_axis',(0.,1.,0.));
#66176=DIRECTION('center_axis',(0.,-0.225287236675832,0.974292389886613));
#66177=DIRECTION('ref_axis',(0.,-0.974292389886613,-0.225287236675832));
#66178=DIRECTION('',(1.,0.,0.));
#66179=DIRECTION('',(0.,0.974292389886613,0.225287236675832));
#66180=DIRECTION('',(1.,0.,0.));
#66181=DIRECTION('',(0.,-0.974292389886613,-0.225287236675832));
#66182=DIRECTION('center_axis',(1.,0.,0.));
#66183=DIRECTION('ref_axis',(0.,-0.642787609686539,0.766044443118978));
#66184=DIRECTION('center_axis',(1.,0.,0.));
#66185=DIRECTION('ref_axis',(0.,0.,-1.));
#66186=DIRECTION('',(0.,0.391048715351624,0.920369981160753));
#66187=DIRECTION('center_axis',(0.,0.920369981160753,-0.391048715351624));
#66188=DIRECTION('ref_axis',(0.,0.391048715351624,0.920369981160753));
#66189=DIRECTION('',(-1.,0.,0.));
#66190=DIRECTION('',(0.,-0.391048715351624,-0.920369981160753));
#66191=DIRECTION('center_axis',(1.,0.,0.));
#66192=DIRECTION('ref_axis',(0.,-0.642787609686539,0.766044443118978));
#66193=DIRECTION('center_axis',(-1.,0.,0.));
#66194=DIRECTION('ref_axis',(0.,1.,0.));
#66195=DIRECTION('center_axis',(0.,-0.0526805193144861,0.998611417361506));
#66196=DIRECTION('ref_axis',(0.,-0.998611417361506,-0.0526805193144861));
#66197=DIRECTION('',(1.,0.,0.));
#66198=DIRECTION('',(0.,0.998611417361506,0.0526805193144861));
#66199=DIRECTION('',(1.,0.,0.));
#66200=DIRECTION('',(0.,-0.998611417361506,-0.0526805193144861));
#66201=DIRECTION('center_axis',(1.,0.,0.));
#66202=DIRECTION('ref_axis',(0.,-0.5,0.866025403784439));
#66203=DIRECTION('center_axis',(1.,0.,0.));
#66204=DIRECTION('ref_axis',(0.,0.,-1.));
#66205=DIRECTION('',(0.,0.544928376691655,0.838482596287005));
#66206=DIRECTION('center_axis',(0.,0.838482596287005,-0.544928376691655));
#66207=DIRECTION('ref_axis',(0.,0.544928376691655,0.838482596287005));
#66208=DIRECTION('',(-1.,0.,0.));
#66209=DIRECTION('',(0.,-0.544928376691655,-0.838482596287005));
#66210=DIRECTION('center_axis',(1.,0.,0.));
#66211=DIRECTION('ref_axis',(0.,-0.5,0.866025403784439));
#66212=DIRECTION('center_axis',(-1.,0.,0.));
#66213=DIRECTION('ref_axis',(0.,1.,0.));
#66214=DIRECTION('center_axis',(0.,0.1215268689686,0.992588142241629));
#66215=DIRECTION('ref_axis',(0.,-0.992588142241629,0.1215268689686));
#66216=DIRECTION('',(1.,0.,0.));
#66217=DIRECTION('',(0.,0.992588142241629,-0.1215268689686));
#66218=DIRECTION('',(1.,0.,0.));
#66219=DIRECTION('',(0.,-0.992588142241629,0.1215268689686));
#66220=DIRECTION('center_axis',(1.,0.,0.));
#66221=DIRECTION('ref_axis',(0.,-0.342020143325669,0.939692620785909));
#66222=DIRECTION('center_axis',(1.,0.,0.));
#66223=DIRECTION('ref_axis',(0.,0.,-1.));
#66224=DIRECTION('',(0.,0.682250665052974,0.731118342017744));
#66225=DIRECTION('center_axis',(0.,0.731118342017744,-0.682250665052974));
#66226=DIRECTION('ref_axis',(0.,0.682250665052974,0.731118342017744));
#66227=DIRECTION('',(-1.,0.,0.));
#66228=DIRECTION('',(0.,-0.682250665052974,-0.731118342017744));
#66229=DIRECTION('center_axis',(1.,0.,0.));
#66230=DIRECTION('ref_axis',(0.,-0.342020143325669,0.939692620785909));
#66231=DIRECTION('center_axis',(-1.,0.,0.));
#66232=DIRECTION('ref_axis',(0.,1.,0.));
#66233=DIRECTION('center_axis',(0.,0.292041724833639,0.956405578693575));
#66234=DIRECTION('ref_axis',(0.,-0.956405578693575,0.292041724833639));
#66235=DIRECTION('',(1.,0.,0.));
#66236=DIRECTION('',(0.,0.956405578693575,-0.292041724833639));
#66237=DIRECTION('',(1.,0.,0.));
#66238=DIRECTION('',(0.,-0.956405578693575,0.292041724833639));
#66239=DIRECTION('center_axis',(1.,0.,0.));
#66240=DIRECTION('ref_axis',(0.,-0.17364817766693,0.984807753012208));
#66241=DIRECTION('center_axis',(1.,0.,0.));
#66242=DIRECTION('ref_axis',(0.,0.,-1.));
#66243=DIRECTION('',(0.,0.798843112192153,0.601539426890005));
#66244=DIRECTION('center_axis',(0.,0.601539426890005,-0.798843112192153));
#66245=DIRECTION('ref_axis',(0.,0.798843112192153,0.601539426890005));
#66246=DIRECTION('',(-1.,0.,0.));
#66247=DIRECTION('',(0.,-0.798843112192153,-0.601539426890005));
#66248=DIRECTION('center_axis',(1.,0.,0.));
#66249=DIRECTION('ref_axis',(0.,-0.17364817766693,0.984807753012208));
#66250=DIRECTION('center_axis',(-1.,0.,0.));
#66251=DIRECTION('ref_axis',(0.,1.,0.));
#66252=DIRECTION('center_axis',(0.,0.453683040669851,0.891163115601492));
#66253=DIRECTION('ref_axis',(0.,-0.891163115601492,0.453683040669851));
#66254=DIRECTION('',(1.,0.,0.));
#66255=DIRECTION('',(0.,0.891163115601492,-0.453683040669851));
#66256=DIRECTION('',(1.,0.,0.));
#66257=DIRECTION('',(0.,-0.891163115601492,0.453683040669851));
#66258=DIRECTION('center_axis',(1.,0.,0.));
#66259=DIRECTION('ref_axis',(0.,1.22464679914735E-16,1.));
#66260=DIRECTION('center_axis',(1.,0.,0.));
#66261=DIRECTION('ref_axis',(0.,0.,-1.));
#66262=DIRECTION('',(0.,0.891163115601492,0.453683040669851));
#66263=DIRECTION('center_axis',(1.,0.,0.));
#66264=DIRECTION('ref_axis',(0.,0.,-1.));
#66265=DIRECTION('center_axis',(0.,0.453683040669851,-0.891163115601492));
#66266=DIRECTION('ref_axis',(0.,0.891163115601492,0.453683040669851));
#66267=DIRECTION('',(-1.,0.,0.));
#66268=DIRECTION('',(0.,-0.891163115601492,-0.453683040669851));
#66269=DIRECTION('center_axis',(1.,0.,0.));
#66270=DIRECTION('ref_axis',(0.,1.22464679914735E-16,1.));
#66271=DIRECTION('center_axis',(-1.,0.,0.));
#66272=DIRECTION('ref_axis',(0.,1.,0.));
#66273=DIRECTION('center_axis',(-1.,0.,0.));
#66274=DIRECTION('ref_axis',(0.,1.,0.));
#66275=DIRECTION('center_axis',(0.,0.601539426890006,0.798843112192152));
#66276=DIRECTION('ref_axis',(0.,-0.798843112192152,0.601539426890006));
#66277=DIRECTION('',(1.,0.,0.));
#66278=DIRECTION('',(0.,0.798843112192152,-0.601539426890006));
#66279=DIRECTION('',(1.,0.,0.));
#66280=DIRECTION('',(0.,-0.798843112192152,0.601539426890006));
#66281=DIRECTION('center_axis',(1.,0.,0.));
#66282=DIRECTION('ref_axis',(0.,0.173648177666931,0.984807753012208));
#66283=DIRECTION('center_axis',(1.,0.,0.));
#66284=DIRECTION('ref_axis',(0.,0.,-1.));
#66285=DIRECTION('',(0.,0.956405578693576,0.292041724833639));
#66286=DIRECTION('center_axis',(0.,0.292041724833639,-0.956405578693576));
#66287=DIRECTION('ref_axis',(0.,0.956405578693576,0.292041724833639));
#66288=DIRECTION('',(-1.,0.,0.));
#66289=DIRECTION('',(0.,-0.956405578693576,-0.292041724833639));
#66290=DIRECTION('center_axis',(1.,0.,0.));
#66291=DIRECTION('ref_axis',(0.,0.173648177666931,0.984807753012208));
#66292=DIRECTION('center_axis',(-1.,0.,0.));
#66293=DIRECTION('ref_axis',(0.,1.,0.));
#66294=DIRECTION('center_axis',(0.,0.731118342017744,0.682250665052974));
#66295=DIRECTION('ref_axis',(0.,-0.682250665052974,0.731118342017744));
#66296=DIRECTION('',(1.,0.,0.));
#66297=DIRECTION('',(0.,0.682250665052974,-0.731118342017744));
#66298=DIRECTION('',(1.,0.,0.));
#66299=DIRECTION('',(0.,-0.682250665052974,0.731118342017744));
#66300=DIRECTION('center_axis',(1.,0.,0.));
#66301=DIRECTION('ref_axis',(0.,0.342020143325669,0.939692620785908));
#66302=DIRECTION('center_axis',(1.,0.,0.));
#66303=DIRECTION('ref_axis',(0.,0.,-1.));
#66304=DIRECTION('',(0.,0.992588142241629,0.1215268689686));
#66305=DIRECTION('center_axis',(0.,0.1215268689686,-0.992588142241629));
#66306=DIRECTION('ref_axis',(0.,0.992588142241629,0.1215268689686));
#66307=DIRECTION('',(-1.,0.,0.));
#66308=DIRECTION('',(0.,-0.992588142241629,-0.1215268689686));
#66309=DIRECTION('center_axis',(1.,0.,0.));
#66310=DIRECTION('ref_axis',(0.,0.342020143325669,0.939692620785908));
#66311=DIRECTION('center_axis',(-1.,0.,0.));
#66312=DIRECTION('ref_axis',(0.,1.,0.));
#66313=DIRECTION('center_axis',(0.,0.838482596287006,0.544928376691655));
#66314=DIRECTION('ref_axis',(0.,-0.544928376691655,0.838482596287006));
#66315=DIRECTION('',(1.,0.,0.));
#66316=DIRECTION('',(0.,0.544928376691655,-0.838482596287006));
#66317=DIRECTION('',(1.,0.,0.));
#66318=DIRECTION('',(0.,-0.544928376691655,0.838482596287006));
#66319=DIRECTION('center_axis',(1.,0.,0.));
#66320=DIRECTION('ref_axis',(0.,0.5,0.866025403784439));
#66321=DIRECTION('center_axis',(1.,0.,0.));
#66322=DIRECTION('ref_axis',(0.,0.,-1.));
#66323=DIRECTION('',(0.,0.998611417361506,-0.0526805193144864));
#66324=DIRECTION('center_axis',(0.,-0.0526805193144864,-0.998611417361506));
#66325=DIRECTION('ref_axis',(0.,0.998611417361506,-0.0526805193144864));
#66326=DIRECTION('',(-1.,0.,0.));
#66327=DIRECTION('',(0.,-0.998611417361506,0.0526805193144864));
#66328=DIRECTION('center_axis',(1.,0.,0.));
#66329=DIRECTION('ref_axis',(0.,0.5,0.866025403784439));
#66330=DIRECTION('center_axis',(-1.,0.,0.));
#66331=DIRECTION('ref_axis',(0.,1.,0.));
#66332=DIRECTION('center_axis',(0.,0.920369981160753,0.391048715351624));
#66333=DIRECTION('ref_axis',(0.,-0.391048715351624,0.920369981160753));
#66334=DIRECTION('',(1.,0.,0.));
#66335=DIRECTION('',(0.,0.391048715351624,-0.920369981160753));
#66336=DIRECTION('',(1.,0.,0.));
#66337=DIRECTION('',(0.,-0.391048715351624,0.920369981160753));
#66338=DIRECTION('center_axis',(1.,0.,0.));
#66339=DIRECTION('ref_axis',(0.,0.642787609686539,0.766044443118978));
#66340=DIRECTION('center_axis',(1.,0.,0.));
#66341=DIRECTION('ref_axis',(0.,0.,-1.));
#66342=DIRECTION('',(0.,0.974292389886613,-0.225287236675832));
#66343=DIRECTION('center_axis',(0.,-0.225287236675832,-0.974292389886613));
#66344=DIRECTION('ref_axis',(0.,0.974292389886613,-0.225287236675832));
#66345=DIRECTION('',(-1.,0.,0.));
#66346=DIRECTION('',(0.,-0.974292389886613,0.225287236675832));
#66347=DIRECTION('center_axis',(1.,0.,0.));
#66348=DIRECTION('ref_axis',(0.,0.642787609686539,0.766044443118978));
#66349=DIRECTION('center_axis',(-1.,0.,0.));
#66350=DIRECTION('ref_axis',(0.,1.,0.));
#66351=DIRECTION('center_axis',(0.,0.974292389886613,0.225287236675832));
#66352=DIRECTION('ref_axis',(0.,-0.225287236675832,0.974292389886613));
#66353=DIRECTION('',(1.,0.,0.));
#66354=DIRECTION('',(0.,0.225287236675832,-0.974292389886613));
#66355=DIRECTION('',(1.,0.,0.));
#66356=DIRECTION('',(0.,-0.225287236675832,0.974292389886613));
#66357=DIRECTION('center_axis',(1.,0.,0.));
#66358=DIRECTION('ref_axis',(0.,0.766044443118978,0.642787609686539));
#66359=DIRECTION('center_axis',(1.,0.,0.));
#66360=DIRECTION('ref_axis',(0.,0.,-1.));
#66361=DIRECTION('',(0.,0.920369981160753,-0.391048715351624));
#66362=DIRECTION('center_axis',(0.,-0.391048715351624,-0.920369981160753));
#66363=DIRECTION('ref_axis',(0.,0.920369981160753,-0.391048715351624));
#66364=DIRECTION('',(-1.,0.,0.));
#66365=DIRECTION('',(0.,-0.920369981160753,0.391048715351624));
#66366=DIRECTION('center_axis',(1.,0.,0.));
#66367=DIRECTION('ref_axis',(0.,0.766044443118978,0.642787609686539));
#66368=DIRECTION('center_axis',(-1.,0.,0.));
#66369=DIRECTION('ref_axis',(0.,1.,0.));
#66370=DIRECTION('center_axis',(0.,0.998611417361506,0.0526805193144862));
#66371=DIRECTION('ref_axis',(0.,-0.0526805193144862,0.998611417361506));
#66372=DIRECTION('',(1.,0.,0.));
#66373=DIRECTION('',(0.,0.0526805193144862,-0.998611417361506));
#66374=DIRECTION('',(1.,0.,0.));
#66375=DIRECTION('',(0.,-0.0526805193144862,0.998611417361506));
#66376=DIRECTION('center_axis',(1.,0.,0.));
#66377=DIRECTION('ref_axis',(0.,0.866025403784439,0.5));
#66378=DIRECTION('center_axis',(1.,0.,0.));
#66379=DIRECTION('ref_axis',(0.,0.,-1.));
#66380=DIRECTION('',(0.,0.838482596287005,-0.544928376691655));
#66381=DIRECTION('center_axis',(0.,-0.544928376691655,-0.838482596287005));
#66382=DIRECTION('ref_axis',(0.,0.838482596287005,-0.544928376691655));
#66383=DIRECTION('',(-1.,0.,0.));
#66384=DIRECTION('',(0.,-0.838482596287005,0.544928376691655));
#66385=DIRECTION('center_axis',(1.,0.,0.));
#66386=DIRECTION('ref_axis',(0.,0.866025403784439,0.5));
#66387=DIRECTION('center_axis',(-1.,0.,0.));
#66388=DIRECTION('ref_axis',(0.,1.,0.));
#66389=DIRECTION('center_axis',(0.,0.992588142241629,-0.1215268689686));
#66390=DIRECTION('ref_axis',(0.,0.1215268689686,0.992588142241629));
#66391=DIRECTION('',(1.,0.,0.));
#66392=DIRECTION('',(0.,-0.1215268689686,-0.992588142241629));
#66393=DIRECTION('',(1.,0.,0.));
#66394=DIRECTION('',(0.,0.1215268689686,0.992588142241629));
#66395=DIRECTION('center_axis',(1.,0.,0.));
#66396=DIRECTION('ref_axis',(0.,0.939692620785908,0.342020143325669));
#66397=DIRECTION('center_axis',(1.,0.,0.));
#66398=DIRECTION('ref_axis',(0.,0.,-1.));
#66399=DIRECTION('',(0.,0.731118342017744,-0.682250665052974));
#66400=DIRECTION('center_axis',(0.,-0.682250665052974,-0.731118342017744));
#66401=DIRECTION('ref_axis',(0.,0.731118342017744,-0.682250665052974));
#66402=DIRECTION('',(-1.,0.,0.));
#66403=DIRECTION('',(0.,-0.731118342017744,0.682250665052974));
#66404=DIRECTION('center_axis',(1.,0.,0.));
#66405=DIRECTION('ref_axis',(0.,0.939692620785908,0.342020143325669));
#66406=DIRECTION('center_axis',(-1.,0.,0.));
#66407=DIRECTION('ref_axis',(0.,1.,0.));
#66408=DIRECTION('center_axis',(0.,0.956405578693576,-0.292041724833639));
#66409=DIRECTION('ref_axis',(0.,0.292041724833639,0.956405578693576));
#66410=DIRECTION('',(1.,0.,0.));
#66411=DIRECTION('',(0.,-0.292041724833639,-0.956405578693576));
#66412=DIRECTION('',(1.,0.,0.));
#66413=DIRECTION('',(0.,0.292041724833639,0.956405578693576));
#66414=DIRECTION('center_axis',(1.,0.,0.));
#66415=DIRECTION('ref_axis',(0.,0.984807753012208,0.17364817766693));
#66416=DIRECTION('center_axis',(1.,0.,0.));
#66417=DIRECTION('ref_axis',(0.,0.,-1.));
#66418=DIRECTION('',(0.,0.601539426890005,-0.798843112192153));
#66419=DIRECTION('center_axis',(0.,-0.798843112192153,-0.601539426890005));
#66420=DIRECTION('ref_axis',(0.,0.601539426890005,-0.798843112192153));
#66421=DIRECTION('',(-1.,0.,0.));
#66422=DIRECTION('',(0.,-0.601539426890005,0.798843112192153));
#66423=DIRECTION('center_axis',(1.,0.,0.));
#66424=DIRECTION('ref_axis',(0.,0.984807753012208,0.17364817766693));
#66425=DIRECTION('center_axis',(-1.,0.,0.));
#66426=DIRECTION('ref_axis',(0.,1.,0.));
#66427=DIRECTION('center_axis',(0.,0.891163115601492,-0.453683040669851));
#66428=DIRECTION('ref_axis',(0.,0.453683040669851,0.891163115601492));
#66429=DIRECTION('',(1.,0.,0.));
#66430=DIRECTION('',(0.,-0.453683040669851,-0.891163115601492));
#66431=DIRECTION('',(1.,0.,0.));
#66432=DIRECTION('',(0.,0.453683040669851,0.891163115601492));
#66433=DIRECTION('center_axis',(1.,0.,0.));
#66434=DIRECTION('ref_axis',(0.,1.,-6.12323399573677E-17));
#66435=DIRECTION('center_axis',(1.,0.,0.));
#66436=DIRECTION('ref_axis',(0.,0.,-1.));
#66437=DIRECTION('',(0.,0.453683040669851,-0.891163115601492));
#66438=DIRECTION('center_axis',(0.,-0.891163115601492,-0.453683040669851));
#66439=DIRECTION('ref_axis',(0.,0.453683040669851,-0.891163115601492));
#66440=DIRECTION('',(-1.,0.,0.));
#66441=DIRECTION('',(0.,-0.453683040669851,0.891163115601492));
#66442=DIRECTION('center_axis',(1.,0.,0.));
#66443=DIRECTION('ref_axis',(0.,1.,-6.12323399573677E-17));
#66444=DIRECTION('center_axis',(-1.,0.,0.));
#66445=DIRECTION('ref_axis',(0.,1.,0.));
#66446=DIRECTION('center_axis',(0.,0.798843112192153,-0.601539426890005));
#66447=DIRECTION('ref_axis',(0.,0.601539426890005,0.798843112192152));
#66448=DIRECTION('',(1.,0.,0.));
#66449=DIRECTION('',(0.,-0.601539426890005,-0.798843112192152));
#66450=DIRECTION('',(1.,0.,0.));
#66451=DIRECTION('',(0.,0.601539426890005,0.798843112192152));
#66452=DIRECTION('center_axis',(1.,0.,0.));
#66453=DIRECTION('ref_axis',(0.,0.984807753012208,-0.17364817766693));
#66454=DIRECTION('center_axis',(1.,0.,0.));
#66455=DIRECTION('ref_axis',(0.,0.,-1.));
#66456=DIRECTION('',(0.,0.292041724833639,-0.956405578693576));
#66457=DIRECTION('center_axis',(0.,-0.956405578693576,-0.292041724833639));
#66458=DIRECTION('ref_axis',(0.,0.292041724833639,-0.956405578693576));
#66459=DIRECTION('',(-1.,0.,0.));
#66460=DIRECTION('',(0.,-0.292041724833639,0.956405578693576));
#66461=DIRECTION('center_axis',(1.,0.,0.));
#66462=DIRECTION('ref_axis',(0.,0.984807753012208,-0.17364817766693));
#66463=DIRECTION('center_axis',(-1.,0.,0.));
#66464=DIRECTION('ref_axis',(0.,1.,0.));
#66465=DIRECTION('center_axis',(0.,0.682250665052974,-0.731118342017744));
#66466=DIRECTION('ref_axis',(0.,0.731118342017744,0.682250665052974));
#66467=DIRECTION('',(1.,0.,0.));
#66468=DIRECTION('',(0.,-0.731118342017744,-0.682250665052974));
#66469=DIRECTION('',(1.,0.,0.));
#66470=DIRECTION('',(0.,0.731118342017744,0.682250665052974));
#66471=DIRECTION('center_axis',(1.,0.,0.));
#66472=DIRECTION('ref_axis',(0.,0.939692620785908,-0.342020143325669));
#66473=DIRECTION('center_axis',(1.,0.,0.));
#66474=DIRECTION('ref_axis',(0.,0.,-1.));
#66475=DIRECTION('',(0.,0.1215268689686,-0.992588142241629));
#66476=DIRECTION('center_axis',(0.,-0.992588142241629,-0.1215268689686));
#66477=DIRECTION('ref_axis',(0.,0.1215268689686,-0.992588142241629));
#66478=DIRECTION('',(-1.,0.,0.));
#66479=DIRECTION('',(0.,-0.1215268689686,0.992588142241629));
#66480=DIRECTION('center_axis',(1.,0.,0.));
#66481=DIRECTION('ref_axis',(0.,0.939692620785908,-0.342020143325669));
#66482=DIRECTION('center_axis',(-1.,0.,0.));
#66483=DIRECTION('ref_axis',(0.,1.,0.));
#66484=DIRECTION('center_axis',(0.,0.544928376691655,-0.838482596287006));
#66485=DIRECTION('ref_axis',(0.,0.838482596287006,0.544928376691655));
#66486=DIRECTION('',(1.,0.,0.));
#66487=DIRECTION('',(0.,-0.838482596287006,-0.544928376691655));
#66488=DIRECTION('',(1.,0.,0.));
#66489=DIRECTION('',(0.,0.838482596287006,0.544928376691655));
#66490=DIRECTION('center_axis',(1.,0.,0.));
#66491=DIRECTION('ref_axis',(0.,0.866025403784439,-0.5));
#66492=DIRECTION('center_axis',(1.,0.,0.));
#66493=DIRECTION('ref_axis',(0.,0.,-1.));
#66494=DIRECTION('',(0.,-0.0526805193144866,-0.998611417361506));
#66495=DIRECTION('center_axis',(0.,-0.998611417361506,0.0526805193144866));
#66496=DIRECTION('ref_axis',(0.,-0.0526805193144866,-0.998611417361506));
#66497=DIRECTION('',(-1.,0.,0.));
#66498=DIRECTION('',(0.,0.0526805193144866,0.998611417361506));
#66499=DIRECTION('center_axis',(1.,0.,0.));
#66500=DIRECTION('ref_axis',(0.,0.866025403784439,-0.5));
#66501=DIRECTION('center_axis',(-1.,0.,0.));
#66502=DIRECTION('ref_axis',(0.,1.,0.));
#66503=DIRECTION('center_axis',(0.,0.391048715351624,-0.920369981160753));
#66504=DIRECTION('ref_axis',(0.,0.920369981160753,0.391048715351624));
#66505=DIRECTION('',(1.,0.,0.));
#66506=DIRECTION('',(0.,-0.920369981160753,-0.391048715351624));
#66507=DIRECTION('',(1.,0.,0.));
#66508=DIRECTION('',(0.,0.920369981160753,0.391048715351624));
#66509=DIRECTION('center_axis',(1.,0.,0.));
#66510=DIRECTION('ref_axis',(0.,0.766044443118978,-0.642787609686539));
#66511=DIRECTION('center_axis',(1.,0.,0.));
#66512=DIRECTION('ref_axis',(0.,0.,-1.));
#66513=DIRECTION('',(0.,-0.225287236675832,-0.974292389886613));
#66514=DIRECTION('center_axis',(0.,-0.974292389886613,0.225287236675832));
#66515=DIRECTION('ref_axis',(0.,-0.225287236675832,-0.974292389886613));
#66516=DIRECTION('',(-1.,0.,0.));
#66517=DIRECTION('',(0.,0.225287236675832,0.974292389886613));
#66518=DIRECTION('center_axis',(1.,0.,0.));
#66519=DIRECTION('ref_axis',(0.,0.766044443118978,-0.642787609686539));
#66520=DIRECTION('center_axis',(-1.,0.,0.));
#66521=DIRECTION('ref_axis',(0.,1.,0.));
#66522=DIRECTION('center_axis',(0.,0.225287236675832,-0.974292389886613));
#66523=DIRECTION('ref_axis',(0.,0.974292389886613,0.225287236675832));
#66524=DIRECTION('',(1.,0.,0.));
#66525=DIRECTION('',(0.,-0.974292389886613,-0.225287236675832));
#66526=DIRECTION('',(1.,0.,0.));
#66527=DIRECTION('',(0.,0.974292389886613,0.225287236675832));
#66528=DIRECTION('center_axis',(1.,0.,0.));
#66529=DIRECTION('ref_axis',(0.,0.642787609686539,-0.766044443118978));
#66530=DIRECTION('center_axis',(1.,0.,0.));
#66531=DIRECTION('ref_axis',(0.,0.,-1.));
#66532=DIRECTION('',(0.,-0.391048715351624,-0.920369981160753));
#66533=DIRECTION('center_axis',(0.,-0.920369981160753,0.391048715351624));
#66534=DIRECTION('ref_axis',(0.,-0.391048715351624,-0.920369981160753));
#66535=DIRECTION('',(-1.,0.,0.));
#66536=DIRECTION('',(0.,0.391048715351624,0.920369981160753));
#66537=DIRECTION('center_axis',(1.,0.,0.));
#66538=DIRECTION('ref_axis',(0.,0.642787609686539,-0.766044443118978));
#66539=DIRECTION('center_axis',(-1.,0.,0.));
#66540=DIRECTION('ref_axis',(0.,1.,0.));
#66541=DIRECTION('center_axis',(0.,0.0526805193144864,-0.998611417361506));
#66542=DIRECTION('ref_axis',(0.,0.998611417361506,0.0526805193144864));
#66543=DIRECTION('',(1.,0.,0.));
#66544=DIRECTION('',(0.,-0.998611417361506,-0.0526805193144864));
#66545=DIRECTION('',(1.,0.,0.));
#66546=DIRECTION('',(0.,0.998611417361506,0.0526805193144864));
#66547=DIRECTION('center_axis',(1.,0.,0.));
#66548=DIRECTION('ref_axis',(0.,0.5,-0.866025403784439));
#66549=DIRECTION('center_axis',(1.,0.,0.));
#66550=DIRECTION('ref_axis',(0.,0.,-1.));
#66551=DIRECTION('',(0.,-0.544928376691655,-0.838482596287006));
#66552=DIRECTION('center_axis',(0.,-0.838482596287006,0.544928376691655));
#66553=DIRECTION('ref_axis',(0.,-0.544928376691655,-0.838482596287006));
#66554=DIRECTION('',(-1.,0.,0.));
#66555=DIRECTION('',(0.,0.544928376691655,0.838482596287006));
#66556=DIRECTION('center_axis',(1.,0.,0.));
#66557=DIRECTION('ref_axis',(0.,0.5,-0.866025403784439));
#66558=DIRECTION('center_axis',(-1.,0.,0.));
#66559=DIRECTION('ref_axis',(0.,1.,0.));
#66560=DIRECTION('center_axis',(0.,-0.1215268689686,-0.992588142241629));
#66561=DIRECTION('ref_axis',(0.,0.992588142241629,-0.1215268689686));
#66562=DIRECTION('',(1.,0.,0.));
#66563=DIRECTION('',(0.,-0.992588142241629,0.1215268689686));
#66564=DIRECTION('',(1.,0.,0.));
#66565=DIRECTION('',(0.,0.992588142241629,-0.1215268689686));
#66566=DIRECTION('center_axis',(1.,0.,0.));
#66567=DIRECTION('ref_axis',(0.,0.342020143325669,-0.939692620785908));
#66568=DIRECTION('center_axis',(1.,0.,0.));
#66569=DIRECTION('ref_axis',(0.,0.,-1.));
#66570=DIRECTION('',(0.,-0.682250665052974,-0.731118342017744));
#66571=DIRECTION('center_axis',(0.,-0.731118342017744,0.682250665052974));
#66572=DIRECTION('ref_axis',(0.,-0.682250665052974,-0.731118342017744));
#66573=DIRECTION('',(-1.,0.,0.));
#66574=DIRECTION('',(0.,0.682250665052974,0.731118342017744));
#66575=DIRECTION('center_axis',(1.,0.,0.));
#66576=DIRECTION('ref_axis',(0.,0.342020143325669,-0.939692620785908));
#66577=DIRECTION('center_axis',(-1.,0.,0.));
#66578=DIRECTION('ref_axis',(0.,1.,0.));
#66579=DIRECTION('center_axis',(0.,-0.292041724833639,-0.956405578693576));
#66580=DIRECTION('ref_axis',(0.,0.956405578693576,-0.292041724833639));
#66581=DIRECTION('',(1.,0.,0.));
#66582=DIRECTION('',(0.,-0.956405578693576,0.292041724833639));
#66583=DIRECTION('',(1.,0.,0.));
#66584=DIRECTION('',(0.,0.956405578693576,-0.292041724833639));
#66585=DIRECTION('center_axis',(1.,0.,0.));
#66586=DIRECTION('ref_axis',(0.,0.17364817766693,-0.984807753012208));
#66587=DIRECTION('center_axis',(1.,0.,0.));
#66588=DIRECTION('ref_axis',(0.,0.,-1.));
#66589=DIRECTION('',(0.,-0.798843112192153,-0.601539426890005));
#66590=DIRECTION('center_axis',(0.,-0.601539426890005,0.798843112192153));
#66591=DIRECTION('ref_axis',(0.,-0.798843112192153,-0.601539426890005));
#66592=DIRECTION('',(-1.,0.,0.));
#66593=DIRECTION('',(0.,0.798843112192153,0.601539426890005));
#66594=DIRECTION('center_axis',(1.,0.,0.));
#66595=DIRECTION('ref_axis',(0.,0.17364817766693,-0.984807753012208));
#66596=DIRECTION('center_axis',(-1.,0.,0.));
#66597=DIRECTION('ref_axis',(0.,1.,0.));
#66598=DIRECTION('center_axis',(1.,0.,0.));
#66599=DIRECTION('ref_axis',(0.,0.,-1.));
#66600=DIRECTION('center_axis',(1.,0.,0.));
#66601=DIRECTION('ref_axis',(0.,0.,-1.));
#66602=DIRECTION('',(0.,0.891163115601492,-0.453683040669851));
#66603=DIRECTION('',(0.,-0.891163115601492,-0.453683040669851));
#66604=DIRECTION('center_axis',(0.,-0.453683040669851,-0.891163115601492));
#66605=DIRECTION('ref_axis',(0.,0.891163115601492,-0.453683040669851));
#66606=DIRECTION('',(1.,0.,0.));
#66607=DIRECTION('',(0.,-0.891163115601492,0.453683040669851));
#66608=DIRECTION('',(1.,0.,0.));
#66609=DIRECTION('center_axis',(0.,-0.453683040669851,0.891163115601492));
#66610=DIRECTION('ref_axis',(0.,-0.891163115601492,-0.453683040669851));
#66611=DIRECTION('',(-1.,0.,0.));
#66612=DIRECTION('',(0.,0.891163115601492,0.453683040669851));
#66613=DIRECTION('center_axis',(1.,0.,0.));
#66614=DIRECTION('ref_axis',(0.,0.,-1.));
#66615=DIRECTION('center_axis',(-1.,0.,0.));
#66616=DIRECTION('ref_axis',(0.,1.,0.));
#66617=DIRECTION('center_axis',(1.,0.,0.));
#66618=DIRECTION('ref_axis',(0.,1.,0.));
#66619=DIRECTION('',(0.516609948219971,-0.856220860175784,-1.04856813577747E-16));
#66620=DIRECTION('center_axis',(-1.,0.,0.));
#66621=DIRECTION('ref_axis',(0.,1.,0.));
#66622=DIRECTION('center_axis',(0.,-0.5,0.866025403784439));
#66623=DIRECTION('ref_axis',(0.,-0.866025403784439,-0.5));
#66624=DIRECTION('',(0.,0.866025403784439,0.5));
#66625=DIRECTION('',(1.,0.,0.));
#66626=DIRECTION('',(0.,-0.866025403784439,-0.5));
#66627=DIRECTION('',(1.,0.,0.));
#66628=DIRECTION('center_axis',(0.,0.5,0.866025403784439));
#66629=DIRECTION('ref_axis',(0.,-0.866025403784439,0.5));
#66630=DIRECTION('',(0.,0.866025403784439,-0.5));
#66631=DIRECTION('',(0.,-0.866025403784439,0.5));
#66632=DIRECTION('',(1.,0.,0.));
#66633=DIRECTION('center_axis',(0.,1.,-3.60555503696918E-16));
#66634=DIRECTION('ref_axis',(0.,3.60555503696918E-16,1.));
#66635=DIRECTION('',(0.,-3.60555503696918E-16,-1.));
#66636=DIRECTION('',(0.,3.60555503696918E-16,1.));
#66637=DIRECTION('',(1.,0.,0.));
#66638=DIRECTION('center_axis',(0.,0.5,-0.866025403784439));
#66639=DIRECTION('ref_axis',(0.,0.866025403784439,0.5));
#66640=DIRECTION('',(0.,-0.866025403784439,-0.5));
#66641=DIRECTION('',(0.,0.866025403784439,0.5));
#66642=DIRECTION('',(1.,0.,0.));
#66643=DIRECTION('center_axis',(0.,-0.5,-0.866025403784439));
#66644=DIRECTION('ref_axis',(0.,0.866025403784439,-0.5));
#66645=DIRECTION('',(0.,-0.866025403784439,0.5));
#66646=DIRECTION('',(0.,0.866025403784439,-0.5));
#66647=DIRECTION('',(1.,0.,0.));
#66648=DIRECTION('center_axis',(0.,-1.,-1.20185167898973E-16));
#66649=DIRECTION('ref_axis',(0.,1.20185167898973E-16,-1.));
#66650=DIRECTION('',(0.,-1.20185167898973E-16,1.));
#66651=DIRECTION('',(0.,1.20185167898973E-16,-1.));
#66652=DIRECTION('center_axis',(1.,0.,0.));
#66653=DIRECTION('ref_axis',(0.,0.,-1.));
#66654=DIRECTION('center_axis',(-1.,0.,0.));
#66655=DIRECTION('ref_axis',(0.,0.,1.));
#66656=DIRECTION('center_axis',(1.,0.,0.));
#66657=DIRECTION('ref_axis',(0.,0.,-1.));
#66658=DIRECTION('center_axis',(1.,0.,0.));
#66659=DIRECTION('ref_axis',(0.,1.,0.));
#66660=DIRECTION('',(-0.707106781186548,0.707106781186547,8.65956056235493E-17));
#66661=DIRECTION('center_axis',(1.,0.,0.));
#66662=DIRECTION('ref_axis',(0.,1.,0.));
#66663=DIRECTION('center_axis',(1.,0.,0.));
#66664=DIRECTION('ref_axis',(0.,0.,-1.));
#66665=DIRECTION('center_axis',(1.,0.,0.));
#66666=DIRECTION('ref_axis',(0.,0.,-1.));
#66667=DIRECTION('center_axis',(1.,0.,0.));
#66668=DIRECTION('ref_axis',(0.,0.,-1.));
#66669=DIRECTION('center_axis',(1.,0.,0.));
#66670=DIRECTION('ref_axis',(0.,0.,-1.));
#66671=DIRECTION('center_axis',(1.,0.,0.));
#66672=DIRECTION('ref_axis',(0.,0.,-1.));
#66673=DIRECTION('center_axis',(1.,0.,0.));
#66674=DIRECTION('ref_axis',(0.,0.,-1.));
#66675=DIRECTION('center_axis',(1.,0.,0.));
#66676=DIRECTION('ref_axis',(0.,0.,-1.));
#66677=DIRECTION('center_axis',(1.,0.,0.));
#66678=DIRECTION('ref_axis',(0.,0.,-1.));
#66679=DIRECTION('center_axis',(1.,0.,0.));
#66680=DIRECTION('ref_axis',(0.,0.,-1.));
#66681=DIRECTION('center_axis',(1.,0.,0.));
#66682=DIRECTION('ref_axis',(0.,0.,-1.));
#66683=DIRECTION('center_axis',(1.,0.,0.));
#66684=DIRECTION('ref_axis',(0.,0.,-1.));
#66685=DIRECTION('center_axis',(1.,0.,0.));
#66686=DIRECTION('ref_axis',(0.,0.,-1.));
#66687=DIRECTION('center_axis',(1.,0.,0.));
#66688=DIRECTION('ref_axis',(0.,0.,-1.));
#66689=DIRECTION('center_axis',(1.,0.,0.));
#66690=DIRECTION('ref_axis',(0.,0.,-1.));
#66691=DIRECTION('center_axis',(1.,0.,0.));
#66692=DIRECTION('ref_axis',(0.,0.,-1.));
#66693=DIRECTION('center_axis',(1.,0.,0.));
#66694=DIRECTION('ref_axis',(0.,0.,-1.));
#66695=DIRECTION('center_axis',(1.,0.,0.));
#66696=DIRECTION('ref_axis',(0.,0.,-1.));
#66697=DIRECTION('',(-1.,0.,0.));
#66698=DIRECTION('center_axis',(1.,0.,0.));
#66699=DIRECTION('ref_axis',(0.,0.,-1.));
#66700=DIRECTION('center_axis',(1.,0.,0.));
#66701=DIRECTION('ref_axis',(0.,0.,-1.));
#66702=DIRECTION('center_axis',(1.,0.,0.));
#66703=DIRECTION('ref_axis',(0.,0.,-1.));
#66704=DIRECTION('center_axis',(1.,0.,0.));
#66705=DIRECTION('ref_axis',(0.,0.,-1.));
#66706=DIRECTION('center_axis',(1.,0.,0.));
#66707=DIRECTION('ref_axis',(0.,0.,-1.));
#66708=DIRECTION('center_axis',(1.,0.,0.));
#66709=DIRECTION('ref_axis',(0.,0.,-1.));
#66710=DIRECTION('center_axis',(1.,0.,0.));
#66711=DIRECTION('ref_axis',(0.,0.,-1.));
#66712=DIRECTION('center_axis',(1.,0.,0.));
#66713=DIRECTION('ref_axis',(0.,0.,-1.));
#66714=DIRECTION('center_axis',(1.,0.,0.));
#66715=DIRECTION('ref_axis',(0.,0.,-1.));
#66716=DIRECTION('center_axis',(1.,0.,0.));
#66717=DIRECTION('ref_axis',(0.,0.,-1.));
#66718=DIRECTION('center_axis',(1.,0.,0.));
#66719=DIRECTION('ref_axis',(0.,0.,-1.));
#66720=DIRECTION('center_axis',(1.,0.,0.));
#66721=DIRECTION('ref_axis',(0.,0.,-1.));
#66722=DIRECTION('center_axis',(1.,0.,0.));
#66723=DIRECTION('ref_axis',(0.,0.,-1.));
#66724=DIRECTION('center_axis',(1.,0.,0.));
#66725=DIRECTION('ref_axis',(0.,0.,-1.));
#66726=DIRECTION('center_axis',(1.,0.,0.));
#66727=DIRECTION('ref_axis',(0.,0.,-1.));
#66728=DIRECTION('center_axis',(1.,0.,0.));
#66729=DIRECTION('ref_axis',(0.,0.,-1.));
#66730=DIRECTION('center_axis',(1.,0.,0.));
#66731=DIRECTION('ref_axis',(0.,0.,-1.));
#66732=DIRECTION('center_axis',(1.,0.,0.));
#66733=DIRECTION('ref_axis',(0.,0.,-1.));
#66734=DIRECTION('center_axis',(1.,0.,0.));
#66735=DIRECTION('ref_axis',(0.,0.,-1.));
#66736=DIRECTION('center_axis',(-1.,0.,0.));
#66737=DIRECTION('ref_axis',(0.,1.,0.));
#66738=DIRECTION('center_axis',(1.,0.,0.));
#66739=DIRECTION('ref_axis',(0.,0.,-1.));
#66740=DIRECTION('',(-0.707106781186547,-0.707106781186548,-8.65956056235494E-17));
#66741=DIRECTION('center_axis',(1.,0.,0.));
#66742=DIRECTION('ref_axis',(0.,0.,-1.));
#66743=DIRECTION('axis',(0.,0.,1.));
#66744=DIRECTION('refdir',(1.,0.,0.));
#66745=DIRECTION('center_axis',(1.,0.,0.));
#66746=DIRECTION('ref_axis',(0.,1.,0.));
#66747=DIRECTION('center_axis',(1.,0.,0.));
#66748=DIRECTION('ref_axis',(0.,0.,-1.));
#66749=DIRECTION('',(-0.707106781186549,0.707106781186546,8.65956056235492E-17));
#66750=DIRECTION('center_axis',(1.,0.,0.));
#66751=DIRECTION('ref_axis',(0.,0.,-1.));
#66752=DIRECTION('center_axis',(1.,0.,0.));
#66753=DIRECTION('ref_axis',(0.,1.,0.));
#66754=DIRECTION('center_axis',(1.,0.,0.));
#66755=DIRECTION('ref_axis',(0.,0.,-1.));
#66756=DIRECTION('',(-1.,0.,0.));
#66757=DIRECTION('center_axis',(-1.,0.,0.));
#66758=DIRECTION('ref_axis',(0.,1.,0.));
#66759=DIRECTION('center_axis',(1.,0.,0.));
#66760=DIRECTION('ref_axis',(0.,0.,-1.));
#66761=DIRECTION('',(-0.707106781186549,-0.707106781186545,-8.65956056235491E-17));
#66762=DIRECTION('center_axis',(1.,0.,0.));
#66763=DIRECTION('ref_axis',(0.,0.,-1.));
#66764=DIRECTION('center_axis',(1.,0.,0.));
#66765=DIRECTION('ref_axis',(0.,0.,-1.));
#66766=DIRECTION('center_axis',(1.,0.,0.));
#66767=DIRECTION('ref_axis',(0.,1.,0.));
#66768=DIRECTION('',(-0.707106781186548,0.707106781186548,8.65956056235493E-17));
#66769=DIRECTION('center_axis',(1.,0.,0.));
#66770=DIRECTION('ref_axis',(0.,0.,-1.));
#66771=DIRECTION('center_axis',(1.,0.,0.));
#66772=DIRECTION('ref_axis',(0.,1.,0.));
#66773=DIRECTION('',(-1.,0.,0.));
#66774=DIRECTION('center_axis',(1.,0.,0.));
#66775=DIRECTION('ref_axis',(0.,0.,-1.));
#66776=DIRECTION('center_axis',(-1.,0.,0.));
#66777=DIRECTION('ref_axis',(0.,1.,0.));
#66778=DIRECTION('',(-0.707106781186547,-0.707106781186548,-8.65956056235494E-17));
#66779=DIRECTION('center_axis',(1.,0.,0.));
#66780=DIRECTION('ref_axis',(0.,0.,-1.));
#66781=DIRECTION('center_axis',(-1.,0.,0.));
#66782=DIRECTION('ref_axis',(0.,0.,1.));
#66783=DIRECTION('axis',(0.,0.,1.));
#66784=DIRECTION('refdir',(1.,0.,0.));
#66785=DIRECTION('center_axis',(1.,0.,0.));
#66786=DIRECTION('ref_axis',(0.,1.,0.));
#66787=DIRECTION('',(-1.,0.,0.));
#66788=DIRECTION('center_axis',(-1.,0.,0.));
#66789=DIRECTION('ref_axis',(0.,-1.,0.));
#66790=DIRECTION('center_axis',(0.5,-0.866025403784439,0.));
#66791=DIRECTION('ref_axis',(0.866025403784439,0.5,0.));
#66792=DIRECTION('center_axis',(1.,0.,0.));
#66793=DIRECTION('ref_axis',(0.,-1.,0.));
#66794=DIRECTION('center_axis',(1.,0.,0.));
#66795=DIRECTION('ref_axis',(0.,1.,0.));
#66796=DIRECTION('',(-1.,0.,0.));
#66797=DIRECTION('center_axis',(1.,0.,0.));
#66798=DIRECTION('ref_axis',(0.,-1.,0.));
#66799=DIRECTION('center_axis',(0.5,-0.866025403784439,0.));
#66800=DIRECTION('ref_axis',(0.866025403784439,0.5,0.));
#66801=DIRECTION('center_axis',(-1.,0.,0.));
#66802=DIRECTION('ref_axis',(0.,-1.,0.));
#66803=DIRECTION('center_axis',(-0.5,0.866025403784439,0.));
#66804=DIRECTION('ref_axis',(-0.866025403784439,-0.5,0.));
#66805=DIRECTION('',(0.,0.,-1.));
#66806=DIRECTION('center_axis',(-0.5,0.866025403784439,0.));
#66807=DIRECTION('ref_axis',(0.866025403784439,0.5,0.));
#66808=DIRECTION('',(0.,0.,1.));
#66809=DIRECTION('center_axis',(0.5,-0.866025403784439,0.));
#66810=DIRECTION('ref_axis',(0.866025403784439,0.5,0.));
#66811=DIRECTION('center_axis',(-0.5,0.866025403784439,0.));
#66812=DIRECTION('ref_axis',(0.866025403784439,0.5,0.));
#66813=DIRECTION('',(0.,0.,-1.));
#66814=DIRECTION('',(0.,0.,1.));
#66815=DIRECTION('center_axis',(1.,0.,0.));
#66816=DIRECTION('ref_axis',(0.,-0.00506609645795909,-0.999987167251));
#66817=DIRECTION('center_axis',(-1.,0.,0.));
#66818=DIRECTION('ref_axis',(0.,-1.,0.));
#66819=DIRECTION('center_axis',(1.,0.,0.));
#66820=DIRECTION('ref_axis',(0.,-1.,0.));
#66821=DIRECTION('center_axis',(1.,0.,0.));
#66822=DIRECTION('ref_axis',(0.,1.,0.));
#66823=DIRECTION('center_axis',(1.,0.,0.));
#66824=DIRECTION('ref_axis',(0.,-1.,0.));
#66825=DIRECTION('center_axis',(-1.,0.,0.));
#66826=DIRECTION('ref_axis',(0.,-0.13652151564835,-0.990637105990421));
#66827=DIRECTION('center_axis',(-1.,0.,0.));
#66828=DIRECTION('ref_axis',(0.,-1.,0.));
#66829=DIRECTION('center_axis',(1.,0.,0.));
#66830=DIRECTION('ref_axis',(0.,0.,-1.));
#66831=DIRECTION('center_axis',(1.,0.,0.));
#66832=DIRECTION('ref_axis',(0.,-1.,0.));
#66833=DIRECTION('center_axis',(1.,0.,0.));
#66834=DIRECTION('ref_axis',(0.,-0.212428563289972,-0.977176598931103));
#66835=DIRECTION('center_axis',(-1.,0.,0.));
#66836=DIRECTION('ref_axis',(0.,-1.,0.));
#66837=DIRECTION('center_axis',(1.,0.,0.));
#66838=DIRECTION('ref_axis',(0.,1.,0.));
#66839=DIRECTION('center_axis',(1.,0.,0.));
#66840=DIRECTION('ref_axis',(0.,-1.,0.));
#66841=DIRECTION('center_axis',(-1.,0.,0.));
#66842=DIRECTION('ref_axis',(0.,-0.0256854359394706,-0.999670074764969));
#66843=DIRECTION('center_axis',(-1.,0.,0.));
#66844=DIRECTION('ref_axis',(0.,-1.,0.));
#66845=DIRECTION('center_axis',(-1.,0.,0.));
#66846=DIRECTION('ref_axis',(0.,0.,1.));
#66847=DIRECTION('axis',(0.,0.,1.));
#66848=DIRECTION('refdir',(1.,0.,0.));
#66849=DIRECTION('center_axis',(1.,0.,0.));
#66850=DIRECTION('ref_axis',(0.,1.,0.));
#66851=DIRECTION('',(-1.,0.,0.));
#66852=DIRECTION('center_axis',(1.,0.,0.));
#66853=DIRECTION('ref_axis',(0.,1.,0.));
#66854=DIRECTION('center_axis',(1.,0.,0.));
#66855=DIRECTION('ref_axis',(0.,1.,0.));
#66856=DIRECTION('',(-1.,0.,0.));
#66857=DIRECTION('center_axis',(1.,0.,0.));
#66858=DIRECTION('ref_axis',(0.,1.,0.));
#66859=DIRECTION('',(-1.,0.,0.));
#66860=DIRECTION('center_axis',(1.,0.,0.));
#66861=DIRECTION('ref_axis',(0.,1.,0.));
#66862=DIRECTION('',(-1.,0.,0.));
#66863=DIRECTION('center_axis',(1.,0.,0.));
#66864=DIRECTION('ref_axis',(0.,1.,0.));
#66865=DIRECTION('',(-1.,0.,0.));
#66866=DIRECTION('center_axis',(1.,0.,0.));
#66867=DIRECTION('ref_axis',(0.,1.,0.));
#66868=DIRECTION('',(-1.,0.,0.));
#66869=DIRECTION('center_axis',(1.,0.,0.));
#66870=DIRECTION('ref_axis',(0.,1.,0.));
#66871=DIRECTION('',(-1.,0.,0.));
#66872=DIRECTION('center_axis',(1.,0.,0.));
#66873=DIRECTION('ref_axis',(0.,1.,0.));
#66874=DIRECTION('',(-1.,0.,0.));
#66875=DIRECTION('center_axis',(1.,0.,0.));
#66876=DIRECTION('ref_axis',(0.,1.,0.));
#66877=DIRECTION('',(-1.,0.,0.));
#66878=DIRECTION('center_axis',(1.,0.,0.));
#66879=DIRECTION('ref_axis',(0.,1.,0.));
#66880=DIRECTION('',(-1.,0.,0.));
#66881=DIRECTION('center_axis',(1.,0.,0.));
#66882=DIRECTION('ref_axis',(0.,1.,0.));
#66883=DIRECTION('',(-1.,0.,0.));
#66884=DIRECTION('center_axis',(1.,0.,0.));
#66885=DIRECTION('ref_axis',(0.,1.,0.));
#66886=DIRECTION('',(-1.,0.,0.));
#66887=DIRECTION('center_axis',(1.,0.,0.));
#66888=DIRECTION('ref_axis',(0.,1.,0.));
#66889=DIRECTION('',(-1.,0.,0.));
#66890=DIRECTION('center_axis',(1.,0.,0.));
#66891=DIRECTION('ref_axis',(0.,1.,0.));
#66892=DIRECTION('',(-1.,0.,0.));
#66893=DIRECTION('center_axis',(1.,0.,0.));
#66894=DIRECTION('ref_axis',(0.,1.,0.));
#66895=DIRECTION('',(-1.,0.,0.));
#66896=DIRECTION('center_axis',(1.,0.,0.));
#66897=DIRECTION('ref_axis',(0.,1.,0.));
#66898=DIRECTION('',(-1.,0.,0.));
#66899=DIRECTION('center_axis',(1.,0.,0.));
#66900=DIRECTION('ref_axis',(0.,1.,0.));
#66901=DIRECTION('center_axis',(1.,0.,0.));
#66902=DIRECTION('ref_axis',(0.,0.1768138132289,-0.984244316951566));
#66903=DIRECTION('',(1.,0.,0.));
#66904=DIRECTION('center_axis',(1.,0.,0.));
#66905=DIRECTION('ref_axis',(0.,1.,9.72557910080328E-14));
#66906=DIRECTION('center_axis',(1.,0.,0.));
#66907=DIRECTION('ref_axis',(0.,1.,9.72557910080328E-14));
#66908=DIRECTION('',(1.,0.,0.));
#66909=DIRECTION('center_axis',(1.,0.,0.));
#66910=DIRECTION('ref_axis',(0.,1.,9.72557910080328E-14));
#66911=DIRECTION('',(1.,0.,0.));
#66912=DIRECTION('center_axis',(1.,0.,0.));
#66913=DIRECTION('ref_axis',(0.,1.,9.72557910080328E-14));
#66914=DIRECTION('',(1.,0.,0.));
#66915=DIRECTION('center_axis',(1.,0.,0.));
#66916=DIRECTION('ref_axis',(0.,1.,9.72557910080328E-14));
#66917=DIRECTION('',(1.,0.,0.));
#66918=DIRECTION('center_axis',(1.,0.,0.));
#66919=DIRECTION('ref_axis',(0.,1.,9.72557910080328E-14));
#66920=DIRECTION('',(1.,0.,0.));
#66921=DIRECTION('center_axis',(1.,0.,0.));
#66922=DIRECTION('ref_axis',(0.,1.,9.72557910080328E-14));
#66923=DIRECTION('',(1.,0.,0.));
#66924=DIRECTION('center_axis',(1.,0.,0.));
#66925=DIRECTION('ref_axis',(0.,1.,9.72557910080328E-14));
#66926=DIRECTION('',(1.,0.,0.));
#66927=DIRECTION('center_axis',(1.,0.,0.));
#66928=DIRECTION('ref_axis',(0.,1.,9.72557910080328E-14));
#66929=DIRECTION('',(1.,0.,0.));
#66930=DIRECTION('center_axis',(1.,0.,0.));
#66931=DIRECTION('ref_axis',(0.,1.,9.72557910080328E-14));
#66932=DIRECTION('',(1.,0.,0.));
#66933=DIRECTION('center_axis',(1.,0.,0.));
#66934=DIRECTION('ref_axis',(0.,1.,9.72557910080328E-14));
#66935=DIRECTION('',(1.,0.,0.));
#66936=DIRECTION('center_axis',(1.,0.,0.));
#66937=DIRECTION('ref_axis',(0.,1.,9.72557910080328E-14));
#66938=DIRECTION('',(1.,0.,0.));
#66939=DIRECTION('center_axis',(1.,0.,0.));
#66940=DIRECTION('ref_axis',(0.,1.,9.72557910080328E-14));
#66941=DIRECTION('',(1.,0.,0.));
#66942=DIRECTION('center_axis',(1.,0.,0.));
#66943=DIRECTION('ref_axis',(0.,1.,9.72557910080328E-14));
#66944=DIRECTION('',(1.,0.,0.));
#66945=DIRECTION('center_axis',(1.,0.,0.));
#66946=DIRECTION('ref_axis',(0.,1.,9.72557910080328E-14));
#66947=DIRECTION('',(1.,0.,0.));
#66948=DIRECTION('center_axis',(1.,0.,0.));
#66949=DIRECTION('ref_axis',(0.,0.,-1.));
#66950=DIRECTION('center_axis',(1.,0.,0.));
#66951=DIRECTION('ref_axis',(0.,1.,0.));
#66952=DIRECTION('center_axis',(1.,0.,0.));
#66953=DIRECTION('ref_axis',(0.,1.,0.));
#66954=DIRECTION('center_axis',(1.,0.,0.));
#66955=DIRECTION('ref_axis',(0.,0.,-1.));
#66956=DIRECTION('center_axis',(1.,0.,0.));
#66957=DIRECTION('ref_axis',(0.,1.,0.));
#66958=DIRECTION('center_axis',(1.,0.,0.));
#66959=DIRECTION('ref_axis',(0.,1.,0.));
#66960=DIRECTION('center_axis',(-1.,0.,0.));
#66961=DIRECTION('ref_axis',(0.,1.,9.72557910080328E-14));
#66962=DIRECTION('center_axis',(1.,0.,0.));
#66963=DIRECTION('ref_axis',(0.,1.,9.72557910080328E-14));
#66964=DIRECTION('center_axis',(1.,0.,0.));
#66965=DIRECTION('ref_axis',(0.,0.,-1.));
#66966=DIRECTION('center_axis',(1.,0.,0.));
#66967=DIRECTION('ref_axis',(0.,1.,0.));
#66968=DIRECTION('center_axis',(0.,-1.,-1.22464679914735E-16));
#66969=DIRECTION('ref_axis',(0.,-1.22464679914735E-16,1.));
#66970=DIRECTION('center_axis',(-1.,0.,0.));
#66971=DIRECTION('ref_axis',(0.,1.,0.));
#66972=DIRECTION('center_axis',(1.,0.,0.));
#66973=DIRECTION('ref_axis',(0.,1.,0.));
#66974=DIRECTION('center_axis',(-1.,0.,0.));
#66975=DIRECTION('ref_axis',(0.,0.,1.));
#66976=DIRECTION('center_axis',(1.,0.,0.));
#66977=DIRECTION('ref_axis',(0.,0.,-1.));
#66978=DIRECTION('center_axis',(0.,-0.540769022303984,-0.841171126772902));
#66979=DIRECTION('ref_axis',(0.,0.841171126772902,-0.540769022303984));
#66980=DIRECTION('',(1.,0.,0.));
#66981=DIRECTION('',(0.,-0.841171126772902,0.540769022303984));
#66982=DIRECTION('',(1.,0.,0.));
#66983=DIRECTION('',(0.,0.841171126772902,-0.540769022303984));
#66984=DIRECTION('center_axis',(1.,0.,0.));
#66985=DIRECTION('ref_axis',(0.,-0.17364817766693,-0.984807753012208));
#66986=DIRECTION('center_axis',(1.,0.,0.));
#66987=DIRECTION('ref_axis',(0.,0.,-1.));
#66988=DIRECTION('',(0.,-0.975396199161154,-0.220459190468382));
#66989=DIRECTION('center_axis',(0.,-0.220459190468382,0.975396199161154));
#66990=DIRECTION('ref_axis',(0.,-0.975396199161154,-0.220459190468382));
#66991=DIRECTION('',(-1.,0.,0.));
#66992=DIRECTION('',(0.,0.975396199161154,0.220459190468382));
#66993=DIRECTION('center_axis',(1.,0.,0.));
#66994=DIRECTION('ref_axis',(0.,-0.17364817766693,-0.984807753012208));
#66995=DIRECTION('center_axis',(-1.,0.,0.));
#66996=DIRECTION('ref_axis',(0.,1.,0.));
#66997=DIRECTION('center_axis',(0.,-0.678621359023949,-0.734488291994154));
#66998=DIRECTION('ref_axis',(0.,0.734488291994153,-0.678621359023949));
#66999=DIRECTION('',(1.,0.,0.));
#67000=DIRECTION('',(0.,-0.734488291994153,0.678621359023949));
#67001=DIRECTION('',(1.,0.,0.));
#67002=DIRECTION('',(0.,0.734488291994153,-0.678621359023949));
#67003=DIRECTION('center_axis',(1.,0.,0.));
#67004=DIRECTION('ref_axis',(0.,-0.342020143325669,-0.939692620785908));
#67005=DIRECTION('center_axis',(1.,0.,0.));
#67006=DIRECTION('ref_axis',(0.,0.,-1.));
#67007=DIRECTION('',(0.,-0.998860075867306,-0.0477341475084725));
#67008=DIRECTION('center_axis',(0.,-0.0477341475084725,0.998860075867306));
#67009=DIRECTION('ref_axis',(0.,-0.998860075867306,-0.0477341475084725));
#67010=DIRECTION('',(-1.,0.,0.));
#67011=DIRECTION('',(0.,0.998860075867306,0.0477341475084725));
#67012=DIRECTION('center_axis',(1.,0.,0.));
#67013=DIRECTION('ref_axis',(0.,-0.342020143325669,-0.939692620785908));
#67014=DIRECTION('center_axis',(-1.,0.,0.));
#67015=DIRECTION('ref_axis',(0.,1.,0.));
#67016=DIRECTION('center_axis',(0.,-0.795854129148947,-0.605488402132173));
#67017=DIRECTION('ref_axis',(0.,0.605488402132173,-0.795854129148947));
#67018=DIRECTION('',(1.,0.,0.));
#67019=DIRECTION('',(0.,-0.605488402132173,0.795854129148947));
#67020=DIRECTION('',(1.,0.,0.));
#67021=DIRECTION('',(0.,0.605488402132173,-0.795854129148947));
#67022=DIRECTION('center_axis',(1.,0.,0.));
#67023=DIRECTION('ref_axis',(0.,-0.5,-0.866025403784438));
#67024=DIRECTION('center_axis',(1.,0.,0.));
#67025=DIRECTION('ref_axis',(0.,0.,-1.));
#67026=DIRECTION('',(0.,-0.991974094615816,0.126441273368837));
#67027=DIRECTION('center_axis',(0.,0.126441273368837,0.991974094615816));
#67028=DIRECTION('ref_axis',(0.,-0.991974094615816,0.126441273368837));
#67029=DIRECTION('',(-1.,0.,0.));
#67030=DIRECTION('',(0.,0.991974094615816,-0.126441273368837));
#67031=DIRECTION('center_axis',(1.,0.,0.));
#67032=DIRECTION('ref_axis',(0.,-0.5,-0.866025403784438));
#67033=DIRECTION('center_axis',(-1.,0.,0.));
#67034=DIRECTION('ref_axis',(0.,1.,0.));
#67035=DIRECTION('center_axis',(0.,-0.888905274281375,-0.458091053563321));
#67036=DIRECTION('ref_axis',(0.,0.458091053563321,-0.888905274281375));
#67037=DIRECTION('',(1.,0.,0.));
#67038=DIRECTION('',(0.,-0.458091053563321,0.888905274281375));
#67039=DIRECTION('',(1.,0.,0.));
#67040=DIRECTION('',(0.,0.458091053563321,-0.888905274281375));
#67041=DIRECTION('center_axis',(1.,0.,0.));
#67042=DIRECTION('ref_axis',(0.,-0.64278760968654,-0.766044443118978));
#67043=DIRECTION('center_axis',(1.,0.,0.));
#67044=DIRECTION('ref_axis',(0.,0.,-1.));
#67045=DIRECTION('',(0.,-0.954947482462536,0.296774840137206));
#67046=DIRECTION('center_axis',(0.,0.296774840137206,0.954947482462536));
#67047=DIRECTION('ref_axis',(0.,-0.954947482462536,0.296774840137206));
#67048=DIRECTION('',(-1.,0.,0.));
#67049=DIRECTION('',(0.,0.954947482462536,-0.296774840137206));
#67050=DIRECTION('center_axis',(1.,0.,0.));
#67051=DIRECTION('ref_axis',(0.,-0.64278760968654,-0.766044443118978));
#67052=DIRECTION('center_axis',(-1.,0.,0.));
#67053=DIRECTION('ref_axis',(0.,1.,0.));
#67054=DIRECTION('center_axis',(0.,-0.954947482462536,-0.296774840137206));
#67055=DIRECTION('ref_axis',(0.,0.296774840137206,-0.954947482462536));
#67056=DIRECTION('',(1.,0.,0.));
#67057=DIRECTION('',(0.,-0.296774840137206,0.954947482462536));
#67058=DIRECTION('',(1.,0.,0.));
#67059=DIRECTION('',(0.,0.296774840137206,-0.954947482462536));
#67060=DIRECTION('center_axis',(1.,0.,0.));
#67061=DIRECTION('ref_axis',(0.,-0.766044443118978,-0.642787609686539));
#67062=DIRECTION('center_axis',(1.,0.,0.));
#67063=DIRECTION('ref_axis',(0.,0.,-1.));
#67064=DIRECTION('',(0.,-0.888905274281375,0.458091053563321));
#67065=DIRECTION('center_axis',(0.,0.458091053563321,0.888905274281375));
#67066=DIRECTION('ref_axis',(0.,-0.888905274281375,0.458091053563321));
#67067=DIRECTION('',(-1.,0.,0.));
#67068=DIRECTION('',(0.,0.888905274281375,-0.458091053563321));
#67069=DIRECTION('center_axis',(1.,0.,0.));
#67070=DIRECTION('ref_axis',(0.,-0.766044443118978,-0.642787609686539));
#67071=DIRECTION('center_axis',(-1.,0.,0.));
#67072=DIRECTION('ref_axis',(0.,1.,0.));
#67073=DIRECTION('center_axis',(0.,-0.991974094615816,-0.126441273368837));
#67074=DIRECTION('ref_axis',(0.,0.126441273368837,-0.991974094615816));
#67075=DIRECTION('',(1.,0.,0.));
#67076=DIRECTION('',(0.,-0.126441273368837,0.991974094615816));
#67077=DIRECTION('',(1.,0.,0.));
#67078=DIRECTION('',(0.,0.126441273368837,-0.991974094615816));
#67079=DIRECTION('center_axis',(1.,0.,0.));
#67080=DIRECTION('ref_axis',(0.,-0.866025403784439,-0.5));
#67081=DIRECTION('center_axis',(1.,0.,0.));
#67082=DIRECTION('ref_axis',(0.,0.,-1.));
#67083=DIRECTION('',(0.,-0.795854129148946,0.605488402132173));
#67084=DIRECTION('center_axis',(0.,0.605488402132173,0.795854129148946));
#67085=DIRECTION('ref_axis',(0.,-0.795854129148946,0.605488402132173));
#67086=DIRECTION('',(-1.,0.,0.));
#67087=DIRECTION('',(0.,0.795854129148946,-0.605488402132173));
#67088=DIRECTION('center_axis',(1.,0.,0.));
#67089=DIRECTION('ref_axis',(0.,-0.866025403784439,-0.5));
#67090=DIRECTION('center_axis',(-1.,0.,0.));
#67091=DIRECTION('ref_axis',(0.,1.,0.));
#67092=DIRECTION('center_axis',(0.,-0.998860075867306,0.0477341475084739));
#67093=DIRECTION('ref_axis',(0.,-0.0477341475084739,-0.998860075867306));
#67094=DIRECTION('',(1.,0.,0.));
#67095=DIRECTION('',(0.,0.0477341475084739,0.998860075867306));
#67096=DIRECTION('',(1.,0.,0.));
#67097=DIRECTION('',(0.,-0.0477341475084739,-0.998860075867306));
#67098=DIRECTION('center_axis',(1.,0.,0.));
#67099=DIRECTION('ref_axis',(0.,-0.939692620785909,-0.342020143325668));
#67100=DIRECTION('center_axis',(1.,0.,0.));
#67101=DIRECTION('ref_axis',(0.,0.,-1.));
#67102=DIRECTION('',(0.,-0.678621359023948,0.734488291994154));
#67103=DIRECTION('center_axis',(0.,0.734488291994154,0.678621359023948));
#67104=DIRECTION('ref_axis',(0.,-0.678621359023948,0.734488291994154));
#67105=DIRECTION('',(-1.,0.,0.));
#67106=DIRECTION('',(0.,0.678621359023948,-0.734488291994154));
#67107=DIRECTION('center_axis',(1.,0.,0.));
#67108=DIRECTION('ref_axis',(0.,-0.939692620785909,-0.342020143325668));
#67109=DIRECTION('center_axis',(-1.,0.,0.));
#67110=DIRECTION('ref_axis',(0.,1.,0.));
#67111=DIRECTION('center_axis',(0.,-0.975396199161154,0.220459190468383));
#67112=DIRECTION('ref_axis',(0.,-0.220459190468383,-0.975396199161154));
#67113=DIRECTION('',(1.,0.,0.));
#67114=DIRECTION('',(0.,0.220459190468383,0.975396199161154));
#67115=DIRECTION('',(1.,0.,0.));
#67116=DIRECTION('',(0.,-0.220459190468383,-0.975396199161154));
#67117=DIRECTION('center_axis',(1.,0.,0.));
#67118=DIRECTION('ref_axis',(0.,-0.984807753012208,-0.17364817766693));
#67119=DIRECTION('center_axis',(1.,0.,0.));
#67120=DIRECTION('ref_axis',(0.,0.,-1.));
#67121=DIRECTION('',(0.,-0.540769022303984,0.841171126772902));
#67122=DIRECTION('center_axis',(0.,0.841171126772902,0.540769022303984));
#67123=DIRECTION('ref_axis',(0.,-0.540769022303984,0.841171126772902));
#67124=DIRECTION('',(-1.,0.,0.));
#67125=DIRECTION('',(0.,0.540769022303984,-0.841171126772902));
#67126=DIRECTION('center_axis',(1.,0.,0.));
#67127=DIRECTION('ref_axis',(0.,-0.984807753012208,-0.17364817766693));
#67128=DIRECTION('center_axis',(-1.,0.,0.));
#67129=DIRECTION('ref_axis',(0.,1.,0.));
#67130=DIRECTION('center_axis',(0.,-0.922295402517783,0.386485692483643));
#67131=DIRECTION('ref_axis',(0.,-0.386485692483643,-0.922295402517783));
#67132=DIRECTION('',(1.,0.,0.));
#67133=DIRECTION('',(0.,0.386485692483643,0.922295402517783));
#67134=DIRECTION('',(1.,0.,0.));
#67135=DIRECTION('',(0.,-0.386485692483643,-0.922295402517783));
#67136=DIRECTION('center_axis',(1.,0.,0.));
#67137=DIRECTION('ref_axis',(0.,-1.,1.83697019872103E-16));
#67138=DIRECTION('center_axis',(1.,0.,0.));
#67139=DIRECTION('ref_axis',(0.,0.,-1.));
#67140=DIRECTION('',(0.,-0.386485692483642,0.922295402517783));
#67141=DIRECTION('center_axis',(0.,0.922295402517783,0.386485692483642));
#67142=DIRECTION('ref_axis',(0.,-0.386485692483642,0.922295402517783));
#67143=DIRECTION('',(-1.,0.,0.));
#67144=DIRECTION('',(0.,0.386485692483642,-0.922295402517783));
#67145=DIRECTION('center_axis',(1.,0.,0.));
#67146=DIRECTION('ref_axis',(0.,-1.,1.83697019872103E-16));
#67147=DIRECTION('center_axis',(-1.,0.,0.));
#67148=DIRECTION('ref_axis',(0.,1.,0.));
#67149=DIRECTION('center_axis',(0.,-0.841171126772902,0.540769022303984));
#67150=DIRECTION('ref_axis',(0.,-0.540769022303984,-0.841171126772902));
#67151=DIRECTION('',(1.,0.,0.));
#67152=DIRECTION('',(0.,0.540769022303984,0.841171126772902));
#67153=DIRECTION('',(1.,0.,0.));
#67154=DIRECTION('',(0.,-0.540769022303984,-0.841171126772902));
#67155=DIRECTION('center_axis',(1.,0.,0.));
#67156=DIRECTION('ref_axis',(0.,-0.984807753012208,0.17364817766693));
#67157=DIRECTION('center_axis',(1.,0.,0.));
#67158=DIRECTION('ref_axis',(0.,0.,-1.));
#67159=DIRECTION('',(0.,-0.220459190468382,0.975396199161154));
#67160=DIRECTION('center_axis',(0.,0.975396199161154,0.220459190468382));
#67161=DIRECTION('ref_axis',(0.,-0.220459190468382,0.975396199161154));
#67162=DIRECTION('',(-1.,0.,0.));
#67163=DIRECTION('',(0.,0.220459190468382,-0.975396199161154));
#67164=DIRECTION('center_axis',(1.,0.,0.));
#67165=DIRECTION('ref_axis',(0.,-0.984807753012208,0.17364817766693));
#67166=DIRECTION('center_axis',(-1.,0.,0.));
#67167=DIRECTION('ref_axis',(0.,1.,0.));
#67168=DIRECTION('center_axis',(0.,-0.734488291994154,0.678621359023949));
#67169=DIRECTION('ref_axis',(0.,-0.678621359023949,-0.734488291994154));
#67170=DIRECTION('',(1.,0.,0.));
#67171=DIRECTION('',(0.,0.678621359023949,0.734488291994154));
#67172=DIRECTION('',(1.,0.,0.));
#67173=DIRECTION('',(0.,-0.678621359023949,-0.734488291994154));
#67174=DIRECTION('center_axis',(1.,0.,0.));
#67175=DIRECTION('ref_axis',(0.,-0.939692620785908,0.342020143325669));
#67176=DIRECTION('center_axis',(1.,0.,0.));
#67177=DIRECTION('ref_axis',(0.,0.,-1.));
#67178=DIRECTION('',(0.,-0.0477341475084726,0.998860075867306));
#67179=DIRECTION('center_axis',(0.,0.998860075867306,0.0477341475084726));
#67180=DIRECTION('ref_axis',(0.,-0.0477341475084726,0.998860075867306));
#67181=DIRECTION('',(-1.,0.,0.));
#67182=DIRECTION('',(0.,0.0477341475084726,-0.998860075867306));
#67183=DIRECTION('center_axis',(1.,0.,0.));
#67184=DIRECTION('ref_axis',(0.,-0.939692620785908,0.342020143325669));
#67185=DIRECTION('center_axis',(-1.,0.,0.));
#67186=DIRECTION('ref_axis',(0.,1.,0.));
#67187=DIRECTION('center_axis',(0.,-0.605488402132173,0.795854129148947));
#67188=DIRECTION('ref_axis',(0.,-0.795854129148947,-0.605488402132173));
#67189=DIRECTION('',(1.,0.,0.));
#67190=DIRECTION('',(0.,0.795854129148947,0.605488402132173));
#67191=DIRECTION('',(1.,0.,0.));
#67192=DIRECTION('',(0.,-0.795854129148947,-0.605488402132173));
#67193=DIRECTION('center_axis',(1.,0.,0.));
#67194=DIRECTION('ref_axis',(0.,-0.866025403784438,0.5));
#67195=DIRECTION('center_axis',(1.,0.,0.));
#67196=DIRECTION('ref_axis',(0.,0.,-1.));
#67197=DIRECTION('',(0.,0.126441273368837,0.991974094615816));
#67198=DIRECTION('center_axis',(0.,0.991974094615816,-0.126441273368837));
#67199=DIRECTION('ref_axis',(0.,0.126441273368837,0.991974094615816));
#67200=DIRECTION('',(-1.,0.,0.));
#67201=DIRECTION('',(0.,-0.126441273368837,-0.991974094615816));
#67202=DIRECTION('center_axis',(1.,0.,0.));
#67203=DIRECTION('ref_axis',(0.,-0.866025403784438,0.5));
#67204=DIRECTION('center_axis',(-1.,0.,0.));
#67205=DIRECTION('ref_axis',(0.,1.,0.));
#67206=DIRECTION('center_axis',(0.,-0.458091053563321,0.888905274281375));
#67207=DIRECTION('ref_axis',(0.,-0.888905274281375,-0.458091053563321));
#67208=DIRECTION('',(1.,0.,0.));
#67209=DIRECTION('',(0.,0.888905274281375,0.458091053563321));
#67210=DIRECTION('',(1.,0.,0.));
#67211=DIRECTION('',(0.,-0.888905274281375,-0.458091053563321));
#67212=DIRECTION('center_axis',(1.,0.,0.));
#67213=DIRECTION('ref_axis',(0.,-0.766044443118978,0.642787609686539));
#67214=DIRECTION('center_axis',(1.,0.,0.));
#67215=DIRECTION('ref_axis',(0.,0.,-1.));
#67216=DIRECTION('',(0.,0.296774840137206,0.954947482462536));
#67217=DIRECTION('center_axis',(0.,0.954947482462536,-0.296774840137206));
#67218=DIRECTION('ref_axis',(0.,0.296774840137206,0.954947482462536));
#67219=DIRECTION('',(-1.,0.,0.));
#67220=DIRECTION('',(0.,-0.296774840137206,-0.954947482462536));
#67221=DIRECTION('center_axis',(1.,0.,0.));
#67222=DIRECTION('ref_axis',(0.,-0.766044443118978,0.642787609686539));
#67223=DIRECTION('center_axis',(-1.,0.,0.));
#67224=DIRECTION('ref_axis',(0.,1.,0.));
#67225=DIRECTION('center_axis',(0.,-0.296774840137206,0.954947482462536));
#67226=DIRECTION('ref_axis',(0.,-0.954947482462536,-0.296774840137206));
#67227=DIRECTION('',(1.,0.,0.));
#67228=DIRECTION('',(0.,0.954947482462536,0.296774840137206));
#67229=DIRECTION('',(1.,0.,0.));
#67230=DIRECTION('',(0.,-0.954947482462536,-0.296774840137206));
#67231=DIRECTION('center_axis',(1.,0.,0.));
#67232=DIRECTION('ref_axis',(0.,-0.642787609686539,0.766044443118978));
#67233=DIRECTION('center_axis',(1.,0.,0.));
#67234=DIRECTION('ref_axis',(0.,0.,-1.));
#67235=DIRECTION('',(0.,0.458091053563321,0.888905274281375));
#67236=DIRECTION('center_axis',(0.,0.888905274281375,-0.458091053563321));
#67237=DIRECTION('ref_axis',(0.,0.458091053563321,0.888905274281375));
#67238=DIRECTION('',(-1.,0.,0.));
#67239=DIRECTION('',(0.,-0.458091053563321,-0.888905274281375));
#67240=DIRECTION('center_axis',(1.,0.,0.));
#67241=DIRECTION('ref_axis',(0.,-0.642787609686539,0.766044443118978));
#67242=DIRECTION('center_axis',(-1.,0.,0.));
#67243=DIRECTION('ref_axis',(0.,1.,0.));
#67244=DIRECTION('center_axis',(0.,-0.126441273368836,0.991974094615816));
#67245=DIRECTION('ref_axis',(0.,-0.991974094615816,-0.126441273368836));
#67246=DIRECTION('',(1.,0.,0.));
#67247=DIRECTION('',(0.,0.991974094615816,0.126441273368836));
#67248=DIRECTION('',(1.,0.,0.));
#67249=DIRECTION('',(0.,-0.991974094615816,-0.126441273368836));
#67250=DIRECTION('center_axis',(1.,0.,0.));
#67251=DIRECTION('ref_axis',(0.,-0.5,0.866025403784439));
#67252=DIRECTION('center_axis',(1.,0.,0.));
#67253=DIRECTION('ref_axis',(0.,0.,-1.));
#67254=DIRECTION('',(0.,0.605488402132173,0.795854129148946));
#67255=DIRECTION('center_axis',(0.,0.795854129148946,-0.605488402132173));
#67256=DIRECTION('ref_axis',(0.,0.605488402132173,0.795854129148946));
#67257=DIRECTION('',(-1.,0.,0.));
#67258=DIRECTION('',(0.,-0.605488402132173,-0.795854129148946));
#67259=DIRECTION('center_axis',(1.,0.,0.));
#67260=DIRECTION('ref_axis',(0.,-0.5,0.866025403784439));
#67261=DIRECTION('center_axis',(-1.,0.,0.));
#67262=DIRECTION('ref_axis',(0.,1.,0.));
#67263=DIRECTION('center_axis',(0.,0.0477341475084734,0.998860075867306));
#67264=DIRECTION('ref_axis',(0.,-0.998860075867306,0.0477341475084734));
#67265=DIRECTION('',(1.,0.,0.));
#67266=DIRECTION('',(0.,0.998860075867306,-0.0477341475084734));
#67267=DIRECTION('',(1.,0.,0.));
#67268=DIRECTION('',(0.,-0.998860075867306,0.0477341475084734));
#67269=DIRECTION('center_axis',(1.,0.,0.));
#67270=DIRECTION('ref_axis',(0.,-0.342020143325669,0.939692620785909));
#67271=DIRECTION('center_axis',(1.,0.,0.));
#67272=DIRECTION('ref_axis',(0.,0.,-1.));
#67273=DIRECTION('',(0.,0.734488291994154,0.678621359023948));
#67274=DIRECTION('center_axis',(0.,0.678621359023948,-0.734488291994154));
#67275=DIRECTION('ref_axis',(0.,0.734488291994154,0.678621359023948));
#67276=DIRECTION('',(-1.,0.,0.));
#67277=DIRECTION('',(0.,-0.734488291994154,-0.678621359023948));
#67278=DIRECTION('center_axis',(1.,0.,0.));
#67279=DIRECTION('ref_axis',(0.,-0.342020143325669,0.939692620785909));
#67280=DIRECTION('center_axis',(-1.,0.,0.));
#67281=DIRECTION('ref_axis',(0.,1.,0.));
#67282=DIRECTION('center_axis',(0.,0.220459190468383,0.975396199161154));
#67283=DIRECTION('ref_axis',(0.,-0.975396199161154,0.220459190468383));
#67284=DIRECTION('',(1.,0.,0.));
#67285=DIRECTION('',(0.,0.975396199161154,-0.220459190468383));
#67286=DIRECTION('',(1.,0.,0.));
#67287=DIRECTION('',(0.,-0.975396199161154,0.220459190468383));
#67288=DIRECTION('center_axis',(1.,0.,0.));
#67289=DIRECTION('ref_axis',(0.,-0.17364817766693,0.984807753012208));
#67290=DIRECTION('center_axis',(1.,0.,0.));
#67291=DIRECTION('ref_axis',(0.,0.,-1.));
#67292=DIRECTION('',(0.,0.841171126772902,0.540769022303984));
#67293=DIRECTION('center_axis',(0.,0.540769022303984,-0.841171126772902));
#67294=DIRECTION('ref_axis',(0.,0.841171126772902,0.540769022303984));
#67295=DIRECTION('',(-1.,0.,0.));
#67296=DIRECTION('',(0.,-0.841171126772902,-0.540769022303984));
#67297=DIRECTION('center_axis',(1.,0.,0.));
#67298=DIRECTION('ref_axis',(0.,-0.17364817766693,0.984807753012208));
#67299=DIRECTION('center_axis',(-1.,0.,0.));
#67300=DIRECTION('ref_axis',(0.,1.,0.));
#67301=DIRECTION('center_axis',(0.,0.386485692483643,0.922295402517783));
#67302=DIRECTION('ref_axis',(0.,-0.922295402517783,0.386485692483643));
#67303=DIRECTION('',(1.,0.,0.));
#67304=DIRECTION('',(0.,0.922295402517783,-0.386485692483643));
#67305=DIRECTION('',(1.,0.,0.));
#67306=DIRECTION('',(0.,-0.922295402517783,0.386485692483643));
#67307=DIRECTION('center_axis',(1.,0.,0.));
#67308=DIRECTION('ref_axis',(0.,1.22464679914735E-16,1.));
#67309=DIRECTION('center_axis',(1.,0.,0.));
#67310=DIRECTION('ref_axis',(0.,0.,-1.));
#67311=DIRECTION('',(0.,0.922295402517783,0.386485692483642));
#67312=DIRECTION('center_axis',(1.,0.,0.));
#67313=DIRECTION('ref_axis',(0.,0.,-1.));
#67314=DIRECTION('center_axis',(0.,0.386485692483643,-0.922295402517783));
#67315=DIRECTION('ref_axis',(0.,0.922295402517783,0.386485692483642));
#67316=DIRECTION('',(-1.,0.,0.));
#67317=DIRECTION('',(0.,-0.922295402517783,-0.386485692483642));
#67318=DIRECTION('center_axis',(1.,0.,0.));
#67319=DIRECTION('ref_axis',(0.,1.22464679914735E-16,1.));
#67320=DIRECTION('center_axis',(-1.,0.,0.));
#67321=DIRECTION('ref_axis',(0.,1.,0.));
#67322=DIRECTION('center_axis',(-1.,0.,0.));
#67323=DIRECTION('ref_axis',(0.,1.,0.));
#67324=DIRECTION('center_axis',(0.,0.540769022303985,0.841171126772901));
#67325=DIRECTION('ref_axis',(0.,-0.841171126772902,0.540769022303985));
#67326=DIRECTION('',(1.,0.,0.));
#67327=DIRECTION('',(0.,0.841171126772902,-0.540769022303985));
#67328=DIRECTION('',(1.,0.,0.));
#67329=DIRECTION('',(0.,-0.841171126772902,0.540769022303985));
#67330=DIRECTION('center_axis',(1.,0.,0.));
#67331=DIRECTION('ref_axis',(0.,0.173648177666931,0.984807753012208));
#67332=DIRECTION('center_axis',(1.,0.,0.));
#67333=DIRECTION('ref_axis',(0.,0.,-1.));
#67334=DIRECTION('',(0.,0.975396199161154,0.220459190468382));
#67335=DIRECTION('center_axis',(0.,0.220459190468382,-0.975396199161154));
#67336=DIRECTION('ref_axis',(0.,0.975396199161154,0.220459190468382));
#67337=DIRECTION('',(-1.,0.,0.));
#67338=DIRECTION('',(0.,-0.975396199161154,-0.220459190468382));
#67339=DIRECTION('center_axis',(1.,0.,0.));
#67340=DIRECTION('ref_axis',(0.,0.173648177666931,0.984807753012208));
#67341=DIRECTION('center_axis',(-1.,0.,0.));
#67342=DIRECTION('ref_axis',(0.,1.,0.));
#67343=DIRECTION('center_axis',(0.,0.678621359023948,0.734488291994154));
#67344=DIRECTION('ref_axis',(0.,-0.734488291994154,0.678621359023948));
#67345=DIRECTION('',(1.,0.,0.));
#67346=DIRECTION('',(0.,0.734488291994154,-0.678621359023948));
#67347=DIRECTION('',(1.,0.,0.));
#67348=DIRECTION('',(0.,-0.734488291994154,0.678621359023948));
#67349=DIRECTION('center_axis',(1.,0.,0.));
#67350=DIRECTION('ref_axis',(0.,0.342020143325669,0.939692620785908));
#67351=DIRECTION('center_axis',(1.,0.,0.));
#67352=DIRECTION('ref_axis',(0.,0.,-1.));
#67353=DIRECTION('',(0.,0.998860075867306,0.0477341475084732));
#67354=DIRECTION('center_axis',(0.,0.0477341475084731,-0.998860075867306));
#67355=DIRECTION('ref_axis',(0.,0.998860075867306,0.0477341475084732));
#67356=DIRECTION('',(-1.,0.,0.));
#67357=DIRECTION('',(0.,-0.998860075867306,-0.0477341475084732));
#67358=DIRECTION('center_axis',(1.,0.,0.));
#67359=DIRECTION('ref_axis',(0.,0.342020143325669,0.939692620785908));
#67360=DIRECTION('center_axis',(-1.,0.,0.));
#67361=DIRECTION('ref_axis',(0.,1.,0.));
#67362=DIRECTION('center_axis',(0.,0.795854129148946,0.605488402132173));
#67363=DIRECTION('ref_axis',(0.,-0.605488402132173,0.795854129148946));
#67364=DIRECTION('',(1.,0.,0.));
#67365=DIRECTION('',(0.,0.605488402132173,-0.795854129148946));
#67366=DIRECTION('',(1.,0.,0.));
#67367=DIRECTION('',(0.,-0.605488402132173,0.795854129148946));
#67368=DIRECTION('center_axis',(1.,0.,0.));
#67369=DIRECTION('ref_axis',(0.,0.5,0.866025403784439));
#67370=DIRECTION('center_axis',(1.,0.,0.));
#67371=DIRECTION('ref_axis',(0.,0.,-1.));
#67372=DIRECTION('',(0.,0.991974094615816,-0.126441273368836));
#67373=DIRECTION('center_axis',(0.,-0.126441273368836,-0.991974094615816));
#67374=DIRECTION('ref_axis',(0.,0.991974094615816,-0.126441273368836));
#67375=DIRECTION('',(-1.,0.,0.));
#67376=DIRECTION('',(0.,-0.991974094615816,0.126441273368836));
#67377=DIRECTION('center_axis',(1.,0.,0.));
#67378=DIRECTION('ref_axis',(0.,0.5,0.866025403784439));
#67379=DIRECTION('center_axis',(-1.,0.,0.));
#67380=DIRECTION('ref_axis',(0.,1.,0.));
#67381=DIRECTION('center_axis',(0.,0.888905274281375,0.458091053563321));
#67382=DIRECTION('ref_axis',(0.,-0.458091053563321,0.888905274281375));
#67383=DIRECTION('',(1.,0.,0.));
#67384=DIRECTION('',(0.,0.458091053563321,-0.888905274281375));
#67385=DIRECTION('',(1.,0.,0.));
#67386=DIRECTION('',(0.,-0.458091053563321,0.888905274281375));
#67387=DIRECTION('center_axis',(1.,0.,0.));
#67388=DIRECTION('ref_axis',(0.,0.642787609686539,0.766044443118978));
#67389=DIRECTION('center_axis',(1.,0.,0.));
#67390=DIRECTION('ref_axis',(0.,0.,-1.));
#67391=DIRECTION('',(0.,0.954947482462536,-0.296774840137206));
#67392=DIRECTION('center_axis',(0.,-0.296774840137206,-0.954947482462536));
#67393=DIRECTION('ref_axis',(0.,0.954947482462536,-0.296774840137206));
#67394=DIRECTION('',(-1.,0.,0.));
#67395=DIRECTION('',(0.,-0.954947482462536,0.296774840137206));
#67396=DIRECTION('center_axis',(1.,0.,0.));
#67397=DIRECTION('ref_axis',(0.,0.642787609686539,0.766044443118978));
#67398=DIRECTION('center_axis',(-1.,0.,0.));
#67399=DIRECTION('ref_axis',(0.,1.,0.));
#67400=DIRECTION('center_axis',(0.,0.954947482462536,0.296774840137206));
#67401=DIRECTION('ref_axis',(0.,-0.296774840137206,0.954947482462536));
#67402=DIRECTION('',(1.,0.,0.));
#67403=DIRECTION('',(0.,0.296774840137206,-0.954947482462536));
#67404=DIRECTION('',(1.,0.,0.));
#67405=DIRECTION('',(0.,-0.296774840137206,0.954947482462536));
#67406=DIRECTION('center_axis',(1.,0.,0.));
#67407=DIRECTION('ref_axis',(0.,0.766044443118978,0.642787609686539));
#67408=DIRECTION('center_axis',(1.,0.,0.));
#67409=DIRECTION('ref_axis',(0.,0.,-1.));
#67410=DIRECTION('',(0.,0.888905274281375,-0.458091053563321));
#67411=DIRECTION('center_axis',(0.,-0.458091053563321,-0.888905274281375));
#67412=DIRECTION('ref_axis',(0.,0.888905274281375,-0.458091053563321));
#67413=DIRECTION('',(-1.,0.,0.));
#67414=DIRECTION('',(0.,-0.888905274281375,0.458091053563321));
#67415=DIRECTION('center_axis',(1.,0.,0.));
#67416=DIRECTION('ref_axis',(0.,0.766044443118978,0.642787609686539));
#67417=DIRECTION('center_axis',(-1.,0.,0.));
#67418=DIRECTION('ref_axis',(0.,1.,0.));
#67419=DIRECTION('center_axis',(0.,0.991974094615816,0.126441273368836));
#67420=DIRECTION('ref_axis',(0.,-0.126441273368836,0.991974094615816));
#67421=DIRECTION('',(1.,0.,0.));
#67422=DIRECTION('',(0.,0.126441273368836,-0.991974094615816));
#67423=DIRECTION('',(1.,0.,0.));
#67424=DIRECTION('',(0.,-0.126441273368836,0.991974094615816));
#67425=DIRECTION('center_axis',(1.,0.,0.));
#67426=DIRECTION('ref_axis',(0.,0.866025403784439,0.5));
#67427=DIRECTION('center_axis',(1.,0.,0.));
#67428=DIRECTION('ref_axis',(0.,0.,-1.));
#67429=DIRECTION('',(0.,0.795854129148946,-0.605488402132173));
#67430=DIRECTION('center_axis',(0.,-0.605488402132173,-0.795854129148946));
#67431=DIRECTION('ref_axis',(0.,0.795854129148946,-0.605488402132173));
#67432=DIRECTION('',(-1.,0.,0.));
#67433=DIRECTION('',(0.,-0.795854129148946,0.605488402132173));
#67434=DIRECTION('center_axis',(1.,0.,0.));
#67435=DIRECTION('ref_axis',(0.,0.866025403784439,0.5));
#67436=DIRECTION('center_axis',(-1.,0.,0.));
#67437=DIRECTION('ref_axis',(0.,1.,0.));
#67438=DIRECTION('center_axis',(0.,0.998860075867306,-0.0477341475084733));
#67439=DIRECTION('ref_axis',(0.,0.0477341475084733,0.998860075867306));
#67440=DIRECTION('',(1.,0.,0.));
#67441=DIRECTION('',(0.,-0.0477341475084733,-0.998860075867306));
#67442=DIRECTION('',(1.,0.,0.));
#67443=DIRECTION('',(0.,0.0477341475084733,0.998860075867306));
#67444=DIRECTION('center_axis',(1.,0.,0.));
#67445=DIRECTION('ref_axis',(0.,0.939692620785908,0.342020143325669));
#67446=DIRECTION('center_axis',(1.,0.,0.));
#67447=DIRECTION('ref_axis',(0.,0.,-1.));
#67448=DIRECTION('',(0.,0.678621359023948,-0.734488291994154));
#67449=DIRECTION('center_axis',(0.,-0.734488291994154,-0.678621359023948));
#67450=DIRECTION('ref_axis',(0.,0.678621359023948,-0.734488291994154));
#67451=DIRECTION('',(-1.,0.,0.));
#67452=DIRECTION('',(0.,-0.678621359023948,0.734488291994154));
#67453=DIRECTION('center_axis',(1.,0.,0.));
#67454=DIRECTION('ref_axis',(0.,0.939692620785908,0.342020143325669));
#67455=DIRECTION('center_axis',(-1.,0.,0.));
#67456=DIRECTION('ref_axis',(0.,1.,0.));
#67457=DIRECTION('center_axis',(0.,0.975396199161154,-0.220459190468382));
#67458=DIRECTION('ref_axis',(0.,0.220459190468382,0.975396199161154));
#67459=DIRECTION('',(1.,0.,0.));
#67460=DIRECTION('',(0.,-0.220459190468382,-0.975396199161154));
#67461=DIRECTION('',(1.,0.,0.));
#67462=DIRECTION('',(0.,0.220459190468382,0.975396199161154));
#67463=DIRECTION('center_axis',(1.,0.,0.));
#67464=DIRECTION('ref_axis',(0.,0.984807753012208,0.17364817766693));
#67465=DIRECTION('center_axis',(1.,0.,0.));
#67466=DIRECTION('ref_axis',(0.,0.,-1.));
#67467=DIRECTION('',(0.,0.540769022303984,-0.841171126772902));
#67468=DIRECTION('center_axis',(0.,-0.841171126772902,-0.540769022303984));
#67469=DIRECTION('ref_axis',(0.,0.540769022303984,-0.841171126772902));
#67470=DIRECTION('',(-1.,0.,0.));
#67471=DIRECTION('',(0.,-0.540769022303984,0.841171126772902));
#67472=DIRECTION('center_axis',(1.,0.,0.));
#67473=DIRECTION('ref_axis',(0.,0.984807753012208,0.17364817766693));
#67474=DIRECTION('center_axis',(-1.,0.,0.));
#67475=DIRECTION('ref_axis',(0.,1.,0.));
#67476=DIRECTION('center_axis',(0.,0.922295402517783,-0.386485692483643));
#67477=DIRECTION('ref_axis',(0.,0.386485692483643,0.922295402517783));
#67478=DIRECTION('',(1.,0.,0.));
#67479=DIRECTION('',(0.,-0.386485692483643,-0.922295402517783));
#67480=DIRECTION('',(1.,0.,0.));
#67481=DIRECTION('',(0.,0.386485692483643,0.922295402517783));
#67482=DIRECTION('center_axis',(1.,0.,0.));
#67483=DIRECTION('ref_axis',(0.,1.,-6.12323399573677E-17));
#67484=DIRECTION('center_axis',(1.,0.,0.));
#67485=DIRECTION('ref_axis',(0.,0.,-1.));
#67486=DIRECTION('',(0.,0.386485692483643,-0.922295402517783));
#67487=DIRECTION('center_axis',(0.,-0.922295402517783,-0.386485692483643));
#67488=DIRECTION('ref_axis',(0.,0.386485692483643,-0.922295402517783));
#67489=DIRECTION('',(-1.,0.,0.));
#67490=DIRECTION('',(0.,-0.386485692483643,0.922295402517783));
#67491=DIRECTION('center_axis',(1.,0.,0.));
#67492=DIRECTION('ref_axis',(0.,1.,-6.12323399573677E-17));
#67493=DIRECTION('center_axis',(-1.,0.,0.));
#67494=DIRECTION('ref_axis',(0.,1.,0.));
#67495=DIRECTION('center_axis',(0.,0.841171126772902,-0.540769022303984));
#67496=DIRECTION('ref_axis',(0.,0.540769022303984,0.841171126772902));
#67497=DIRECTION('',(1.,0.,0.));
#67498=DIRECTION('',(0.,-0.540769022303984,-0.841171126772902));
#67499=DIRECTION('',(1.,0.,0.));
#67500=DIRECTION('',(0.,0.540769022303984,0.841171126772902));
#67501=DIRECTION('center_axis',(1.,0.,0.));
#67502=DIRECTION('ref_axis',(0.,0.984807753012208,-0.17364817766693));
#67503=DIRECTION('center_axis',(1.,0.,0.));
#67504=DIRECTION('ref_axis',(0.,0.,-1.));
#67505=DIRECTION('',(0.,0.220459190468382,-0.975396199161154));
#67506=DIRECTION('center_axis',(0.,-0.975396199161154,-0.220459190468382));
#67507=DIRECTION('ref_axis',(0.,0.220459190468382,-0.975396199161154));
#67508=DIRECTION('',(-1.,0.,0.));
#67509=DIRECTION('',(0.,-0.220459190468382,0.975396199161154));
#67510=DIRECTION('center_axis',(1.,0.,0.));
#67511=DIRECTION('ref_axis',(0.,0.984807753012208,-0.17364817766693));
#67512=DIRECTION('center_axis',(-1.,0.,0.));
#67513=DIRECTION('ref_axis',(0.,1.,0.));
#67514=DIRECTION('center_axis',(0.,0.734488291994154,-0.678621359023948));
#67515=DIRECTION('ref_axis',(0.,0.678621359023948,0.734488291994154));
#67516=DIRECTION('',(1.,0.,0.));
#67517=DIRECTION('',(0.,-0.678621359023948,-0.734488291994154));
#67518=DIRECTION('',(1.,0.,0.));
#67519=DIRECTION('',(0.,0.678621359023948,0.734488291994154));
#67520=DIRECTION('center_axis',(1.,0.,0.));
#67521=DIRECTION('ref_axis',(0.,0.939692620785908,-0.342020143325669));
#67522=DIRECTION('center_axis',(1.,0.,0.));
#67523=DIRECTION('ref_axis',(0.,0.,-1.));
#67524=DIRECTION('',(0.,0.0477341475084732,-0.998860075867306));
#67525=DIRECTION('center_axis',(0.,-0.998860075867306,-0.0477341475084731));
#67526=DIRECTION('ref_axis',(0.,0.0477341475084732,-0.998860075867306));
#67527=DIRECTION('',(-1.,0.,0.));
#67528=DIRECTION('',(0.,-0.0477341475084732,0.998860075867306));
#67529=DIRECTION('center_axis',(1.,0.,0.));
#67530=DIRECTION('ref_axis',(0.,0.939692620785908,-0.342020143325669));
#67531=DIRECTION('center_axis',(-1.,0.,0.));
#67532=DIRECTION('ref_axis',(0.,1.,0.));
#67533=DIRECTION('center_axis',(0.,0.605488402132173,-0.795854129148946));
#67534=DIRECTION('ref_axis',(0.,0.795854129148946,0.605488402132173));
#67535=DIRECTION('',(1.,0.,0.));
#67536=DIRECTION('',(0.,-0.795854129148946,-0.605488402132173));
#67537=DIRECTION('',(1.,0.,0.));
#67538=DIRECTION('',(0.,0.795854129148946,0.605488402132173));
#67539=DIRECTION('center_axis',(1.,0.,0.));
#67540=DIRECTION('ref_axis',(0.,0.866025403784439,-0.5));
#67541=DIRECTION('center_axis',(1.,0.,0.));
#67542=DIRECTION('ref_axis',(0.,0.,-1.));
#67543=DIRECTION('',(0.,-0.126441273368837,-0.991974094615816));
#67544=DIRECTION('center_axis',(0.,-0.991974094615816,0.126441273368837));
#67545=DIRECTION('ref_axis',(0.,-0.126441273368837,-0.991974094615816));
#67546=DIRECTION('',(-1.,0.,0.));
#67547=DIRECTION('',(0.,0.126441273368837,0.991974094615816));
#67548=DIRECTION('center_axis',(1.,0.,0.));
#67549=DIRECTION('ref_axis',(0.,0.866025403784439,-0.5));
#67550=DIRECTION('center_axis',(-1.,0.,0.));
#67551=DIRECTION('ref_axis',(0.,1.,0.));
#67552=DIRECTION('center_axis',(0.,0.458091053563321,-0.888905274281375));
#67553=DIRECTION('ref_axis',(0.,0.888905274281375,0.458091053563321));
#67554=DIRECTION('',(1.,0.,0.));
#67555=DIRECTION('',(0.,-0.888905274281375,-0.458091053563321));
#67556=DIRECTION('',(1.,0.,0.));
#67557=DIRECTION('',(0.,0.888905274281375,0.458091053563321));
#67558=DIRECTION('center_axis',(1.,0.,0.));
#67559=DIRECTION('ref_axis',(0.,0.766044443118978,-0.642787609686539));
#67560=DIRECTION('center_axis',(1.,0.,0.));
#67561=DIRECTION('ref_axis',(0.,0.,-1.));
#67562=DIRECTION('',(0.,-0.296774840137206,-0.954947482462536));
#67563=DIRECTION('center_axis',(0.,-0.954947482462536,0.296774840137206));
#67564=DIRECTION('ref_axis',(0.,-0.296774840137206,-0.954947482462536));
#67565=DIRECTION('',(-1.,0.,0.));
#67566=DIRECTION('',(0.,0.296774840137206,0.954947482462536));
#67567=DIRECTION('center_axis',(1.,0.,0.));
#67568=DIRECTION('ref_axis',(0.,0.766044443118978,-0.642787609686539));
#67569=DIRECTION('center_axis',(-1.,0.,0.));
#67570=DIRECTION('ref_axis',(0.,1.,0.));
#67571=DIRECTION('center_axis',(0.,0.296774840137206,-0.954947482462536));
#67572=DIRECTION('ref_axis',(0.,0.954947482462536,0.296774840137206));
#67573=DIRECTION('',(1.,0.,0.));
#67574=DIRECTION('',(0.,-0.954947482462536,-0.296774840137206));
#67575=DIRECTION('',(1.,0.,0.));
#67576=DIRECTION('',(0.,0.954947482462536,0.296774840137206));
#67577=DIRECTION('center_axis',(1.,0.,0.));
#67578=DIRECTION('ref_axis',(0.,0.642787609686539,-0.766044443118978));
#67579=DIRECTION('center_axis',(1.,0.,0.));
#67580=DIRECTION('ref_axis',(0.,0.,-1.));
#67581=DIRECTION('',(0.,-0.458091053563321,-0.888905274281375));
#67582=DIRECTION('center_axis',(0.,-0.888905274281375,0.458091053563321));
#67583=DIRECTION('ref_axis',(0.,-0.458091053563321,-0.888905274281375));
#67584=DIRECTION('',(-1.,0.,0.));
#67585=DIRECTION('',(0.,0.458091053563321,0.888905274281375));
#67586=DIRECTION('center_axis',(1.,0.,0.));
#67587=DIRECTION('ref_axis',(0.,0.642787609686539,-0.766044443118978));
#67588=DIRECTION('center_axis',(-1.,0.,0.));
#67589=DIRECTION('ref_axis',(0.,1.,0.));
#67590=DIRECTION('center_axis',(0.,0.126441273368836,-0.991974094615816));
#67591=DIRECTION('ref_axis',(0.,0.991974094615816,0.126441273368836));
#67592=DIRECTION('',(1.,0.,0.));
#67593=DIRECTION('',(0.,-0.991974094615816,-0.126441273368836));
#67594=DIRECTION('',(1.,0.,0.));
#67595=DIRECTION('',(0.,0.991974094615816,0.126441273368836));
#67596=DIRECTION('center_axis',(1.,0.,0.));
#67597=DIRECTION('ref_axis',(0.,0.5,-0.866025403784439));
#67598=DIRECTION('center_axis',(1.,0.,0.));
#67599=DIRECTION('ref_axis',(0.,0.,-1.));
#67600=DIRECTION('',(0.,-0.605488402132173,-0.795854129148946));
#67601=DIRECTION('center_axis',(0.,-0.795854129148946,0.605488402132173));
#67602=DIRECTION('ref_axis',(0.,-0.605488402132173,-0.795854129148946));
#67603=DIRECTION('',(-1.,0.,0.));
#67604=DIRECTION('',(0.,0.605488402132173,0.795854129148946));
#67605=DIRECTION('center_axis',(1.,0.,0.));
#67606=DIRECTION('ref_axis',(0.,0.5,-0.866025403784439));
#67607=DIRECTION('center_axis',(-1.,0.,0.));
#67608=DIRECTION('ref_axis',(0.,1.,0.));
#67609=DIRECTION('center_axis',(0.,-0.0477341475084733,-0.998860075867306));
#67610=DIRECTION('ref_axis',(0.,0.998860075867306,-0.0477341475084733));
#67611=DIRECTION('',(1.,0.,0.));
#67612=DIRECTION('',(0.,-0.998860075867306,0.0477341475084733));
#67613=DIRECTION('',(1.,0.,0.));
#67614=DIRECTION('',(0.,0.998860075867306,-0.0477341475084733));
#67615=DIRECTION('center_axis',(1.,0.,0.));
#67616=DIRECTION('ref_axis',(0.,0.342020143325669,-0.939692620785908));
#67617=DIRECTION('center_axis',(1.,0.,0.));
#67618=DIRECTION('ref_axis',(0.,0.,-1.));
#67619=DIRECTION('',(0.,-0.734488291994154,-0.678621359023948));
#67620=DIRECTION('center_axis',(0.,-0.678621359023948,0.734488291994154));
#67621=DIRECTION('ref_axis',(0.,-0.734488291994154,-0.678621359023948));
#67622=DIRECTION('',(-1.,0.,0.));
#67623=DIRECTION('',(0.,0.734488291994154,0.678621359023948));
#67624=DIRECTION('center_axis',(1.,0.,0.));
#67625=DIRECTION('ref_axis',(0.,0.342020143325669,-0.939692620785908));
#67626=DIRECTION('center_axis',(-1.,0.,0.));
#67627=DIRECTION('ref_axis',(0.,1.,0.));
#67628=DIRECTION('center_axis',(0.,-0.220459190468382,-0.975396199161154));
#67629=DIRECTION('ref_axis',(0.,0.975396199161154,-0.220459190468382));
#67630=DIRECTION('',(1.,0.,0.));
#67631=DIRECTION('',(0.,-0.975396199161154,0.220459190468382));
#67632=DIRECTION('',(1.,0.,0.));
#67633=DIRECTION('',(0.,0.975396199161154,-0.220459190468382));
#67634=DIRECTION('center_axis',(1.,0.,0.));
#67635=DIRECTION('ref_axis',(0.,0.17364817766693,-0.984807753012208));
#67636=DIRECTION('center_axis',(1.,0.,0.));
#67637=DIRECTION('ref_axis',(0.,0.,-1.));
#67638=DIRECTION('',(0.,-0.841171126772902,-0.540769022303984));
#67639=DIRECTION('center_axis',(0.,-0.540769022303984,0.841171126772902));
#67640=DIRECTION('ref_axis',(0.,-0.841171126772902,-0.540769022303984));
#67641=DIRECTION('',(-1.,0.,0.));
#67642=DIRECTION('',(0.,0.841171126772902,0.540769022303984));
#67643=DIRECTION('center_axis',(1.,0.,0.));
#67644=DIRECTION('ref_axis',(0.,0.17364817766693,-0.984807753012208));
#67645=DIRECTION('center_axis',(-1.,0.,0.));
#67646=DIRECTION('ref_axis',(0.,1.,0.));
#67647=DIRECTION('center_axis',(1.,0.,0.));
#67648=DIRECTION('ref_axis',(0.,0.,-1.));
#67649=DIRECTION('center_axis',(1.,0.,0.));
#67650=DIRECTION('ref_axis',(0.,0.,-1.));
#67651=DIRECTION('',(0.,0.922295402517783,-0.386485692483643));
#67652=DIRECTION('',(0.,-0.922295402517783,-0.386485692483643));
#67653=DIRECTION('center_axis',(0.,-0.386485692483643,-0.922295402517783));
#67654=DIRECTION('ref_axis',(0.,0.922295402517783,-0.386485692483643));
#67655=DIRECTION('',(1.,0.,0.));
#67656=DIRECTION('',(0.,-0.922295402517783,0.386485692483643));
#67657=DIRECTION('',(1.,0.,0.));
#67658=DIRECTION('center_axis',(0.,-0.386485692483643,0.922295402517783));
#67659=DIRECTION('ref_axis',(0.,-0.922295402517783,-0.386485692483643));
#67660=DIRECTION('',(-1.,0.,0.));
#67661=DIRECTION('',(0.,0.922295402517783,0.386485692483643));
#67662=DIRECTION('center_axis',(1.,0.,0.));
#67663=DIRECTION('ref_axis',(0.,0.,-1.));
#67664=DIRECTION('center_axis',(-1.,0.,0.));
#67665=DIRECTION('ref_axis',(0.,1.,0.));
#67666=DIRECTION('center_axis',(1.,0.,0.));
#67667=DIRECTION('ref_axis',(0.,1.,0.));
#67668=DIRECTION('',(0.517550572850554,-0.855652619082103,-1.04787224114095E-16));
#67669=DIRECTION('center_axis',(-1.,0.,0.));
#67670=DIRECTION('ref_axis',(0.,1.,0.));
#67671=DIRECTION('center_axis',(0.,-0.5,0.866025403784439));
#67672=DIRECTION('ref_axis',(0.,-0.866025403784439,-0.5));
#67673=DIRECTION('',(0.,0.866025403784439,0.5));
#67674=DIRECTION('',(1.,0.,0.));
#67675=DIRECTION('',(0.,-0.866025403784439,-0.5));
#67676=DIRECTION('',(1.,0.,0.));
#67677=DIRECTION('center_axis',(0.,0.5,0.866025403784439));
#67678=DIRECTION('ref_axis',(0.,-0.866025403784439,0.5));
#67679=DIRECTION('',(0.,0.866025403784439,-0.5));
#67680=DIRECTION('',(0.,-0.866025403784439,0.5));
#67681=DIRECTION('',(1.,0.,0.));
#67682=DIRECTION('center_axis',(0.,1.,-3.84592537276713E-16));
#67683=DIRECTION('ref_axis',(0.,3.84592537276713E-16,1.));
#67684=DIRECTION('',(0.,-3.84592537276713E-16,-1.));
#67685=DIRECTION('',(0.,3.84592537276713E-16,1.));
#67686=DIRECTION('',(1.,0.,0.));
#67687=DIRECTION('center_axis',(0.,0.5,-0.866025403784439));
#67688=DIRECTION('ref_axis',(0.,0.866025403784439,0.5));
#67689=DIRECTION('',(0.,-0.866025403784439,-0.5));
#67690=DIRECTION('',(0.,0.866025403784439,0.5));
#67691=DIRECTION('',(1.,0.,0.));
#67692=DIRECTION('center_axis',(0.,-0.5,-0.866025403784439));
#67693=DIRECTION('ref_axis',(0.,0.866025403784439,-0.5));
#67694=DIRECTION('',(0.,-0.866025403784439,0.5));
#67695=DIRECTION('',(0.,0.866025403784439,-0.5));
#67696=DIRECTION('',(1.,0.,0.));
#67697=DIRECTION('center_axis',(0.,-1.,-1.92296268638356E-16));
#67698=DIRECTION('ref_axis',(0.,1.92296268638356E-16,-1.));
#67699=DIRECTION('',(0.,-1.92296268638356E-16,1.));
#67700=DIRECTION('',(0.,1.92296268638356E-16,-1.));
#67701=DIRECTION('center_axis',(1.,0.,0.));
#67702=DIRECTION('ref_axis',(0.,0.,-1.));
#67703=DIRECTION('center_axis',(-1.,0.,0.));
#67704=DIRECTION('ref_axis',(0.,0.,1.));
#67705=DIRECTION('center_axis',(1.,0.,0.));
#67706=DIRECTION('ref_axis',(0.,0.,-1.));
#67707=DIRECTION('center_axis',(1.,0.,0.));
#67708=DIRECTION('ref_axis',(0.,1.,0.));
#67709=DIRECTION('',(-0.707106781186548,0.707106781186547,8.65956056235493E-17));
#67710=DIRECTION('center_axis',(1.,0.,0.));
#67711=DIRECTION('ref_axis',(0.,1.,0.));
#67712=DIRECTION('center_axis',(1.,0.,0.));
#67713=DIRECTION('ref_axis',(0.,0.,-1.));
#67714=DIRECTION('center_axis',(1.,0.,0.));
#67715=DIRECTION('ref_axis',(0.,0.,-1.));
#67716=DIRECTION('center_axis',(1.,0.,0.));
#67717=DIRECTION('ref_axis',(0.,0.,-1.));
#67718=DIRECTION('center_axis',(1.,0.,0.));
#67719=DIRECTION('ref_axis',(0.,0.,-1.));
#67720=DIRECTION('center_axis',(1.,0.,0.));
#67721=DIRECTION('ref_axis',(0.,0.,-1.));
#67722=DIRECTION('center_axis',(1.,0.,0.));
#67723=DIRECTION('ref_axis',(0.,0.,-1.));
#67724=DIRECTION('center_axis',(1.,0.,0.));
#67725=DIRECTION('ref_axis',(0.,0.,-1.));
#67726=DIRECTION('center_axis',(1.,0.,0.));
#67727=DIRECTION('ref_axis',(0.,0.,-1.));
#67728=DIRECTION('center_axis',(1.,0.,0.));
#67729=DIRECTION('ref_axis',(0.,0.,-1.));
#67730=DIRECTION('center_axis',(1.,0.,0.));
#67731=DIRECTION('ref_axis',(0.,0.,-1.));
#67732=DIRECTION('center_axis',(1.,0.,0.));
#67733=DIRECTION('ref_axis',(0.,0.,-1.));
#67734=DIRECTION('center_axis',(1.,0.,0.));
#67735=DIRECTION('ref_axis',(0.,0.,-1.));
#67736=DIRECTION('center_axis',(1.,0.,0.));
#67737=DIRECTION('ref_axis',(0.,0.,-1.));
#67738=DIRECTION('center_axis',(1.,0.,0.));
#67739=DIRECTION('ref_axis',(0.,0.,-1.));
#67740=DIRECTION('center_axis',(1.,0.,0.));
#67741=DIRECTION('ref_axis',(0.,0.,-1.));
#67742=DIRECTION('center_axis',(1.,0.,0.));
#67743=DIRECTION('ref_axis',(0.,0.,-1.));
#67744=DIRECTION('center_axis',(1.,0.,0.));
#67745=DIRECTION('ref_axis',(0.,0.,-1.));
#67746=DIRECTION('',(-1.,0.,0.));
#67747=DIRECTION('center_axis',(1.,0.,0.));
#67748=DIRECTION('ref_axis',(0.,0.,-1.));
#67749=DIRECTION('center_axis',(1.,0.,0.));
#67750=DIRECTION('ref_axis',(0.,0.,-1.));
#67751=DIRECTION('center_axis',(1.,0.,0.));
#67752=DIRECTION('ref_axis',(0.,0.,-1.));
#67753=DIRECTION('center_axis',(1.,0.,0.));
#67754=DIRECTION('ref_axis',(0.,0.,-1.));
#67755=DIRECTION('center_axis',(1.,0.,0.));
#67756=DIRECTION('ref_axis',(0.,0.,-1.));
#67757=DIRECTION('center_axis',(1.,0.,0.));
#67758=DIRECTION('ref_axis',(0.,0.,-1.));
#67759=DIRECTION('center_axis',(1.,0.,0.));
#67760=DIRECTION('ref_axis',(0.,0.,-1.));
#67761=DIRECTION('center_axis',(1.,0.,0.));
#67762=DIRECTION('ref_axis',(0.,0.,-1.));
#67763=DIRECTION('center_axis',(1.,0.,0.));
#67764=DIRECTION('ref_axis',(0.,0.,-1.));
#67765=DIRECTION('center_axis',(1.,0.,0.));
#67766=DIRECTION('ref_axis',(0.,0.,-1.));
#67767=DIRECTION('center_axis',(1.,0.,0.));
#67768=DIRECTION('ref_axis',(0.,0.,-1.));
#67769=DIRECTION('center_axis',(1.,0.,0.));
#67770=DIRECTION('ref_axis',(0.,0.,-1.));
#67771=DIRECTION('center_axis',(1.,0.,0.));
#67772=DIRECTION('ref_axis',(0.,0.,-1.));
#67773=DIRECTION('center_axis',(1.,0.,0.));
#67774=DIRECTION('ref_axis',(0.,0.,-1.));
#67775=DIRECTION('center_axis',(1.,0.,0.));
#67776=DIRECTION('ref_axis',(0.,0.,-1.));
#67777=DIRECTION('center_axis',(1.,0.,0.));
#67778=DIRECTION('ref_axis',(0.,0.,-1.));
#67779=DIRECTION('center_axis',(1.,0.,0.));
#67780=DIRECTION('ref_axis',(0.,0.,-1.));
#67781=DIRECTION('center_axis',(1.,0.,0.));
#67782=DIRECTION('ref_axis',(0.,0.,-1.));
#67783=DIRECTION('center_axis',(1.,0.,0.));
#67784=DIRECTION('ref_axis',(0.,0.,-1.));
#67785=DIRECTION('center_axis',(-1.,0.,0.));
#67786=DIRECTION('ref_axis',(0.,1.,0.));
#67787=DIRECTION('center_axis',(1.,0.,0.));
#67788=DIRECTION('ref_axis',(0.,0.,-1.));
#67789=DIRECTION('',(-0.707106781186547,-0.707106781186548,-8.65956056235493E-17));
#67790=DIRECTION('center_axis',(1.,0.,0.));
#67791=DIRECTION('ref_axis',(0.,0.,-1.));
#67792=DIRECTION('axis',(0.,0.,1.));
#67793=DIRECTION('refdir',(1.,0.,0.));
#67794=DIRECTION('center_axis',(1.,0.,0.));
#67795=DIRECTION('ref_axis',(0.,0.,-1.));
#67796=DIRECTION('center_axis',(-1.,0.,0.));
#67797=DIRECTION('ref_axis',(0.,-1.,1.83697019872103E-16));
#67798=DIRECTION('center_axis',(0.,-1.,-1.22464679914735E-16));
#67799=DIRECTION('ref_axis',(0.,-1.22464679914735E-16,1.));
#67800=DIRECTION('center_axis',(1.,0.,0.));
#67801=DIRECTION('ref_axis',(0.,-1.,3.06161699786838E-17));
#67802=DIRECTION('center_axis',(1.,0.,0.));
#67803=DIRECTION('ref_axis',(0.,-1.,3.06161699786838E-17));
#67804=DIRECTION('center_axis',(-1.,0.,0.));
#67805=DIRECTION('ref_axis',(0.,1.,0.));
#67806=DIRECTION('',(-0.707106781186548,-0.707106781186547,-8.65956056235493E-17));
#67807=DIRECTION('center_axis',(1.,0.,0.));
#67808=DIRECTION('ref_axis',(0.,0.,-1.));
#67809=DIRECTION('center_axis',(1.,0.,0.));
#67810=DIRECTION('ref_axis',(0.,0.,-1.));
#67811=DIRECTION('center_axis',(-1.,0.,0.));
#67812=DIRECTION('ref_axis',(0.,0.,1.));
#67813=DIRECTION('center_axis',(1.,0.,0.));
#67814=DIRECTION('ref_axis',(0.,0.,-1.));
#67815=DIRECTION('center_axis',(1.,0.,0.));
#67816=DIRECTION('ref_axis',(0.,1.,0.));
#67817=DIRECTION('center_axis',(1.,0.,0.));
#67818=DIRECTION('ref_axis',(0.,0.,-1.));
#67819=DIRECTION('',(-0.707106781186547,0.707106781186548,8.65956056235493E-17));
#67820=DIRECTION('center_axis',(1.,0.,0.));
#67821=DIRECTION('ref_axis',(0.,1.,0.));
#67822=DIRECTION('',(-1.,0.,0.));
#67823=DIRECTION('axis',(0.,0.,1.));
#67824=DIRECTION('refdir',(1.,0.,0.));
#67825=DIRECTION('center_axis',(1.,0.,0.));
#67826=DIRECTION('ref_axis',(0.,1.,0.));
#67827=DIRECTION('',(-1.,0.,0.));
#67828=DIRECTION('center_axis',(1.,0.,0.));
#67829=DIRECTION('ref_axis',(0.,1.,0.));
#67830=DIRECTION('center_axis',(1.,0.,0.));
#67831=DIRECTION('ref_axis',(0.,1.,0.));
#67832=DIRECTION('',(-1.,0.,0.));
#67833=DIRECTION('center_axis',(1.,0.,0.));
#67834=DIRECTION('ref_axis',(0.,1.,0.));
#67835=DIRECTION('',(-1.,0.,0.));
#67836=DIRECTION('center_axis',(1.,0.,0.));
#67837=DIRECTION('ref_axis',(0.,1.,0.));
#67838=DIRECTION('',(-1.,0.,0.));
#67839=DIRECTION('center_axis',(1.,0.,0.));
#67840=DIRECTION('ref_axis',(0.,1.,0.));
#67841=DIRECTION('',(-1.,0.,0.));
#67842=DIRECTION('center_axis',(1.,0.,0.));
#67843=DIRECTION('ref_axis',(0.,1.,0.));
#67844=DIRECTION('',(-1.,0.,0.));
#67845=DIRECTION('center_axis',(1.,0.,0.));
#67846=DIRECTION('ref_axis',(0.,1.,0.));
#67847=DIRECTION('',(-1.,0.,0.));
#67848=DIRECTION('center_axis',(1.,0.,0.));
#67849=DIRECTION('ref_axis',(0.,1.,0.));
#67850=DIRECTION('',(-1.,0.,0.));
#67851=DIRECTION('center_axis',(1.,0.,0.));
#67852=DIRECTION('ref_axis',(0.,1.,0.));
#67853=DIRECTION('',(-1.,0.,0.));
#67854=DIRECTION('center_axis',(1.,0.,0.));
#67855=DIRECTION('ref_axis',(0.,1.,0.));
#67856=DIRECTION('',(-1.,0.,0.));
#67857=DIRECTION('center_axis',(1.,0.,0.));
#67858=DIRECTION('ref_axis',(0.,1.,0.));
#67859=DIRECTION('',(-1.,0.,0.));
#67860=DIRECTION('center_axis',(1.,0.,0.));
#67861=DIRECTION('ref_axis',(0.,1.,0.));
#67862=DIRECTION('',(-1.,0.,0.));
#67863=DIRECTION('center_axis',(1.,0.,0.));
#67864=DIRECTION('ref_axis',(0.,1.,0.));
#67865=DIRECTION('',(-1.,0.,0.));
#67866=DIRECTION('center_axis',(1.,0.,0.));
#67867=DIRECTION('ref_axis',(0.,1.,0.));
#67868=DIRECTION('',(-1.,0.,0.));
#67869=DIRECTION('center_axis',(1.,0.,0.));
#67870=DIRECTION('ref_axis',(0.,1.,0.));
#67871=DIRECTION('',(-1.,0.,0.));
#67872=DIRECTION('center_axis',(1.,0.,0.));
#67873=DIRECTION('ref_axis',(0.,1.,0.));
#67874=DIRECTION('',(-1.,0.,0.));
#67875=DIRECTION('center_axis',(1.,0.,0.));
#67876=DIRECTION('ref_axis',(0.,1.,0.));
#67877=DIRECTION('',(-1.,0.,0.));
#67878=DIRECTION('center_axis',(1.,0.,0.));
#67879=DIRECTION('ref_axis',(0.,1.,0.));
#67880=DIRECTION('',(-1.,0.,0.));
#67881=DIRECTION('center_axis',(1.,0.,0.));
#67882=DIRECTION('ref_axis',(0.,1.,0.));
#67883=DIRECTION('',(-1.,0.,0.));
#67884=DIRECTION('center_axis',(1.,0.,0.));
#67885=DIRECTION('ref_axis',(0.,1.,0.));
#67886=DIRECTION('',(-1.,0.,0.));
#67887=DIRECTION('center_axis',(1.,0.,0.));
#67888=DIRECTION('ref_axis',(0.,1.,0.));
#67889=DIRECTION('',(-1.,0.,0.));
#67890=DIRECTION('center_axis',(1.,0.,0.));
#67891=DIRECTION('ref_axis',(0.,1.,0.));
#67892=DIRECTION('',(-1.,0.,0.));
#67893=DIRECTION('center_axis',(1.,0.,0.));
#67894=DIRECTION('ref_axis',(0.,1.,0.));
#67895=DIRECTION('',(-1.,0.,0.));
#67896=DIRECTION('center_axis',(1.,0.,0.));
#67897=DIRECTION('ref_axis',(0.,-0.18069699119509,-0.983538813353617));
#67898=DIRECTION('',(1.,0.,0.));
#67899=DIRECTION('center_axis',(1.,0.,0.));
#67900=DIRECTION('ref_axis',(0.,1.,4.63459159752748E-15));
#67901=DIRECTION('center_axis',(1.,0.,0.));
#67902=DIRECTION('ref_axis',(0.,1.,4.63459159752748E-15));
#67903=DIRECTION('',(1.,0.,0.));
#67904=DIRECTION('center_axis',(1.,0.,0.));
#67905=DIRECTION('ref_axis',(0.,1.,4.63459159752748E-15));
#67906=DIRECTION('',(1.,0.,0.));
#67907=DIRECTION('center_axis',(1.,0.,0.));
#67908=DIRECTION('ref_axis',(0.,1.,4.63459159752748E-15));
#67909=DIRECTION('',(1.,0.,0.));
#67910=DIRECTION('center_axis',(1.,0.,0.));
#67911=DIRECTION('ref_axis',(0.,1.,4.63459159752748E-15));
#67912=DIRECTION('',(1.,0.,0.));
#67913=DIRECTION('center_axis',(1.,0.,0.));
#67914=DIRECTION('ref_axis',(0.,1.,4.63459159752748E-15));
#67915=DIRECTION('',(1.,0.,0.));
#67916=DIRECTION('center_axis',(1.,0.,0.));
#67917=DIRECTION('ref_axis',(0.,1.,4.63459159752748E-15));
#67918=DIRECTION('',(1.,0.,0.));
#67919=DIRECTION('center_axis',(1.,0.,0.));
#67920=DIRECTION('ref_axis',(0.,1.,4.63459159752748E-15));
#67921=DIRECTION('',(1.,0.,0.));
#67922=DIRECTION('center_axis',(1.,0.,0.));
#67923=DIRECTION('ref_axis',(0.,1.,4.63459159752748E-15));
#67924=DIRECTION('',(1.,0.,0.));
#67925=DIRECTION('center_axis',(1.,0.,0.));
#67926=DIRECTION('ref_axis',(0.,1.,4.63459159752748E-15));
#67927=DIRECTION('',(1.,0.,0.));
#67928=DIRECTION('center_axis',(1.,0.,0.));
#67929=DIRECTION('ref_axis',(0.,1.,4.63459159752748E-15));
#67930=DIRECTION('',(1.,0.,0.));
#67931=DIRECTION('center_axis',(1.,0.,0.));
#67932=DIRECTION('ref_axis',(0.,1.,4.63459159752748E-15));
#67933=DIRECTION('',(1.,0.,0.));
#67934=DIRECTION('center_axis',(1.,0.,0.));
#67935=DIRECTION('ref_axis',(0.,1.,4.63459159752748E-15));
#67936=DIRECTION('',(1.,0.,0.));
#67937=DIRECTION('center_axis',(1.,0.,0.));
#67938=DIRECTION('ref_axis',(0.,1.,4.63459159752748E-15));
#67939=DIRECTION('',(1.,0.,0.));
#67940=DIRECTION('center_axis',(1.,0.,0.));
#67941=DIRECTION('ref_axis',(0.,1.,4.63459159752748E-15));
#67942=DIRECTION('',(1.,0.,0.));
#67943=DIRECTION('center_axis',(1.,0.,0.));
#67944=DIRECTION('ref_axis',(0.,1.,4.63459159752748E-15));
#67945=DIRECTION('',(1.,0.,0.));
#67946=DIRECTION('center_axis',(1.,0.,0.));
#67947=DIRECTION('ref_axis',(0.,1.,4.63459159752748E-15));
#67948=DIRECTION('',(1.,0.,0.));
#67949=DIRECTION('center_axis',(1.,0.,0.));
#67950=DIRECTION('ref_axis',(0.,1.,4.63459159752748E-15));
#67951=DIRECTION('',(1.,0.,0.));
#67952=DIRECTION('center_axis',(1.,0.,0.));
#67953=DIRECTION('ref_axis',(0.,1.,4.63459159752748E-15));
#67954=DIRECTION('',(1.,0.,0.));
#67955=DIRECTION('center_axis',(1.,0.,0.));
#67956=DIRECTION('ref_axis',(0.,1.,4.63459159752748E-15));
#67957=DIRECTION('',(1.,0.,0.));
#67958=DIRECTION('center_axis',(1.,0.,0.));
#67959=DIRECTION('ref_axis',(0.,1.,4.63459159752748E-15));
#67960=DIRECTION('',(1.,0.,0.));
#67961=DIRECTION('center_axis',(1.,0.,0.));
#67962=DIRECTION('ref_axis',(0.,1.,4.63459159752748E-15));
#67963=DIRECTION('',(1.,0.,0.));
#67964=DIRECTION('center_axis',(1.,0.,0.));
#67965=DIRECTION('ref_axis',(0.,1.,4.63459159752748E-15));
#67966=DIRECTION('',(1.,0.,0.));
#67967=DIRECTION('center_axis',(1.,0.,0.));
#67968=DIRECTION('ref_axis',(0.,0.,-1.));
#67969=DIRECTION('center_axis',(1.,0.,0.));
#67970=DIRECTION('ref_axis',(0.,1.,0.));
#67971=DIRECTION('center_axis',(1.,0.,0.));
#67972=DIRECTION('ref_axis',(0.,1.,0.));
#67973=DIRECTION('center_axis',(1.,0.,0.));
#67974=DIRECTION('ref_axis',(0.,0.,-1.));
#67975=DIRECTION('center_axis',(1.,0.,0.));
#67976=DIRECTION('ref_axis',(0.,1.,0.));
#67977=DIRECTION('center_axis',(1.,0.,0.));
#67978=DIRECTION('ref_axis',(0.,1.,0.));
#67979=DIRECTION('center_axis',(-1.,0.,0.));
#67980=DIRECTION('ref_axis',(0.,1.,4.63459159752748E-15));
#67981=DIRECTION('center_axis',(1.,0.,0.));
#67982=DIRECTION('ref_axis',(0.,1.,4.63459159752748E-15));
#67983=DIRECTION('center_axis',(1.,0.,0.));
#67984=DIRECTION('ref_axis',(0.,0.,-1.));
#67985=DIRECTION('center_axis',(0.,-1.,-1.22464679914735E-16));
#67986=DIRECTION('ref_axis',(0.,-1.22464679914735E-16,1.));
#67987=DIRECTION('center_axis',(-1.,0.,0.));
#67988=DIRECTION('ref_axis',(0.,1.,0.));
#67989=DIRECTION('center_axis',(1.,0.,0.));
#67990=DIRECTION('ref_axis',(0.,1.,0.));
#67991=DIRECTION('center_axis',(1.,0.,0.));
#67992=DIRECTION('ref_axis',(0.,0.966096391796101,-0.258181644890869));
#67993=DIRECTION('center_axis',(-1.,0.,0.));
#67994=DIRECTION('ref_axis',(0.,0.,1.));
#67995=DIRECTION('center_axis',(1.,0.,0.));
#67996=DIRECTION('ref_axis',(0.,0.,-1.));
#67997=DIRECTION('center_axis',(-1.,0.,0.));
#67998=DIRECTION('ref_axis',(0.,1.,0.));
#67999=DIRECTION('',(0.534234448563085,0.845336355522757,1.03523846199383E-16));
#68000=DIRECTION('center_axis',(1.,0.,0.));
#68001=DIRECTION('ref_axis',(0.,1.,0.));
#68002=DIRECTION('center_axis',(0.,1.4792020664489E-16,1.));
#68003=DIRECTION('ref_axis',(0.,-1.,1.4792020664489E-16));
#68004=DIRECTION('',(1.,0.,0.));
#68005=DIRECTION('',(0.,-1.,1.4792020664489E-16));
#68006=DIRECTION('',(1.,0.,0.));
#68007=DIRECTION('center_axis',(0.,0.866025403784439,0.5));
#68008=DIRECTION('ref_axis',(0.,-0.5,0.866025403784439));
#68009=DIRECTION('',(1.,0.,0.));
#68010=DIRECTION('',(0.,-0.5,0.866025403784439));
#68011=DIRECTION('center_axis',(0.,0.866025403784439,-0.5));
#68012=DIRECTION('ref_axis',(0.,0.5,0.866025403784439));
#68013=DIRECTION('',(1.,0.,0.));
#68014=DIRECTION('',(0.,0.5,0.866025403784439));
#68015=DIRECTION('center_axis',(1.,0.,0.));
#68016=DIRECTION('ref_axis',(0.,1.,0.));
#68017=DIRECTION('center_axis',(1.,0.,0.));
#68018=DIRECTION('ref_axis',(0.,1.,0.));
#68019=DIRECTION('',(-1.,0.,0.));
#68020=DIRECTION('center_axis',(-1.,0.,0.));
#68021=DIRECTION('ref_axis',(0.,0.,1.));
#68022=DIRECTION('center_axis',(1.,0.,0.));
#68023=DIRECTION('ref_axis',(0.,0.,-1.));
#68024=DIRECTION('center_axis',(1.,0.,0.));
#68025=DIRECTION('ref_axis',(0.,1.,0.));
#68026=DIRECTION('',(-0.707106781186548,0.707106781186547,8.65956056235493E-17));
#68027=DIRECTION('center_axis',(0.,-2.95840413289779E-16,-1.));
#68028=DIRECTION('ref_axis',(0.,1.,-2.95840413289779E-16));
#68029=DIRECTION('',(1.,0.,0.));
#68030=DIRECTION('',(0.,1.,-2.95840413289779E-16));
#68031=DIRECTION('center_axis',(0.,-0.866025403784439,-0.5));
#68032=DIRECTION('ref_axis',(0.,0.5,-0.866025403784439));
#68033=DIRECTION('',(1.,0.,0.));
#68034=DIRECTION('',(0.,0.5,-0.866025403784439));
#68035=DIRECTION('center_axis',(0.,-0.866025403784439,0.5));
#68036=DIRECTION('ref_axis',(0.,-0.5,-0.866025403784439));
#68037=DIRECTION('',(0.,-0.5,-0.866025403784439));
#68038=DIRECTION('center_axis',(1.,0.,0.));
#68039=DIRECTION('ref_axis',(0.,0.,-1.));
#68040=DIRECTION('center_axis',(1.,0.,0.));
#68041=DIRECTION('ref_axis',(0.,0.,-1.));
#68042=DIRECTION('axis',(0.,0.,1.));
#68043=DIRECTION('refdir',(1.,0.,0.));
#68044=DIRECTION('center_axis',(1.,0.,0.));
#68045=DIRECTION('ref_axis',(0.,1.,0.));
#68046=DIRECTION('center_axis',(1.,0.,0.));
#68047=DIRECTION('ref_axis',(0.,0.,-1.));
#68048=DIRECTION('',(-0.707106781186547,0.707106781186548,8.65956056235494E-17));
#68049=DIRECTION('center_axis',(1.,0.,0.));
#68050=DIRECTION('ref_axis',(0.,0.,-1.));
#68051=DIRECTION('center_axis',(1.,0.,0.));
#68052=DIRECTION('ref_axis',(0.,1.,0.));
#68053=DIRECTION('center_axis',(1.,0.,0.));
#68054=DIRECTION('ref_axis',(0.,0.,-1.));
#68055=DIRECTION('',(-1.,0.,0.));
#68056=DIRECTION('center_axis',(-1.,0.,0.));
#68057=DIRECTION('ref_axis',(0.,1.,0.));
#68058=DIRECTION('center_axis',(1.,0.,0.));
#68059=DIRECTION('ref_axis',(0.,0.,-1.));
#68060=DIRECTION('',(-0.707106781186547,-0.707106781186548,-8.65956056235494E-17));
#68061=DIRECTION('center_axis',(1.,0.,0.));
#68062=DIRECTION('ref_axis',(0.,0.,-1.));
#68063=DIRECTION('center_axis',(1.,0.,0.));
#68064=DIRECTION('ref_axis',(0.,0.,-1.));
#68065=DIRECTION('center_axis',(1.,0.,0.));
#68066=DIRECTION('ref_axis',(0.,1.,0.));
#68067=DIRECTION('',(-0.707106781186547,0.707106781186548,8.65956056235494E-17));
#68068=DIRECTION('center_axis',(1.,0.,0.));
#68069=DIRECTION('ref_axis',(0.,0.,-1.));
#68070=DIRECTION('center_axis',(1.,0.,0.));
#68071=DIRECTION('ref_axis',(0.,1.,0.));
#68072=DIRECTION('',(-1.,0.,0.));
#68073=DIRECTION('center_axis',(1.,0.,0.));
#68074=DIRECTION('ref_axis',(0.,0.,-1.));
#68075=DIRECTION('center_axis',(-1.,0.,0.));
#68076=DIRECTION('ref_axis',(0.,1.,0.));
#68077=DIRECTION('',(-0.707106781186547,-0.707106781186548,-8.65956056235494E-17));
#68078=DIRECTION('center_axis',(1.,0.,0.));
#68079=DIRECTION('ref_axis',(0.,0.,-1.));
#68080=DIRECTION('center_axis',(-1.,0.,0.));
#68081=DIRECTION('ref_axis',(0.,0.,1.));
#68082=DIRECTION('axis',(0.,0.,1.));
#68083=DIRECTION('refdir',(1.,0.,0.));
#68084=DIRECTION('center_axis',(1.,0.,0.));
#68085=DIRECTION('ref_axis',(0.,1.,0.));
#68086=DIRECTION('',(-1.,0.,0.));
#68087=DIRECTION('center_axis',(1.,0.,0.));
#68088=DIRECTION('ref_axis',(0.,-1.,0.));
#68089=DIRECTION('center_axis',(0.5,-0.866025403784439,0.));
#68090=DIRECTION('ref_axis',(0.866025403784439,0.5,0.));
#68091=DIRECTION('center_axis',(-1.,0.,0.));
#68092=DIRECTION('ref_axis',(0.,-1.,0.));
#68093=DIRECTION('center_axis',(-0.5,0.866025403784439,0.));
#68094=DIRECTION('ref_axis',(-0.866025403784439,-0.5,0.));
#68095=DIRECTION('',(0.,0.,-1.));
#68096=DIRECTION('center_axis',(-0.5,0.866025403784439,0.));
#68097=DIRECTION('ref_axis',(0.866025403784439,0.5,0.));
#68098=DIRECTION('',(0.,0.,1.));
#68099=DIRECTION('center_axis',(0.5,-0.866025403784439,0.));
#68100=DIRECTION('ref_axis',(0.866025403784439,0.5,0.));
#68101=DIRECTION('center_axis',(0.5,-0.866025403784439,0.));
#68102=DIRECTION('ref_axis',(0.866025403784439,0.5,0.));
#68103=DIRECTION('center_axis',(-0.5,0.866025403784439,0.));
#68104=DIRECTION('ref_axis',(0.866025403784439,0.5,0.));
#68105=DIRECTION('',(0.,0.,-1.));
#68106=DIRECTION('',(0.,0.,1.));
#68107=DIRECTION('center_axis',(1.,0.,0.));
#68108=DIRECTION('ref_axis',(0.,-0.00627477638988747,-0.999980313396847));
#68109=DIRECTION('center_axis',(-1.,0.,0.));
#68110=DIRECTION('ref_axis',(0.,-1.,0.));
#68111=DIRECTION('center_axis',(1.,0.,0.));
#68112=DIRECTION('ref_axis',(0.,-1.,0.));
#68113=DIRECTION('center_axis',(1.,0.,0.));
#68114=DIRECTION('ref_axis',(0.,1.,0.));
#68115=DIRECTION('center_axis',(1.,0.,0.));
#68116=DIRECTION('ref_axis',(0.,-1.,0.));
#68117=DIRECTION('center_axis',(-1.,0.,0.));
#68118=DIRECTION('ref_axis',(0.,-0.151470903394779,-0.988461716721882));
#68119=DIRECTION('center_axis',(-1.,0.,0.));
#68120=DIRECTION('ref_axis',(0.,-1.,0.));
#68121=DIRECTION('center_axis',(1.,0.,0.));
#68122=DIRECTION('ref_axis',(0.,0.,-1.));
#68123=DIRECTION('center_axis',(1.,0.,0.));
#68124=DIRECTION('ref_axis',(0.,-1.,0.));
#68125=DIRECTION('center_axis',(1.,0.,0.));
#68126=DIRECTION('ref_axis',(0.,-0.238193136410173,-0.971217807583389));
#68127=DIRECTION('center_axis',(-1.,0.,0.));
#68128=DIRECTION('ref_axis',(0.,-1.,0.));
#68129=DIRECTION('center_axis',(1.,0.,0.));
#68130=DIRECTION('ref_axis',(0.,-0.142556190914054,-0.989786710575605));
#68131=DIRECTION('center_axis',(1.,0.,0.));
#68132=DIRECTION('ref_axis',(0.,-1.,0.));
#68133=DIRECTION('center_axis',(-1.,0.,0.));
#68134=DIRECTION('ref_axis',(0.,-0.0315875774899171,-0.999500987967655));
#68135=DIRECTION('center_axis',(-1.,0.,0.));
#68136=DIRECTION('ref_axis',(0.,-1.,0.));
#68137=DIRECTION('center_axis',(-1.,0.,0.));
#68138=DIRECTION('ref_axis',(0.,0.,1.));
#68139=DIRECTION('axis',(0.,0.,1.));
#68140=DIRECTION('refdir',(1.,0.,0.));
#68141=DIRECTION('center_axis',(-1.,0.,0.));
#68142=DIRECTION('ref_axis',(0.,1.,0.));
#68143=DIRECTION('center_axis',(1.,0.,0.));
#68144=DIRECTION('ref_axis',(0.,1.,0.));
#68145=DIRECTION('',(0.682318250360011,0.731055268242869,8.95284494253439E-17));
#68146=DIRECTION('center_axis',(1.,0.,0.));
#68147=DIRECTION('ref_axis',(0.,0.,-1.));
#68148=DIRECTION('center_axis',(1.,0.,0.));
#68149=DIRECTION('ref_axis',(0.,1.,0.));
#68150=DIRECTION('',(1.,0.,0.));
#68151=DIRECTION('center_axis',(1.,0.,0.));
#68152=DIRECTION('ref_axis',(0.,0.,-1.));
#68153=DIRECTION('center_axis',(1.,0.,0.));
#68154=DIRECTION('ref_axis',(0.,1.,0.));
#68155=DIRECTION('',(0.682318250360011,-0.731055268242869,-8.9528449425344E-17));
#68156=DIRECTION('center_axis',(-1.,0.,0.));
#68157=DIRECTION('ref_axis',(0.,1.,0.));
#68158=DIRECTION('center_axis',(1.,0.,0.));
#68159=DIRECTION('ref_axis',(0.,1.,0.));
#68160=DIRECTION('center_axis',(-1.,0.,0.));
#68161=DIRECTION('ref_axis',(0.,1.,0.));
#68162=DIRECTION('',(0.534234448563085,-0.845336355522756,-1.03523846199383E-16));
#68163=DIRECTION('center_axis',(0.,-2.95840413289779E-16,-1.));
#68164=DIRECTION('ref_axis',(0.,1.,-2.95840413289779E-16));
#68165=DIRECTION('',(1.,0.,0.));
#68166=DIRECTION('',(1.,0.,0.));
#68167=DIRECTION('center_axis',(0.,0.866025403784439,-0.5));
#68168=DIRECTION('ref_axis',(0.,0.5,0.866025403784439));
#68169=DIRECTION('',(1.,0.,0.));
#68170=DIRECTION('center_axis',(0.,0.866025403784439,0.5));
#68171=DIRECTION('ref_axis',(0.,-0.5,0.866025403784439));
#68172=DIRECTION('',(1.,0.,0.));
#68173=DIRECTION('center_axis',(-1.,0.,0.));
#68174=DIRECTION('ref_axis',(0.,1.,0.));
#68175=DIRECTION('',(0.534234448563085,0.845336355522756,1.03523846199383E-16));
#68176=DIRECTION('center_axis',(1.,0.,0.));
#68177=DIRECTION('ref_axis',(0.,1.,0.));
#68178=DIRECTION('center_axis',(0.,1.4792020664489E-16,1.));
#68179=DIRECTION('ref_axis',(0.,-1.,1.4792020664489E-16));
#68180=DIRECTION('',(1.,0.,0.));
#68181=DIRECTION('center_axis',(0.,-0.866025403784439,-0.5));
#68182=DIRECTION('ref_axis',(0.,0.5,-0.866025403784439));
#68183=DIRECTION('',(1.,0.,0.));
#68184=DIRECTION('center_axis',(0.,-0.866025403784439,0.5));
#68185=DIRECTION('ref_axis',(0.,-0.5,-0.866025403784439));
#68186=DIRECTION('center_axis',(1.,0.,0.));
#68187=DIRECTION('ref_axis',(0.,0.,-1.));
#68188=DIRECTION('center_axis',(1.,0.,0.));
#68189=DIRECTION('ref_axis',(0.,0.,-1.));
#68190=DIRECTION('',(0.,1.,0.));
#68191=DIRECTION('',(0.,0.,1.));
#68192=DIRECTION('',(0.,1.,0.));
#68193=DIRECTION('',(0.,0.,1.));
#68194=DIRECTION('',(0.,1.,0.));
#68195=DIRECTION('',(0.,0.,1.));
#68196=DIRECTION('',(0.,0.,1.));
#68197=DIRECTION('',(1.,0.,0.));
#68198=DIRECTION('',(0.,1.,0.));
#68199=DIRECTION('',(0.,0.,1.));
#68200=DIRECTION('',(0.,1.,0.));
#68201=DIRECTION('',(0.,0.,1.));
#68202=DIRECTION('',(0.,1.,0.));
#68203=DIRECTION('',(0.,0.,1.));
#68204=DIRECTION('',(0.,1.,0.));
#68205=DIRECTION('',(0.,0.,1.));
#68206=DIRECTION('',(0.,1.,0.));
#68207=DIRECTION('',(0.,0.,1.));
#68208=DIRECTION('',(0.,1.,0.));
#68209=DIRECTION('',(0.,0.,1.));
#68210=DIRECTION('',(0.,1.,0.));
#68211=DIRECTION('',(0.,0.,1.));
#68212=DIRECTION('',(0.,1.,0.));
#68213=DIRECTION('',(0.,0.,1.));
#68214=DIRECTION('',(0.,1.,0.));
#68215=DIRECTION('',(0.,0.,1.));
#68216=DIRECTION('',(0.,1.,0.));
#68217=DIRECTION('',(0.,0.,1.));
#68218=DIRECTION('',(0.,1.,0.));
#68219=DIRECTION('',(0.,0.,1.));
#68220=DIRECTION('',(0.,1.,0.));
#68221=DIRECTION('',(0.,0.,1.));
#68222=DIRECTION('',(0.,1.,0.));
#68223=DIRECTION('',(0.,0.,1.));
#68224=DIRECTION('',(0.,1.,0.));
#68225=DIRECTION('',(0.,0.,1.));
#68226=DIRECTION('',(0.,1.,0.));
#68227=DIRECTION('',(0.,0.,1.));
#68228=DIRECTION('',(0.,1.,0.));
#68229=DIRECTION('',(0.,0.,1.));
#68230=DIRECTION('',(0.,1.,0.));
#68231=DIRECTION('',(0.,0.,1.));
#68232=DIRECTION('',(0.,1.,0.));
#68233=DIRECTION('',(0.,0.,1.));
#68234=DIRECTION('',(0.,1.,0.));
#68235=DIRECTION('',(0.,0.,1.));
#68236=DIRECTION('',(0.,1.,0.));
#68237=DIRECTION('',(0.,0.,1.));
#68238=DIRECTION('',(0.,1.,0.));
#68239=DIRECTION('',(0.,0.,1.));
#68240=DIRECTION('',(0.,1.,0.));
#68241=DIRECTION('',(0.,0.,1.));
#68242=DIRECTION('',(0.,1.,0.));
#68243=DIRECTION('',(0.,0.,1.));
#68244=DIRECTION('',(0.,1.,0.));
#68245=DIRECTION('',(0.,0.,1.));
#68246=DIRECTION('',(0.,1.,0.));
#68247=DIRECTION('',(0.,0.,1.));
#68248=DIRECTION('',(0.,1.,0.));
#68249=DIRECTION('',(0.,0.,1.));
#68250=DIRECTION('',(0.,1.,0.));
#68251=DIRECTION('',(0.,0.,1.));
#68252=DIRECTION('',(0.,1.,0.));
#68253=DIRECTION('',(0.,0.,1.));
#68254=DIRECTION('',(0.,1.,0.));
#68255=DIRECTION('',(0.,0.,1.));
#68256=DIRECTION('',(0.,1.,0.));
#68257=DIRECTION('',(0.,0.,1.));
#68258=CARTESIAN_POINT('',(0.,0.,0.));
#68259=CARTESIAN_POINT('',(0.,0.,0.));
#68260=CARTESIAN_POINT('Origin',(34.2,0.,0.));
#68261=CARTESIAN_POINT('',(35.,39.0489657041002,-6.5831814071929));
#68262=CARTESIAN_POINT('',(35.,38.9456055698919,-7.16936585720129));
#68263=CARTESIAN_POINT('Origin',(35.,0.,0.));
#68264=CARTESIAN_POINT('',(33.4246193974437,37.6602615890763,-5.25132148728276));
#68265=CARTESIAN_POINT('Ctrl Pts',(33.4246193974437,37.6602615890763,-5.25132148728276));
#68266=CARTESIAN_POINT('Ctrl Pts',(34.1981589442507,38.350106913703,-5.90521241418151));
#68267=CARTESIAN_POINT('Ctrl Pts',(35.,39.0489657041002,-6.5831814071929));
#68268=CARTESIAN_POINT('',(33.4246193974437,37.1851276398516,-7.94594001540395));
#68269=CARTESIAN_POINT('Ctrl Pts',(33.4246193974437,37.1851276398516,-7.94594001540396));
#68270=CARTESIAN_POINT('Ctrl Pts',(33.3753965426192,37.4226946144693,-6.59863075131265));
#68271=CARTESIAN_POINT('Ctrl Pts',(33.4246193974437,37.6602615890763,-5.25132148728276));
#68272=CARTESIAN_POINT('Ctrl Pts',(35.,38.9456055698919,-7.1693658572013));
#68273=CARTESIAN_POINT('Ctrl Pts',(34.1981589442511,38.0570140694247,-7.56742453339956));
#68274=CARTESIAN_POINT('Ctrl Pts',(33.4246193974437,37.1851276398516,-7.94594001540395));
#68275=CARTESIAN_POINT('Origin',(34.2,0.,0.));
#68276=CARTESIAN_POINT('',(35.,37.3125667178958,-13.2639498235849));
#68277=CARTESIAN_POINT('',(35.,37.1089869948545,-13.8232805156997));
#68278=CARTESIAN_POINT('Origin',(35.,0.,0.));
#68279=CARTESIAN_POINT('',(33.4246193974437,36.1762351867803,-11.7111779096387));
#68280=CARTESIAN_POINT('Ctrl Pts',(33.4246193974437,36.1762351867803,-11.7111779096387));
#68281=CARTESIAN_POINT('Ctrl Pts',(34.1981589442499,36.7420532430025,-12.4749251475656));
#68282=CARTESIAN_POINT('Ctrl Pts',(35.,37.3125667178958,-13.2639498235849));
#68283=CARTESIAN_POINT('',(33.4246193974437,35.2404039929487,-14.2823529831122));
#68284=CARTESIAN_POINT('Ctrl Pts',(33.4246193974437,35.2404039929487,-14.2823529831122));
#68285=CARTESIAN_POINT('Ctrl Pts',(33.3753965426192,35.7083195898752,-12.9967654463461));
#68286=CARTESIAN_POINT('Ctrl Pts',(33.4246193974437,36.1762351867803,-11.7111779096387));
#68287=CARTESIAN_POINT('Ctrl Pts',(35.,37.1089869948545,-13.8232805156997));
#68288=CARTESIAN_POINT('Ctrl Pts',(34.1981589442488,36.1647730322046,-14.0609894914277));
#68289=CARTESIAN_POINT('Ctrl Pts',(33.4246193974437,35.2404039929487,-14.2823529831122));
#68290=CARTESIAN_POINT('Origin',(34.2,0.,0.));
#68291=CARTESIAN_POINT('',(35.,34.4424442730379,-19.5416998364696));
#68292=CARTESIAN_POINT('',(35.,34.1448306280319,-20.0571817906459));
#68293=CARTESIAN_POINT('Origin',(35.,0.,0.));
#68294=CARTESIAN_POINT('',(33.4246193974437,33.5930121843923,-17.8151961173521));
#68295=CARTESIAN_POINT('Ctrl Pts',(33.4246193974437,33.5930121843923,-17.8151961173521));
#68296=CARTESIAN_POINT('Ctrl Pts',(34.1981589442498,34.01761087689,-18.6655935929581));
#68297=CARTESIAN_POINT('Ctrl Pts',(35.,34.4424442730379,-19.5416998364696));
#68298=CARTESIAN_POINT('',(33.4246193974437,32.224918503225,-20.1848038826479));
#68299=CARTESIAN_POINT('Ctrl Pts',(33.4246193974437,32.224918503225,-20.1848038826479));
#68300=CARTESIAN_POINT('Ctrl Pts',(33.3753965426192,32.9089653438242,-18.999999999973));
#68301=CARTESIAN_POINT('Ctrl Pts',(33.4246193974437,33.5930121843923,-17.8151961173521));
#68302=CARTESIAN_POINT('Ctrl Pts',(35.,34.1448306280319,-20.0571817906459));
#68303=CARTESIAN_POINT('Ctrl Pts',(34.1981589442497,33.1736836666627,-20.1273183989616));
#68304=CARTESIAN_POINT('Ctrl Pts',(33.4246193974437,32.224918503225,-20.1848038826479));
#68305=CARTESIAN_POINT('Origin',(34.2,0.,0.));
#68306=CARTESIAN_POINT('',(35.,30.5258055876616,-25.2256851884005));
#68307=CARTESIAN_POINT('',(35.,30.1432008606945,-25.6816557463071));
#68308=CARTESIAN_POINT('Origin',(35.,0.,0.));
#68309=CARTESIAN_POINT('',(33.4246193974437,29.989082505666,-23.3779086059641));
#68310=CARTESIAN_POINT('Ctrl Pts',(33.4246193974437,29.989082505666,-23.3779086059641));
#68311=CARTESIAN_POINT('Ctrl Pts',(34.1981589442508,30.2595606180253,-24.2891174222761));
#68312=CARTESIAN_POINT('Ctrl Pts',(35.,30.5258055876616,-25.2256851884005));
#68313=CARTESIAN_POINT('',(33.4246193974437,28.2302951713763,-25.4739497302129));
#68314=CARTESIAN_POINT('Ctrl Pts',(33.4246193974437,28.2302951713763,-25.4739497302129));
#68315=CARTESIAN_POINT('Ctrl Pts',(33.3753965426191,29.1096888385412,-24.4259291680646));
#68316=CARTESIAN_POINT('Ctrl Pts',(33.4246193974437,29.989082505666,-23.3779086059641));
#68317=CARTESIAN_POINT('Ctrl Pts',(35.,30.1432008606945,-25.6816557463071));
#68318=CARTESIAN_POINT('Ctrl Pts',(34.1981589442493,29.1746287096016,-25.5820889218577));
#68319=CARTESIAN_POINT('Ctrl Pts',(33.4246193974437,28.2302951713763,-25.4739497302129));
#68320=CARTESIAN_POINT('Origin',(34.2,0.,0.));
#68321=CARTESIAN_POINT('',(35.,25.6816557463071,-30.1432008606945));
#68322=CARTESIAN_POINT('',(35.,25.2256851884005,-30.5258055876616));
#68323=CARTESIAN_POINT('Origin',(35.,0.,0.));
#68324=CARTESIAN_POINT('',(33.4246193974437,25.4739497302129,-28.2302951713764));
#68325=CARTESIAN_POINT('Ctrl Pts',(33.4246193974437,25.4739497302129,-28.2302951713764));
#68326=CARTESIAN_POINT('Ctrl Pts',(34.198158944251,25.5820889218579,-29.1746287096037));
#68327=CARTESIAN_POINT('Ctrl Pts',(35.,25.6816557463071,-30.1432008606945));
#68328=CARTESIAN_POINT('',(33.4246193974437,23.3779086059641,-29.989082505666));
#68329=CARTESIAN_POINT('Ctrl Pts',(33.4246193974437,23.3779086059641,-29.989082505666));
#68330=CARTESIAN_POINT('Ctrl Pts',(33.3753965426192,24.4259291681124,-29.1096888385011));
#68331=CARTESIAN_POINT('Ctrl Pts',(33.4246193974437,25.4739497302129,-28.2302951713764));
#68332=CARTESIAN_POINT('Ctrl Pts',(35.,25.2256851884005,-30.5258055876616));
#68333=CARTESIAN_POINT('Ctrl Pts',(34.1981589442506,24.2891174222758,-30.2595606180253));
#68334=CARTESIAN_POINT('Ctrl Pts',(33.4246193974437,23.3779086059641,-29.989082505666));
#68335=CARTESIAN_POINT('Origin',(34.2,0.,0.));
#68336=CARTESIAN_POINT('',(35.,20.0571817906459,-34.1448306280319));
#68337=CARTESIAN_POINT('',(35.,19.5416998364696,-34.4424442730379));
#68338=CARTESIAN_POINT('Origin',(35.,0.,0.));
#68339=CARTESIAN_POINT('',(33.4246193974437,20.1848038826479,-32.224918503225));
#68340=CARTESIAN_POINT('Ctrl Pts',(33.4246193974437,20.1848038826479,-32.224918503225));
#68341=CARTESIAN_POINT('Ctrl Pts',(34.1981589442498,20.1273183989615,-33.1736836666628));
#68342=CARTESIAN_POINT('Ctrl Pts',(35.,20.0571817906459,-34.1448306280319));
#68343=CARTESIAN_POINT('',(33.4246193974437,17.8151961173521,-33.5930121843923));
#68344=CARTESIAN_POINT('Ctrl Pts',(33.4246193974437,17.8151961173521,-33.5930121843923));
#68345=CARTESIAN_POINT('Ctrl Pts',(33.3753965426191,19.000000000027,-32.9089653437931));
#68346=CARTESIAN_POINT('Ctrl Pts',(33.4246193974437,20.1848038826479,-32.224918503225));
#68347=CARTESIAN_POINT('Ctrl Pts',(35.,19.5416998364696,-34.4424442730379));
#68348=CARTESIAN_POINT('Ctrl Pts',(34.1981589442509,18.6655935929594,-34.0176108768906));
#68349=CARTESIAN_POINT('Ctrl Pts',(33.4246193974437,17.8151961173521,-33.5930121843923));
#68350=CARTESIAN_POINT('Origin',(34.2,0.,0.));
#68351=CARTESIAN_POINT('',(35.,13.8232805156996,-37.1089869948545));
#68352=CARTESIAN_POINT('',(35.,13.2639498235848,-37.3125667178958));
#68353=CARTESIAN_POINT('Origin',(35.,0.,0.));
#68354=CARTESIAN_POINT('',(33.4246193974437,14.2823529831122,-35.2404039929487));
#68355=CARTESIAN_POINT('Ctrl Pts',(33.4246193974437,14.2823529831122,-35.2404039929487));
#68356=CARTESIAN_POINT('Ctrl Pts',(34.1981589442504,14.0609894914272,-36.1647730322064));
#68357=CARTESIAN_POINT('Ctrl Pts',(35.,13.8232805156996,-37.1089869948545));
#68358=CARTESIAN_POINT('',(33.4246193974437,11.7111779096386,-36.1762351867803));
#68359=CARTESIAN_POINT('Ctrl Pts',(33.4246193974437,11.7111779096386,-36.1762351867803));
#68360=CARTESIAN_POINT('Ctrl Pts',(33.3753965426192,12.9967654464047,-35.7083195898539));
#68361=CARTESIAN_POINT('Ctrl Pts',(33.4246193974437,14.2823529831122,-35.2404039929487));
#68362=CARTESIAN_POINT('Ctrl Pts',(35.,13.2639498235848,-37.3125667178958));
#68363=CARTESIAN_POINT('Ctrl Pts',(34.1981589442509,12.4749251475665,-36.7420532430032));
#68364=CARTESIAN_POINT('Ctrl Pts',(33.4246193974437,11.7111779096386,-36.1762351867803));
#68365=CARTESIAN_POINT('Origin',(34.2,0.,0.));
#68366=CARTESIAN_POINT('',(35.,7.16936585720128,-38.9456055698919));
#68367=CARTESIAN_POINT('',(35.,6.58318140719288,-39.0489657041002));
#68368=CARTESIAN_POINT('Origin',(35.,0.,0.));
#68369=CARTESIAN_POINT('',(33.4246193974437,7.94594001540394,-37.1851276398516));
#68370=CARTESIAN_POINT('Ctrl Pts',(33.4246193974437,7.94594001540394,-37.1851276398516));
#68371=CARTESIAN_POINT('Ctrl Pts',(34.1981589442496,7.56742453340028,-38.057014069423));
#68372=CARTESIAN_POINT('Ctrl Pts',(35.,7.16936585720128,-38.9456055698919));
#68373=CARTESIAN_POINT('',(33.4246193974437,5.25132148728273,-37.6602615890763));
#68374=CARTESIAN_POINT('Ctrl Pts',(33.4246193974437,5.25132148728273,-37.6602615890763));
#68375=CARTESIAN_POINT('Ctrl Pts',(33.3753965426191,6.59863075137404,-37.4226946144585));
#68376=CARTESIAN_POINT('Ctrl Pts',(33.4246193974437,7.94594001540394,-37.1851276398516));
#68377=CARTESIAN_POINT('Ctrl Pts',(35.,6.58318140719289,-39.0489657041002));
#68378=CARTESIAN_POINT('Ctrl Pts',(34.1981589442503,5.90521241418118,-38.3501069137027));
#68379=CARTESIAN_POINT('Ctrl Pts',(33.4246193974437,5.25132148728273,-37.6602615890763));
#68380=CARTESIAN_POINT('Origin',(34.2,0.,0.));
#68381=CARTESIAN_POINT('',(35.,0.297613645006055,-39.5988816271155));
#68382=CARTESIAN_POINT('',(35.,-0.297613645006067,-39.5988816271155));
#68383=CARTESIAN_POINT('Origin',(35.,0.,0.));
#68384=CARTESIAN_POINT('',(33.4246193974437,1.36809368116733,-38.));
#68385=CARTESIAN_POINT('Ctrl Pts',(33.4246193974437,1.36809368116733,-38.));
#68386=CARTESIAN_POINT('Ctrl Pts',(34.1981589442509,0.843927210226466,-38.7929119919208));
#68387=CARTESIAN_POINT('Ctrl Pts',(35.,0.297613645006061,-39.5988816271155));
#68388=CARTESIAN_POINT('',(33.4246193974437,-1.36809368116734,-38.));
#68389=CARTESIAN_POINT('Ctrl Pts',(33.4246193974437,-1.36809368116734,-38.));
#68390=CARTESIAN_POINT('Ctrl Pts',(33.3753965426191,3.11772829775236E-11,
-38.));
#68391=CARTESIAN_POINT('Ctrl Pts',(33.4246193974437,1.36809368116733,-38.));
#68392=CARTESIAN_POINT('Ctrl Pts',(35.,-0.297613645006074,-39.5988816271155));
#68393=CARTESIAN_POINT('Ctrl Pts',(34.1981589442498,-0.843927210227242,
-38.7929119919196));
#68394=CARTESIAN_POINT('Ctrl Pts',(33.4246193974437,-1.36809368116734,-38.));
#68395=CARTESIAN_POINT('Origin',(34.2,0.,0.));
#68396=CARTESIAN_POINT('',(35.,-6.5831814071929,-39.0489657041002));
#68397=CARTESIAN_POINT('',(35.,-7.16936585720129,-38.9456055698919));
#68398=CARTESIAN_POINT('Origin',(35.,0.,0.));
#68399=CARTESIAN_POINT('',(33.4246193974437,-5.25132148728275,-37.6602615890763));
#68400=CARTESIAN_POINT('Ctrl Pts',(33.4246193974437,-5.25132148728275,-37.6602615890763));
#68401=CARTESIAN_POINT('Ctrl Pts',(34.19815894425,-5.90521241418094,-38.3501069137024));
#68402=CARTESIAN_POINT('Ctrl Pts',(35.,-6.5831814071929,-39.0489657041002));
#68403=CARTESIAN_POINT('',(33.4246193974437,-7.94594001540395,-37.1851276398516));
#68404=CARTESIAN_POINT('Ctrl Pts',(33.4246193974437,-7.94594001540395,-37.1851276398516));
#68405=CARTESIAN_POINT('Ctrl Pts',(33.3753965426192,-6.59863075131264,-37.4226946144693));
#68406=CARTESIAN_POINT('Ctrl Pts',(33.4246193974437,-5.25132148728275,-37.6602615890763));
#68407=CARTESIAN_POINT('Ctrl Pts',(35.,-7.16936585720129,-38.9456055698919));
#68408=CARTESIAN_POINT('Ctrl Pts',(34.1981589442516,-7.56742453339929,-38.0570140694253));
#68409=CARTESIAN_POINT('Ctrl Pts',(33.4246193974437,-7.94594001540395,-37.1851276398516));
#68410=CARTESIAN_POINT('Origin',(34.2,0.,0.));
#68411=CARTESIAN_POINT('',(35.,-13.2639498235849,-37.3125667178958));
#68412=CARTESIAN_POINT('',(35.,-13.8232805156997,-37.1089869948545));
#68413=CARTESIAN_POINT('Origin',(35.,0.,0.));
#68414=CARTESIAN_POINT('',(33.4246193974437,-11.7111779096387,-36.1762351867803));
#68415=CARTESIAN_POINT('Ctrl Pts',(33.4246193974437,-11.7111779096387,-36.1762351867803));
#68416=CARTESIAN_POINT('Ctrl Pts',(34.1981589442511,-12.4749251475667,-36.7420532430033));
#68417=CARTESIAN_POINT('Ctrl Pts',(35.,-13.2639498235849,-37.3125667178958));
#68418=CARTESIAN_POINT('',(33.4246193974437,-14.2823529831122,-35.2404039929487));
#68419=CARTESIAN_POINT('Ctrl Pts',(33.4246193974437,-14.2823529831122,-35.2404039929487));
#68420=CARTESIAN_POINT('Ctrl Pts',(33.3753965426192,-12.9967654463461,-35.7083195898752));
#68421=CARTESIAN_POINT('Ctrl Pts',(33.4246193974437,-11.7111779096387,-36.1762351867803));
#68422=CARTESIAN_POINT('Ctrl Pts',(35.,-13.8232805156997,-37.1089869948545));
#68423=CARTESIAN_POINT('Ctrl Pts',(34.1981589442496,-14.0609894914275,-36.1647730322054));
#68424=CARTESIAN_POINT('Ctrl Pts',(33.4246193974437,-14.2823529831122,-35.2404039929487));
#68425=CARTESIAN_POINT('Origin',(34.2,0.,0.));
#68426=CARTESIAN_POINT('',(35.,-19.5416998364696,-34.4424442730379));
#68427=CARTESIAN_POINT('',(35.,-20.0571817906459,-34.1448306280318));
#68428=CARTESIAN_POINT('Origin',(35.,0.,0.));
#68429=CARTESIAN_POINT('',(33.4246193974437,-17.8151961173521,-33.5930121843923));
#68430=CARTESIAN_POINT('Ctrl Pts',(33.4246193974437,-17.8151961173521,-33.5930121843923));
#68431=CARTESIAN_POINT('Ctrl Pts',(34.1981589442509,-18.6655935929594,-34.0176108768906));
#68432=CARTESIAN_POINT('Ctrl Pts',(35.,-19.5416998364696,-34.4424442730379));
#68433=CARTESIAN_POINT('',(33.4246193974437,-20.1848038826479,-32.224918503225));
#68434=CARTESIAN_POINT('Ctrl Pts',(33.4246193974437,-20.1848038826479,-32.224918503225));
#68435=CARTESIAN_POINT('Ctrl Pts',(33.3753965426192,-18.999999999973,-32.9089653438242));
#68436=CARTESIAN_POINT('Ctrl Pts',(33.4246193974437,-17.8151961173521,-33.5930121843923));
#68437=CARTESIAN_POINT('Ctrl Pts',(35.,-20.0571817906459,-34.1448306280319));
#68438=CARTESIAN_POINT('Ctrl Pts',(34.1981589442493,-20.1273183989616,-33.1736836666622));
#68439=CARTESIAN_POINT('Ctrl Pts',(33.4246193974437,-20.1848038826479,-32.224918503225));
#68440=CARTESIAN_POINT('Origin',(34.2,0.,0.));
#68441=CARTESIAN_POINT('',(35.,-25.2256851884005,-30.5258055876616));
#68442=CARTESIAN_POINT('',(35.,-25.6816557463071,-30.1432008606945));
#68443=CARTESIAN_POINT('Origin',(35.,0.,0.));
#68444=CARTESIAN_POINT('',(33.4246193974437,-23.3779086059641,-29.989082505666));
#68445=CARTESIAN_POINT('Ctrl Pts',(33.4246193974437,-23.3779086059641,-29.989082505666));
#68446=CARTESIAN_POINT('Ctrl Pts',(34.1981589442511,-24.2891174222764,-30.2595606180254));
#68447=CARTESIAN_POINT('Ctrl Pts',(35.,-25.2256851884005,-30.5258055876616));
#68448=CARTESIAN_POINT('',(33.4246193974437,-25.4739497302129,-28.2302951713763));
#68449=CARTESIAN_POINT('Ctrl Pts',(33.4246193974437,-25.4739497302129,-28.2302951713763));
#68450=CARTESIAN_POINT('Ctrl Pts',(33.3753965426191,-24.4259291680646,-29.1096888385412));
#68451=CARTESIAN_POINT('Ctrl Pts',(33.4246193974437,-23.3779086059641,-29.989082505666));
#68452=CARTESIAN_POINT('Ctrl Pts',(35.,-25.6816557463071,-30.1432008606945));
#68453=CARTESIAN_POINT('Ctrl Pts',(34.1981589442511,-25.582088921858,-29.1746287096039));
#68454=CARTESIAN_POINT('Ctrl Pts',(33.4246193974437,-25.4739497302129,-28.2302951713763));
#68455=CARTESIAN_POINT('Origin',(34.2,0.,0.));
#68456=CARTESIAN_POINT('',(35.,-30.1432008606945,-25.6816557463071));
#68457=CARTESIAN_POINT('',(35.,-30.5258055876616,-25.2256851884005));
#68458=CARTESIAN_POINT('Origin',(35.,0.,0.));
#68459=CARTESIAN_POINT('',(33.4246193974437,-28.2302951713764,-25.4739497302129));
#68460=CARTESIAN_POINT('Ctrl Pts',(33.4246193974437,-28.2302951713764,-25.4739497302129));
#68461=CARTESIAN_POINT('Ctrl Pts',(34.1981589442485,-29.1746287096007,-25.5820889218576));
#68462=CARTESIAN_POINT('Ctrl Pts',(35.,-30.1432008606945,-25.6816557463071));
#68463=CARTESIAN_POINT('',(33.4246193974437,-29.989082505666,-23.3779086059641));
#68464=CARTESIAN_POINT('Ctrl Pts',(33.4246193974437,-29.989082505666,-23.3779086059641));
#68465=CARTESIAN_POINT('Ctrl Pts',(33.3753965426192,-29.1096888385011,-24.4259291681124));
#68466=CARTESIAN_POINT('Ctrl Pts',(33.4246193974437,-28.2302951713764,-25.4739497302129));
#68467=CARTESIAN_POINT('Ctrl Pts',(35.,-30.5258055876616,-25.2256851884005));
#68468=CARTESIAN_POINT('Ctrl Pts',(34.1981589442495,-30.2595606180249,-24.2891174222746));
#68469=CARTESIAN_POINT('Ctrl Pts',(33.4246193974437,-29.989082505666,-23.3779086059641));
#68470=CARTESIAN_POINT('Origin',(34.2,0.,0.));
#68471=CARTESIAN_POINT('',(35.,-34.1448306280319,-20.0571817906459));
#68472=CARTESIAN_POINT('',(35.,-34.4424442730379,-19.5416998364696));
#68473=CARTESIAN_POINT('Origin',(35.,0.,0.));
#68474=CARTESIAN_POINT('',(33.4246193974437,-32.224918503225,-20.1848038826479));
#68475=CARTESIAN_POINT('Ctrl Pts',(33.4246193974437,-32.224918503225,-20.1848038826479));
#68476=CARTESIAN_POINT('Ctrl Pts',(34.1981589442514,-33.1736836666648,-20.1273183989614));
#68477=CARTESIAN_POINT('Ctrl Pts',(35.,-34.1448306280319,-20.0571817906459));
#68478=CARTESIAN_POINT('',(33.4246193974437,-33.5930121843923,-17.8151961173521));
#68479=CARTESIAN_POINT('Ctrl Pts',(33.4246193974437,-33.5930121843923,-17.8151961173521));
#68480=CARTESIAN_POINT('Ctrl Pts',(33.3753965426191,-32.9089653437931,-19.000000000027));
#68481=CARTESIAN_POINT('Ctrl Pts',(33.4246193974437,-32.224918503225,-20.1848038826479));
#68482=CARTESIAN_POINT('Ctrl Pts',(35.,-34.4424442730379,-19.5416998364696));
#68483=CARTESIAN_POINT('Ctrl Pts',(34.1981589442506,-34.0176108768905,-18.665593592959));
#68484=CARTESIAN_POINT('Ctrl Pts',(33.4246193974437,-33.5930121843923,-17.8151961173521));
#68485=CARTESIAN_POINT('Origin',(34.2,0.,0.));
#68486=CARTESIAN_POINT('',(35.,-37.1089869948545,-13.8232805156996));
#68487=CARTESIAN_POINT('',(35.,-37.3125667178958,-13.2639498235848));
#68488=CARTESIAN_POINT('Origin',(35.,0.,0.));
#68489=CARTESIAN_POINT('',(33.4246193974437,-35.2404039929487,-14.2823529831122));
#68490=CARTESIAN_POINT('Ctrl Pts',(33.4246193974437,-35.2404039929487,-14.2823529831122));
#68491=CARTESIAN_POINT('Ctrl Pts',(34.1981589442501,-36.1647730322061,-14.0609894914273));
#68492=CARTESIAN_POINT('Ctrl Pts',(35.,-37.1089869948545,-13.8232805156996));
#68493=CARTESIAN_POINT('',(33.4246193974437,-36.1762351867803,-11.7111779096386));
#68494=CARTESIAN_POINT('Ctrl Pts',(33.4246193974437,-36.1762351867803,-11.7111779096386));
#68495=CARTESIAN_POINT('Ctrl Pts',(33.3753965426192,-35.7083195898539,-12.9967654464047));
#68496=CARTESIAN_POINT('Ctrl Pts',(33.4246193974437,-35.2404039929487,-14.2823529831122));
#68497=CARTESIAN_POINT('Ctrl Pts',(35.,-37.3125667178958,-13.2639498235848));
#68498=CARTESIAN_POINT('Ctrl Pts',(34.1981589442499,-36.7420532430025,-12.4749251475656));
#68499=CARTESIAN_POINT('Ctrl Pts',(33.4246193974437,-36.1762351867803,-11.7111779096386));
#68500=CARTESIAN_POINT('Origin',(34.2,0.,0.));
#68501=CARTESIAN_POINT('',(35.,-38.9456055698919,-7.16936585720128));
#68502=CARTESIAN_POINT('',(35.,-39.0489657041002,-6.58318140719289));
#68503=CARTESIAN_POINT('Origin',(35.,0.,0.));
#68504=CARTESIAN_POINT('',(33.4246193974437,-37.1851276398516,-7.94594001540395));
#68505=CARTESIAN_POINT('Ctrl Pts',(33.4246193974437,-37.1851276398516,-7.94594001540395));
#68506=CARTESIAN_POINT('Ctrl Pts',(34.1981589442497,-38.0570140694232,-7.5674245334002));
#68507=CARTESIAN_POINT('Ctrl Pts',(35.,-38.9456055698919,-7.16936585720128));
#68508=CARTESIAN_POINT('',(33.4246193974437,-37.6602615890763,-5.25132148728274));
#68509=CARTESIAN_POINT('Ctrl Pts',(33.4246193974437,-37.6602615890763,-5.25132148728274));
#68510=CARTESIAN_POINT('Ctrl Pts',(33.3753965426191,-37.4226946144585,-6.59863075137405));
#68511=CARTESIAN_POINT('Ctrl Pts',(33.4246193974437,-37.1851276398516,-7.94594001540395));
#68512=CARTESIAN_POINT('Ctrl Pts',(35.,-39.0489657041002,-6.58318140719289));
#68513=CARTESIAN_POINT('Ctrl Pts',(34.1981589442488,-38.3501069137014,-5.90521241417989));
#68514=CARTESIAN_POINT('Ctrl Pts',(33.4246193974437,-37.6602615890763,-5.25132148728274));
#68515=CARTESIAN_POINT('Origin',(34.2,0.,0.));
#68516=CARTESIAN_POINT('',(35.,-39.5988816271155,-0.29761364500606));
#68517=CARTESIAN_POINT('',(35.,-39.5988816271155,0.297613645006073));
#68518=CARTESIAN_POINT('Origin',(35.,0.,0.));
#68519=CARTESIAN_POINT('',(33.4246193974437,-38.,-1.36809368116733));
#68520=CARTESIAN_POINT('Ctrl Pts',(33.4246193974437,-38.,-1.36809368116733));
#68521=CARTESIAN_POINT('Ctrl Pts',(34.1981589442507,-38.7929119919205,-0.843927210226627));
#68522=CARTESIAN_POINT('Ctrl Pts',(35.,-39.5988816271155,-0.297613645006064));
#68523=CARTESIAN_POINT('',(33.4246193974437,-38.,1.36809368116734));
#68524=CARTESIAN_POINT('Ctrl Pts',(33.4246193974437,-38.,1.36809368116734));
#68525=CARTESIAN_POINT('Ctrl Pts',(33.3753965426192,-38.,-3.11753400872306E-11));
#68526=CARTESIAN_POINT('Ctrl Pts',(33.4246193974437,-38.,-1.36809368116733));
#68527=CARTESIAN_POINT('Ctrl Pts',(35.,-39.5988816271155,0.297613645006073));
#68528=CARTESIAN_POINT('Ctrl Pts',(34.1981589442507,-38.7929119919206,0.843927210226618));
#68529=CARTESIAN_POINT('Ctrl Pts',(33.4246193974437,-38.,1.36809368116734));
#68530=CARTESIAN_POINT('Origin',(34.2,0.,0.));
#68531=CARTESIAN_POINT('',(35.,-39.0489657041001,6.58318140719291));
#68532=CARTESIAN_POINT('',(35.,-38.9456055698919,7.16936585720131));
#68533=CARTESIAN_POINT('Origin',(35.,0.,0.));
#68534=CARTESIAN_POINT('',(33.4246193974437,-37.6602615890763,5.25132148728276));
#68535=CARTESIAN_POINT('Ctrl Pts',(33.4246193974437,-37.6602615890763,5.25132148728276));
#68536=CARTESIAN_POINT('Ctrl Pts',(34.1981589442494,-38.3501069137019,5.90521241418043));
#68537=CARTESIAN_POINT('Ctrl Pts',(35.,-39.0489657041001,6.58318140719291));
#68538=CARTESIAN_POINT('',(33.4246193974437,-37.1851276398516,7.94594001540397));
#68539=CARTESIAN_POINT('Ctrl Pts',(33.4246193974437,-37.1851276398516,7.94594001540397));
#68540=CARTESIAN_POINT('Ctrl Pts',(33.3753965426191,-37.4226946144693,6.59863075131266));
#68541=CARTESIAN_POINT('Ctrl Pts',(33.4246193974437,-37.6602615890763,5.25132148728276));
#68542=CARTESIAN_POINT('Ctrl Pts',(35.,-38.9456055698919,7.16936585720131));
#68543=CARTESIAN_POINT('Ctrl Pts',(34.1981589442514,-38.057014069425,7.56742453339942));
#68544=CARTESIAN_POINT('Ctrl Pts',(33.4246193974437,-37.1851276398516,7.94594001540397));
#68545=CARTESIAN_POINT('Origin',(34.2,0.,0.));
#68546=CARTESIAN_POINT('',(35.,-37.3125667178958,13.2639498235848));
#68547=CARTESIAN_POINT('',(35.,-37.1089869948545,13.8232805156996));
#68548=CARTESIAN_POINT('Origin',(35.,0.,0.));
#68549=CARTESIAN_POINT('',(33.4246193974437,-36.1762351867803,11.7111779096386));
#68550=CARTESIAN_POINT('Ctrl Pts',(33.4246193974437,-36.1762351867803,11.7111779096386));
#68551=CARTESIAN_POINT('Ctrl Pts',(34.1981589442498,-36.7420532430025,12.4749251475655));
#68552=CARTESIAN_POINT('Ctrl Pts',(35.,-37.3125667178958,13.2639498235848));
#68553=CARTESIAN_POINT('',(33.4246193974437,-35.2404039929487,14.2823529831122));
#68554=CARTESIAN_POINT('Ctrl Pts',(33.4246193974437,-35.2404039929487,14.2823529831122));
#68555=CARTESIAN_POINT('Ctrl Pts',(33.3753965426191,-35.7083195898752,12.9967654463461));
#68556=CARTESIAN_POINT('Ctrl Pts',(33.4246193974437,-36.1762351867803,11.7111779096386));
#68557=CARTESIAN_POINT('Ctrl Pts',(35.,-37.1089869948545,13.8232805156996));
#68558=CARTESIAN_POINT('Ctrl Pts',(34.1981589442512,-36.1647730322074,14.060989491427));
#68559=CARTESIAN_POINT('Ctrl Pts',(33.4246193974437,-35.2404039929487,14.2823529831122));
#68560=CARTESIAN_POINT('Origin',(34.2,0.,0.));
#68561=CARTESIAN_POINT('',(35.,-34.4424442730379,19.5416998364696));
#68562=CARTESIAN_POINT('',(35.,-34.1448306280319,20.0571817906459));
#68563=CARTESIAN_POINT('Origin',(35.,0.,0.));
#68564=CARTESIAN_POINT('',(33.4246193974437,-33.5930121843923,17.8151961173521));
#68565=CARTESIAN_POINT('Ctrl Pts',(33.4246193974437,-33.5930121843923,17.8151961173521));
#68566=CARTESIAN_POINT('Ctrl Pts',(34.1981589442509,-34.0176108768906,18.6655935929593));
#68567=CARTESIAN_POINT('Ctrl Pts',(35.,-34.4424442730379,19.5416998364696));
#68568=CARTESIAN_POINT('',(33.4246193974437,-32.224918503225,20.1848038826479));
#68569=CARTESIAN_POINT('Ctrl Pts',(33.4246193974437,-32.224918503225,20.1848038826479));
#68570=CARTESIAN_POINT('Ctrl Pts',(33.3753965426192,-32.9089653438243,18.999999999973));
#68571=CARTESIAN_POINT('Ctrl Pts',(33.4246193974437,-33.5930121843923,17.8151961173521));
#68572=CARTESIAN_POINT('Ctrl Pts',(35.,-34.1448306280319,20.0571817906459));
#68573=CARTESIAN_POINT('Ctrl Pts',(34.19815894425,-33.173683666663,20.1273183989615));
#68574=CARTESIAN_POINT('Ctrl Pts',(33.4246193974437,-32.224918503225,20.1848038826479));
#68575=CARTESIAN_POINT('Origin',(34.2,0.,0.));
#68576=CARTESIAN_POINT('',(35.,-30.5258055876616,25.2256851884005));
#68577=CARTESIAN_POINT('',(35.,-30.1432008606945,25.6816557463071));
#68578=CARTESIAN_POINT('Origin',(35.,0.,0.));
#68579=CARTESIAN_POINT('',(33.4246193974437,-29.989082505666,23.3779086059641));
#68580=CARTESIAN_POINT('Ctrl Pts',(33.4246193974437,-29.989082505666,23.3779086059641));
#68581=CARTESIAN_POINT('Ctrl Pts',(34.1981589442502,-30.2595606180251,24.2891174222754));
#68582=CARTESIAN_POINT('Ctrl Pts',(35.,-30.5258055876616,25.2256851884005));
#68583=CARTESIAN_POINT('',(33.4246193974437,-28.2302951713763,25.4739497302129));
#68584=CARTESIAN_POINT('Ctrl Pts',(33.4246193974437,-28.2302951713763,25.4739497302129));
#68585=CARTESIAN_POINT('Ctrl Pts',(33.3753965426192,-29.1096888385412,24.4259291680646));
#68586=CARTESIAN_POINT('Ctrl Pts',(33.4246193974437,-29.989082505666,23.3779086059641));
#68587=CARTESIAN_POINT('Ctrl Pts',(35.,-30.1432008606945,25.6816557463071));
#68588=CARTESIAN_POINT('Ctrl Pts',(34.1981589442515,-29.1746287096043,25.582088921858));
#68589=CARTESIAN_POINT('Ctrl Pts',(33.4246193974437,-28.2302951713763,25.4739497302129));
#68590=CARTESIAN_POINT('Origin',(34.2,0.,0.));
#68591=CARTESIAN_POINT('',(35.,-25.6816557463071,30.1432008606945));
#68592=CARTESIAN_POINT('',(35.,-25.2256851884005,30.5258055876616));
#68593=CARTESIAN_POINT('Origin',(35.,0.,0.));
#68594=CARTESIAN_POINT('',(33.4246193974437,-25.4739497302129,28.2302951713764));
#68595=CARTESIAN_POINT('Ctrl Pts',(33.4246193974437,-25.4739497302129,28.2302951713764));
#68596=CARTESIAN_POINT('Ctrl Pts',(34.1981589442499,-25.5820889218578,29.1746287096024));
#68597=CARTESIAN_POINT('Ctrl Pts',(35.,-25.6816557463071,30.1432008606945));
#68598=CARTESIAN_POINT('',(33.4246193974437,-23.3779086059641,29.989082505666));
#68599=CARTESIAN_POINT('Ctrl Pts',(33.4246193974437,-23.3779086059641,29.989082505666));
#68600=CARTESIAN_POINT('Ctrl Pts',(33.3753965426191,-24.4259291681124,29.1096888385011));
#68601=CARTESIAN_POINT('Ctrl Pts',(33.4246193974437,-25.4739497302129,28.2302951713764));
#68602=CARTESIAN_POINT('Ctrl Pts',(35.,-25.2256851884005,30.5258055876616));
#68603=CARTESIAN_POINT('Ctrl Pts',(34.1981589442511,-24.2891174222765,30.2595606180255));
#68604=CARTESIAN_POINT('Ctrl Pts',(33.4246193974437,-23.3779086059641,29.989082505666));
#68605=CARTESIAN_POINT('Origin',(34.2,0.,0.));
#68606=CARTESIAN_POINT('',(35.,-20.0571817906459,34.1448306280319));
#68607=CARTESIAN_POINT('',(35.,-19.5416998364696,34.4424442730379));
#68608=CARTESIAN_POINT('Origin',(35.,0.,0.));
#68609=CARTESIAN_POINT('',(33.4246193974437,-20.1848038826479,32.224918503225));
#68610=CARTESIAN_POINT('Ctrl Pts',(33.4246193974437,-20.1848038826479,32.224918503225));
#68611=CARTESIAN_POINT('Ctrl Pts',(34.1981589442516,-20.1273183989614,33.173683666665));
#68612=CARTESIAN_POINT('Ctrl Pts',(35.,-20.0571817906459,34.1448306280319));
#68613=CARTESIAN_POINT('',(33.4246193974437,-17.8151961173521,33.5930121843923));
#68614=CARTESIAN_POINT('Ctrl Pts',(33.4246193974437,-17.8151961173521,33.5930121843923));
#68615=CARTESIAN_POINT('Ctrl Pts',(33.3753965426191,-19.000000000027,32.9089653437931));
#68616=CARTESIAN_POINT('Ctrl Pts',(33.4246193974437,-20.1848038826479,32.224918503225));
#68617=CARTESIAN_POINT('Ctrl Pts',(35.,-19.5416998364696,34.4424442730379));
#68618=CARTESIAN_POINT('Ctrl Pts',(34.1981589442509,-18.6655935929593,34.0176108768906));
#68619=CARTESIAN_POINT('Ctrl Pts',(33.4246193974437,-17.8151961173521,33.5930121843923));
#68620=CARTESIAN_POINT('Origin',(34.2,0.,0.));
#68621=CARTESIAN_POINT('',(35.,-13.8232805156996,37.1089869948545));
#68622=CARTESIAN_POINT('',(35.,-13.2639498235848,37.3125667178958));
#68623=CARTESIAN_POINT('Origin',(35.,0.,0.));
#68624=CARTESIAN_POINT('',(33.4246193974437,-14.2823529831122,35.2404039929487));
#68625=CARTESIAN_POINT('Ctrl Pts',(33.4246193974437,-14.2823529831122,35.2404039929487));
#68626=CARTESIAN_POINT('Ctrl Pts',(34.1981589442515,-14.0609894914269,36.1647730322078));
#68627=CARTESIAN_POINT('Ctrl Pts',(35.,-13.8232805156996,37.1089869948545));
#68628=CARTESIAN_POINT('',(33.4246193974437,-11.7111779096386,36.1762351867803));
#68629=CARTESIAN_POINT('Ctrl Pts',(33.4246193974437,-11.7111779096386,36.1762351867803));
#68630=CARTESIAN_POINT('Ctrl Pts',(33.3753965426191,-12.9967654464047,35.7083195898539));
#68631=CARTESIAN_POINT('Ctrl Pts',(33.4246193974437,-14.2823529831122,35.2404039929487));
#68632=CARTESIAN_POINT('Ctrl Pts',(35.,-13.2639498235848,37.3125667178958));
#68633=CARTESIAN_POINT('Ctrl Pts',(34.1981589442494,-12.4749251475651,36.7420532430021));
#68634=CARTESIAN_POINT('Ctrl Pts',(33.4246193974437,-11.7111779096386,36.1762351867803));
#68635=CARTESIAN_POINT('Origin',(34.2,0.,0.));
#68636=CARTESIAN_POINT('',(35.,-7.16936585720129,38.9456055698919));
#68637=CARTESIAN_POINT('',(35.,-6.5831814071929,39.0489657041001));
#68638=CARTESIAN_POINT('Origin',(35.,0.,0.));
#68639=CARTESIAN_POINT('',(33.4246193974437,-7.94594001540395,37.1851276398516));
#68640=CARTESIAN_POINT('Ctrl Pts',(33.4246193974437,-7.94594001540395,37.1851276398516));
#68641=CARTESIAN_POINT('Ctrl Pts',(34.1981589442492,-7.56742453340049,38.0570140694225));
#68642=CARTESIAN_POINT('Ctrl Pts',(35.,-7.16936585720129,38.9456055698919));
#68643=CARTESIAN_POINT('',(33.4246193974437,-5.25132148728275,37.6602615890763));
#68644=CARTESIAN_POINT('Ctrl Pts',(33.4246193974437,-5.25132148728275,37.6602615890763));
#68645=CARTESIAN_POINT('Ctrl Pts',(33.3753965426191,-6.59863075137406,37.4226946144585));
#68646=CARTESIAN_POINT('Ctrl Pts',(33.4246193974437,-7.94594001540395,37.1851276398516));
#68647=CARTESIAN_POINT('Ctrl Pts',(35.,-6.5831814071929,39.0489657041001));
#68648=CARTESIAN_POINT('Ctrl Pts',(34.1981589442491,-5.90521241418012,38.3501069137016));
#68649=CARTESIAN_POINT('Ctrl Pts',(33.4246193974437,-5.25132148728275,37.6602615890762));
#68650=CARTESIAN_POINT('Origin',(34.2,0.,0.));
#68651=CARTESIAN_POINT('',(35.,-0.297613645006061,39.5988816271155));
#68652=CARTESIAN_POINT('',(35.,0.29761364500607,39.5988816271155));
#68653=CARTESIAN_POINT('Origin',(35.,0.,0.));
#68654=CARTESIAN_POINT('',(33.4246193974437,-1.36809368116733,38.));
#68655=CARTESIAN_POINT('Ctrl Pts',(33.4246193974437,-1.36809368116733,38.));
#68656=CARTESIAN_POINT('Ctrl Pts',(34.1981589442505,-0.843927210226743,
38.7929119919204));
#68657=CARTESIAN_POINT('Ctrl Pts',(35.,-0.297613645006066,39.5988816271155));
#68658=CARTESIAN_POINT('',(33.4246193974437,1.36809368116733,38.));
#68659=CARTESIAN_POINT('Ctrl Pts',(33.4246193974437,1.36809368116733,38.));
#68660=CARTESIAN_POINT('Ctrl Pts',(33.3753965426191,-3.11806136465975E-11,
38.));
#68661=CARTESIAN_POINT('Ctrl Pts',(33.4246193974437,-1.36809368116733,38.));
#68662=CARTESIAN_POINT('Ctrl Pts',(35.,0.297613645006069,39.5988816271155));
#68663=CARTESIAN_POINT('Ctrl Pts',(34.1981589442504,0.843927210226807,38.7929119919203));
#68664=CARTESIAN_POINT('Ctrl Pts',(33.4246193974437,1.36809368116733,38.));
#68665=CARTESIAN_POINT('Origin',(34.2,0.,0.));
#68666=CARTESIAN_POINT('',(35.,6.5831814071929,39.0489657041002));
#68667=CARTESIAN_POINT('',(35.,7.1693658572013,38.9456055698919));
#68668=CARTESIAN_POINT('Origin',(35.,0.,0.));
#68669=CARTESIAN_POINT('',(33.4246193974437,5.25132148728276,37.6602615890763));
#68670=CARTESIAN_POINT('Ctrl Pts',(33.4246193974437,5.25132148728276,37.6602615890763));
#68671=CARTESIAN_POINT('Ctrl Pts',(34.1981589442498,5.90521241418073,38.3501069137022));
#68672=CARTESIAN_POINT('Ctrl Pts',(35.,6.5831814071929,39.0489657041002));
#68673=CARTESIAN_POINT('',(33.4246193974437,7.94594001540395,37.1851276398516));
#68674=CARTESIAN_POINT('Ctrl Pts',(33.4246193974437,7.94594001540395,37.1851276398516));
#68675=CARTESIAN_POINT('Ctrl Pts',(33.3753965426192,6.59863075131265,37.4226946144693));
#68676=CARTESIAN_POINT('Ctrl Pts',(33.4246193974437,5.25132148728276,37.6602615890763));
#68677=CARTESIAN_POINT('Ctrl Pts',(35.,7.1693658572013,38.9456055698919));
#68678=CARTESIAN_POINT('Ctrl Pts',(34.1981589442516,7.56742453339927,38.0570140694253));
#68679=CARTESIAN_POINT('Ctrl Pts',(33.4246193974437,7.94594001540395,37.1851276398516));
#68680=CARTESIAN_POINT('Origin',(34.2,0.,0.));
#68681=CARTESIAN_POINT('',(35.,13.2639498235848,37.3125667178958));
#68682=CARTESIAN_POINT('',(35.,13.8232805156997,37.1089869948545));
#68683=CARTESIAN_POINT('Origin',(35.,0.,0.));
#68684=CARTESIAN_POINT('',(33.4246193974437,11.7111779096386,36.1762351867803));
#68685=CARTESIAN_POINT('Ctrl Pts',(33.4246193974437,11.7111779096386,36.1762351867803));
#68686=CARTESIAN_POINT('Ctrl Pts',(34.1981589442503,12.4749251475659,36.7420532430028));
#68687=CARTESIAN_POINT('Ctrl Pts',(35.,13.2639498235848,37.3125667178958));
#68688=CARTESIAN_POINT('',(33.4246193974437,14.2823529831122,35.2404039929487));
#68689=CARTESIAN_POINT('Ctrl Pts',(33.4246193974437,14.2823529831122,35.2404039929487));
#68690=CARTESIAN_POINT('Ctrl Pts',(33.3753965426192,12.9967654463461,35.7083195898752));
#68691=CARTESIAN_POINT('Ctrl Pts',(33.4246193974437,11.7111779096386,36.1762351867803));
#68692=CARTESIAN_POINT('Ctrl Pts',(35.,13.8232805156996,37.1089869948545));
#68693=CARTESIAN_POINT('Ctrl Pts',(34.1981589442506,14.0609894914271,36.1647730322067));
#68694=CARTESIAN_POINT('Ctrl Pts',(33.4246193974437,14.2823529831122,35.2404039929487));
#68695=CARTESIAN_POINT('Origin',(34.2,0.,0.));
#68696=CARTESIAN_POINT('',(35.,19.5416998364696,34.4424442730379));
#68697=CARTESIAN_POINT('',(35.,20.0571817906459,34.1448306280319));
#68698=CARTESIAN_POINT('Origin',(35.,0.,0.));
#68699=CARTESIAN_POINT('',(33.4246193974437,17.8151961173521,33.5930121843923));
#68700=CARTESIAN_POINT('Ctrl Pts',(33.4246193974437,17.8151961173521,33.5930121843923));
#68701=CARTESIAN_POINT('Ctrl Pts',(34.1981589442516,18.6655935929601,34.017610876891));
#68702=CARTESIAN_POINT('Ctrl Pts',(35.,19.5416998364696,34.4424442730379));
#68703=CARTESIAN_POINT('',(33.4246193974437,20.1848038826479,32.224918503225));
#68704=CARTESIAN_POINT('Ctrl Pts',(33.4246193974437,20.1848038826479,32.224918503225));
#68705=CARTESIAN_POINT('Ctrl Pts',(33.3753965426192,18.999999999973,32.9089653438243));
#68706=CARTESIAN_POINT('Ctrl Pts',(33.4246193974437,17.8151961173521,33.5930121843923));
#68707=CARTESIAN_POINT('Ctrl Pts',(35.,20.0571817906459,34.1448306280319));
#68708=CARTESIAN_POINT('Ctrl Pts',(34.1981589442511,20.1273183989614,33.1736836666644));
#68709=CARTESIAN_POINT('Ctrl Pts',(33.4246193974437,20.1848038826479,32.224918503225));
#68710=CARTESIAN_POINT('Origin',(34.2,0.,0.));
#68711=CARTESIAN_POINT('',(35.,25.2256851884005,30.5258055876616));
#68712=CARTESIAN_POINT('',(35.,25.6816557463071,30.1432008606945));
#68713=CARTESIAN_POINT('Origin',(35.,0.,0.));
#68714=CARTESIAN_POINT('',(33.4246193974437,23.3779086059641,29.989082505666));
#68715=CARTESIAN_POINT('Ctrl Pts',(33.4246193974437,23.3779086059641,29.989082505666));
#68716=CARTESIAN_POINT('Ctrl Pts',(34.1981589442514,24.2891174222768,30.2595606180256));
#68717=CARTESIAN_POINT('Ctrl Pts',(35.,25.2256851884005,30.5258055876616));
#68718=CARTESIAN_POINT('',(33.4246193974437,25.4739497302129,28.2302951713764));
#68719=CARTESIAN_POINT('Ctrl Pts',(33.4246193974437,25.4739497302129,28.2302951713764));
#68720=CARTESIAN_POINT('Ctrl Pts',(33.3753965426192,24.4259291680646,29.1096888385412));
#68721=CARTESIAN_POINT('Ctrl Pts',(33.4246193974437,23.3779086059641,29.989082505666));
#68722=CARTESIAN_POINT('Ctrl Pts',(35.,25.6816557463071,30.1432008606945));
#68723=CARTESIAN_POINT('Ctrl Pts',(34.1981589442496,25.5820889218578,29.174628709602));
#68724=CARTESIAN_POINT('Ctrl Pts',(33.4246193974437,25.4739497302129,28.2302951713764));
#68725=CARTESIAN_POINT('Origin',(34.2,0.,0.));
#68726=CARTESIAN_POINT('',(35.,30.1432008606945,25.6816557463071));
#68727=CARTESIAN_POINT('',(35.,30.5258055876616,25.2256851884005));
#68728=CARTESIAN_POINT('Origin',(35.,0.,0.));
#68729=CARTESIAN_POINT('',(33.4246193974437,28.2302951713764,25.4739497302129));
#68730=CARTESIAN_POINT('Ctrl Pts',(33.4246193974437,28.2302951713764,25.4739497302129));
#68731=CARTESIAN_POINT('Ctrl Pts',(34.1981589442485,29.1746287096007,25.5820889218576));
#68732=CARTESIAN_POINT('Ctrl Pts',(35.,30.1432008606945,25.6816557463071));
#68733=CARTESIAN_POINT('',(33.4246193974437,29.989082505666,23.3779086059641));
#68734=CARTESIAN_POINT('Ctrl Pts',(33.4246193974437,29.989082505666,23.3779086059641));
#68735=CARTESIAN_POINT('Ctrl Pts',(33.3753965426192,29.1096888385011,24.4259291681124));
#68736=CARTESIAN_POINT('Ctrl Pts',(33.4246193974437,28.2302951713764,25.4739497302129));
#68737=CARTESIAN_POINT('Ctrl Pts',(35.,30.5258055876616,25.2256851884005));
#68738=CARTESIAN_POINT('Ctrl Pts',(34.1981589442495,30.2595606180249,24.2891174222746));
#68739=CARTESIAN_POINT('Ctrl Pts',(33.4246193974437,29.989082505666,23.3779086059641));
#68740=CARTESIAN_POINT('Origin',(34.2,0.,0.));
#68741=CARTESIAN_POINT('',(35.,34.1448306280319,20.0571817906459));
#68742=CARTESIAN_POINT('',(35.,34.4424442730379,19.5416998364696));
#68743=CARTESIAN_POINT('Origin',(35.,0.,0.));
#68744=CARTESIAN_POINT('',(33.4246193974437,32.224918503225,20.1848038826479));
#68745=CARTESIAN_POINT('Ctrl Pts',(33.4246193974437,32.224918503225,20.1848038826479));
#68746=CARTESIAN_POINT('Ctrl Pts',(34.1981589442511,33.1736836666644,20.1273183989614));
#68747=CARTESIAN_POINT('Ctrl Pts',(35.,34.1448306280319,20.0571817906459));
#68748=CARTESIAN_POINT('',(33.4246193974437,33.5930121843923,17.8151961173521));
#68749=CARTESIAN_POINT('Ctrl Pts',(33.4246193974437,33.5930121843923,17.8151961173521));
#68750=CARTESIAN_POINT('Ctrl Pts',(33.3753965426192,32.9089653437931,19.000000000027));
#68751=CARTESIAN_POINT('Ctrl Pts',(33.4246193974437,32.224918503225,20.1848038826479));
#68752=CARTESIAN_POINT('Ctrl Pts',(35.,34.4424442730379,19.5416998364696));
#68753=CARTESIAN_POINT('Ctrl Pts',(34.1981589442499,34.0176108768901,18.6655935929583));
#68754=CARTESIAN_POINT('Ctrl Pts',(33.4246193974437,33.5930121843923,17.8151961173521));
#68755=CARTESIAN_POINT('Origin',(34.2,0.,0.));
#68756=CARTESIAN_POINT('',(35.,37.1089869948545,13.8232805156996));
#68757=CARTESIAN_POINT('',(35.,37.3125667178958,13.2639498235848));
#68758=CARTESIAN_POINT('Origin',(35.,0.,0.));
#68759=CARTESIAN_POINT('',(33.4246193974437,35.2404039929487,14.2823529831122));
#68760=CARTESIAN_POINT('Ctrl Pts',(33.4246193974437,35.2404039929487,14.2823529831122));
#68761=CARTESIAN_POINT('Ctrl Pts',(34.1981589442501,36.1647730322061,14.0609894914273));
#68762=CARTESIAN_POINT('Ctrl Pts',(35.,37.1089869948545,13.8232805156996));
#68763=CARTESIAN_POINT('',(33.4246193974437,36.1762351867803,11.7111779096386));
#68764=CARTESIAN_POINT('Ctrl Pts',(33.4246193974437,36.1762351867803,11.7111779096386));
#68765=CARTESIAN_POINT('Ctrl Pts',(33.3753965426191,35.7083195898539,12.9967654464047));
#68766=CARTESIAN_POINT('Ctrl Pts',(33.4246193974437,35.2404039929487,14.2823529831122));
#68767=CARTESIAN_POINT('Ctrl Pts',(35.,37.3125667178958,13.2639498235848));
#68768=CARTESIAN_POINT('Ctrl Pts',(34.1981589442503,36.7420532430028,12.474925147566));
#68769=CARTESIAN_POINT('Ctrl Pts',(33.4246193974437,36.1762351867803,11.7111779096386));
#68770=CARTESIAN_POINT('Origin',(34.2,0.,0.));
#68771=CARTESIAN_POINT('',(35.,38.9456055698919,7.16936585720129));
#68772=CARTESIAN_POINT('',(35.,39.0489657041002,6.5831814071929));
#68773=CARTESIAN_POINT('Origin',(35.,0.,0.));
#68774=CARTESIAN_POINT('',(33.4246193974437,37.1851276398516,7.94594001540395));
#68775=CARTESIAN_POINT('Ctrl Pts',(33.4246193974437,37.1851276398516,7.94594001540395));
#68776=CARTESIAN_POINT('Ctrl Pts',(34.1981589442508,38.0570140694243,7.56742453339971));
#68777=CARTESIAN_POINT('Ctrl Pts',(35.,38.9456055698919,7.16936585720129));
#68778=CARTESIAN_POINT('',(33.4246193974437,37.6602615890763,5.25132148728275));
#68779=CARTESIAN_POINT('Ctrl Pts',(33.4246193974437,37.6602615890763,5.25132148728275));
#68780=CARTESIAN_POINT('Ctrl Pts',(33.3753965426192,37.4226946144585,6.59863075137406));
#68781=CARTESIAN_POINT('Ctrl Pts',(33.4246193974437,37.1851276398516,7.94594001540395));
#68782=CARTESIAN_POINT('Ctrl Pts',(35.,39.0489657041001,6.5831814071929));
#68783=CARTESIAN_POINT('Ctrl Pts',(34.1981589442489,38.3501069137015,5.90521241418));
#68784=CARTESIAN_POINT('Ctrl Pts',(33.4246193974437,37.6602615890763,5.25132148728275));
#68785=CARTESIAN_POINT('Origin',(34.2,0.,0.));
#68786=CARTESIAN_POINT('',(35.,39.5988816271155,0.297613645006066));
#68787=CARTESIAN_POINT('',(35.,39.5988816271155,-0.297613645006066));
#68788=CARTESIAN_POINT('Origin',(35.,0.,0.));
#68789=CARTESIAN_POINT('',(33.4246193974437,38.,1.36809368116734));
#68790=CARTESIAN_POINT('Ctrl Pts',(33.4246193974437,38.,1.36809368116734));
#68791=CARTESIAN_POINT('Ctrl Pts',(34.1981589442493,38.7929119919191,0.84392721022757));
#68792=CARTESIAN_POINT('Ctrl Pts',(35.,39.5988816271155,0.297613645006068));
#68793=CARTESIAN_POINT('',(33.4246193974437,38.,-1.36809368116733));
#68794=CARTESIAN_POINT('Ctrl Pts',(33.4246193974437,38.,-1.36809368116733));
#68795=CARTESIAN_POINT('Ctrl Pts',(33.3753965426191,38.,3.11825565368906E-11));
#68796=CARTESIAN_POINT('Ctrl Pts',(33.4246193974437,38.,1.36809368116734));
#68797=CARTESIAN_POINT('Ctrl Pts',(35.,39.5988816271155,-0.297613645006068));
#68798=CARTESIAN_POINT('Ctrl Pts',(34.1981589442501,38.7929119919199,-0.84392721022704));
#68799=CARTESIAN_POINT('Ctrl Pts',(33.4246193974437,38.,-1.36809368116733));
#68800=CARTESIAN_POINT('Origin',(17.5,38.,0.));
#68801=CARTESIAN_POINT('',(33.1,38.,1.65));
#68802=CARTESIAN_POINT('',(33.1,38.,1.65));
#68803=CARTESIAN_POINT('',(30.5,38.,1.65));
#68804=CARTESIAN_POINT('',(30.5,38.,1.65));
#68805=CARTESIAN_POINT('',(30.5,38.,1.15));
#68806=CARTESIAN_POINT('',(30.5,38.,1.15));
#68807=CARTESIAN_POINT('',(24.1,38.,0.75));
#68808=CARTESIAN_POINT('',(24.1,38.,0.75));
#68809=CARTESIAN_POINT('',(23.1,38.,1.05));
#68810=CARTESIAN_POINT('',(23.1,38.,1.05));
#68811=CARTESIAN_POINT('',(22.4,38.,1.45));
#68812=CARTESIAN_POINT('',(22.4,38.,1.45));
#68813=CARTESIAN_POINT('',(21.8,38.,1.65));
#68814=CARTESIAN_POINT('',(21.8,38.,1.65));
#68815=CARTESIAN_POINT('',(13.2,38.,1.65));
#68816=CARTESIAN_POINT('',(13.2,38.,1.65));
#68817=CARTESIAN_POINT('',(12.6,38.,1.45));
#68818=CARTESIAN_POINT('',(12.6,38.,1.45));
#68819=CARTESIAN_POINT('',(11.9,38.,1.05));
#68820=CARTESIAN_POINT('',(11.9,38.,1.05));
#68821=CARTESIAN_POINT('',(10.9,38.,0.75));
#68822=CARTESIAN_POINT('',(10.9,38.,0.75));
#68823=CARTESIAN_POINT('',(4.5,38.,1.15));
#68824=CARTESIAN_POINT('',(4.5,38.,1.15));
#68825=CARTESIAN_POINT('',(4.5,38.,1.65));
#68826=CARTESIAN_POINT('',(4.5,38.,1.65));
#68827=CARTESIAN_POINT('',(1.9,38.,1.65));
#68828=CARTESIAN_POINT('',(1.9,38.,1.65));
#68829=CARTESIAN_POINT('',(1.57538060255633,38.,1.36809368116734));
#68830=CARTESIAN_POINT('',(0.,38.,0.));
#68831=CARTESIAN_POINT('',(1.57538060255632,38.,-1.36809368116733));
#68832=CARTESIAN_POINT('Ctrl Pts',(1.57538060255633,38.,1.36809368116734));
#68833=CARTESIAN_POINT('Ctrl Pts',(1.62460345738085,38.,-3.1172564529669E-11));
#68834=CARTESIAN_POINT('Ctrl Pts',(1.57538060255632,38.,-1.36809368116733));
#68835=CARTESIAN_POINT('',(1.9,38.,-1.65));
#68836=CARTESIAN_POINT('',(1.9,38.,-1.65));
#68837=CARTESIAN_POINT('',(4.5,38.,-1.65));
#68838=CARTESIAN_POINT('',(4.5,38.,-1.65));
#68839=CARTESIAN_POINT('',(4.5,38.,-1.15));
#68840=CARTESIAN_POINT('',(4.5,38.,-1.15));
#68841=CARTESIAN_POINT('',(10.9,38.,-0.75));
#68842=CARTESIAN_POINT('',(10.9,38.,-0.75));
#68843=CARTESIAN_POINT('',(11.9,38.,-1.05));
#68844=CARTESIAN_POINT('',(11.9,38.,-1.05));
#68845=CARTESIAN_POINT('',(12.6,38.,-1.45));
#68846=CARTESIAN_POINT('',(12.6,38.,-1.45));
#68847=CARTESIAN_POINT('',(13.2,38.,-1.65));
#68848=CARTESIAN_POINT('',(13.2,38.,-1.65));
#68849=CARTESIAN_POINT('',(21.8,38.,-1.65));
#68850=CARTESIAN_POINT('',(21.8,38.,-1.65));
#68851=CARTESIAN_POINT('',(22.4,38.,-1.45));
#68852=CARTESIAN_POINT('',(22.4,38.,-1.45));
#68853=CARTESIAN_POINT('',(23.1,38.,-1.05));
#68854=CARTESIAN_POINT('',(23.1,38.,-1.05));
#68855=CARTESIAN_POINT('',(24.1,38.,-0.75));
#68856=CARTESIAN_POINT('',(24.1,38.,-0.75));
#68857=CARTESIAN_POINT('',(30.5,38.,-1.15));
#68858=CARTESIAN_POINT('',(30.5,38.,-1.15));
#68859=CARTESIAN_POINT('',(30.5,38.,-1.65));
#68860=CARTESIAN_POINT('',(30.5,38.,-1.65));
#68861=CARTESIAN_POINT('',(33.1,38.,-1.65));
#68862=CARTESIAN_POINT('',(33.1,38.,-1.65));
#68863=CARTESIAN_POINT('',(35.,38.,0.));
#68864=CARTESIAN_POINT('Origin',(35.,38.,0.));
#68865=CARTESIAN_POINT('',(35.,42.75,0.884158520433536));
#68866=CARTESIAN_POINT('',(35.,44.7655886465086,1.25933744159137));
#68867=CARTESIAN_POINT('',(34.8617922858584,42.75,1.00418100903022));
#68868=CARTESIAN_POINT('',(33.5377160618333,42.75,2.15403667726254));
#68869=CARTESIAN_POINT('',(34.4,42.2794732300362,1.31762794090604));
#68870=CARTESIAN_POINT('Ctrl Pts',(34.4,42.2794732300361,1.31762794090604));
#68871=CARTESIAN_POINT('Ctrl Pts',(34.6297825291038,42.5142243943581,1.16177621660371));
#68872=CARTESIAN_POINT('Ctrl Pts',(34.8617922858584,42.75,1.00418100903022));
#68873=CARTESIAN_POINT('',(33.322645308031,42.240333256585,2.24593997529677));
#68874=CARTESIAN_POINT('Origin',(26.8550245390365,0.,0.));
#68875=CARTESIAN_POINT('',(33.0966075166785,37.9353893420094,1.64091956419534));
#68876=CARTESIAN_POINT('Origin',(17.5,37.4226946144639,6.59863075134335));
#68877=CARTESIAN_POINT('',(33.1,37.1361751213135,8.2235635438135));
#68878=CARTESIAN_POINT('',(33.1,37.1361751213135,8.2235635438135));
#68879=CARTESIAN_POINT('',(30.5,37.1361751213135,8.2235635438135));
#68880=CARTESIAN_POINT('',(30.5,37.1361751213135,8.2235635438135));
#68881=CARTESIAN_POINT('',(30.5,37.2229992101469,7.73115966730739));
#68882=CARTESIAN_POINT('',(30.5,37.2229992101469,7.73115966730739));
#68883=CARTESIAN_POINT('',(24.1,37.2924584812137,7.33723656610251));
#68884=CARTESIAN_POINT('',(24.1,37.2924584812137,7.33723656610251));
#68885=CARTESIAN_POINT('',(23.1,37.2403640279136,7.63267889200617));
#68886=CARTESIAN_POINT('',(23.1,37.2403640279136,7.63267889200617));
#68887=CARTESIAN_POINT('',(22.4,37.1709047568469,8.02660199321105));
#68888=CARTESIAN_POINT('',(22.4,37.1709047568469,8.02660199321105));
#68889=CARTESIAN_POINT('',(21.8,37.1361751213135,8.2235635438135));
#68890=CARTESIAN_POINT('',(21.8,37.1361751213135,8.2235635438135));
#68891=CARTESIAN_POINT('',(13.2,37.1361751213135,8.2235635438135));
#68892=CARTESIAN_POINT('',(13.2,37.1361751213135,8.2235635438135));
#68893=CARTESIAN_POINT('',(12.6,37.1709047568469,8.02660199321105));
#68894=CARTESIAN_POINT('',(12.6,37.1709047568469,8.02660199321105));
#68895=CARTESIAN_POINT('',(11.9,37.2403640279136,7.63267889200617));
#68896=CARTESIAN_POINT('',(11.9,37.2403640279136,7.63267889200617));
#68897=CARTESIAN_POINT('',(10.9,37.2924584812137,7.33723656610251));
#68898=CARTESIAN_POINT('',(10.9,37.2924584812137,7.33723656610251));
#68899=CARTESIAN_POINT('',(4.5,37.2229992101469,7.73115966730739));
#68900=CARTESIAN_POINT('',(4.5,37.2229992101469,7.73115966730739));
#68901=CARTESIAN_POINT('',(4.5,37.1361751213135,8.2235635438135));
#68902=CARTESIAN_POINT('',(4.5,37.1361751213135,8.2235635438135));
#68903=CARTESIAN_POINT('',(1.9,37.1361751213135,8.2235635438135));
#68904=CARTESIAN_POINT('',(1.9,37.1361751213135,8.2235635438135));
#68905=CARTESIAN_POINT('',(1.57538060255632,37.1851276398516,7.94594001540396));
#68906=CARTESIAN_POINT('',(0.,37.4226946144639,6.59863075134335));
#68907=CARTESIAN_POINT('',(1.57538060255632,37.6602615890763,5.25132148728275));
#68908=CARTESIAN_POINT('Ctrl Pts',(1.57538060255632,37.1851276398516,7.94594001540396));
#68909=CARTESIAN_POINT('Ctrl Pts',(1.62460345738085,37.4226946144693,6.59863075131265));
#68910=CARTESIAN_POINT('Ctrl Pts',(1.57538060255632,37.6602615890763,5.25132148728275));
#68911=CARTESIAN_POINT('',(1.9,37.7092141076143,4.97369795887321));
#68912=CARTESIAN_POINT('',(1.9,37.7092141076143,4.97369795887321));
#68913=CARTESIAN_POINT('',(4.5,37.7092141076143,4.97369795887321));
#68914=CARTESIAN_POINT('',(4.5,37.7092141076143,4.97369795887321));
#68915=CARTESIAN_POINT('',(4.5,37.6223900187809,5.46610183537931));
#68916=CARTESIAN_POINT('',(4.5,37.6223900187809,5.46610183537931));
#68917=CARTESIAN_POINT('',(10.9,37.5529307477141,5.8600249365842));
#68918=CARTESIAN_POINT('',(10.9,37.5529307477141,5.8600249365842));
#68919=CARTESIAN_POINT('',(11.9,37.6050252010142,5.56458261068053));
#68920=CARTESIAN_POINT('',(11.9,37.6050252010142,5.56458261068053));
#68921=CARTESIAN_POINT('',(12.6,37.674484472081,5.17065950947565));
#68922=CARTESIAN_POINT('',(12.6,37.674484472081,5.17065950947565));
#68923=CARTESIAN_POINT('',(13.2,37.7092141076143,4.97369795887321));
#68924=CARTESIAN_POINT('',(13.2,37.7092141076143,4.97369795887321));
#68925=CARTESIAN_POINT('',(21.8,37.7092141076143,4.97369795887321));
#68926=CARTESIAN_POINT('',(21.8,37.7092141076143,4.97369795887321));
#68927=CARTESIAN_POINT('',(22.4,37.674484472081,5.17065950947565));
#68928=CARTESIAN_POINT('',(22.4,37.674484472081,5.17065950947565));
#68929=CARTESIAN_POINT('',(23.1,37.6050252010142,5.56458261068053));
#68930=CARTESIAN_POINT('',(23.1,37.6050252010142,5.56458261068053));
#68931=CARTESIAN_POINT('',(24.1,37.5529307477141,5.8600249365842));
#68932=CARTESIAN_POINT('',(24.1,37.5529307477141,5.8600249365842));
#68933=CARTESIAN_POINT('',(30.5,37.6223900187809,5.46610183537931));
#68934=CARTESIAN_POINT('',(30.5,37.6223900187809,5.46610183537931));
#68935=CARTESIAN_POINT('',(30.5,37.7092141076143,4.97369795887321));
#68936=CARTESIAN_POINT('',(30.5,37.7092141076143,4.97369795887321));
#68937=CARTESIAN_POINT('',(33.1,37.7092141076143,4.97369795887321));
#68938=CARTESIAN_POINT('',(33.1,37.7092141076143,4.97369795887321));
#68939=CARTESIAN_POINT('',(35.,37.4226946144639,6.59863075134335));
#68940=CARTESIAN_POINT('Origin',(35.,37.4226946144639,6.59863075134335));
#68941=CARTESIAN_POINT('',(35.,41.9469989254299,8.29418576107602));
#68942=CARTESIAN_POINT('',(35.,42.7295335855124,8.58745307290921));
#68943=CARTESIAN_POINT('',(34.8617922858584,41.9261572390061,8.41238483838185));
#68944=CARTESIAN_POINT('',(33.5377160618333,41.7264868976375,9.54477161530208));
#68945=CARTESIAN_POINT('',(34.4,41.4083493394303,8.63936369090333));
#68946=CARTESIAN_POINT('Ctrl Pts',(34.4,41.4083493394303,8.63936369090333));
#68947=CARTESIAN_POINT('Ctrl Pts',(34.6297825291033,41.6665974739941,8.52664381637996));
#68948=CARTESIAN_POINT('Ctrl Pts',(34.8617922858584,41.9261572390061,8.41238483838185));
#68949=CARTESIAN_POINT('',(33.3226453080309,41.2086042970448,9.54677599452213));
#68950=CARTESIAN_POINT('Origin',(26.8550245390365,0.,0.));
#68951=CARTESIAN_POINT('',(33.0966075166785,37.0741228455271,8.20340153721441));
#68952=CARTESIAN_POINT('Origin',(17.5,35.7083195898645,12.9967654463754));
#68953=CARTESIAN_POINT('',(33.1,35.1439863533772,14.5472582706722));
#68954=CARTESIAN_POINT('',(33.1,35.1439863533772,14.5472582706722));
#68955=CARTESIAN_POINT('',(30.5,35.1439863533772,14.5472582706722));
#68956=CARTESIAN_POINT('',(30.5,35.1439863533772,14.5472582706722));
#68957=CARTESIAN_POINT('',(30.5,35.31499642504,14.0774119602792));
#68958=CARTESIAN_POINT('',(30.5,35.31499642504,14.0774119602792));
#68959=CARTESIAN_POINT('',(24.1,35.4518044823703,13.7015349119648));
#68960=CARTESIAN_POINT('',(24.1,35.4518044823703,13.7015349119648));
#68961=CARTESIAN_POINT('',(23.1,35.3491984393726,13.9834426982006));
#68962=CARTESIAN_POINT('',(23.1,35.3491984393726,13.9834426982006));
#68963=CARTESIAN_POINT('',(22.4,35.2123903820423,14.359319746515));
#68964=CARTESIAN_POINT('',(22.4,35.2123903820423,14.359319746515));
#68965=CARTESIAN_POINT('',(21.8,35.1439863533772,14.5472582706722));
#68966=CARTESIAN_POINT('',(21.8,35.1439863533772,14.5472582706722));
#68967=CARTESIAN_POINT('',(13.2,35.1439863533772,14.5472582706722));
#68968=CARTESIAN_POINT('',(13.2,35.1439863533772,14.5472582706722));
#68969=CARTESIAN_POINT('',(12.6,35.2123903820423,14.359319746515));
#68970=CARTESIAN_POINT('',(12.6,35.2123903820423,14.359319746515));
#68971=CARTESIAN_POINT('',(11.9,35.3491984393726,13.9834426982006));
#68972=CARTESIAN_POINT('',(11.9,35.3491984393726,13.9834426982006));
#68973=CARTESIAN_POINT('',(10.9,35.4518044823703,13.7015349119648));
#68974=CARTESIAN_POINT('',(10.9,35.4518044823703,13.7015349119648));
#68975=CARTESIAN_POINT('',(4.5,35.31499642504,14.0774119602792));
#68976=CARTESIAN_POINT('',(4.5,35.31499642504,14.0774119602792));
#68977=CARTESIAN_POINT('',(4.5,35.1439863533772,14.5472582706722));
#68978=CARTESIAN_POINT('',(4.5,35.1439863533772,14.5472582706722));
#68979=CARTESIAN_POINT('',(1.9,35.1439863533772,14.5472582706722));
#68980=CARTESIAN_POINT('',(1.9,35.1439863533772,14.5472582706722));
#68981=CARTESIAN_POINT('',(1.57538060255633,35.2404039929487,14.2823529831122));
#68982=CARTESIAN_POINT('',(0.,35.7083195898645,12.9967654463754));
#68983=CARTESIAN_POINT('',(1.57538060255632,36.1762351867803,11.7111779096386));
#68984=CARTESIAN_POINT('Ctrl Pts',(1.57538060255633,35.2404039929487,14.2823529831122));
#68985=CARTESIAN_POINT('Ctrl Pts',(1.62460345738085,35.7083195898752,12.9967654463461));
#68986=CARTESIAN_POINT('Ctrl Pts',(1.57538060255632,36.1762351867803,11.7111779096386));
#68987=CARTESIAN_POINT('',(1.9,36.2726528263519,11.4462726220787));
#68988=CARTESIAN_POINT('',(1.9,36.2726528263519,11.4462726220787));
#68989=CARTESIAN_POINT('',(4.5,36.2726528263519,11.4462726220787));
#68990=CARTESIAN_POINT('',(4.5,36.2726528263519,11.4462726220787));
#68991=CARTESIAN_POINT('',(4.5,36.101642754689,11.9161189324716));
#68992=CARTESIAN_POINT('',(4.5,36.101642754689,11.9161189324716));
#68993=CARTESIAN_POINT('',(10.9,35.9648346973588,12.291995980786));
#68994=CARTESIAN_POINT('',(10.9,35.9648346973588,12.291995980786));
#68995=CARTESIAN_POINT('',(11.9,36.0674407403565,12.0100881945502));
#68996=CARTESIAN_POINT('',(11.9,36.0674407403565,12.0100881945502));
#68997=CARTESIAN_POINT('',(12.6,36.2042487976867,11.6342111462358));
#68998=CARTESIAN_POINT('',(12.6,36.2042487976867,11.6342111462358));
#68999=CARTESIAN_POINT('',(13.2,36.2726528263519,11.4462726220787));
#69000=CARTESIAN_POINT('',(13.2,36.2726528263519,11.4462726220787));
#69001=CARTESIAN_POINT('',(21.8,36.2726528263519,11.4462726220787));
#69002=CARTESIAN_POINT('',(21.8,36.2726528263519,11.4462726220787));
#69003=CARTESIAN_POINT('',(22.4,36.2042487976867,11.6342111462358));
#69004=CARTESIAN_POINT('',(22.4,36.2042487976867,11.6342111462358));
#69005=CARTESIAN_POINT('',(23.1,36.0674407403565,12.0100881945502));
#69006=CARTESIAN_POINT('',(23.1,36.0674407403565,12.0100881945502));
#69007=CARTESIAN_POINT('',(24.1,35.9648346973588,12.291995980786));
#69008=CARTESIAN_POINT('',(24.1,35.9648346973588,12.291995980786));
#69009=CARTESIAN_POINT('',(30.5,36.101642754689,11.9161189324716));
#69010=CARTESIAN_POINT('',(30.5,36.101642754689,11.9161189324716));
#69011=CARTESIAN_POINT('',(30.5,36.2726528263519,11.4462726220787));
#69012=CARTESIAN_POINT('',(30.5,36.2726528263519,11.4462726220787));
#69013=CARTESIAN_POINT('',(33.1,36.2726528263519,11.4462726220787));
#69014=CARTESIAN_POINT('',(33.1,36.2726528263519,11.4462726220787));
#69015=CARTESIAN_POINT('',(35.,35.7083195898645,12.9967654463754));
#69016=CARTESIAN_POINT('Origin',(35.,35.7083195898645,12.9967654463754));
#69017=CARTESIAN_POINT('',(35.,39.8694595147163,15.4521983644287));
#69018=CARTESIAN_POINT('',(35.,38.9060829772051,14.8837227771125));
#69019=CARTESIAN_POINT('',(34.8617922858584,39.8284094059642,15.5649826112914));
#69020=CARTESIAN_POINT('',(33.5377160618333,39.4351356055115,16.6454934976981));
#69021=CARTESIAN_POINT('',(34.4,39.2790537077817,15.6985967468815));
#69022=CARTESIAN_POINT('Ctrl Pts',(34.4,39.2790537077817,15.6985967468815));
#69023=CARTESIAN_POINT('Ctrl Pts',(34.6297825290998,39.5529520736946,15.6324336584862));
#69024=CARTESIAN_POINT('Ctrl Pts',(34.8617922858584,39.8284094059642,15.5649826112914));
#69025=CARTESIAN_POINT('',(33.3226453080309,38.9247727484987,16.5575380560557));
#69026=CARTESIAN_POINT('Origin',(26.8550245390365,0.,0.));
#69027=CARTESIAN_POINT('',(33.0966075166785,35.0863778867947,14.5166273056467));
#69028=CARTESIAN_POINT('Origin',(17.5,32.9089653438087,19.));
#69029=CARTESIAN_POINT('',(33.1,32.0839653438087,20.4289419162443));
#69030=CARTESIAN_POINT('',(33.1,32.0839653438087,20.4289419162443));
#69031=CARTESIAN_POINT('',(30.5,32.0839653438087,20.4289419162443));
#69032=CARTESIAN_POINT('',(30.5,32.0839653438087,20.4289419162443));
#69033=CARTESIAN_POINT('',(30.5,32.3339653438087,19.9959292143521));
#69034=CARTESIAN_POINT('',(30.5,32.3339653438087,19.9959292143521));
#69035=CARTESIAN_POINT('',(24.1,32.5339653438087,19.6495190528383));
#69036=CARTESIAN_POINT('',(24.1,32.5339653438087,19.6495190528383));
#69037=CARTESIAN_POINT('',(23.1,32.3839653438087,19.9093266739737));
#69038=CARTESIAN_POINT('',(23.1,32.3839653438087,19.9093266739737));
#69039=CARTESIAN_POINT('',(22.4,32.1839653438087,20.2557368354874));
#69040=CARTESIAN_POINT('',(22.4,32.1839653438087,20.2557368354874));
#69041=CARTESIAN_POINT('',(21.8,32.0839653438087,20.4289419162443));
#69042=CARTESIAN_POINT('',(21.8,32.0839653438087,20.4289419162443));
#69043=CARTESIAN_POINT('',(13.2,32.0839653438087,20.4289419162443));
#69044=CARTESIAN_POINT('',(13.2,32.0839653438087,20.4289419162443));
#69045=CARTESIAN_POINT('',(12.6,32.1839653438087,20.2557368354874));
#69046=CARTESIAN_POINT('',(12.6,32.1839653438087,20.2557368354874));
#69047=CARTESIAN_POINT('',(11.9,32.3839653438087,19.9093266739737));
#69048=CARTESIAN_POINT('',(11.9,32.3839653438087,19.9093266739737));
#69049=CARTESIAN_POINT('',(10.9,32.5339653438087,19.6495190528383));
#69050=CARTESIAN_POINT('',(10.9,32.5339653438087,19.6495190528383));
#69051=CARTESIAN_POINT('',(4.5,32.3339653438087,19.9959292143521));
#69052=CARTESIAN_POINT('',(4.5,32.3339653438087,19.9959292143521));
#69053=CARTESIAN_POINT('',(4.5,32.0839653438087,20.4289419162443));
#69054=CARTESIAN_POINT('',(4.5,32.0839653438087,20.4289419162443));
#69055=CARTESIAN_POINT('',(1.9,32.0839653438087,20.4289419162443));
#69056=CARTESIAN_POINT('',(1.9,32.0839653438087,20.4289419162443));
#69057=CARTESIAN_POINT('',(1.57538060255632,32.224918503225,20.1848038826479));
#69058=CARTESIAN_POINT('',(0.,32.9089653438087,19.));
#69059=CARTESIAN_POINT('',(1.57538060255632,33.5930121843923,17.8151961173521));
#69060=CARTESIAN_POINT('Ctrl Pts',(1.57538060255632,32.224918503225,20.1848038826479));
#69061=CARTESIAN_POINT('Ctrl Pts',(1.62460345738085,32.9089653438243,18.999999999973));
#69062=CARTESIAN_POINT('Ctrl Pts',(1.57538060255632,33.5930121843923,17.8151961173521));
#69063=CARTESIAN_POINT('',(1.9,33.7339653438087,17.5710580837557));
#69064=CARTESIAN_POINT('',(1.9,33.7339653438087,17.5710580837557));
#69065=CARTESIAN_POINT('',(4.5,33.7339653438087,17.5710580837557));
#69066=CARTESIAN_POINT('',(4.5,33.7339653438087,17.5710580837557));
#69067=CARTESIAN_POINT('',(4.5,33.4839653438087,18.0040707856479));
#69068=CARTESIAN_POINT('',(4.5,33.4839653438087,18.0040707856479));
#69069=CARTESIAN_POINT('',(10.9,33.2839653438087,18.3504809471617));
#69070=CARTESIAN_POINT('',(10.9,33.2839653438087,18.3504809471617));
#69071=CARTESIAN_POINT('',(11.9,33.4339653438087,18.0906733260263));
#69072=CARTESIAN_POINT('',(11.9,33.4339653438087,18.0906733260263));
#69073=CARTESIAN_POINT('',(12.6,33.6339653438087,17.7442631645126));
#69074=CARTESIAN_POINT('',(12.6,33.6339653438087,17.7442631645126));
#69075=CARTESIAN_POINT('',(13.2,33.7339653438087,17.5710580837557));
#69076=CARTESIAN_POINT('',(13.2,33.7339653438087,17.5710580837557));
#69077=CARTESIAN_POINT('',(21.8,33.7339653438087,17.5710580837557));
#69078=CARTESIAN_POINT('',(21.8,33.7339653438087,17.5710580837557));
#69079=CARTESIAN_POINT('',(22.4,33.6339653438087,17.7442631645126));
#69080=CARTESIAN_POINT('',(22.4,33.6339653438087,17.7442631645126));
#69081=CARTESIAN_POINT('',(23.1,33.4339653438087,18.0906733260263));
#69082=CARTESIAN_POINT('',(23.1,33.4339653438087,18.0906733260263));
#69083=CARTESIAN_POINT('',(24.1,33.2839653438087,18.3504809471617));
#69084=CARTESIAN_POINT('',(24.1,33.2839653438087,18.3504809471617));
#69085=CARTESIAN_POINT('',(30.5,33.4839653438087,18.0040707856479));
#69086=CARTESIAN_POINT('',(30.5,33.4839653438087,18.0040707856479));
#69087=CARTESIAN_POINT('',(30.5,33.7339653438087,17.5710580837557));
#69088=CARTESIAN_POINT('',(30.5,33.7339653438087,17.5710580837557));
#69089=CARTESIAN_POINT('',(33.1,33.7339653438087,17.5710580837557));
#69090=CARTESIAN_POINT('',(33.1,33.7339653438087,17.5710580837557));
#69091=CARTESIAN_POINT('',(35.,32.9089653438087,19.));
#69092=CARTESIAN_POINT('Origin',(35.,32.9089653438087,19.));
#69093=CARTESIAN_POINT('',(35.,36.580506751568,22.1407037396679));
#69094=CARTESIAN_POINT('',(35.,33.7283972474216,19.7009570527085));
#69095=CARTESIAN_POINT('',(34.8617922858584,36.5204955072696,22.244646263818));
#69096=CARTESIAN_POINT('',(33.5377160618333,35.9455676731535,23.2404504831928));
#69097=CARTESIAN_POINT('',(34.4,35.9562839053824,22.2808358845789));
#69098=CARTESIAN_POINT('Ctrl Pts',(34.4,35.9562839053824,22.2808358845789));
#69099=CARTESIAN_POINT('Ctrl Pts',(34.6297825291007,36.2375102394006,22.2632399142707));
#69100=CARTESIAN_POINT('Ctrl Pts',(34.8617922858584,36.5204955072696,22.244646263818));
#69101=CARTESIAN_POINT('',(33.322645308031,35.4582316768749,23.0652077022745));
#69102=CARTESIAN_POINT('Origin',(26.8550245390365,0.,0.));
#69103=CARTESIAN_POINT('',(33.0966075166785,32.0325510905359,20.3887726991648));
#69104=CARTESIAN_POINT('Origin',(17.5,29.1096888385212,24.4259291680885));
#69105=CARTESIAN_POINT('',(33.1,28.0490892825384,25.6899024992348));
#69106=CARTESIAN_POINT('',(33.1,28.0490892825384,25.6899024992348));
#69107=CARTESIAN_POINT('',(30.5,28.0490892825384,25.6899024992348));
#69108=CARTESIAN_POINT('',(30.5,28.0490892825384,25.6899024992348));
#69109=CARTESIAN_POINT('',(30.5,28.3704830873816,25.3068802776753));
#69110=CARTESIAN_POINT('',(30.5,28.3704830873816,25.3068802776753));
#69111=CARTESIAN_POINT('',(24.1,28.6275981312563,25.0004625004277));
#69112=CARTESIAN_POINT('',(24.1,28.6275981312563,25.0004625004277));
#69113=CARTESIAN_POINT('',(23.1,28.4347618483503,25.2302758333634));
#69114=CARTESIAN_POINT('',(23.1,28.4347618483503,25.2302758333634));
#69115=CARTESIAN_POINT('',(22.4,28.1776468044757,25.536693610611));
#69116=CARTESIAN_POINT('',(22.4,28.1776468044757,25.536693610611));
#69117=CARTESIAN_POINT('',(21.8,28.0490892825384,25.6899024992348));
#69118=CARTESIAN_POINT('',(21.8,28.0490892825384,25.6899024992348));
#69119=CARTESIAN_POINT('',(13.2,28.0490892825384,25.6899024992348));
#69120=CARTESIAN_POINT('',(13.2,28.0490892825384,25.6899024992348));
#69121=CARTESIAN_POINT('',(12.6,28.1776468044757,25.536693610611));
#69122=CARTESIAN_POINT('',(12.6,28.1776468044757,25.536693610611));
#69123=CARTESIAN_POINT('',(11.9,28.4347618483503,25.2302758333634));
#69124=CARTESIAN_POINT('',(11.9,28.4347618483503,25.2302758333634));
#69125=CARTESIAN_POINT('',(10.9,28.6275981312563,25.0004625004277));
#69126=CARTESIAN_POINT('',(10.9,28.6275981312563,25.0004625004277));
#69127=CARTESIAN_POINT('',(4.5,28.3704830873816,25.3068802776753));
#69128=CARTESIAN_POINT('',(4.5,28.3704830873816,25.3068802776753));
#69129=CARTESIAN_POINT('',(4.5,28.0490892825384,25.6899024992348));
#69130=CARTESIAN_POINT('',(4.5,28.0490892825384,25.6899024992348));
#69131=CARTESIAN_POINT('',(1.9,28.0490892825384,25.6899024992348));
#69132=CARTESIAN_POINT('',(1.9,28.0490892825384,25.6899024992348));
#69133=CARTESIAN_POINT('',(1.57538060255632,28.2302951713764,25.4739497302129));
#69134=CARTESIAN_POINT('',(0.,29.1096888385212,24.4259291680885));
#69135=CARTESIAN_POINT('',(1.57538060255632,29.989082505666,23.3779086059641));
#69136=CARTESIAN_POINT('Ctrl Pts',(1.57538060255632,28.2302951713764,25.4739497302129));
#69137=CARTESIAN_POINT('Ctrl Pts',(1.62460345738085,29.1096888385412,24.4259291680646));
#69138=CARTESIAN_POINT('Ctrl Pts',(1.57538060255632,29.989082505666,23.3779086059641));
#69139=CARTESIAN_POINT('',(1.9,30.170288394504,23.1619558369422));
#69140=CARTESIAN_POINT('',(1.9,30.170288394504,23.1619558369422));
#69141=CARTESIAN_POINT('',(4.5,30.170288394504,23.1619558369422));
#69142=CARTESIAN_POINT('',(4.5,30.170288394504,23.1619558369422));
#69143=CARTESIAN_POINT('',(4.5,29.8488945896607,23.5449780585017));
#69144=CARTESIAN_POINT('',(4.5,29.8488945896607,23.5449780585017));
#69145=CARTESIAN_POINT('',(10.9,29.5917795457861,23.8513958357493));
#69146=CARTESIAN_POINT('',(10.9,29.5917795457861,23.8513958357493));
#69147=CARTESIAN_POINT('',(11.9,29.784615828692,23.6215825028136));
#69148=CARTESIAN_POINT('',(11.9,29.784615828692,23.6215825028136));
#69149=CARTESIAN_POINT('',(12.6,30.0417308725667,23.315164725566));
#69150=CARTESIAN_POINT('',(12.6,30.0417308725667,23.315164725566));
#69151=CARTESIAN_POINT('',(13.2,30.170288394504,23.1619558369422));
#69152=CARTESIAN_POINT('',(13.2,30.170288394504,23.1619558369422));
#69153=CARTESIAN_POINT('',(21.8,30.170288394504,23.1619558369422));
#69154=CARTESIAN_POINT('',(21.8,30.170288394504,23.1619558369422));
#69155=CARTESIAN_POINT('',(22.4,30.0417308725667,23.315164725566));
#69156=CARTESIAN_POINT('',(22.4,30.0417308725667,23.315164725566));
#69157=CARTESIAN_POINT('',(23.1,29.784615828692,23.6215825028136));
#69158=CARTESIAN_POINT('',(23.1,29.784615828692,23.6215825028136));
#69159=CARTESIAN_POINT('',(24.1,29.5917795457861,23.8513958357493));
#69160=CARTESIAN_POINT('',(24.1,29.5917795457861,23.8513958357493));
#69161=CARTESIAN_POINT('',(30.5,29.8488945896607,23.5449780585017));
#69162=CARTESIAN_POINT('',(30.5,29.8488945896607,23.5449780585017));
#69163=CARTESIAN_POINT('',(30.5,30.170288394504,23.1619558369422));
#69164=CARTESIAN_POINT('',(30.5,30.170288394504,23.1619558369422));
#69165=CARTESIAN_POINT('',(33.1,30.170288394504,23.1619558369422));
#69166=CARTESIAN_POINT('',(33.1,30.170288394504,23.1619558369422));
#69167=CARTESIAN_POINT('',(35.,29.1096888385212,24.4259291680885));
#69168=CARTESIAN_POINT('Origin',(35.,29.1096888385212,24.4259291680885));
#69169=CARTESIAN_POINT('',(35.,32.1800738014028,28.156475035514));
#69170=CARTESIAN_POINT('',(35.,27.7391842233302,22.7607535010967));
#69171=CARTESIAN_POINT('',(34.8617922858584,32.1029248328492,28.2484175959528));
#69172=CARTESIAN_POINT('',(33.5377160618333,31.3638118563816,29.129258140991));
#69173=CARTESIAN_POINT('',(34.4,31.5410006112756,28.1860830985703));
#69174=CARTESIAN_POINT('Ctrl Pts',(34.4,31.5410006112756,28.1860830985703));
#69175=CARTESIAN_POINT('Ctrl Pts',(34.6297825290998,31.8210099935452,28.2175888910031));
#69176=CARTESIAN_POINT('Ctrl Pts',(34.8617922858584,32.1029248328492,28.2484175959527));
#69177=CARTESIAN_POINT('',(33.3226453080309,30.9143101784803,28.872052684018));
#69178=CARTESIAN_POINT('Origin',(26.8550245390365,0.,0.));
#69179=CARTESIAN_POINT('',(33.0966075166785,28.0054314386442,25.6414155514355));
#69180=CARTESIAN_POINT('Origin',(17.5,24.4259291680885,29.1096888385212));
#69181=CARTESIAN_POINT('',(33.1,23.1619558369422,30.170288394504));
#69182=CARTESIAN_POINT('',(33.1,23.1619558369422,30.170288394504));
#69183=CARTESIAN_POINT('',(30.5,23.1619558369422,30.170288394504));
#69184=CARTESIAN_POINT('',(30.5,23.1619558369422,30.170288394504));
#69185=CARTESIAN_POINT('',(30.5,23.5449780585017,29.8488945896607));
#69186=CARTESIAN_POINT('',(30.5,23.5449780585017,29.8488945896607));
#69187=CARTESIAN_POINT('',(24.1,23.8513958357493,29.5917795457861));
#69188=CARTESIAN_POINT('',(24.1,23.8513958357493,29.5917795457861));
#69189=CARTESIAN_POINT('',(23.1,23.6215825028136,29.784615828692));
#69190=CARTESIAN_POINT('',(23.1,23.6215825028136,29.784615828692));
#69191=CARTESIAN_POINT('',(22.4,23.315164725566,30.0417308725666));
#69192=CARTESIAN_POINT('',(22.4,23.315164725566,30.0417308725666));
#69193=CARTESIAN_POINT('',(21.8,23.1619558369422,30.170288394504));
#69194=CARTESIAN_POINT('',(21.8,23.1619558369422,30.170288394504));
#69195=CARTESIAN_POINT('',(13.2,23.1619558369422,30.170288394504));
#69196=CARTESIAN_POINT('',(13.2,23.1619558369422,30.170288394504));
#69197=CARTESIAN_POINT('',(12.6,23.315164725566,30.0417308725666));
#69198=CARTESIAN_POINT('',(12.6,23.315164725566,30.0417308725666));
#69199=CARTESIAN_POINT('',(11.9,23.6215825028136,29.784615828692));
#69200=CARTESIAN_POINT('',(11.9,23.6215825028136,29.784615828692));
#69201=CARTESIAN_POINT('',(10.9,23.8513958357493,29.5917795457861));
#69202=CARTESIAN_POINT('',(10.9,23.8513958357493,29.5917795457861));
#69203=CARTESIAN_POINT('',(4.5,23.5449780585017,29.8488945896607));
#69204=CARTESIAN_POINT('',(4.5,23.5449780585017,29.8488945896607));
#69205=CARTESIAN_POINT('',(4.5,23.1619558369422,30.170288394504));
#69206=CARTESIAN_POINT('',(4.5,23.1619558369422,30.170288394504));
#69207=CARTESIAN_POINT('',(1.9,23.1619558369422,30.170288394504));
#69208=CARTESIAN_POINT('',(1.9,23.1619558369422,30.170288394504));
#69209=CARTESIAN_POINT('',(1.57538060255632,23.3779086059641,29.989082505666));
#69210=CARTESIAN_POINT('',(0.,24.4259291680885,29.1096888385212));
#69211=CARTESIAN_POINT('',(1.57538060255632,25.4739497302129,28.2302951713764));
#69212=CARTESIAN_POINT('Ctrl Pts',(1.57538060255632,23.3779086059641,29.989082505666));
#69213=CARTESIAN_POINT('Ctrl Pts',(1.62460345738085,24.4259291681124,29.1096888385011));
#69214=CARTESIAN_POINT('Ctrl Pts',(1.57538060255632,25.4739497302129,28.2302951713764));
#69215=CARTESIAN_POINT('',(1.9,25.6899024992348,28.0490892825384));
#69216=CARTESIAN_POINT('',(1.9,25.6899024992348,28.0490892825384));
#69217=CARTESIAN_POINT('',(4.5,25.6899024992348,28.0490892825384));
#69218=CARTESIAN_POINT('',(4.5,25.6899024992348,28.0490892825384));
#69219=CARTESIAN_POINT('',(4.5,25.3068802776753,28.3704830873816));
#69220=CARTESIAN_POINT('',(4.5,25.3068802776753,28.3704830873816));
#69221=CARTESIAN_POINT('',(10.9,25.0004625004277,28.6275981312563));
#69222=CARTESIAN_POINT('',(10.9,25.0004625004277,28.6275981312563));
#69223=CARTESIAN_POINT('',(11.9,25.2302758333634,28.4347618483503));
#69224=CARTESIAN_POINT('',(11.9,25.2302758333634,28.4347618483503));
#69225=CARTESIAN_POINT('',(12.6,25.536693610611,28.1776468044757));
#69226=CARTESIAN_POINT('',(12.6,25.536693610611,28.1776468044757));
#69227=CARTESIAN_POINT('',(13.2,25.6899024992348,28.0490892825384));
#69228=CARTESIAN_POINT('',(13.2,25.6899024992348,28.0490892825384));
#69229=CARTESIAN_POINT('',(21.8,25.6899024992348,28.0490892825384));
#69230=CARTESIAN_POINT('',(21.8,25.6899024992348,28.0490892825384));
#69231=CARTESIAN_POINT('',(22.4,25.536693610611,28.1776468044757));
#69232=CARTESIAN_POINT('',(22.4,25.536693610611,28.1776468044757));
#69233=CARTESIAN_POINT('',(23.1,25.2302758333634,28.4347618483503));
#69234=CARTESIAN_POINT('',(23.1,25.2302758333634,28.4347618483503));
#69235=CARTESIAN_POINT('',(24.1,25.0004625004277,28.6275981312563));
#69236=CARTESIAN_POINT('',(24.1,25.0004625004277,28.6275981312563));
#69237=CARTESIAN_POINT('',(30.5,25.3068802776753,28.3704830873816));
#69238=CARTESIAN_POINT('',(30.5,25.3068802776753,28.3704830873816));
#69239=CARTESIAN_POINT('',(30.5,25.6899024992348,28.0490892825384));
#69240=CARTESIAN_POINT('',(30.5,25.6899024992348,28.0490892825384));
#69241=CARTESIAN_POINT('',(33.1,25.6899024992348,28.0490892825384));
#69242=CARTESIAN_POINT('',(33.1,25.6899024992348,28.0490892825384));
#69243=CARTESIAN_POINT('',(35.,24.4259291680885,29.1096888385212));
#69244=CARTESIAN_POINT('Origin',(35.,24.4259291680885,29.1096888385212));
#69245=CARTESIAN_POINT('',(35.,26.8018655926851,33.3167260852698));
#69246=CARTESIAN_POINT('',(35.,21.5277259351931,23.97788109181));
#69247=CARTESIAN_POINT('',(34.8617922858584,26.7099230322463,33.3938750538235));
#69248=CARTESIAN_POINT('',(33.5377160618333,25.8290824872081,34.132988030291));
#69249=CARTESIAN_POINT('',(34.4,26.1673599741116,33.234910440458));
#69250=CARTESIAN_POINT('Ctrl Pts',(34.4,26.1673599741116,33.234910440458));
#69251=CARTESIAN_POINT('Ctrl Pts',(34.6297825291018,26.4376444612473,33.314560708072));
#69252=CARTESIAN_POINT('Ctrl Pts',(34.8617922858584,26.7099230322463,33.3938750538235));
#69253=CARTESIAN_POINT('',(33.3226453080309,25.4310730087083,33.8016349549212));
#69254=CARTESIAN_POINT('Origin',(26.8550245390365,0.,0.));
#69255=CARTESIAN_POINT('',(33.0966075166785,23.1273809239214,30.1149569673582));
#69256=CARTESIAN_POINT('Origin',(17.5,19.,32.9089653438087));
#69257=CARTESIAN_POINT('',(33.1,17.5710580837557,33.7339653438087));
#69258=CARTESIAN_POINT('',(33.1,17.5710580837557,33.7339653438087));
#69259=CARTESIAN_POINT('',(30.5,17.5710580837557,33.7339653438087));
#69260=CARTESIAN_POINT('',(30.5,17.5710580837557,33.7339653438087));
#69261=CARTESIAN_POINT('',(30.5,18.0040707856479,33.4839653438087));
#69262=CARTESIAN_POINT('',(30.5,18.0040707856479,33.4839653438087));
#69263=CARTESIAN_POINT('',(24.1,18.3504809471617,33.2839653438087));
#69264=CARTESIAN_POINT('',(24.1,18.3504809471617,33.2839653438087));
#69265=CARTESIAN_POINT('',(23.1,18.0906733260263,33.4339653438087));
#69266=CARTESIAN_POINT('',(23.1,18.0906733260263,33.4339653438087));
#69267=CARTESIAN_POINT('',(22.4,17.7442631645126,33.6339653438087));
#69268=CARTESIAN_POINT('',(22.4,17.7442631645126,33.6339653438087));
#69269=CARTESIAN_POINT('',(21.8,17.5710580837557,33.7339653438087));
#69270=CARTESIAN_POINT('',(21.8,17.5710580837557,33.7339653438087));
#69271=CARTESIAN_POINT('',(13.2,17.5710580837557,33.7339653438087));
#69272=CARTESIAN_POINT('',(13.2,17.5710580837557,33.7339653438087));
#69273=CARTESIAN_POINT('',(12.6,17.7442631645126,33.6339653438087));
#69274=CARTESIAN_POINT('',(12.6,17.7442631645126,33.6339653438087));
#69275=CARTESIAN_POINT('',(11.9,18.0906733260263,33.4339653438087));
#69276=CARTESIAN_POINT('',(11.9,18.0906733260263,33.4339653438087));
#69277=CARTESIAN_POINT('',(10.9,18.3504809471617,33.2839653438087));
#69278=CARTESIAN_POINT('',(10.9,18.3504809471617,33.2839653438087));
#69279=CARTESIAN_POINT('',(4.5,18.0040707856479,33.4839653438087));
#69280=CARTESIAN_POINT('',(4.5,18.0040707856479,33.4839653438087));
#69281=CARTESIAN_POINT('',(4.5,17.5710580837557,33.7339653438087));
#69282=CARTESIAN_POINT('',(4.5,17.5710580837557,33.7339653438087));
#69283=CARTESIAN_POINT('',(1.9,17.5710580837557,33.7339653438087));
#69284=CARTESIAN_POINT('',(1.9,17.5710580837557,33.7339653438087));
#69285=CARTESIAN_POINT('',(1.57538060255632,17.8151961173521,33.5930121843923));
#69286=CARTESIAN_POINT('',(0.,19.,32.9089653438087));
#69287=CARTESIAN_POINT('',(1.57538060255632,20.1848038826479,32.224918503225));
#69288=CARTESIAN_POINT('Ctrl Pts',(1.57538060255632,17.8151961173521,33.5930121843923));
#69289=CARTESIAN_POINT('Ctrl Pts',(1.62460345738085,19.000000000027,32.9089653437931));
#69290=CARTESIAN_POINT('Ctrl Pts',(1.57538060255632,20.1848038826479,32.224918503225));
#69291=CARTESIAN_POINT('',(1.9,20.4289419162443,32.0839653438087));
#69292=CARTESIAN_POINT('',(1.9,20.4289419162443,32.0839653438087));
#69293=CARTESIAN_POINT('',(4.5,20.4289419162443,32.0839653438087));
#69294=CARTESIAN_POINT('',(4.5,20.4289419162443,32.0839653438087));
#69295=CARTESIAN_POINT('',(4.5,19.9959292143521,32.3339653438087));
#69296=CARTESIAN_POINT('',(4.5,19.9959292143521,32.3339653438087));
#69297=CARTESIAN_POINT('',(10.9,19.6495190528383,32.5339653438087));
#69298=CARTESIAN_POINT('',(10.9,19.6495190528383,32.5339653438087));
#69299=CARTESIAN_POINT('',(11.9,19.9093266739737,32.3839653438087));
#69300=CARTESIAN_POINT('',(11.9,19.9093266739737,32.3839653438087));
#69301=CARTESIAN_POINT('',(12.6,20.2557368354874,32.1839653438087));
#69302=CARTESIAN_POINT('',(12.6,20.2557368354874,32.1839653438087));
#69303=CARTESIAN_POINT('',(13.2,20.4289419162443,32.0839653438087));
#69304=CARTESIAN_POINT('',(13.2,20.4289419162443,32.0839653438087));
#69305=CARTESIAN_POINT('',(21.8,20.4289419162443,32.0839653438087));
#69306=CARTESIAN_POINT('',(21.8,20.4289419162443,32.0839653438087));
#69307=CARTESIAN_POINT('',(22.4,20.2557368354874,32.1839653438087));
#69308=CARTESIAN_POINT('',(22.4,20.2557368354874,32.1839653438087));
#69309=CARTESIAN_POINT('',(23.1,19.9093266739737,32.3839653438087));
#69310=CARTESIAN_POINT('',(23.1,19.9093266739737,32.3839653438087));
#69311=CARTESIAN_POINT('',(24.1,19.6495190528383,32.5339653438087));
#69312=CARTESIAN_POINT('',(24.1,19.6495190528383,32.5339653438087));
#69313=CARTESIAN_POINT('',(30.5,19.9959292143521,32.3339653438087));
#69314=CARTESIAN_POINT('',(30.5,19.9959292143521,32.3339653438087));
#69315=CARTESIAN_POINT('',(30.5,20.4289419162443,32.0839653438087));
#69316=CARTESIAN_POINT('',(30.5,20.4289419162443,32.0839653438087));
#69317=CARTESIAN_POINT('',(33.1,20.4289419162443,32.0839653438087));
#69318=CARTESIAN_POINT('',(33.1,20.4289419162443,32.0839653438087));
#69319=CARTESIAN_POINT('',(35.,19.,32.9089653438087));
#69320=CARTESIAN_POINT('Origin',(35.,19.,32.9089653438087));
#69321=CARTESIAN_POINT('',(35.,20.6092962603321,37.4646652720015));
#69322=CARTESIAN_POINT('',(35.,15.6628468484386,23.4619363860708));
#69323=CARTESIAN_POINT('',(34.8617922858584,20.5053537361819,37.5246765162999));
#69324=CARTESIAN_POINT('',(33.5377160618333,19.5095495168072,38.099604350416));
#69325=CARTESIAN_POINT('',(34.4,19.9986373454573,37.2739118462884));
#69326=CARTESIAN_POINT('Ctrl Pts',(34.4,19.9986373454573,37.2739118462884));
#69327=CARTESIAN_POINT('Ctrl Pts',(34.6297825291024,20.2509844800861,37.3992864560073));
#69328=CARTESIAN_POINT('Ctrl Pts',(34.8617922858584,20.5053537361819,37.5246765162999));
#69329=CARTESIAN_POINT('',(33.3226453080309,19.1751255543105,37.7041716521717));
#69330=CARTESIAN_POINT('Origin',(26.8550245390365,0.,0.));
#69331=CARTESIAN_POINT('',(33.0966075166785,17.5466166428447,33.6734706547313));
#69332=CARTESIAN_POINT('Origin',(17.5,12.9967654463754,35.7083195898645));
#69333=CARTESIAN_POINT('',(33.1,11.4462726220787,36.2726528263519));
#69334=CARTESIAN_POINT('',(33.1,11.4462726220787,36.2726528263519));
#69335=CARTESIAN_POINT('',(30.5,11.4462726220787,36.2726528263519));
#69336=CARTESIAN_POINT('',(30.5,11.4462726220787,36.2726528263519));
#69337=CARTESIAN_POINT('',(30.5,11.9161189324716,36.101642754689));
#69338=CARTESIAN_POINT('',(30.5,11.9161189324716,36.101642754689));
#69339=CARTESIAN_POINT('',(24.1,12.291995980786,35.9648346973588));
#69340=CARTESIAN_POINT('',(24.1,12.291995980786,35.9648346973588));
#69341=CARTESIAN_POINT('',(23.1,12.0100881945502,36.0674407403565));
#69342=CARTESIAN_POINT('',(23.1,12.0100881945502,36.0674407403565));
#69343=CARTESIAN_POINT('',(22.4,11.6342111462359,36.2042487976867));
#69344=CARTESIAN_POINT('',(22.4,11.6342111462359,36.2042487976867));
#69345=CARTESIAN_POINT('',(21.8,11.4462726220787,36.2726528263519));
#69346=CARTESIAN_POINT('',(21.8,11.4462726220787,36.2726528263519));
#69347=CARTESIAN_POINT('',(13.2,11.4462726220787,36.2726528263519));
#69348=CARTESIAN_POINT('',(13.2,11.4462726220787,36.2726528263519));
#69349=CARTESIAN_POINT('',(12.6,11.6342111462359,36.2042487976867));
#69350=CARTESIAN_POINT('',(12.6,11.6342111462359,36.2042487976867));
#69351=CARTESIAN_POINT('',(11.9,12.0100881945502,36.0674407403565));
#69352=CARTESIAN_POINT('',(11.9,12.0100881945502,36.0674407403565));
#69353=CARTESIAN_POINT('',(10.9,12.291995980786,35.9648346973588));
#69354=CARTESIAN_POINT('',(10.9,12.291995980786,35.9648346973588));
#69355=CARTESIAN_POINT('',(4.5,11.9161189324716,36.101642754689));
#69356=CARTESIAN_POINT('',(4.5,11.9161189324716,36.101642754689));
#69357=CARTESIAN_POINT('',(4.5,11.4462726220787,36.2726528263519));
#69358=CARTESIAN_POINT('',(4.5,11.4462726220787,36.2726528263519));
#69359=CARTESIAN_POINT('',(1.9,11.4462726220787,36.2726528263519));
#69360=CARTESIAN_POINT('',(1.9,11.4462726220787,36.2726528263519));
#69361=CARTESIAN_POINT('',(1.57538060255632,11.7111779096386,36.1762351867803));
#69362=CARTESIAN_POINT('',(0.,12.9967654463754,35.7083195898645));
#69363=CARTESIAN_POINT('',(1.57538060255633,14.2823529831122,35.2404039929487));
#69364=CARTESIAN_POINT('Ctrl Pts',(1.57538060255632,11.7111779096386,36.1762351867803));
#69365=CARTESIAN_POINT('Ctrl Pts',(1.62460345738085,12.9967654464047,35.7083195898538));
#69366=CARTESIAN_POINT('Ctrl Pts',(1.57538060255633,14.2823529831122,35.2404039929487));
#69367=CARTESIAN_POINT('',(1.9,14.5472582706722,35.1439863533772));
#69368=CARTESIAN_POINT('',(1.9,14.5472582706722,35.1439863533772));
#69369=CARTESIAN_POINT('',(4.5,14.5472582706722,35.1439863533772));
#69370=CARTESIAN_POINT('',(4.5,14.5472582706722,35.1439863533772));
#69371=CARTESIAN_POINT('',(4.5,14.0774119602792,35.31499642504));
#69372=CARTESIAN_POINT('',(4.5,14.0774119602792,35.31499642504));
#69373=CARTESIAN_POINT('',(10.9,13.7015349119648,35.4518044823703));
#69374=CARTESIAN_POINT('',(10.9,13.7015349119648,35.4518044823703));
#69375=CARTESIAN_POINT('',(11.9,13.9834426982006,35.3491984393726));
#69376=CARTESIAN_POINT('',(11.9,13.9834426982006,35.3491984393726));
#69377=CARTESIAN_POINT('',(12.6,14.359319746515,35.2123903820423));
#69378=CARTESIAN_POINT('',(12.6,14.359319746515,35.2123903820423));
#69379=CARTESIAN_POINT('',(13.2,14.5472582706722,35.1439863533772));
#69380=CARTESIAN_POINT('',(13.2,14.5472582706722,35.1439863533772));
#69381=CARTESIAN_POINT('',(21.8,14.5472582706722,35.1439863533772));
#69382=CARTESIAN_POINT('',(21.8,14.5472582706722,35.1439863533772));
#69383=CARTESIAN_POINT('',(22.4,14.359319746515,35.2123903820423));
#69384=CARTESIAN_POINT('',(22.4,14.359319746515,35.2123903820423));
#69385=CARTESIAN_POINT('',(23.1,13.9834426982006,35.3491984393726));
#69386=CARTESIAN_POINT('',(23.1,13.9834426982006,35.3491984393726));
#69387=CARTESIAN_POINT('',(24.1,13.7015349119648,35.4518044823703));
#69388=CARTESIAN_POINT('',(24.1,13.7015349119648,35.4518044823703));
#69389=CARTESIAN_POINT('',(30.5,14.0774119602792,35.31499642504));
#69390=CARTESIAN_POINT('',(30.5,14.0774119602792,35.31499642504));
#69391=CARTESIAN_POINT('',(30.5,14.5472582706722,35.1439863533772));
#69392=CARTESIAN_POINT('',(30.5,14.5472582706722,35.1439863533772));
#69393=CARTESIAN_POINT('',(33.1,14.5472582706722,35.1439863533772));
#69394=CARTESIAN_POINT('',(33.1,14.5472582706722,35.1439863533772));
#69395=CARTESIAN_POINT('',(35.,12.9967654463754,35.7083195898645));
#69396=CARTESIAN_POINT('Origin',(35.,12.9967654463754,35.7083195898645));
#69397=CARTESIAN_POINT('',(35.,13.790523889916,40.4742595624789));
#69398=CARTESIAN_POINT('',(35.,10.6297856612634,21.4963339863891));
#69399=CARTESIAN_POINT('',(34.8617922858584,13.6777396430533,40.515309671231));
#69400=CARTESIAN_POINT('',(33.5377160618333,12.5972287566465,40.9085834716837));
#69401=CARTESIAN_POINT('',(34.4,13.22226624086,40.1803643021789));
#69402=CARTESIAN_POINT('Ctrl Pts',(34.4,13.22226624086,40.1803643021789));
#69403=CARTESIAN_POINT('Ctrl Pts',(34.6297825291026,13.4490085829898,40.3476538099288));
#69404=CARTESIAN_POINT('Ctrl Pts',(34.8617922858584,13.6777396430533,40.515309671231));
#69405=CARTESIAN_POINT('',(33.3226453080309,12.3365516130268,40.4610861730024));
#69406=CARTESIAN_POINT('Origin',(26.8550245390365,0.,0.));
#69407=CARTESIAN_POINT('',(33.0966075166785,11.4327072940915,36.2088329758587));
#69408=CARTESIAN_POINT('Origin',(17.5,6.59863075134336,37.4226946144639));
#69409=CARTESIAN_POINT('',(33.1,4.97369795887321,37.7092141076143));
#69410=CARTESIAN_POINT('',(33.1,4.97369795887321,37.7092141076143));
#69411=CARTESIAN_POINT('',(30.5,4.97369795887321,37.7092141076143));
#69412=CARTESIAN_POINT('',(30.5,4.97369795887321,37.7092141076143));
#69413=CARTESIAN_POINT('',(30.5,5.46610183537932,37.6223900187809));
#69414=CARTESIAN_POINT('',(30.5,5.46610183537932,37.6223900187809));
#69415=CARTESIAN_POINT('',(24.1,5.8600249365842,37.5529307477141));
#69416=CARTESIAN_POINT('',(24.1,5.8600249365842,37.5529307477141));
#69417=CARTESIAN_POINT('',(23.1,5.56458261068054,37.6050252010142));
#69418=CARTESIAN_POINT('',(23.1,5.56458261068054,37.6050252010142));
#69419=CARTESIAN_POINT('',(22.4,5.17065950947566,37.674484472081));
#69420=CARTESIAN_POINT('',(22.4,5.17065950947566,37.674484472081));
#69421=CARTESIAN_POINT('',(21.8,4.97369795887321,37.7092141076143));
#69422=CARTESIAN_POINT('',(21.8,4.97369795887321,37.7092141076143));
#69423=CARTESIAN_POINT('',(13.2,4.97369795887321,37.7092141076143));
#69424=CARTESIAN_POINT('',(13.2,4.97369795887321,37.7092141076143));
#69425=CARTESIAN_POINT('',(12.6,5.17065950947566,37.674484472081));
#69426=CARTESIAN_POINT('',(12.6,5.17065950947566,37.674484472081));
#69427=CARTESIAN_POINT('',(11.9,5.56458261068054,37.6050252010142));
#69428=CARTESIAN_POINT('',(11.9,5.56458261068054,37.6050252010142));
#69429=CARTESIAN_POINT('',(10.9,5.8600249365842,37.5529307477141));
#69430=CARTESIAN_POINT('',(10.9,5.8600249365842,37.5529307477141));
#69431=CARTESIAN_POINT('',(4.5,5.46610183537932,37.6223900187809));
#69432=CARTESIAN_POINT('',(4.5,5.46610183537932,37.6223900187809));
#69433=CARTESIAN_POINT('',(4.5,4.97369795887321,37.7092141076143));
#69434=CARTESIAN_POINT('',(4.5,4.97369795887321,37.7092141076143));
#69435=CARTESIAN_POINT('',(1.9,4.97369795887321,37.7092141076143));
#69436=CARTESIAN_POINT('',(1.9,4.97369795887321,37.7092141076143));
#69437=CARTESIAN_POINT('',(1.57538060255632,5.25132148728276,37.6602615890763));
#69438=CARTESIAN_POINT('',(0.,6.59863075134336,37.4226946144639));
#69439=CARTESIAN_POINT('',(1.57538060255632,7.94594001540395,37.1851276398516));
#69440=CARTESIAN_POINT('Ctrl Pts',(1.57538060255632,5.25132148728276,37.6602615890763));
#69441=CARTESIAN_POINT('Ctrl Pts',(1.62460345738085,6.59863075137406,37.4226946144585));
#69442=CARTESIAN_POINT('Ctrl Pts',(1.57538060255632,7.94594001540395,37.1851276398516));
#69443=CARTESIAN_POINT('',(1.9,8.2235635438135,37.1361751213135));
#69444=CARTESIAN_POINT('',(1.9,8.2235635438135,37.1361751213135));
#69445=CARTESIAN_POINT('',(4.5,8.2235635438135,37.1361751213135));
#69446=CARTESIAN_POINT('',(4.5,8.2235635438135,37.1361751213135));
#69447=CARTESIAN_POINT('',(4.5,7.7311596673074,37.2229992101469));
#69448=CARTESIAN_POINT('',(4.5,7.7311596673074,37.2229992101469));
#69449=CARTESIAN_POINT('',(10.9,7.33723656610251,37.2924584812137));
#69450=CARTESIAN_POINT('',(10.9,7.33723656610251,37.2924584812137));
#69451=CARTESIAN_POINT('',(11.9,7.63267889200617,37.2403640279136));
#69452=CARTESIAN_POINT('',(11.9,7.63267889200617,37.2403640279136));
#69453=CARTESIAN_POINT('',(12.6,8.02660199321106,37.1709047568469));
#69454=CARTESIAN_POINT('',(12.6,8.02660199321106,37.1709047568469));
#69455=CARTESIAN_POINT('',(13.2,8.2235635438135,37.1361751213135));
#69456=CARTESIAN_POINT('',(13.2,8.2235635438135,37.1361751213135));
#69457=CARTESIAN_POINT('',(21.8,8.2235635438135,37.1361751213135));
#69458=CARTESIAN_POINT('',(21.8,8.2235635438135,37.1361751213135));
#69459=CARTESIAN_POINT('',(22.4,8.02660199321106,37.1709047568469));
#69460=CARTESIAN_POINT('',(22.4,8.02660199321106,37.1709047568469));
#69461=CARTESIAN_POINT('',(23.1,7.63267889200617,37.2403640279136));
#69462=CARTESIAN_POINT('',(23.1,7.63267889200617,37.2403640279136));
#69463=CARTESIAN_POINT('',(24.1,7.33723656610251,37.2924584812137));
#69464=CARTESIAN_POINT('',(24.1,7.33723656610251,37.2924584812137));
#69465=CARTESIAN_POINT('',(30.5,7.7311596673074,37.2229992101469));
#69466=CARTESIAN_POINT('',(30.5,7.7311596673074,37.2229992101469));
#69467=CARTESIAN_POINT('',(30.5,8.2235635438135,37.1361751213135));
#69468=CARTESIAN_POINT('',(30.5,8.2235635438135,37.1361751213135));
#69469=CARTESIAN_POINT('',(33.1,8.2235635438135,37.1361751213135));
#69470=CARTESIAN_POINT('',(33.1,8.2235635438135,37.1361751213135));
#69471=CARTESIAN_POINT('',(35.,6.59863075134336,37.4226946144639));
#69472=CARTESIAN_POINT('Origin',(35.,6.59863075134336,37.4226946144639));
#69473=CARTESIAN_POINT('',(35.,6.55273342944653,42.2540639571139));
#69474=CARTESIAN_POINT('',(35.,6.77841834076261,18.497401987115));
#69475=CARTESIAN_POINT('',(34.8617922858584,6.4345343521407,42.2749056435377));
#69476=CARTESIAN_POINT('',(33.5377160618333,5.30214757522047,42.4745759849063));
#69477=CARTESIAN_POINT('',(34.4,6.04414326732376,41.8659567209931));
#69478=CARTESIAN_POINT('Ctrl Pts',(34.4,6.04414326732376,41.8659567209931));
#69479=CARTESIAN_POINT('Ctrl Pts',(34.6297825290984,6.23839136562223,42.0700781197299));
#69480=CARTESIAN_POINT('Ctrl Pts',(34.8617922858584,6.4345343521407,42.2749056435377));
#69481=CARTESIAN_POINT('',(33.3226453080309,5.12313779357752,41.9886110647639));
#69482=CARTESIAN_POINT('Origin',(26.8550245390365,0.,0.));
#69483=CARTESIAN_POINT('',(33.0966075166785,4.97142091943645,37.6440082295681));
#69484=CARTESIAN_POINT('Origin',(17.5,2.32682891837997E-15,38.));
#69485=CARTESIAN_POINT('',(33.1,-1.65,38.));
#69486=CARTESIAN_POINT('',(33.1,-1.65,38.));
#69487=CARTESIAN_POINT('',(30.5,-1.65,38.));
#69488=CARTESIAN_POINT('',(30.5,-1.65,38.));
#69489=CARTESIAN_POINT('',(30.5,-1.15,38.));
#69490=CARTESIAN_POINT('',(30.5,-1.15,38.));
#69491=CARTESIAN_POINT('',(24.1,-0.749999999999998,38.));
#69492=CARTESIAN_POINT('',(24.1,-0.749999999999998,38.));
#69493=CARTESIAN_POINT('',(23.1,-1.05,38.));
#69494=CARTESIAN_POINT('',(23.1,-1.05,38.));
#69495=CARTESIAN_POINT('',(22.4,-1.45,38.));
#69496=CARTESIAN_POINT('',(22.4,-1.45,38.));
#69497=CARTESIAN_POINT('',(21.8,-1.65,38.));
#69498=CARTESIAN_POINT('',(21.8,-1.65,38.));
#69499=CARTESIAN_POINT('',(13.2,-1.65,38.));
#69500=CARTESIAN_POINT('',(13.2,-1.65,38.));
#69501=CARTESIAN_POINT('',(12.6,-1.45,38.));
#69502=CARTESIAN_POINT('',(12.6,-1.45,38.));
#69503=CARTESIAN_POINT('',(11.9,-1.05,38.));
#69504=CARTESIAN_POINT('',(11.9,-1.05,38.));
#69505=CARTESIAN_POINT('',(10.9,-0.749999999999998,38.));
#69506=CARTESIAN_POINT('',(10.9,-0.749999999999998,38.));
#69507=CARTESIAN_POINT('',(4.5,-1.15,38.));
#69508=CARTESIAN_POINT('',(4.5,-1.15,38.));
#69509=CARTESIAN_POINT('',(4.5,-1.65,38.));
#69510=CARTESIAN_POINT('',(4.5,-1.65,38.));
#69511=CARTESIAN_POINT('',(1.9,-1.65,38.));
#69512=CARTESIAN_POINT('',(1.9,-1.65,38.));
#69513=CARTESIAN_POINT('',(1.57538060255632,-1.36809368116733,38.));
#69514=CARTESIAN_POINT('',(0.,2.32682891837997E-15,38.));
#69515=CARTESIAN_POINT('',(1.57538060255633,1.36809368116734,38.));
#69516=CARTESIAN_POINT('Ctrl Pts',(1.57538060255632,-1.36809368116733,38.));
#69517=CARTESIAN_POINT('Ctrl Pts',(1.62460345738085,3.1181446313866E-11,
38.));
#69518=CARTESIAN_POINT('Ctrl Pts',(1.57538060255633,1.36809368116734,38.));
#69519=CARTESIAN_POINT('',(1.9,1.65,38.));
#69520=CARTESIAN_POINT('',(1.9,1.65,38.));
#69521=CARTESIAN_POINT('',(4.5,1.65,38.));
#69522=CARTESIAN_POINT('',(4.5,1.65,38.));
#69523=CARTESIAN_POINT('',(4.5,1.15,38.));
#69524=CARTESIAN_POINT('',(4.5,1.15,38.));
#69525=CARTESIAN_POINT('',(10.9,0.750000000000002,38.));
#69526=CARTESIAN_POINT('',(10.9,0.750000000000002,38.));
#69527=CARTESIAN_POINT('',(11.9,1.05,38.));
#69528=CARTESIAN_POINT('',(11.9,1.05,38.));
#69529=CARTESIAN_POINT('',(12.6,1.45,38.));
#69530=CARTESIAN_POINT('',(12.6,1.45,38.));
#69531=CARTESIAN_POINT('',(13.2,1.65,38.));
#69532=CARTESIAN_POINT('',(13.2,1.65,38.));
#69533=CARTESIAN_POINT('',(21.8,1.65,38.));
#69534=CARTESIAN_POINT('',(21.8,1.65,38.));
#69535=CARTESIAN_POINT('',(22.4,1.45,38.));
#69536=CARTESIAN_POINT('',(22.4,1.45,38.));
#69537=CARTESIAN_POINT('',(23.1,1.05,38.));
#69538=CARTESIAN_POINT('',(23.1,1.05,38.));
#69539=CARTESIAN_POINT('',(24.1,0.750000000000002,38.));
#69540=CARTESIAN_POINT('',(24.1,0.750000000000002,38.));
#69541=CARTESIAN_POINT('',(30.5,1.15,38.));
#69542=CARTESIAN_POINT('',(30.5,1.15,38.));
#69543=CARTESIAN_POINT('',(30.5,1.65,38.));
#69544=CARTESIAN_POINT('',(30.5,1.65,38.));
#69545=CARTESIAN_POINT('',(33.1,1.65,38.));
#69546=CARTESIAN_POINT('',(33.1,1.65,38.));
#69547=CARTESIAN_POINT('',(35.,2.32682891837997E-15,38.));
#69548=CARTESIAN_POINT('Origin',(35.,2.32682891837997E-15,38.));
#69549=CARTESIAN_POINT('',(35.,-0.884158520433533,42.75));
#69550=CARTESIAN_POINT('',(35.,4.28887236871593,14.95872031928));
#69551=CARTESIAN_POINT('',(34.8617922858584,-1.0041810090302,42.75));
#69552=CARTESIAN_POINT('',(33.5377160618333,-2.15403667726254,42.75));
#69553=CARTESIAN_POINT('',(34.4,-1.31762794090604,42.2794732300362));
#69554=CARTESIAN_POINT('Ctrl Pts',(34.4,-1.31762794090604,42.2794732300361));
#69555=CARTESIAN_POINT('Ctrl Pts',(34.6297825291,-1.16177621660623,42.5142243943543));
#69556=CARTESIAN_POINT('Ctrl Pts',(34.8617922858584,-1.0041810090302,42.75));
#69557=CARTESIAN_POINT('',(33.3226453080309,-2.24593997529677,42.240333256585));
#69558=CARTESIAN_POINT('Origin',(26.8550245390365,0.,0.));
#69559=CARTESIAN_POINT('',(33.0966075166785,-1.64091956419533,37.9353893420094));
#69560=CARTESIAN_POINT('Origin',(17.5,-6.59863075134335,37.4226946144639));
#69561=CARTESIAN_POINT('',(33.1,-8.22356354381349,37.1361751213135));
#69562=CARTESIAN_POINT('',(33.1,-8.22356354381349,37.1361751213135));
#69563=CARTESIAN_POINT('',(30.5,-8.22356354381349,37.1361751213135));
#69564=CARTESIAN_POINT('',(30.5,-8.22356354381349,37.1361751213135));
#69565=CARTESIAN_POINT('',(30.5,-7.73115966730739,37.2229992101469));
#69566=CARTESIAN_POINT('',(30.5,-7.73115966730739,37.2229992101469));
#69567=CARTESIAN_POINT('',(24.1,-7.33723656610251,37.2924584812137));
#69568=CARTESIAN_POINT('',(24.1,-7.33723656610251,37.2924584812137));
#69569=CARTESIAN_POINT('',(23.1,-7.63267889200617,37.2403640279136));
#69570=CARTESIAN_POINT('',(23.1,-7.63267889200617,37.2403640279136));
#69571=CARTESIAN_POINT('',(22.4,-8.02660199321105,37.1709047568469));
#69572=CARTESIAN_POINT('',(22.4,-8.02660199321105,37.1709047568469));
#69573=CARTESIAN_POINT('',(21.8,-8.22356354381349,37.1361751213135));
#69574=CARTESIAN_POINT('',(21.8,-8.22356354381349,37.1361751213135));
#69575=CARTESIAN_POINT('',(13.2,-8.22356354381349,37.1361751213135));
#69576=CARTESIAN_POINT('',(13.2,-8.22356354381349,37.1361751213135));
#69577=CARTESIAN_POINT('',(12.6,-8.02660199321105,37.1709047568469));
#69578=CARTESIAN_POINT('',(12.6,-8.02660199321105,37.1709047568469));
#69579=CARTESIAN_POINT('',(11.9,-7.63267889200617,37.2403640279136));
#69580=CARTESIAN_POINT('',(11.9,-7.63267889200617,37.2403640279136));
#69581=CARTESIAN_POINT('',(10.9,-7.33723656610251,37.2924584812137));
#69582=CARTESIAN_POINT('',(10.9,-7.33723656610251,37.2924584812137));
#69583=CARTESIAN_POINT('',(4.5,-7.73115966730739,37.2229992101469));
#69584=CARTESIAN_POINT('',(4.5,-7.73115966730739,37.2229992101469));
#69585=CARTESIAN_POINT('',(4.5,-8.22356354381349,37.1361751213135));
#69586=CARTESIAN_POINT('',(4.5,-8.22356354381349,37.1361751213135));
#69587=CARTESIAN_POINT('',(1.9,-8.22356354381349,37.1361751213135));
#69588=CARTESIAN_POINT('',(1.9,-8.22356354381349,37.1361751213135));
#69589=CARTESIAN_POINT('',(1.57538060255632,-7.94594001540396,37.1851276398516));
#69590=CARTESIAN_POINT('',(0.,-6.59863075134335,37.4226946144639));
#69591=CARTESIAN_POINT('',(1.57538060255632,-5.25132148728275,37.6602615890763));
#69592=CARTESIAN_POINT('Ctrl Pts',(1.57538060255632,-7.94594001540396,37.1851276398516));
#69593=CARTESIAN_POINT('Ctrl Pts',(1.62460345738085,-6.59863075131265,37.4226946144693));
#69594=CARTESIAN_POINT('Ctrl Pts',(1.57538060255632,-5.25132148728275,37.6602615890763));
#69595=CARTESIAN_POINT('',(1.9,-4.97369795887321,37.7092141076143));
#69596=CARTESIAN_POINT('',(1.9,-4.97369795887321,37.7092141076143));
#69597=CARTESIAN_POINT('',(4.5,-4.97369795887321,37.7092141076143));
#69598=CARTESIAN_POINT('',(4.5,-4.97369795887321,37.7092141076143));
#69599=CARTESIAN_POINT('',(4.5,-5.46610183537931,37.6223900187809));
#69600=CARTESIAN_POINT('',(4.5,-5.46610183537931,37.6223900187809));
#69601=CARTESIAN_POINT('',(10.9,-5.8600249365842,37.5529307477141));
#69602=CARTESIAN_POINT('',(10.9,-5.8600249365842,37.5529307477141));
#69603=CARTESIAN_POINT('',(11.9,-5.56458261068053,37.6050252010142));
#69604=CARTESIAN_POINT('',(11.9,-5.56458261068053,37.6050252010142));
#69605=CARTESIAN_POINT('',(12.6,-5.17065950947565,37.674484472081));
#69606=CARTESIAN_POINT('',(12.6,-5.17065950947565,37.674484472081));
#69607=CARTESIAN_POINT('',(13.2,-4.97369795887321,37.7092141076143));
#69608=CARTESIAN_POINT('',(13.2,-4.97369795887321,37.7092141076143));
#69609=CARTESIAN_POINT('',(21.8,-4.97369795887321,37.7092141076143));
#69610=CARTESIAN_POINT('',(21.8,-4.97369795887321,37.7092141076143));
#69611=CARTESIAN_POINT('',(22.4,-5.17065950947565,37.674484472081));
#69612=CARTESIAN_POINT('',(22.4,-5.17065950947565,37.674484472081));
#69613=CARTESIAN_POINT('',(23.1,-5.56458261068053,37.6050252010142));
#69614=CARTESIAN_POINT('',(23.1,-5.56458261068053,37.6050252010142));
#69615=CARTESIAN_POINT('',(24.1,-5.8600249365842,37.5529307477141));
#69616=CARTESIAN_POINT('',(24.1,-5.8600249365842,37.5529307477141));
#69617=CARTESIAN_POINT('',(30.5,-5.46610183537931,37.6223900187809));
#69618=CARTESIAN_POINT('',(30.5,-5.46610183537931,37.6223900187809));
#69619=CARTESIAN_POINT('',(30.5,-4.97369795887321,37.7092141076143));
#69620=CARTESIAN_POINT('',(30.5,-4.97369795887321,37.7092141076143));
#69621=CARTESIAN_POINT('',(33.1,-4.97369795887321,37.7092141076143));
#69622=CARTESIAN_POINT('',(33.1,-4.97369795887321,37.7092141076143));
#69623=CARTESIAN_POINT('',(35.,-6.59863075134335,37.4226946144639));
#69624=CARTESIAN_POINT('Origin',(35.,-6.59863075134335,37.4226946144639));
#69625=CARTESIAN_POINT('',(35.,-8.29418576107602,41.9469989254299));
#69626=CARTESIAN_POINT('',(35.,3.1584421883261,11.3875810911838));
#69627=CARTESIAN_POINT('',(34.8617922858584,-8.41238483838184,41.9261572390061));
#69628=CARTESIAN_POINT('',(33.5377160618333,-9.54477161530208,41.7264868976375));
#69629=CARTESIAN_POINT('',(34.4,-8.63936369090332,41.4083493394303));
#69630=CARTESIAN_POINT('Ctrl Pts',(34.4,-8.63936369090333,41.4083493394303));
#69631=CARTESIAN_POINT('Ctrl Pts',(34.6297825291073,-8.52664381637799,41.6665974739986));
#69632=CARTESIAN_POINT('Ctrl Pts',(34.8617922858584,-8.41238483838184,41.9261572390061));
#69633=CARTESIAN_POINT('',(33.3226453080309,-9.54677599452213,41.2086042970448));
#69634=CARTESIAN_POINT('Origin',(26.8550245390365,0.,0.));
#69635=CARTESIAN_POINT('',(33.0966075166785,-8.20340153721441,37.0741228455271));
#69636=CARTESIAN_POINT('Origin',(17.5,-12.9967654463754,35.7083195898645));
#69637=CARTESIAN_POINT('',(33.1,-14.5472582706722,35.1439863533772));
#69638=CARTESIAN_POINT('',(33.1,-14.5472582706722,35.1439863533772));
#69639=CARTESIAN_POINT('',(30.5,-14.5472582706722,35.1439863533772));
#69640=CARTESIAN_POINT('',(30.5,-14.5472582706722,35.1439863533772));
#69641=CARTESIAN_POINT('',(30.5,-14.0774119602792,35.31499642504));
#69642=CARTESIAN_POINT('',(30.5,-14.0774119602792,35.31499642504));
#69643=CARTESIAN_POINT('',(24.1,-13.7015349119648,35.4518044823703));
#69644=CARTESIAN_POINT('',(24.1,-13.7015349119648,35.4518044823703));
#69645=CARTESIAN_POINT('',(23.1,-13.9834426982006,35.3491984393726));
#69646=CARTESIAN_POINT('',(23.1,-13.9834426982006,35.3491984393726));
#69647=CARTESIAN_POINT('',(22.4,-14.359319746515,35.2123903820423));
#69648=CARTESIAN_POINT('',(22.4,-14.359319746515,35.2123903820423));
#69649=CARTESIAN_POINT('',(21.8,-14.5472582706722,35.1439863533772));
#69650=CARTESIAN_POINT('',(21.8,-14.5472582706722,35.1439863533772));
#69651=CARTESIAN_POINT('',(13.2,-14.5472582706722,35.1439863533772));
#69652=CARTESIAN_POINT('',(13.2,-14.5472582706722,35.1439863533772));
#69653=CARTESIAN_POINT('',(12.6,-14.359319746515,35.2123903820423));
#69654=CARTESIAN_POINT('',(12.6,-14.359319746515,35.2123903820423));
#69655=CARTESIAN_POINT('',(11.9,-13.9834426982006,35.3491984393726));
#69656=CARTESIAN_POINT('',(11.9,-13.9834426982006,35.3491984393726));
#69657=CARTESIAN_POINT('',(10.9,-13.7015349119648,35.4518044823703));
#69658=CARTESIAN_POINT('',(10.9,-13.7015349119648,35.4518044823703));
#69659=CARTESIAN_POINT('',(4.5,-14.0774119602792,35.31499642504));
#69660=CARTESIAN_POINT('',(4.5,-14.0774119602792,35.31499642504));
#69661=CARTESIAN_POINT('',(4.5,-14.5472582706722,35.1439863533772));
#69662=CARTESIAN_POINT('',(4.5,-14.5472582706722,35.1439863533772));
#69663=CARTESIAN_POINT('',(1.9,-14.5472582706722,35.1439863533772));
#69664=CARTESIAN_POINT('',(1.9,-14.5472582706722,35.1439863533772));
#69665=CARTESIAN_POINT('',(1.57538060255632,-14.2823529831122,35.2404039929487));
#69666=CARTESIAN_POINT('',(0.,-12.9967654463754,35.7083195898645));
#69667=CARTESIAN_POINT('',(1.57538060255632,-11.7111779096386,36.1762351867803));
#69668=CARTESIAN_POINT('Ctrl Pts',(1.57538060255632,-14.2823529831122,35.2404039929487));
#69669=CARTESIAN_POINT('Ctrl Pts',(1.62460345738085,-12.9967654463461,35.7083195898752));
#69670=CARTESIAN_POINT('Ctrl Pts',(1.57538060255632,-11.7111779096386,36.1762351867803));
#69671=CARTESIAN_POINT('',(1.9,-11.4462726220787,36.2726528263519));
#69672=CARTESIAN_POINT('',(1.9,-11.4462726220787,36.2726528263519));
#69673=CARTESIAN_POINT('',(4.5,-11.4462726220787,36.2726528263519));
#69674=CARTESIAN_POINT('',(4.5,-11.4462726220787,36.2726528263519));
#69675=CARTESIAN_POINT('',(4.5,-11.9161189324716,36.101642754689));
#69676=CARTESIAN_POINT('',(4.5,-11.9161189324716,36.101642754689));
#69677=CARTESIAN_POINT('',(10.9,-12.291995980786,35.9648346973588));
#69678=CARTESIAN_POINT('',(10.9,-12.291995980786,35.9648346973588));
#69679=CARTESIAN_POINT('',(11.9,-12.0100881945502,36.0674407403565));
#69680=CARTESIAN_POINT('',(11.9,-12.0100881945502,36.0674407403565));
#69681=CARTESIAN_POINT('',(12.6,-11.6342111462358,36.2042487976867));
#69682=CARTESIAN_POINT('',(12.6,-11.6342111462358,36.2042487976867));
#69683=CARTESIAN_POINT('',(13.2,-11.4462726220787,36.2726528263519));
#69684=CARTESIAN_POINT('',(13.2,-11.4462726220787,36.2726528263519));
#69685=CARTESIAN_POINT('',(21.8,-11.4462726220787,36.2726528263519));
#69686=CARTESIAN_POINT('',(21.8,-11.4462726220787,36.2726528263519));
#69687=CARTESIAN_POINT('',(22.4,-11.6342111462358,36.2042487976867));
#69688=CARTESIAN_POINT('',(22.4,-11.6342111462358,36.2042487976867));
#69689=CARTESIAN_POINT('',(23.1,-12.0100881945502,36.0674407403565));
#69690=CARTESIAN_POINT('',(23.1,-12.0100881945502,36.0674407403565));
#69691=CARTESIAN_POINT('',(24.1,-12.291995980786,35.9648346973588));
#69692=CARTESIAN_POINT('',(24.1,-12.291995980786,35.9648346973588));
#69693=CARTESIAN_POINT('',(30.5,-11.9161189324716,36.101642754689));
#69694=CARTESIAN_POINT('',(30.5,-11.9161189324716,36.101642754689));
#69695=CARTESIAN_POINT('',(30.5,-11.4462726220787,36.2726528263519));
#69696=CARTESIAN_POINT('',(30.5,-11.4462726220787,36.2726528263519));
#69697=CARTESIAN_POINT('',(33.1,-11.4462726220787,36.2726528263519));
#69698=CARTESIAN_POINT('',(33.1,-11.4462726220787,36.2726528263519));
#69699=CARTESIAN_POINT('',(35.,-12.9967654463754,35.7083195898645));
#69700=CARTESIAN_POINT('Origin',(35.,-12.9967654463754,35.7083195898645));
#69701=CARTESIAN_POINT('',(35.,-15.4521983644287,39.8694595147163));
#69702=CARTESIAN_POINT('',(35.,3.21112147516056,8.24135648498115));
#69703=CARTESIAN_POINT('',(34.8617922858584,-15.5649826112914,39.8284094059642));
#69704=CARTESIAN_POINT('',(33.5377160618333,-16.6454934976981,39.4351356055115));
#69705=CARTESIAN_POINT('',(34.4,-15.6985967468815,39.2790537077817));
#69706=CARTESIAN_POINT('Ctrl Pts',(34.4,-15.6985967468815,39.2790537077817));
#69707=CARTESIAN_POINT('Ctrl Pts',(34.6297825291032,-15.6324336584852,39.5529520736987));
#69708=CARTESIAN_POINT('Ctrl Pts',(34.8617922858584,-15.5649826112914,39.8284094059642));
#69709=CARTESIAN_POINT('',(33.3226453080309,-16.5575380560557,38.9247727484987));
#69710=CARTESIAN_POINT('Origin',(26.8550245390365,0.,0.));
#69711=CARTESIAN_POINT('',(33.0966075166785,-14.5166273056467,35.0863778867947));
#69712=CARTESIAN_POINT('Origin',(17.5,-19.,32.9089653438087));
#69713=CARTESIAN_POINT('',(33.1,-20.4289419162443,32.0839653438087));
#69714=CARTESIAN_POINT('',(33.1,-20.4289419162443,32.0839653438087));
#69715=CARTESIAN_POINT('',(30.5,-20.4289419162443,32.0839653438087));
#69716=CARTESIAN_POINT('',(30.5,-20.4289419162443,32.0839653438087));
#69717=CARTESIAN_POINT('',(30.5,-19.9959292143521,32.3339653438087));
#69718=CARTESIAN_POINT('',(30.5,-19.9959292143521,32.3339653438087));
#69719=CARTESIAN_POINT('',(24.1,-19.6495190528383,32.5339653438087));
#69720=CARTESIAN_POINT('',(24.1,-19.6495190528383,32.5339653438087));
#69721=CARTESIAN_POINT('',(23.1,-19.9093266739737,32.3839653438087));
#69722=CARTESIAN_POINT('',(23.1,-19.9093266739737,32.3839653438087));
#69723=CARTESIAN_POINT('',(22.4,-20.2557368354874,32.1839653438087));
#69724=CARTESIAN_POINT('',(22.4,-20.2557368354874,32.1839653438087));
#69725=CARTESIAN_POINT('',(21.8,-20.4289419162443,32.0839653438087));
#69726=CARTESIAN_POINT('',(21.8,-20.4289419162443,32.0839653438087));
#69727=CARTESIAN_POINT('',(13.2,-20.4289419162443,32.0839653438087));
#69728=CARTESIAN_POINT('',(13.2,-20.4289419162443,32.0839653438087));
#69729=CARTESIAN_POINT('',(12.6,-20.2557368354874,32.1839653438087));
#69730=CARTESIAN_POINT('',(12.6,-20.2557368354874,32.1839653438087));
#69731=CARTESIAN_POINT('',(11.9,-19.9093266739737,32.3839653438087));
#69732=CARTESIAN_POINT('',(11.9,-19.9093266739737,32.3839653438087));
#69733=CARTESIAN_POINT('',(10.9,-19.6495190528383,32.5339653438087));
#69734=CARTESIAN_POINT('',(10.9,-19.6495190528383,32.5339653438087));
#69735=CARTESIAN_POINT('',(4.5,-19.9959292143521,32.3339653438087));
#69736=CARTESIAN_POINT('',(4.5,-19.9959292143521,32.3339653438087));
#69737=CARTESIAN_POINT('',(4.5,-20.4289419162443,32.0839653438087));
#69738=CARTESIAN_POINT('',(4.5,-20.4289419162443,32.0839653438087));
#69739=CARTESIAN_POINT('',(1.9,-20.4289419162443,32.0839653438087));
#69740=CARTESIAN_POINT('',(1.9,-20.4289419162443,32.0839653438087));
#69741=CARTESIAN_POINT('',(1.57538060255632,-20.1848038826479,32.224918503225));
#69742=CARTESIAN_POINT('',(0.,-19.,32.9089653438087));
#69743=CARTESIAN_POINT('',(1.57538060255632,-17.8151961173521,33.5930121843923));
#69744=CARTESIAN_POINT('Ctrl Pts',(1.57538060255632,-20.1848038826479,32.224918503225));
#69745=CARTESIAN_POINT('Ctrl Pts',(1.62460345738085,-18.999999999973,32.9089653438243));
#69746=CARTESIAN_POINT('Ctrl Pts',(1.57538060255632,-17.8151961173521,33.5930121843923));
#69747=CARTESIAN_POINT('',(1.9,-17.5710580837557,33.7339653438087));
#69748=CARTESIAN_POINT('',(1.9,-17.5710580837557,33.7339653438087));
#69749=CARTESIAN_POINT('',(4.5,-17.5710580837557,33.7339653438087));
#69750=CARTESIAN_POINT('',(4.5,-17.5710580837557,33.7339653438087));
#69751=CARTESIAN_POINT('',(4.5,-18.0040707856479,33.4839653438087));
#69752=CARTESIAN_POINT('',(4.5,-18.0040707856479,33.4839653438087));
#69753=CARTESIAN_POINT('',(10.9,-18.3504809471617,33.2839653438087));
#69754=CARTESIAN_POINT('',(10.9,-18.3504809471617,33.2839653438087));
#69755=CARTESIAN_POINT('',(11.9,-18.0906733260263,33.4339653438087));
#69756=CARTESIAN_POINT('',(11.9,-18.0906733260263,33.4339653438087));
#69757=CARTESIAN_POINT('',(12.6,-17.7442631645126,33.6339653438087));
#69758=CARTESIAN_POINT('',(12.6,-17.7442631645126,33.6339653438087));
#69759=CARTESIAN_POINT('',(13.2,-17.5710580837557,33.7339653438087));
#69760=CARTESIAN_POINT('',(13.2,-17.5710580837557,33.7339653438087));
#69761=CARTESIAN_POINT('',(21.8,-17.5710580837557,33.7339653438087));
#69762=CARTESIAN_POINT('',(21.8,-17.5710580837557,33.7339653438087));
#69763=CARTESIAN_POINT('',(22.4,-17.7442631645126,33.6339653438087));
#69764=CARTESIAN_POINT('',(22.4,-17.7442631645126,33.6339653438087));
#69765=CARTESIAN_POINT('',(23.1,-18.0906733260263,33.4339653438087));
#69766=CARTESIAN_POINT('',(23.1,-18.0906733260263,33.4339653438087));
#69767=CARTESIAN_POINT('',(24.1,-18.3504809471617,33.2839653438087));
#69768=CARTESIAN_POINT('',(24.1,-18.3504809471617,33.2839653438087));
#69769=CARTESIAN_POINT('',(30.5,-18.0040707856479,33.4839653438087));
#69770=CARTESIAN_POINT('',(30.5,-18.0040707856479,33.4839653438087));
#69771=CARTESIAN_POINT('',(30.5,-17.5710580837557,33.7339653438087));
#69772=CARTESIAN_POINT('',(30.5,-17.5710580837557,33.7339653438087));
#69773=CARTESIAN_POINT('',(33.1,-17.5710580837557,33.7339653438087));
#69774=CARTESIAN_POINT('',(33.1,-17.5710580837557,33.7339653438087));
#69775=CARTESIAN_POINT('',(35.,-19.,32.9089653438087));
#69776=CARTESIAN_POINT('Origin',(35.,-19.,32.9089653438087));
#69777=CARTESIAN_POINT('',(35.,-22.1407037396679,36.580506751568));
#69778=CARTESIAN_POINT('',(35.,4.12832278188515,5.87152347586176));
#69779=CARTESIAN_POINT('',(34.8617922858584,-22.244646263818,36.5204955072697));
#69780=CARTESIAN_POINT('',(33.5377160618333,-23.2404504831928,35.9455676731535));
#69781=CARTESIAN_POINT('',(34.4,-22.2808358845789,35.9562839053824));
#69782=CARTESIAN_POINT('Ctrl Pts',(34.4,-22.2808358845789,35.9562839053824));
#69783=CARTESIAN_POINT('Ctrl Pts',(34.6297825291015,-22.2632399142706,36.2375102394016));
#69784=CARTESIAN_POINT('Ctrl Pts',(34.8617922858584,-22.244646263818,36.5204955072697));
#69785=CARTESIAN_POINT('',(33.3226453080309,-23.0652077022745,35.4582316768749));
#69786=CARTESIAN_POINT('Origin',(26.8550245390365,0.,0.));
#69787=CARTESIAN_POINT('',(33.0966075166785,-20.3887726991648,32.032551090536));
#69788=CARTESIAN_POINT('Origin',(17.5,-24.4259291680885,29.1096888385212));
#69789=CARTESIAN_POINT('',(33.1,-25.6899024992348,28.0490892825384));
#69790=CARTESIAN_POINT('',(33.1,-25.6899024992348,28.0490892825384));
#69791=CARTESIAN_POINT('',(30.5,-25.6899024992348,28.0490892825384));
#69792=CARTESIAN_POINT('',(30.5,-25.6899024992348,28.0490892825384));
#69793=CARTESIAN_POINT('',(30.5,-25.3068802776753,28.3704830873816));
#69794=CARTESIAN_POINT('',(30.5,-25.3068802776753,28.3704830873816));
#69795=CARTESIAN_POINT('',(24.1,-25.0004625004277,28.6275981312563));
#69796=CARTESIAN_POINT('',(24.1,-25.0004625004277,28.6275981312563));
#69797=CARTESIAN_POINT('',(23.1,-25.2302758333634,28.4347618483503));
#69798=CARTESIAN_POINT('',(23.1,-25.2302758333634,28.4347618483503));
#69799=CARTESIAN_POINT('',(22.4,-25.536693610611,28.1776468044757));
#69800=CARTESIAN_POINT('',(22.4,-25.536693610611,28.1776468044757));
#69801=CARTESIAN_POINT('',(21.8,-25.6899024992348,28.0490892825384));
#69802=CARTESIAN_POINT('',(21.8,-25.6899024992348,28.0490892825384));
#69803=CARTESIAN_POINT('',(13.2,-25.6899024992348,28.0490892825384));
#69804=CARTESIAN_POINT('',(13.2,-25.6899024992348,28.0490892825384));
#69805=CARTESIAN_POINT('',(12.6,-25.536693610611,28.1776468044757));
#69806=CARTESIAN_POINT('',(12.6,-25.536693610611,28.1776468044757));
#69807=CARTESIAN_POINT('',(11.9,-25.2302758333634,28.4347618483503));
#69808=CARTESIAN_POINT('',(11.9,-25.2302758333634,28.4347618483503));
#69809=CARTESIAN_POINT('',(10.9,-25.0004625004277,28.6275981312563));
#69810=CARTESIAN_POINT('',(10.9,-25.0004625004277,28.6275981312563));
#69811=CARTESIAN_POINT('',(4.5,-25.3068802776753,28.3704830873816));
#69812=CARTESIAN_POINT('',(4.5,-25.3068802776753,28.3704830873816));
#69813=CARTESIAN_POINT('',(4.5,-25.6899024992348,28.0490892825384));
#69814=CARTESIAN_POINT('',(4.5,-25.6899024992348,28.0490892825384));
#69815=CARTESIAN_POINT('',(1.9,-25.6899024992348,28.0490892825384));
#69816=CARTESIAN_POINT('',(1.9,-25.6899024992348,28.0490892825384));
#69817=CARTESIAN_POINT('',(1.57538060255633,-25.4739497302129,28.2302951713764));
#69818=CARTESIAN_POINT('',(0.,-24.4259291680885,29.1096888385212));
#69819=CARTESIAN_POINT('',(1.57538060255632,-23.3779086059641,29.989082505666));
#69820=CARTESIAN_POINT('Ctrl Pts',(1.57538060255633,-25.4739497302129,28.2302951713764));
#69821=CARTESIAN_POINT('Ctrl Pts',(1.62460345738085,-24.4259291680646,29.1096888385412));
#69822=CARTESIAN_POINT('Ctrl Pts',(1.57538060255632,-23.3779086059641,29.989082505666));
#69823=CARTESIAN_POINT('',(1.9,-23.1619558369422,30.170288394504));
#69824=CARTESIAN_POINT('',(1.9,-23.1619558369422,30.170288394504));
#69825=CARTESIAN_POINT('',(4.5,-23.1619558369422,30.170288394504));
#69826=CARTESIAN_POINT('',(4.5,-23.1619558369422,30.170288394504));
#69827=CARTESIAN_POINT('',(4.5,-23.5449780585017,29.8488945896607));
#69828=CARTESIAN_POINT('',(4.5,-23.5449780585017,29.8488945896607));
#69829=CARTESIAN_POINT('',(10.9,-23.8513958357493,29.5917795457861));
#69830=CARTESIAN_POINT('',(10.9,-23.8513958357493,29.5917795457861));
#69831=CARTESIAN_POINT('',(11.9,-23.6215825028136,29.784615828692));
#69832=CARTESIAN_POINT('',(11.9,-23.6215825028136,29.784615828692));
#69833=CARTESIAN_POINT('',(12.6,-23.315164725566,30.0417308725666));
#69834=CARTESIAN_POINT('',(12.6,-23.315164725566,30.0417308725666));
#69835=CARTESIAN_POINT('',(13.2,-23.1619558369422,30.170288394504));
#69836=CARTESIAN_POINT('',(13.2,-23.1619558369422,30.170288394504));
#69837=CARTESIAN_POINT('',(21.8,-23.1619558369422,30.170288394504));
#69838=CARTESIAN_POINT('',(21.8,-23.1619558369422,30.170288394504));
#69839=CARTESIAN_POINT('',(22.4,-23.315164725566,30.0417308725666));
#69840=CARTESIAN_POINT('',(22.4,-23.315164725566,30.0417308725666));
#69841=CARTESIAN_POINT('',(23.1,-23.6215825028136,29.784615828692));
#69842=CARTESIAN_POINT('',(23.1,-23.6215825028136,29.784615828692));
#69843=CARTESIAN_POINT('',(24.1,-23.8513958357493,29.5917795457861));
#69844=CARTESIAN_POINT('',(24.1,-23.8513958357493,29.5917795457861));
#69845=CARTESIAN_POINT('',(30.5,-23.5449780585017,29.8488945896607));
#69846=CARTESIAN_POINT('',(30.5,-23.5449780585017,29.8488945896607));
#69847=CARTESIAN_POINT('',(30.5,-23.1619558369422,30.170288394504));
#69848=CARTESIAN_POINT('',(30.5,-23.1619558369422,30.170288394504));
#69849=CARTESIAN_POINT('',(33.1,-23.1619558369422,30.170288394504));
#69850=CARTESIAN_POINT('',(33.1,-23.1619558369422,30.170288394504));
#69851=CARTESIAN_POINT('',(35.,-24.4259291680885,29.1096888385212));
#69852=CARTESIAN_POINT('Origin',(35.,-24.4259291680885,29.1096888385212));
#69853=CARTESIAN_POINT('',(35.,-28.156475035514,32.1800738014028));
#69854=CARTESIAN_POINT('',(35.,5.49679094461694,4.48212141338921));
#69855=CARTESIAN_POINT('',(34.8617922858584,-28.2484175959528,32.1029248328492));
#69856=CARTESIAN_POINT('',(33.5377160618333,-29.129258140991,31.3638118563816));
#69857=CARTESIAN_POINT('',(34.4,-28.1860830985703,31.5410006112756));
#69858=CARTESIAN_POINT('Ctrl Pts',(34.4,-28.1860830985703,31.5410006112756));
#69859=CARTESIAN_POINT('Ctrl Pts',(34.6297825290996,-28.2175888910031,31.8210099935449));
#69860=CARTESIAN_POINT('Ctrl Pts',(34.8617922858584,-28.2484175959528,32.1029248328492));
#69861=CARTESIAN_POINT('',(33.322645308031,-28.872052684018,30.9143101784803));
#69862=CARTESIAN_POINT('Origin',(26.8550245390365,0.,0.));
#69863=CARTESIAN_POINT('',(33.0966075166785,-25.6414155514355,28.0054314386442));
#69864=CARTESIAN_POINT('Origin',(17.5,-29.1096888385212,24.4259291680885));
#69865=CARTESIAN_POINT('',(33.1,-30.1702883945039,23.1619558369422));
#69866=CARTESIAN_POINT('',(33.1,-30.1702883945039,23.1619558369422));
#69867=CARTESIAN_POINT('',(30.5,-30.1702883945039,23.1619558369422));
#69868=CARTESIAN_POINT('',(30.5,-30.1702883945039,23.1619558369422));
#69869=CARTESIAN_POINT('',(30.5,-29.8488945896607,23.5449780585017));
#69870=CARTESIAN_POINT('',(30.5,-29.8488945896607,23.5449780585017));
#69871=CARTESIAN_POINT('',(24.1,-29.5917795457861,23.8513958357493));
#69872=CARTESIAN_POINT('',(24.1,-29.5917795457861,23.8513958357493));
#69873=CARTESIAN_POINT('',(23.1,-29.784615828692,23.6215825028136));
#69874=CARTESIAN_POINT('',(23.1,-29.784615828692,23.6215825028136));
#69875=CARTESIAN_POINT('',(22.4,-30.0417308725666,23.315164725566));
#69876=CARTESIAN_POINT('',(22.4,-30.0417308725666,23.315164725566));
#69877=CARTESIAN_POINT('',(21.8,-30.1702883945039,23.1619558369422));
#69878=CARTESIAN_POINT('',(21.8,-30.1702883945039,23.1619558369422));
#69879=CARTESIAN_POINT('',(13.2,-30.1702883945039,23.1619558369422));
#69880=CARTESIAN_POINT('',(13.2,-30.1702883945039,23.1619558369422));
#69881=CARTESIAN_POINT('',(12.6,-30.0417308725666,23.315164725566));
#69882=CARTESIAN_POINT('',(12.6,-30.0417308725666,23.315164725566));
#69883=CARTESIAN_POINT('',(11.9,-29.784615828692,23.6215825028136));
#69884=CARTESIAN_POINT('',(11.9,-29.784615828692,23.6215825028136));
#69885=CARTESIAN_POINT('',(10.9,-29.5917795457861,23.8513958357493));
#69886=CARTESIAN_POINT('',(10.9,-29.5917795457861,23.8513958357493));
#69887=CARTESIAN_POINT('',(4.5,-29.8488945896607,23.5449780585017));
#69888=CARTESIAN_POINT('',(4.5,-29.8488945896607,23.5449780585017));
#69889=CARTESIAN_POINT('',(4.5,-30.1702883945039,23.1619558369422));
#69890=CARTESIAN_POINT('',(4.5,-30.1702883945039,23.1619558369422));
#69891=CARTESIAN_POINT('',(1.9,-30.1702883945039,23.1619558369422));
#69892=CARTESIAN_POINT('',(1.9,-30.1702883945039,23.1619558369422));
#69893=CARTESIAN_POINT('',(1.57538060255632,-29.989082505666,23.3779086059641));
#69894=CARTESIAN_POINT('',(0.,-29.1096888385212,24.4259291680885));
#69895=CARTESIAN_POINT('',(1.57538060255632,-28.2302951713763,25.4739497302129));
#69896=CARTESIAN_POINT('Ctrl Pts',(1.57538060255632,-29.989082505666,23.3779086059641));
#69897=CARTESIAN_POINT('Ctrl Pts',(1.62460345738085,-29.1096888385011,24.4259291681124));
#69898=CARTESIAN_POINT('Ctrl Pts',(1.57538060255632,-28.2302951713763,25.4739497302129));
#69899=CARTESIAN_POINT('',(1.9,-28.0490892825384,25.6899024992348));
#69900=CARTESIAN_POINT('',(1.9,-28.0490892825384,25.6899024992348));
#69901=CARTESIAN_POINT('',(4.5,-28.0490892825384,25.6899024992348));
#69902=CARTESIAN_POINT('',(4.5,-28.0490892825384,25.6899024992348));
#69903=CARTESIAN_POINT('',(4.5,-28.3704830873816,25.3068802776753));
#69904=CARTESIAN_POINT('',(4.5,-28.3704830873816,25.3068802776753));
#69905=CARTESIAN_POINT('',(10.9,-28.6275981312563,25.0004625004277));
#69906=CARTESIAN_POINT('',(10.9,-28.6275981312563,25.0004625004277));
#69907=CARTESIAN_POINT('',(11.9,-28.4347618483503,25.2302758333634));
#69908=CARTESIAN_POINT('',(11.9,-28.4347618483503,25.2302758333634));
#69909=CARTESIAN_POINT('',(12.6,-28.1776468044757,25.536693610611));
#69910=CARTESIAN_POINT('',(12.6,-28.1776468044757,25.536693610611));
#69911=CARTESIAN_POINT('',(13.2,-28.0490892825384,25.6899024992348));
#69912=CARTESIAN_POINT('',(13.2,-28.0490892825384,25.6899024992348));
#69913=CARTESIAN_POINT('',(21.8,-28.0490892825384,25.6899024992348));
#69914=CARTESIAN_POINT('',(21.8,-28.0490892825384,25.6899024992348));
#69915=CARTESIAN_POINT('',(22.4,-28.1776468044757,25.536693610611));
#69916=CARTESIAN_POINT('',(22.4,-28.1776468044757,25.536693610611));
#69917=CARTESIAN_POINT('',(23.1,-28.4347618483503,25.2302758333634));
#69918=CARTESIAN_POINT('',(23.1,-28.4347618483503,25.2302758333634));
#69919=CARTESIAN_POINT('',(24.1,-28.6275981312563,25.0004625004277));
#69920=CARTESIAN_POINT('',(24.1,-28.6275981312563,25.0004625004277));
#69921=CARTESIAN_POINT('',(30.5,-28.3704830873816,25.3068802776753));
#69922=CARTESIAN_POINT('',(30.5,-28.3704830873816,25.3068802776753));
#69923=CARTESIAN_POINT('',(30.5,-28.0490892825384,25.6899024992348));
#69924=CARTESIAN_POINT('',(30.5,-28.0490892825384,25.6899024992348));
#69925=CARTESIAN_POINT('',(33.1,-28.0490892825384,25.6899024992348));
#69926=CARTESIAN_POINT('',(33.1,-28.0490892825384,25.6899024992348));
#69927=CARTESIAN_POINT('',(35.,-29.1096888385212,24.4259291680885));
#69928=CARTESIAN_POINT('Origin',(35.,-29.1096888385212,24.4259291680885));
#69929=CARTESIAN_POINT('',(35.,-33.3167260852698,26.8018655926852));
#69930=CARTESIAN_POINT('',(35.,6.86764292749649,4.10762723987466));
#69931=CARTESIAN_POINT('',(34.8617922858584,-33.3938750538235,26.7099230322464));
#69932=CARTESIAN_POINT('',(33.5377160618333,-34.132988030291,25.8290824872081));
#69933=CARTESIAN_POINT('',(34.4,-33.234910440458,26.1673599741116));
#69934=CARTESIAN_POINT('Ctrl Pts',(34.4,-33.234910440458,26.1673599741116));
#69935=CARTESIAN_POINT('Ctrl Pts',(34.6297825291036,-33.3145607080726,26.4376444612493));
#69936=CARTESIAN_POINT('Ctrl Pts',(34.8617922858584,-33.3938750538235,26.7099230322464));
#69937=CARTESIAN_POINT('',(33.322645308031,-33.8016349549212,25.4310730087083));
#69938=CARTESIAN_POINT('Origin',(26.8550245390365,0.,0.));
#69939=CARTESIAN_POINT('',(33.0966075166785,-30.1149569673582,23.1273809239214));
#69940=CARTESIAN_POINT('Origin',(17.5,-32.9089653438087,19.));
#69941=CARTESIAN_POINT('',(33.1,-33.7339653438087,17.5710580837557));
#69942=CARTESIAN_POINT('',(33.1,-33.7339653438087,17.5710580837557));
#69943=CARTESIAN_POINT('',(30.5,-33.7339653438087,17.5710580837557));
#69944=CARTESIAN_POINT('',(30.5,-33.7339653438087,17.5710580837557));
#69945=CARTESIAN_POINT('',(30.5,-33.4839653438087,18.0040707856479));
#69946=CARTESIAN_POINT('',(30.5,-33.4839653438087,18.0040707856479));
#69947=CARTESIAN_POINT('',(24.1,-33.2839653438087,18.3504809471617));
#69948=CARTESIAN_POINT('',(24.1,-33.2839653438087,18.3504809471617));
#69949=CARTESIAN_POINT('',(23.1,-33.4339653438087,18.0906733260263));
#69950=CARTESIAN_POINT('',(23.1,-33.4339653438087,18.0906733260263));
#69951=CARTESIAN_POINT('',(22.4,-33.6339653438087,17.7442631645126));
#69952=CARTESIAN_POINT('',(22.4,-33.6339653438087,17.7442631645126));
#69953=CARTESIAN_POINT('',(21.8,-33.7339653438087,17.5710580837557));
#69954=CARTESIAN_POINT('',(21.8,-33.7339653438087,17.5710580837557));
#69955=CARTESIAN_POINT('',(13.2,-33.7339653438087,17.5710580837557));
#69956=CARTESIAN_POINT('',(13.2,-33.7339653438087,17.5710580837557));
#69957=CARTESIAN_POINT('',(12.6,-33.6339653438087,17.7442631645126));
#69958=CARTESIAN_POINT('',(12.6,-33.6339653438087,17.7442631645126));
#69959=CARTESIAN_POINT('',(11.9,-33.4339653438087,18.0906733260263));
#69960=CARTESIAN_POINT('',(11.9,-33.4339653438087,18.0906733260263));
#69961=CARTESIAN_POINT('',(10.9,-33.2839653438087,18.3504809471617));
#69962=CARTESIAN_POINT('',(10.9,-33.2839653438087,18.3504809471617));
#69963=CARTESIAN_POINT('',(4.5,-33.4839653438087,18.0040707856479));
#69964=CARTESIAN_POINT('',(4.5,-33.4839653438087,18.0040707856479));
#69965=CARTESIAN_POINT('',(4.5,-33.7339653438087,17.5710580837557));
#69966=CARTESIAN_POINT('',(4.5,-33.7339653438087,17.5710580837557));
#69967=CARTESIAN_POINT('',(1.9,-33.7339653438087,17.5710580837557));
#69968=CARTESIAN_POINT('',(1.9,-33.7339653438087,17.5710580837557));
#69969=CARTESIAN_POINT('',(1.57538060255632,-33.5930121843923,17.8151961173521));
#69970=CARTESIAN_POINT('',(0.,-32.9089653438087,19.));
#69971=CARTESIAN_POINT('',(1.57538060255632,-32.224918503225,20.1848038826479));
#69972=CARTESIAN_POINT('Ctrl Pts',(1.57538060255632,-33.5930121843923,17.8151961173521));
#69973=CARTESIAN_POINT('Ctrl Pts',(1.62460345738084,-32.9089653437931,19.000000000027));
#69974=CARTESIAN_POINT('Ctrl Pts',(1.57538060255632,-32.224918503225,20.1848038826479));
#69975=CARTESIAN_POINT('',(1.9,-32.0839653438087,20.4289419162443));
#69976=CARTESIAN_POINT('',(1.9,-32.0839653438087,20.4289419162443));
#69977=CARTESIAN_POINT('',(4.5,-32.0839653438087,20.4289419162443));
#69978=CARTESIAN_POINT('',(4.5,-32.0839653438087,20.4289419162443));
#69979=CARTESIAN_POINT('',(4.5,-32.3339653438087,19.9959292143521));
#69980=CARTESIAN_POINT('',(4.5,-32.3339653438087,19.9959292143521));
#69981=CARTESIAN_POINT('',(10.9,-32.5339653438087,19.6495190528383));
#69982=CARTESIAN_POINT('',(10.9,-32.5339653438087,19.6495190528383));
#69983=CARTESIAN_POINT('',(11.9,-32.3839653438087,19.9093266739737));
#69984=CARTESIAN_POINT('',(11.9,-32.3839653438087,19.9093266739737));
#69985=CARTESIAN_POINT('',(12.6,-32.1839653438087,20.2557368354874));
#69986=CARTESIAN_POINT('',(12.6,-32.1839653438087,20.2557368354874));
#69987=CARTESIAN_POINT('',(13.2,-32.0839653438087,20.4289419162443));
#69988=CARTESIAN_POINT('',(13.2,-32.0839653438087,20.4289419162443));
#69989=CARTESIAN_POINT('',(21.8,-32.0839653438087,20.4289419162443));
#69990=CARTESIAN_POINT('',(21.8,-32.0839653438087,20.4289419162443));
#69991=CARTESIAN_POINT('',(22.4,-32.1839653438087,20.2557368354874));
#69992=CARTESIAN_POINT('',(22.4,-32.1839653438087,20.2557368354874));
#69993=CARTESIAN_POINT('',(23.1,-32.3839653438087,19.9093266739737));
#69994=CARTESIAN_POINT('',(23.1,-32.3839653438087,19.9093266739737));
#69995=CARTESIAN_POINT('',(24.1,-32.5339653438087,19.6495190528383));
#69996=CARTESIAN_POINT('',(24.1,-32.5339653438087,19.6495190528383));
#69997=CARTESIAN_POINT('',(30.5,-32.3339653438087,19.9959292143521));
#69998=CARTESIAN_POINT('',(30.5,-32.3339653438087,19.9959292143521));
#69999=CARTESIAN_POINT('',(30.5,-32.0839653438087,20.4289419162443));
#70000=CARTESIAN_POINT('',(30.5,-32.0839653438087,20.4289419162443));
#70001=CARTESIAN_POINT('',(33.1,-32.0839653438087,20.4289419162443));
#70002=CARTESIAN_POINT('',(33.1,-32.0839653438087,20.4289419162443));
#70003=CARTESIAN_POINT('',(35.,-32.9089653438087,19.));
#70004=CARTESIAN_POINT('Origin',(35.,-32.9089653438087,19.));
#70005=CARTESIAN_POINT('',(35.,-37.4646652720015,20.6092962603321));
#70006=CARTESIAN_POINT('',(35.,7.81913363821562,4.6128414041074));
#70007=CARTESIAN_POINT('',(34.8617922858584,-37.5246765162999,20.5053537361819));
#70008=CARTESIAN_POINT('',(33.5377160618333,-38.099604350416,19.5095495168072));
#70009=CARTESIAN_POINT('',(34.4,-37.2739118462885,19.9986373454573));
#70010=CARTESIAN_POINT('Ctrl Pts',(34.4,-37.2739118462884,19.9986373454573));
#70011=CARTESIAN_POINT('Ctrl Pts',(34.6297825291036,-37.399286456008,20.2509844800875));
#70012=CARTESIAN_POINT('Ctrl Pts',(34.8617922858584,-37.5246765162998,20.5053537361819));
#70013=CARTESIAN_POINT('',(33.322645308031,-37.7041716521717,19.1751255543105));
#70014=CARTESIAN_POINT('Origin',(26.8550245390365,0.,0.));
#70015=CARTESIAN_POINT('',(33.0966075166785,-33.6734706547313,17.5466166428447));
#70016=CARTESIAN_POINT('Origin',(17.5,-35.7083195898645,12.9967654463754));
#70017=CARTESIAN_POINT('',(33.1,-36.2726528263519,11.4462726220787));
#70018=CARTESIAN_POINT('',(33.1,-36.2726528263519,11.4462726220787));
#70019=CARTESIAN_POINT('',(30.5,-36.2726528263519,11.4462726220787));
#70020=CARTESIAN_POINT('',(30.5,-36.2726528263519,11.4462726220787));
#70021=CARTESIAN_POINT('',(30.5,-36.101642754689,11.9161189324716));
#70022=CARTESIAN_POINT('',(30.5,-36.101642754689,11.9161189324716));
#70023=CARTESIAN_POINT('',(24.1,-35.9648346973588,12.291995980786));
#70024=CARTESIAN_POINT('',(24.1,-35.9648346973588,12.291995980786));
#70025=CARTESIAN_POINT('',(23.1,-36.0674407403565,12.0100881945502));
#70026=CARTESIAN_POINT('',(23.1,-36.0674407403565,12.0100881945502));
#70027=CARTESIAN_POINT('',(22.4,-36.2042487976867,11.6342111462359));
#70028=CARTESIAN_POINT('',(22.4,-36.2042487976867,11.6342111462359));
#70029=CARTESIAN_POINT('',(21.8,-36.2726528263519,11.4462726220787));
#70030=CARTESIAN_POINT('',(21.8,-36.2726528263519,11.4462726220787));
#70031=CARTESIAN_POINT('',(13.2,-36.2726528263519,11.4462726220787));
#70032=CARTESIAN_POINT('',(13.2,-36.2726528263519,11.4462726220787));
#70033=CARTESIAN_POINT('',(12.6,-36.2042487976867,11.6342111462359));
#70034=CARTESIAN_POINT('',(12.6,-36.2042487976867,11.6342111462359));
#70035=CARTESIAN_POINT('',(11.9,-36.0674407403565,12.0100881945502));
#70036=CARTESIAN_POINT('',(11.9,-36.0674407403565,12.0100881945502));
#70037=CARTESIAN_POINT('',(10.9,-35.9648346973588,12.291995980786));
#70038=CARTESIAN_POINT('',(10.9,-35.9648346973588,12.291995980786));
#70039=CARTESIAN_POINT('',(4.5,-36.101642754689,11.9161189324716));
#70040=CARTESIAN_POINT('',(4.5,-36.101642754689,11.9161189324716));
#70041=CARTESIAN_POINT('',(4.5,-36.2726528263519,11.4462726220787));
#70042=CARTESIAN_POINT('',(4.5,-36.2726528263519,11.4462726220787));
#70043=CARTESIAN_POINT('',(1.9,-36.2726528263519,11.4462726220787));
#70044=CARTESIAN_POINT('',(1.9,-36.2726528263519,11.4462726220787));
#70045=CARTESIAN_POINT('',(1.57538060255632,-36.1762351867803,11.7111779096386));
#70046=CARTESIAN_POINT('',(0.,-35.7083195898645,12.9967654463754));
#70047=CARTESIAN_POINT('',(1.57538060255633,-35.2404039929487,14.2823529831122));
#70048=CARTESIAN_POINT('Ctrl Pts',(1.57538060255632,-36.1762351867803,11.7111779096386));
#70049=CARTESIAN_POINT('Ctrl Pts',(1.62460345738085,-35.7083195898539,12.9967654464047));
#70050=CARTESIAN_POINT('Ctrl Pts',(1.57538060255633,-35.2404039929487,14.2823529831122));
#70051=CARTESIAN_POINT('',(1.9,-35.1439863533772,14.5472582706722));
#70052=CARTESIAN_POINT('',(1.9,-35.1439863533772,14.5472582706722));
#70053=CARTESIAN_POINT('',(4.5,-35.1439863533772,14.5472582706722));
#70054=CARTESIAN_POINT('',(4.5,-35.1439863533772,14.5472582706722));
#70055=CARTESIAN_POINT('',(4.5,-35.31499642504,14.0774119602792));
#70056=CARTESIAN_POINT('',(4.5,-35.31499642504,14.0774119602792));
#70057=CARTESIAN_POINT('',(10.9,-35.4518044823703,13.7015349119648));
#70058=CARTESIAN_POINT('',(10.9,-35.4518044823703,13.7015349119648));
#70059=CARTESIAN_POINT('',(11.9,-35.3491984393726,13.9834426982006));
#70060=CARTESIAN_POINT('',(11.9,-35.3491984393726,13.9834426982006));
#70061=CARTESIAN_POINT('',(12.6,-35.2123903820423,14.359319746515));
#70062=CARTESIAN_POINT('',(12.6,-35.2123903820423,14.359319746515));
#70063=CARTESIAN_POINT('',(13.2,-35.1439863533772,14.5472582706722));
#70064=CARTESIAN_POINT('',(13.2,-35.1439863533772,14.5472582706722));
#70065=CARTESIAN_POINT('',(21.8,-35.1439863533772,14.5472582706722));
#70066=CARTESIAN_POINT('',(21.8,-35.1439863533772,14.5472582706722));
#70067=CARTESIAN_POINT('',(22.4,-35.2123903820423,14.359319746515));
#70068=CARTESIAN_POINT('',(22.4,-35.2123903820423,14.359319746515));
#70069=CARTESIAN_POINT('',(23.1,-35.3491984393726,13.9834426982006));
#70070=CARTESIAN_POINT('',(23.1,-35.3491984393726,13.9834426982006));
#70071=CARTESIAN_POINT('',(24.1,-35.4518044823703,13.7015349119648));
#70072=CARTESIAN_POINT('',(24.1,-35.4518044823703,13.7015349119648));
#70073=CARTESIAN_POINT('',(30.5,-35.31499642504,14.0774119602792));
#70074=CARTESIAN_POINT('',(30.5,-35.31499642504,14.0774119602792));
#70075=CARTESIAN_POINT('',(30.5,-35.1439863533772,14.5472582706722));
#70076=CARTESIAN_POINT('',(30.5,-35.1439863533772,14.5472582706722));
#70077=CARTESIAN_POINT('',(33.1,-35.1439863533772,14.5472582706722));
#70078=CARTESIAN_POINT('',(33.1,-35.1439863533772,14.5472582706722));
#70079=CARTESIAN_POINT('',(35.,-35.7083195898645,12.9967654463754));
#70080=CARTESIAN_POINT('Origin',(35.,-35.7083195898645,12.9967654463754));
#70081=CARTESIAN_POINT('',(35.,-40.4742595624789,13.790523889916));
#70082=CARTESIAN_POINT('',(35.,8.01531519808922,5.71467534565107));
#70083=CARTESIAN_POINT('',(34.8617922858584,-40.515309671231,13.6777396430533));
#70084=CARTESIAN_POINT('',(33.5377160618333,-40.9085834716837,12.5972287566465));
#70085=CARTESIAN_POINT('',(34.4,-40.1803643021789,13.22226624086));
#70086=CARTESIAN_POINT('Ctrl Pts',(34.4,-40.1803643021789,13.22226624086));
#70087=CARTESIAN_POINT('Ctrl Pts',(34.6297825291021,-40.3476538099285,13.4490085829893));
#70088=CARTESIAN_POINT('Ctrl Pts',(34.8617922858584,-40.515309671231,13.6777396430533));
#70089=CARTESIAN_POINT('',(33.322645308031,-40.4610861730024,12.3365516130268));
#70090=CARTESIAN_POINT('Origin',(26.8550245390365,0.,0.));
#70091=CARTESIAN_POINT('',(33.0966075166785,-36.2088329758587,11.4327072940915));
#70092=CARTESIAN_POINT('Origin',(17.5,-37.4226946144639,6.59863075134337));
#70093=CARTESIAN_POINT('',(33.1,-37.7092141076143,4.97369795887322));
#70094=CARTESIAN_POINT('',(33.1,-37.7092141076143,4.97369795887322));
#70095=CARTESIAN_POINT('',(30.5,-37.7092141076143,4.97369795887322));
#70096=CARTESIAN_POINT('',(30.5,-37.7092141076143,4.97369795887322));
#70097=CARTESIAN_POINT('',(30.5,-37.6223900187809,5.46610183537933));
#70098=CARTESIAN_POINT('',(30.5,-37.6223900187809,5.46610183537933));
#70099=CARTESIAN_POINT('',(24.1,-37.5529307477141,5.86002493658421));
#70100=CARTESIAN_POINT('',(24.1,-37.5529307477141,5.86002493658421));
#70101=CARTESIAN_POINT('',(23.1,-37.6050252010142,5.56458261068055));
#70102=CARTESIAN_POINT('',(23.1,-37.6050252010142,5.56458261068055));
#70103=CARTESIAN_POINT('',(22.4,-37.674484472081,5.17065950947566));
#70104=CARTESIAN_POINT('',(22.4,-37.674484472081,5.17065950947566));
#70105=CARTESIAN_POINT('',(21.8,-37.7092141076143,4.97369795887322));
#70106=CARTESIAN_POINT('',(21.8,-37.7092141076143,4.97369795887322));
#70107=CARTESIAN_POINT('',(13.2,-37.7092141076143,4.97369795887322));
#70108=CARTESIAN_POINT('',(13.2,-37.7092141076143,4.97369795887322));
#70109=CARTESIAN_POINT('',(12.6,-37.674484472081,5.17065950947566));
#70110=CARTESIAN_POINT('',(12.6,-37.674484472081,5.17065950947566));
#70111=CARTESIAN_POINT('',(11.9,-37.6050252010142,5.56458261068055));
#70112=CARTESIAN_POINT('',(11.9,-37.6050252010142,5.56458261068055));
#70113=CARTESIAN_POINT('',(10.9,-37.5529307477141,5.86002493658421));
#70114=CARTESIAN_POINT('',(10.9,-37.5529307477141,5.86002493658421));
#70115=CARTESIAN_POINT('',(4.5,-37.6223900187809,5.46610183537933));
#70116=CARTESIAN_POINT('',(4.5,-37.6223900187809,5.46610183537933));
#70117=CARTESIAN_POINT('',(4.5,-37.7092141076143,4.97369795887322));
#70118=CARTESIAN_POINT('',(4.5,-37.7092141076143,4.97369795887322));
#70119=CARTESIAN_POINT('',(1.9,-37.7092141076143,4.97369795887322));
#70120=CARTESIAN_POINT('',(1.9,-37.7092141076143,4.97369795887322));
#70121=CARTESIAN_POINT('',(1.57538060255632,-37.6602615890763,5.25132148728276));
#70122=CARTESIAN_POINT('',(0.,-37.4226946144639,6.59863075134337));
#70123=CARTESIAN_POINT('',(1.57538060255632,-37.1851276398516,7.94594001540397));
#70124=CARTESIAN_POINT('Ctrl Pts',(1.57538060255632,-37.6602615890763,5.25132148728276));
#70125=CARTESIAN_POINT('Ctrl Pts',(1.62460345738085,-37.4226946144585,6.59863075137407));
#70126=CARTESIAN_POINT('Ctrl Pts',(1.57538060255632,-37.1851276398516,7.94594001540397));
#70127=CARTESIAN_POINT('',(1.9,-37.1361751213135,8.22356354381351));
#70128=CARTESIAN_POINT('',(1.9,-37.1361751213135,8.22356354381351));
#70129=CARTESIAN_POINT('',(4.5,-37.1361751213135,8.22356354381351));
#70130=CARTESIAN_POINT('',(4.5,-37.1361751213135,8.22356354381351));
#70131=CARTESIAN_POINT('',(4.5,-37.2229992101469,7.73115966730741));
#70132=CARTESIAN_POINT('',(4.5,-37.2229992101469,7.73115966730741));
#70133=CARTESIAN_POINT('',(10.9,-37.2924584812137,7.33723656610252));
#70134=CARTESIAN_POINT('',(10.9,-37.2924584812137,7.33723656610252));
#70135=CARTESIAN_POINT('',(11.9,-37.2403640279136,7.63267889200618));
#70136=CARTESIAN_POINT('',(11.9,-37.2403640279136,7.63267889200618));
#70137=CARTESIAN_POINT('',(12.6,-37.1709047568469,8.02660199321107));
#70138=CARTESIAN_POINT('',(12.6,-37.1709047568469,8.02660199321107));
#70139=CARTESIAN_POINT('',(13.2,-37.1361751213135,8.22356354381351));
#70140=CARTESIAN_POINT('',(13.2,-37.1361751213135,8.22356354381351));
#70141=CARTESIAN_POINT('',(21.8,-37.1361751213135,8.22356354381351));
#70142=CARTESIAN_POINT('',(21.8,-37.1361751213135,8.22356354381351));
#70143=CARTESIAN_POINT('',(22.4,-37.1709047568469,8.02660199321107));
#70144=CARTESIAN_POINT('',(22.4,-37.1709047568469,8.02660199321107));
#70145=CARTESIAN_POINT('',(23.1,-37.2403640279136,7.63267889200618));
#70146=CARTESIAN_POINT('',(23.1,-37.2403640279136,7.63267889200618));
#70147=CARTESIAN_POINT('',(24.1,-37.2924584812137,7.33723656610252));
#70148=CARTESIAN_POINT('',(24.1,-37.2924584812137,7.33723656610252));
#70149=CARTESIAN_POINT('',(30.5,-37.2229992101469,7.73115966730741));
#70150=CARTESIAN_POINT('',(30.5,-37.2229992101469,7.73115966730741));
#70151=CARTESIAN_POINT('',(30.5,-37.1361751213135,8.22356354381351));
#70152=CARTESIAN_POINT('',(30.5,-37.1361751213135,8.22356354381351));
#70153=CARTESIAN_POINT('',(33.1,-37.1361751213135,8.22356354381351));
#70154=CARTESIAN_POINT('',(33.1,-37.1361751213135,8.22356354381351));
#70155=CARTESIAN_POINT('',(35.,-37.4226946144639,6.59863075134337));
#70156=CARTESIAN_POINT('Origin',(35.,-37.4226946144639,6.59863075134337));
#70157=CARTESIAN_POINT('',(35.,-42.2540639571139,6.55273342944654));
#70158=CARTESIAN_POINT('',(35.,7.25327777991845,7.02304613766821));
#70159=CARTESIAN_POINT('',(34.8617922858584,-42.2749056435377,6.43453435214071));
#70160=CARTESIAN_POINT('',(33.5377160618333,-42.4745759849063,5.30214757522048));
#70161=CARTESIAN_POINT('',(34.4,-41.8659567209931,6.04414326732377));
#70162=CARTESIAN_POINT('Ctrl Pts',(34.4,-41.8659567209931,6.04414326732377));
#70163=CARTESIAN_POINT('Ctrl Pts',(34.6297825291009,-42.0700781197321,6.23839136562435));
#70164=CARTESIAN_POINT('Ctrl Pts',(34.8617922858584,-42.2749056435377,6.43453435214071));
#70165=CARTESIAN_POINT('',(33.3226453080309,-41.9886110647639,5.12313779357753));
#70166=CARTESIAN_POINT('Origin',(26.8550245390365,0.,0.));
#70167=CARTESIAN_POINT('',(33.0966075166785,-37.6440082295681,4.97142091943646));
#70168=CARTESIAN_POINT('Origin',(17.5,-38.,4.65365783675994E-15));
#70169=CARTESIAN_POINT('',(33.1,-38.,-1.65));
#70170=CARTESIAN_POINT('',(33.1,-38.,-1.65));
#70171=CARTESIAN_POINT('',(30.5,-38.,-1.65));
#70172=CARTESIAN_POINT('',(30.5,-38.,-1.65));
#70173=CARTESIAN_POINT('',(30.5,-38.,-1.15));
#70174=CARTESIAN_POINT('',(30.5,-38.,-1.15));
#70175=CARTESIAN_POINT('',(24.1,-38.,-0.749999999999995));
#70176=CARTESIAN_POINT('',(24.1,-38.,-0.749999999999995));
#70177=CARTESIAN_POINT('',(23.1,-38.,-1.05));
#70178=CARTESIAN_POINT('',(23.1,-38.,-1.05));
#70179=CARTESIAN_POINT('',(22.4,-38.,-1.45));
#70180=CARTESIAN_POINT('',(22.4,-38.,-1.45));
#70181=CARTESIAN_POINT('',(21.8,-38.,-1.65));
#70182=CARTESIAN_POINT('',(21.8,-38.,-1.65));
#70183=CARTESIAN_POINT('',(13.2,-38.,-1.65));
#70184=CARTESIAN_POINT('',(13.2,-38.,-1.65));
#70185=CARTESIAN_POINT('',(12.6,-38.,-1.45));
#70186=CARTESIAN_POINT('',(12.6,-38.,-1.45));
#70187=CARTESIAN_POINT('',(11.9,-38.,-1.05));
#70188=CARTESIAN_POINT('',(11.9,-38.,-1.05));
#70189=CARTESIAN_POINT('',(10.9,-38.,-0.749999999999995));
#70190=CARTESIAN_POINT('',(10.9,-38.,-0.749999999999995));
#70191=CARTESIAN_POINT('',(4.5,-38.,-1.15));
#70192=CARTESIAN_POINT('',(4.5,-38.,-1.15));
#70193=CARTESIAN_POINT('',(4.5,-38.,-1.65));
#70194=CARTESIAN_POINT('',(4.5,-38.,-1.65));
#70195=CARTESIAN_POINT('',(1.9,-38.,-1.65));
#70196=CARTESIAN_POINT('',(1.9,-38.,-1.65));
#70197=CARTESIAN_POINT('',(1.57538060255632,-38.,-1.36809368116733));
#70198=CARTESIAN_POINT('',(0.,-38.,4.65365783675994E-15));
#70199=CARTESIAN_POINT('',(1.57538060255633,-38.,1.36809368116734));
#70200=CARTESIAN_POINT('Ctrl Pts',(1.57538060255632,-38.,-1.36809368116733));
#70201=CARTESIAN_POINT('Ctrl Pts',(1.62460345738085,-38.,3.11853320944522E-11));
#70202=CARTESIAN_POINT('Ctrl Pts',(1.57538060255633,-38.,1.36809368116734));
#70203=CARTESIAN_POINT('',(1.9,-38.,1.65));
#70204=CARTESIAN_POINT('',(1.9,-38.,1.65));
#70205=CARTESIAN_POINT('',(4.5,-38.,1.65));
#70206=CARTESIAN_POINT('',(4.5,-38.,1.65));
#70207=CARTESIAN_POINT('',(4.5,-38.,1.15));
#70208=CARTESIAN_POINT('',(4.5,-38.,1.15));
#70209=CARTESIAN_POINT('',(10.9,-38.,0.750000000000005));
#70210=CARTESIAN_POINT('',(10.9,-38.,0.750000000000005));
#70211=CARTESIAN_POINT('',(11.9,-38.,1.05));
#70212=CARTESIAN_POINT('',(11.9,-38.,1.05));
#70213=CARTESIAN_POINT('',(12.6,-38.,1.45));
#70214=CARTESIAN_POINT('',(12.6,-38.,1.45));
#70215=CARTESIAN_POINT('',(13.2,-38.,1.65));
#70216=CARTESIAN_POINT('',(13.2,-38.,1.65));
#70217=CARTESIAN_POINT('',(21.8,-38.,1.65));
#70218=CARTESIAN_POINT('',(21.8,-38.,1.65));
#70219=CARTESIAN_POINT('',(22.4,-38.,1.45));
#70220=CARTESIAN_POINT('',(22.4,-38.,1.45));
#70221=CARTESIAN_POINT('',(23.1,-38.,1.05));
#70222=CARTESIAN_POINT('',(23.1,-38.,1.05));
#70223=CARTESIAN_POINT('',(24.1,-38.,0.750000000000005));
#70224=CARTESIAN_POINT('',(24.1,-38.,0.750000000000005));
#70225=CARTESIAN_POINT('',(30.5,-38.,1.15));
#70226=CARTESIAN_POINT('',(30.5,-38.,1.15));
#70227=CARTESIAN_POINT('',(30.5,-38.,1.65));
#70228=CARTESIAN_POINT('',(30.5,-38.,1.65));
#70229=CARTESIAN_POINT('',(33.1,-38.,1.65));
#70230=CARTESIAN_POINT('',(33.1,-38.,1.65));
#70231=CARTESIAN_POINT('',(35.,-38.,4.65365783675994E-15));
#70232=CARTESIAN_POINT('Origin',(35.,-38.,4.65365783675994E-15));
#70233=CARTESIAN_POINT('',(35.,-42.75,-0.884158520433531));
#70234=CARTESIAN_POINT('',(35.,5.49306987041266,8.09574069594452));
#70235=CARTESIAN_POINT('',(34.8617922858584,-42.75,-1.0041810090302));
#70236=CARTESIAN_POINT('',(33.5377160618333,-42.75,-2.15403667726254));
#70237=CARTESIAN_POINT('',(34.4,-42.2794732300362,-1.31762794090604));
#70238=CARTESIAN_POINT('Ctrl Pts',(34.4,-42.2794732300361,-1.31762794090604));
#70239=CARTESIAN_POINT('Ctrl Pts',(34.6297825290972,-42.5142243943514,-1.16177621660812));
#70240=CARTESIAN_POINT('Ctrl Pts',(34.8617922858584,-42.75,-1.0041810090302));
#70241=CARTESIAN_POINT('',(33.3226453080309,-42.240333256585,-2.24593997529677));
#70242=CARTESIAN_POINT('Origin',(26.8550245390365,0.,0.));
#70243=CARTESIAN_POINT('',(33.0966075166785,-37.9353893420094,-1.64091956419533));
#70244=CARTESIAN_POINT('Origin',(17.5,-37.4226946144639,-6.59863075134334));
#70245=CARTESIAN_POINT('',(33.1,-37.1361751213135,-8.22356354381348));
#70246=CARTESIAN_POINT('',(33.1,-37.1361751213135,-8.22356354381348));
#70247=CARTESIAN_POINT('',(30.5,-37.1361751213135,-8.22356354381348));
#70248=CARTESIAN_POINT('',(30.5,-37.1361751213135,-8.22356354381348));
#70249=CARTESIAN_POINT('',(30.5,-37.2229992101469,-7.73115966730738));
#70250=CARTESIAN_POINT('',(30.5,-37.2229992101469,-7.73115966730738));
#70251=CARTESIAN_POINT('',(24.1,-37.2924584812137,-7.3372365661025));
#70252=CARTESIAN_POINT('',(24.1,-37.2924584812137,-7.3372365661025));
#70253=CARTESIAN_POINT('',(23.1,-37.2403640279136,-7.63267889200616));
#70254=CARTESIAN_POINT('',(23.1,-37.2403640279136,-7.63267889200616));
#70255=CARTESIAN_POINT('',(22.4,-37.1709047568469,-8.02660199321104));
#70256=CARTESIAN_POINT('',(22.4,-37.1709047568469,-8.02660199321104));
#70257=CARTESIAN_POINT('',(21.8,-37.1361751213135,-8.22356354381348));
#70258=CARTESIAN_POINT('',(21.8,-37.1361751213135,-8.22356354381348));
#70259=CARTESIAN_POINT('',(13.2,-37.1361751213135,-8.22356354381348));
#70260=CARTESIAN_POINT('',(13.2,-37.1361751213135,-8.22356354381348));
#70261=CARTESIAN_POINT('',(12.6,-37.1709047568469,-8.02660199321104));
#70262=CARTESIAN_POINT('',(12.6,-37.1709047568469,-8.02660199321104));
#70263=CARTESIAN_POINT('',(11.9,-37.2403640279136,-7.63267889200616));
#70264=CARTESIAN_POINT('',(11.9,-37.2403640279136,-7.63267889200616));
#70265=CARTESIAN_POINT('',(10.9,-37.2924584812137,-7.3372365661025));
#70266=CARTESIAN_POINT('',(10.9,-37.2924584812137,-7.3372365661025));
#70267=CARTESIAN_POINT('',(4.5,-37.2229992101469,-7.73115966730738));
#70268=CARTESIAN_POINT('',(4.5,-37.2229992101469,-7.73115966730738));
#70269=CARTESIAN_POINT('',(4.5,-37.1361751213135,-8.22356354381348));
#70270=CARTESIAN_POINT('',(4.5,-37.1361751213135,-8.22356354381348));
#70271=CARTESIAN_POINT('',(1.9,-37.1361751213135,-8.22356354381348));
#70272=CARTESIAN_POINT('',(1.9,-37.1361751213135,-8.22356354381348));
#70273=CARTESIAN_POINT('',(1.57538060255632,-37.1851276398516,-7.94594001540395));
#70274=CARTESIAN_POINT('',(0.,-37.4226946144639,-6.59863075134334));
#70275=CARTESIAN_POINT('',(1.57538060255633,-37.6602615890763,-5.25132148728274));
#70276=CARTESIAN_POINT('Ctrl Pts',(1.57538060255632,-37.1851276398516,-7.94594001540395));
#70277=CARTESIAN_POINT('Ctrl Pts',(1.62460345738085,-37.4226946144693,-6.59863075131264));
#70278=CARTESIAN_POINT('Ctrl Pts',(1.57538060255633,-37.6602615890763,-5.25132148728274));
#70279=CARTESIAN_POINT('',(1.9,-37.7092141076143,-4.9736979588732));
#70280=CARTESIAN_POINT('',(1.9,-37.7092141076143,-4.9736979588732));
#70281=CARTESIAN_POINT('',(4.5,-37.7092141076143,-4.9736979588732));
#70282=CARTESIAN_POINT('',(4.5,-37.7092141076143,-4.9736979588732));
#70283=CARTESIAN_POINT('',(4.5,-37.6223900187809,-5.4661018353793));
#70284=CARTESIAN_POINT('',(4.5,-37.6223900187809,-5.4661018353793));
#70285=CARTESIAN_POINT('',(10.9,-37.5529307477141,-5.86002493658419));
#70286=CARTESIAN_POINT('',(10.9,-37.5529307477141,-5.86002493658419));
#70287=CARTESIAN_POINT('',(11.9,-37.6050252010142,-5.56458261068052));
#70288=CARTESIAN_POINT('',(11.9,-37.6050252010142,-5.56458261068052));
#70289=CARTESIAN_POINT('',(12.6,-37.674484472081,-5.17065950947564));
#70290=CARTESIAN_POINT('',(12.6,-37.674484472081,-5.17065950947564));
#70291=CARTESIAN_POINT('',(13.2,-37.7092141076143,-4.9736979588732));
#70292=CARTESIAN_POINT('',(13.2,-37.7092141076143,-4.9736979588732));
#70293=CARTESIAN_POINT('',(21.8,-37.7092141076143,-4.9736979588732));
#70294=CARTESIAN_POINT('',(21.8,-37.7092141076143,-4.9736979588732));
#70295=CARTESIAN_POINT('',(22.4,-37.674484472081,-5.17065950947564));
#70296=CARTESIAN_POINT('',(22.4,-37.674484472081,-5.17065950947564));
#70297=CARTESIAN_POINT('',(23.1,-37.6050252010142,-5.56458261068052));
#70298=CARTESIAN_POINT('',(23.1,-37.6050252010142,-5.56458261068052));
#70299=CARTESIAN_POINT('',(24.1,-37.5529307477141,-5.86002493658419));
#70300=CARTESIAN_POINT('',(24.1,-37.5529307477141,-5.86002493658419));
#70301=CARTESIAN_POINT('',(30.5,-37.6223900187809,-5.4661018353793));
#70302=CARTESIAN_POINT('',(30.5,-37.6223900187809,-5.4661018353793));
#70303=CARTESIAN_POINT('',(30.5,-37.7092141076143,-4.9736979588732));
#70304=CARTESIAN_POINT('',(30.5,-37.7092141076143,-4.9736979588732));
#70305=CARTESIAN_POINT('',(33.1,-37.7092141076143,-4.9736979588732));
#70306=CARTESIAN_POINT('',(33.1,-37.7092141076143,-4.9736979588732));
#70307=CARTESIAN_POINT('',(35.,-37.4226946144639,-6.59863075134334));
#70308=CARTESIAN_POINT('Origin',(35.,-37.4226946144639,-6.59863075134334));
#70309=CARTESIAN_POINT('',(35.,-41.9469989254299,-8.29418576107601));
#70310=CARTESIAN_POINT('',(35.,2.8665236475809,8.50039468265471));
#70311=CARTESIAN_POINT('',(34.8617922858584,-41.9261572390061,-8.41238483838183));
#70312=CARTESIAN_POINT('',(33.5377160618333,-41.7264868976375,-9.54477161530207));
#70313=CARTESIAN_POINT('',(34.4,-41.4083493394303,-8.63936369090331));
#70314=CARTESIAN_POINT('Ctrl Pts',(34.4,-41.4083493394303,-8.63936369090331));
#70315=CARTESIAN_POINT('Ctrl Pts',(34.6297825290979,-41.666597473988,-8.52664381638261));
#70316=CARTESIAN_POINT('Ctrl Pts',(34.8617922858584,-41.9261572390061,-8.41238483838183));
#70317=CARTESIAN_POINT('',(33.322645308031,-41.2086042970448,-9.54677599452212));
#70318=CARTESIAN_POINT('Origin',(26.8550245390365,0.,0.));
#70319=CARTESIAN_POINT('',(33.0966075166785,-37.0741228455271,-8.2034015372144));
#70320=CARTESIAN_POINT('Origin',(17.5,-35.7083195898645,-12.9967654463754));
#70321=CARTESIAN_POINT('',(33.1,-35.1439863533772,-14.5472582706722));
#70322=CARTESIAN_POINT('',(33.1,-35.1439863533772,-14.5472582706722));
#70323=CARTESIAN_POINT('',(30.5,-35.1439863533772,-14.5472582706722));
#70324=CARTESIAN_POINT('',(30.5,-35.1439863533772,-14.5472582706722));
#70325=CARTESIAN_POINT('',(30.5,-35.31499642504,-14.0774119602792));
#70326=CARTESIAN_POINT('',(30.5,-35.31499642504,-14.0774119602792));
#70327=CARTESIAN_POINT('',(24.1,-35.4518044823703,-13.7015349119648));
#70328=CARTESIAN_POINT('',(24.1,-35.4518044823703,-13.7015349119648));
#70329=CARTESIAN_POINT('',(23.1,-35.3491984393726,-13.9834426982006));
#70330=CARTESIAN_POINT('',(23.1,-35.3491984393726,-13.9834426982006));
#70331=CARTESIAN_POINT('',(22.4,-35.2123903820423,-14.359319746515));
#70332=CARTESIAN_POINT('',(22.4,-35.2123903820423,-14.359319746515));
#70333=CARTESIAN_POINT('',(21.8,-35.1439863533772,-14.5472582706722));
#70334=CARTESIAN_POINT('',(21.8,-35.1439863533772,-14.5472582706722));
#70335=CARTESIAN_POINT('',(13.2,-35.1439863533772,-14.5472582706722));
#70336=CARTESIAN_POINT('',(13.2,-35.1439863533772,-14.5472582706722));
#70337=CARTESIAN_POINT('',(12.6,-35.2123903820423,-14.359319746515));
#70338=CARTESIAN_POINT('',(12.6,-35.2123903820423,-14.359319746515));
#70339=CARTESIAN_POINT('',(11.9,-35.3491984393726,-13.9834426982006));
#70340=CARTESIAN_POINT('',(11.9,-35.3491984393726,-13.9834426982006));
#70341=CARTESIAN_POINT('',(10.9,-35.4518044823703,-13.7015349119648));
#70342=CARTESIAN_POINT('',(10.9,-35.4518044823703,-13.7015349119648));
#70343=CARTESIAN_POINT('',(4.5,-35.31499642504,-14.0774119602792));
#70344=CARTESIAN_POINT('',(4.5,-35.31499642504,-14.0774119602792));
#70345=CARTESIAN_POINT('',(4.5,-35.1439863533772,-14.5472582706722));
#70346=CARTESIAN_POINT('',(4.5,-35.1439863533772,-14.5472582706722));
#70347=CARTESIAN_POINT('',(1.9,-35.1439863533772,-14.5472582706722));
#70348=CARTESIAN_POINT('',(1.9,-35.1439863533772,-14.5472582706722));
#70349=CARTESIAN_POINT('',(1.57538060255633,-35.2404039929487,-14.2823529831122));
#70350=CARTESIAN_POINT('',(0.,-35.7083195898645,-12.9967654463754));
#70351=CARTESIAN_POINT('',(1.57538060255633,-36.1762351867803,-11.7111779096386));
#70352=CARTESIAN_POINT('Ctrl Pts',(1.57538060255633,-35.2404039929487,-14.2823529831122));
#70353=CARTESIAN_POINT('Ctrl Pts',(1.62460345738085,-35.7083195898752,-12.9967654463461));
#70354=CARTESIAN_POINT('Ctrl Pts',(1.57538060255633,-36.1762351867803,-11.7111779096386));
#70355=CARTESIAN_POINT('',(1.9,-36.2726528263519,-11.4462726220787));
#70356=CARTESIAN_POINT('',(1.9,-36.2726528263519,-11.4462726220787));
#70357=CARTESIAN_POINT('',(4.5,-36.2726528263519,-11.4462726220787));
#70358=CARTESIAN_POINT('',(4.5,-36.2726528263519,-11.4462726220787));
#70359=CARTESIAN_POINT('',(4.5,-36.101642754689,-11.9161189324716));
#70360=CARTESIAN_POINT('',(4.5,-36.101642754689,-11.9161189324716));
#70361=CARTESIAN_POINT('',(10.9,-35.9648346973588,-12.291995980786));
#70362=CARTESIAN_POINT('',(10.9,-35.9648346973588,-12.291995980786));
#70363=CARTESIAN_POINT('',(11.9,-36.0674407403565,-12.0100881945502));
#70364=CARTESIAN_POINT('',(11.9,-36.0674407403565,-12.0100881945502));
#70365=CARTESIAN_POINT('',(12.6,-36.2042487976867,-11.6342111462358));
#70366=CARTESIAN_POINT('',(12.6,-36.2042487976867,-11.6342111462358));
#70367=CARTESIAN_POINT('',(13.2,-36.2726528263519,-11.4462726220787));
#70368=CARTESIAN_POINT('',(13.2,-36.2726528263519,-11.4462726220787));
#70369=CARTESIAN_POINT('',(21.8,-36.2726528263519,-11.4462726220787));
#70370=CARTESIAN_POINT('',(21.8,-36.2726528263519,-11.4462726220787));
#70371=CARTESIAN_POINT('',(22.4,-36.2042487976867,-11.6342111462358));
#70372=CARTESIAN_POINT('',(22.4,-36.2042487976867,-11.6342111462358));
#70373=CARTESIAN_POINT('',(23.1,-36.0674407403565,-12.0100881945502));
#70374=CARTESIAN_POINT('',(23.1,-36.0674407403565,-12.0100881945502));
#70375=CARTESIAN_POINT('',(24.1,-35.9648346973588,-12.291995980786));
#70376=CARTESIAN_POINT('',(24.1,-35.9648346973588,-12.291995980786));
#70377=CARTESIAN_POINT('',(30.5,-36.101642754689,-11.9161189324716));
#70378=CARTESIAN_POINT('',(30.5,-36.101642754689,-11.9161189324716));
#70379=CARTESIAN_POINT('',(30.5,-36.2726528263519,-11.4462726220787));
#70380=CARTESIAN_POINT('',(30.5,-36.2726528263519,-11.4462726220787));
#70381=CARTESIAN_POINT('',(33.1,-36.2726528263519,-11.4462726220787));
#70382=CARTESIAN_POINT('',(33.1,-36.2726528263519,-11.4462726220787));
#70383=CARTESIAN_POINT('',(35.,-35.7083195898645,-12.9967654463754));
#70384=CARTESIAN_POINT('Origin',(35.,-35.7083195898645,-12.9967654463754));
#70385=CARTESIAN_POINT('',(35.,-39.8694595147163,-15.4521983644287));
#70386=CARTESIAN_POINT('',(35.,-0.336200737254209,7.87584796738456));
#70387=CARTESIAN_POINT('',(34.8617922858584,-39.8284094059642,-15.5649826112914));
#70388=CARTESIAN_POINT('',(33.5377160618333,-39.4351356055115,-16.6454934976981));
#70389=CARTESIAN_POINT('',(34.4,-39.2790537077817,-15.6985967468815));
#70390=CARTESIAN_POINT('Ctrl Pts',(34.4,-39.2790537077817,-15.6985967468815));
#70391=CARTESIAN_POINT('Ctrl Pts',(34.6297825291028,-39.5529520736982,-15.6324336584854));
#70392=CARTESIAN_POINT('Ctrl Pts',(34.8617922858584,-39.8284094059642,-15.5649826112914));
#70393=CARTESIAN_POINT('',(33.3226453080309,-38.9247727484987,-16.5575380560557));
#70394=CARTESIAN_POINT('Origin',(26.8550245390365,0.,0.));
#70395=CARTESIAN_POINT('',(33.0966075166785,-35.0863778867947,-14.5166273056467));
#70396=CARTESIAN_POINT('Origin',(17.5,-32.9089653438087,-19.));
#70397=CARTESIAN_POINT('',(33.1,-32.0839653438087,-20.4289419162443));
#70398=CARTESIAN_POINT('',(33.1,-32.0839653438087,-20.4289419162443));
#70399=CARTESIAN_POINT('',(30.5,-32.0839653438087,-20.4289419162443));
#70400=CARTESIAN_POINT('',(30.5,-32.0839653438087,-20.4289419162443));
#70401=CARTESIAN_POINT('',(30.5,-32.3339653438087,-19.9959292143521));
#70402=CARTESIAN_POINT('',(30.5,-32.3339653438087,-19.9959292143521));
#70403=CARTESIAN_POINT('',(24.1,-32.5339653438087,-19.6495190528383));
#70404=CARTESIAN_POINT('',(24.1,-32.5339653438087,-19.6495190528383));
#70405=CARTESIAN_POINT('',(23.1,-32.3839653438087,-19.9093266739736));
#70406=CARTESIAN_POINT('',(23.1,-32.3839653438087,-19.9093266739736));
#70407=CARTESIAN_POINT('',(22.4,-32.1839653438087,-20.2557368354874));
#70408=CARTESIAN_POINT('',(22.4,-32.1839653438087,-20.2557368354874));
#70409=CARTESIAN_POINT('',(21.8,-32.0839653438087,-20.4289419162443));
#70410=CARTESIAN_POINT('',(21.8,-32.0839653438087,-20.4289419162443));
#70411=CARTESIAN_POINT('',(13.2,-32.0839653438087,-20.4289419162443));
#70412=CARTESIAN_POINT('',(13.2,-32.0839653438087,-20.4289419162443));
#70413=CARTESIAN_POINT('',(12.6,-32.1839653438087,-20.2557368354874));
#70414=CARTESIAN_POINT('',(12.6,-32.1839653438087,-20.2557368354874));
#70415=CARTESIAN_POINT('',(11.9,-32.3839653438087,-19.9093266739736));
#70416=CARTESIAN_POINT('',(11.9,-32.3839653438087,-19.9093266739736));
#70417=CARTESIAN_POINT('',(10.9,-32.5339653438087,-19.6495190528383));
#70418=CARTESIAN_POINT('',(10.9,-32.5339653438087,-19.6495190528383));
#70419=CARTESIAN_POINT('',(4.5,-32.3339653438087,-19.9959292143521));
#70420=CARTESIAN_POINT('',(4.5,-32.3339653438087,-19.9959292143521));
#70421=CARTESIAN_POINT('',(4.5,-32.0839653438087,-20.4289419162443));
#70422=CARTESIAN_POINT('',(4.5,-32.0839653438087,-20.4289419162443));
#70423=CARTESIAN_POINT('',(1.9,-32.0839653438087,-20.4289419162443));
#70424=CARTESIAN_POINT('',(1.9,-32.0839653438087,-20.4289419162443));
#70425=CARTESIAN_POINT('',(1.57538060255633,-32.224918503225,-20.1848038826479));
#70426=CARTESIAN_POINT('',(0.,-32.9089653438087,-19.));
#70427=CARTESIAN_POINT('',(1.57538060255633,-33.5930121843923,-17.8151961173521));
#70428=CARTESIAN_POINT('Ctrl Pts',(1.57538060255633,-32.224918503225,-20.1848038826479));
#70429=CARTESIAN_POINT('Ctrl Pts',(1.62460345738085,-32.9089653438243,-18.999999999973));
#70430=CARTESIAN_POINT('Ctrl Pts',(1.57538060255633,-33.5930121843923,-17.8151961173521));
#70431=CARTESIAN_POINT('',(1.9,-33.7339653438087,-17.5710580837557));
#70432=CARTESIAN_POINT('',(1.9,-33.7339653438087,-17.5710580837557));
#70433=CARTESIAN_POINT('',(4.5,-33.7339653438087,-17.5710580837557));
#70434=CARTESIAN_POINT('',(4.5,-33.7339653438087,-17.5710580837557));
#70435=CARTESIAN_POINT('',(4.5,-33.4839653438087,-18.0040707856479));
#70436=CARTESIAN_POINT('',(4.5,-33.4839653438087,-18.0040707856479));
#70437=CARTESIAN_POINT('',(10.9,-33.2839653438087,-18.3504809471617));
#70438=CARTESIAN_POINT('',(10.9,-33.2839653438087,-18.3504809471617));
#70439=CARTESIAN_POINT('',(11.9,-33.4339653438087,-18.0906733260263));
#70440=CARTESIAN_POINT('',(11.9,-33.4339653438087,-18.0906733260263));
#70441=CARTESIAN_POINT('',(12.6,-33.6339653438087,-17.7442631645126));
#70442=CARTESIAN_POINT('',(12.6,-33.6339653438087,-17.7442631645126));
#70443=CARTESIAN_POINT('',(13.2,-33.7339653438087,-17.5710580837557));
#70444=CARTESIAN_POINT('',(13.2,-33.7339653438087,-17.5710580837557));
#70445=CARTESIAN_POINT('',(21.8,-33.7339653438087,-17.5710580837557));
#70446=CARTESIAN_POINT('',(21.8,-33.7339653438087,-17.5710580837557));
#70447=CARTESIAN_POINT('',(22.4,-33.6339653438087,-17.7442631645126));
#70448=CARTESIAN_POINT('',(22.4,-33.6339653438087,-17.7442631645126));
#70449=CARTESIAN_POINT('',(23.1,-33.4339653438087,-18.0906733260263));
#70450=CARTESIAN_POINT('',(23.1,-33.4339653438087,-18.0906733260263));
#70451=CARTESIAN_POINT('',(24.1,-33.2839653438087,-18.3504809471617));
#70452=CARTESIAN_POINT('',(24.1,-33.2839653438087,-18.3504809471617));
#70453=CARTESIAN_POINT('',(30.5,-33.4839653438087,-18.0040707856479));
#70454=CARTESIAN_POINT('',(30.5,-33.4839653438087,-18.0040707856479));
#70455=CARTESIAN_POINT('',(30.5,-33.7339653438087,-17.5710580837557));
#70456=CARTESIAN_POINT('',(30.5,-33.7339653438087,-17.5710580837557));
#70457=CARTESIAN_POINT('',(33.1,-33.7339653438087,-17.5710580837557));
#70458=CARTESIAN_POINT('',(33.1,-33.7339653438087,-17.5710580837557));
#70459=CARTESIAN_POINT('',(35.,-32.9089653438087,-19.));
#70460=CARTESIAN_POINT('Origin',(35.,-32.9089653438087,-19.));
#70461=CARTESIAN_POINT('',(35.,-36.580506751568,-22.1407037396679));
#70462=CARTESIAN_POINT('',(35.,-3.70080331045544,5.98519655344499));
#70463=CARTESIAN_POINT('',(34.8617922858584,-36.5204955072697,-22.244646263818));
#70464=CARTESIAN_POINT('',(33.5377160618333,-35.9455676731535,-23.2404504831928));
#70465=CARTESIAN_POINT('',(34.4,-35.9562839053824,-22.2808358845789));
#70466=CARTESIAN_POINT('Ctrl Pts',(34.4,-35.9562839053824,-22.2808358845789));
#70467=CARTESIAN_POINT('Ctrl Pts',(34.6297825291,-36.2375102393997,-22.2632399142707));
#70468=CARTESIAN_POINT('Ctrl Pts',(34.8617922858584,-36.5204955072696,-22.244646263818));
#70469=CARTESIAN_POINT('',(33.322645308031,-35.4582316768749,-23.0652077022745));
#70470=CARTESIAN_POINT('Origin',(26.8550245390365,0.,0.));
#70471=CARTESIAN_POINT('',(33.0966075166785,-32.032551090536,-20.3887726991648));
#70472=CARTESIAN_POINT('Origin',(17.5,-29.1096888385212,-24.4259291680885));
#70473=CARTESIAN_POINT('',(33.1,-28.0490892825384,-25.6899024992348));
#70474=CARTESIAN_POINT('',(33.1,-28.0490892825384,-25.6899024992348));
#70475=CARTESIAN_POINT('',(30.5,-28.0490892825384,-25.6899024992348));
#70476=CARTESIAN_POINT('',(30.5,-28.0490892825384,-25.6899024992348));
#70477=CARTESIAN_POINT('',(30.5,-28.3704830873816,-25.3068802776753));
#70478=CARTESIAN_POINT('',(30.5,-28.3704830873816,-25.3068802776753));
#70479=CARTESIAN_POINT('',(24.1,-28.6275981312563,-25.0004625004277));
#70480=CARTESIAN_POINT('',(24.1,-28.6275981312563,-25.0004625004277));
#70481=CARTESIAN_POINT('',(23.1,-28.4347618483503,-25.2302758333634));
#70482=CARTESIAN_POINT('',(23.1,-28.4347618483503,-25.2302758333634));
#70483=CARTESIAN_POINT('',(22.4,-28.1776468044757,-25.536693610611));
#70484=CARTESIAN_POINT('',(22.4,-28.1776468044757,-25.536693610611));
#70485=CARTESIAN_POINT('',(21.8,-28.0490892825384,-25.6899024992348));
#70486=CARTESIAN_POINT('',(21.8,-28.0490892825384,-25.6899024992348));
#70487=CARTESIAN_POINT('',(13.2,-28.0490892825384,-25.6899024992348));
#70488=CARTESIAN_POINT('',(13.2,-28.0490892825384,-25.6899024992348));
#70489=CARTESIAN_POINT('',(12.6,-28.1776468044757,-25.536693610611));
#70490=CARTESIAN_POINT('',(12.6,-28.1776468044757,-25.536693610611));
#70491=CARTESIAN_POINT('',(11.9,-28.4347618483503,-25.2302758333634));
#70492=CARTESIAN_POINT('',(11.9,-28.4347618483503,-25.2302758333634));
#70493=CARTESIAN_POINT('',(10.9,-28.6275981312563,-25.0004625004277));
#70494=CARTESIAN_POINT('',(10.9,-28.6275981312563,-25.0004625004277));
#70495=CARTESIAN_POINT('',(4.5,-28.3704830873816,-25.3068802776753));
#70496=CARTESIAN_POINT('',(4.5,-28.3704830873816,-25.3068802776753));
#70497=CARTESIAN_POINT('',(4.5,-28.0490892825384,-25.6899024992348));
#70498=CARTESIAN_POINT('',(4.5,-28.0490892825384,-25.6899024992348));
#70499=CARTESIAN_POINT('',(1.9,-28.0490892825384,-25.6899024992348));
#70500=CARTESIAN_POINT('',(1.9,-28.0490892825384,-25.6899024992348));
#70501=CARTESIAN_POINT('',(1.57538060255632,-28.2302951713764,-25.4739497302129));
#70502=CARTESIAN_POINT('',(0.,-29.1096888385212,-24.4259291680885));
#70503=CARTESIAN_POINT('',(1.57538060255632,-29.989082505666,-23.3779086059641));
#70504=CARTESIAN_POINT('Ctrl Pts',(1.57538060255632,-28.2302951713764,-25.4739497302129));
#70505=CARTESIAN_POINT('Ctrl Pts',(1.62460345738085,-29.1096888385412,-24.4259291680646));
#70506=CARTESIAN_POINT('Ctrl Pts',(1.57538060255632,-29.989082505666,-23.3779086059641));
#70507=CARTESIAN_POINT('',(1.9,-30.170288394504,-23.1619558369422));
#70508=CARTESIAN_POINT('',(1.9,-30.170288394504,-23.1619558369422));
#70509=CARTESIAN_POINT('',(4.5,-30.170288394504,-23.1619558369422));
#70510=CARTESIAN_POINT('',(4.5,-30.170288394504,-23.1619558369422));
#70511=CARTESIAN_POINT('',(4.5,-29.8488945896607,-23.5449780585017));
#70512=CARTESIAN_POINT('',(4.5,-29.8488945896607,-23.5449780585017));
#70513=CARTESIAN_POINT('',(10.9,-29.5917795457861,-23.8513958357493));
#70514=CARTESIAN_POINT('',(10.9,-29.5917795457861,-23.8513958357493));
#70515=CARTESIAN_POINT('',(11.9,-29.784615828692,-23.6215825028136));
#70516=CARTESIAN_POINT('',(11.9,-29.784615828692,-23.6215825028136));
#70517=CARTESIAN_POINT('',(12.6,-30.0417308725667,-23.315164725566));
#70518=CARTESIAN_POINT('',(12.6,-30.0417308725667,-23.315164725566));
#70519=CARTESIAN_POINT('',(13.2,-30.170288394504,-23.1619558369422));
#70520=CARTESIAN_POINT('',(13.2,-30.170288394504,-23.1619558369422));
#70521=CARTESIAN_POINT('',(21.8,-30.170288394504,-23.1619558369422));
#70522=CARTESIAN_POINT('',(21.8,-30.170288394504,-23.1619558369422));
#70523=CARTESIAN_POINT('',(22.4,-30.0417308725667,-23.315164725566));
#70524=CARTESIAN_POINT('',(22.4,-30.0417308725667,-23.315164725566));
#70525=CARTESIAN_POINT('',(23.1,-29.784615828692,-23.6215825028136));
#70526=CARTESIAN_POINT('',(23.1,-29.784615828692,-23.6215825028136));
#70527=CARTESIAN_POINT('',(24.1,-29.5917795457861,-23.8513958357493));
#70528=CARTESIAN_POINT('',(24.1,-29.5917795457861,-23.8513958357493));
#70529=CARTESIAN_POINT('',(30.5,-29.8488945896607,-23.5449780585017));
#70530=CARTESIAN_POINT('',(30.5,-29.8488945896607,-23.5449780585017));
#70531=CARTESIAN_POINT('',(30.5,-30.170288394504,-23.1619558369422));
#70532=CARTESIAN_POINT('',(30.5,-30.170288394504,-23.1619558369422));
#70533=CARTESIAN_POINT('',(33.1,-30.170288394504,-23.1619558369422));
#70534=CARTESIAN_POINT('',(33.1,-30.170288394504,-23.1619558369422));
#70535=CARTESIAN_POINT('',(35.,-29.1096888385212,-24.4259291680885));
#70536=CARTESIAN_POINT('Origin',(35.,-29.1096888385212,-24.4259291680885));
#70537=CARTESIAN_POINT('',(35.,-32.1800738014028,-28.156475035514));
#70538=CARTESIAN_POINT('',(35.,-6.7396658591028,2.75385375455791));
#70539=CARTESIAN_POINT('',(34.8617922858584,-32.1029248328492,-28.2484175959528));
#70540=CARTESIAN_POINT('',(33.5377160618333,-31.3638118563816,-29.129258140991));
#70541=CARTESIAN_POINT('',(34.4,-31.5410006112756,-28.1860830985703));
#70542=CARTESIAN_POINT('Ctrl Pts',(34.4,-31.5410006112756,-28.1860830985703));
#70543=CARTESIAN_POINT('Ctrl Pts',(34.6297825290998,-31.8210099935452,-28.2175888910031));
#70544=CARTESIAN_POINT('Ctrl Pts',(34.8617922858584,-32.1029248328492,-28.2484175959527));
#70545=CARTESIAN_POINT('',(33.3226453080309,-30.9143101784803,-28.872052684018));
#70546=CARTESIAN_POINT('Origin',(26.8550245390365,0.,0.));
#70547=CARTESIAN_POINT('',(33.0966075166785,-28.0054314386442,-25.6414155514355));
#70548=CARTESIAN_POINT('Origin',(17.5,-24.4259291680885,-29.1096888385212));
#70549=CARTESIAN_POINT('',(33.1,-23.1619558369422,-30.1702883945039));
#70550=CARTESIAN_POINT('',(33.1,-23.1619558369422,-30.1702883945039));
#70551=CARTESIAN_POINT('',(30.5,-23.1619558369422,-30.1702883945039));
#70552=CARTESIAN_POINT('',(30.5,-23.1619558369422,-30.1702883945039));
#70553=CARTESIAN_POINT('',(30.5,-23.5449780585017,-29.8488945896607));
#70554=CARTESIAN_POINT('',(30.5,-23.5449780585017,-29.8488945896607));
#70555=CARTESIAN_POINT('',(24.1,-23.8513958357493,-29.5917795457861));
#70556=CARTESIAN_POINT('',(24.1,-23.8513958357493,-29.5917795457861));
#70557=CARTESIAN_POINT('',(23.1,-23.6215825028136,-29.784615828692));
#70558=CARTESIAN_POINT('',(23.1,-23.6215825028136,-29.784615828692));
#70559=CARTESIAN_POINT('',(22.4,-23.315164725566,-30.0417308725666));
#70560=CARTESIAN_POINT('',(22.4,-23.315164725566,-30.0417308725666));
#70561=CARTESIAN_POINT('',(21.8,-23.1619558369422,-30.1702883945039));
#70562=CARTESIAN_POINT('',(21.8,-23.1619558369422,-30.1702883945039));
#70563=CARTESIAN_POINT('',(13.2,-23.1619558369422,-30.1702883945039));
#70564=CARTESIAN_POINT('',(13.2,-23.1619558369422,-30.1702883945039));
#70565=CARTESIAN_POINT('',(12.6,-23.315164725566,-30.0417308725666));
#70566=CARTESIAN_POINT('',(12.6,-23.315164725566,-30.0417308725666));
#70567=CARTESIAN_POINT('',(11.9,-23.6215825028136,-29.784615828692));
#70568=CARTESIAN_POINT('',(11.9,-23.6215825028136,-29.784615828692));
#70569=CARTESIAN_POINT('',(10.9,-23.8513958357493,-29.5917795457861));
#70570=CARTESIAN_POINT('',(10.9,-23.8513958357493,-29.5917795457861));
#70571=CARTESIAN_POINT('',(4.5,-23.5449780585017,-29.8488945896607));
#70572=CARTESIAN_POINT('',(4.5,-23.5449780585017,-29.8488945896607));
#70573=CARTESIAN_POINT('',(4.5,-23.1619558369422,-30.1702883945039));
#70574=CARTESIAN_POINT('',(4.5,-23.1619558369422,-30.1702883945039));
#70575=CARTESIAN_POINT('',(1.9,-23.1619558369422,-30.1702883945039));
#70576=CARTESIAN_POINT('',(1.9,-23.1619558369422,-30.1702883945039));
#70577=CARTESIAN_POINT('',(1.57538060255632,-23.3779086059641,-29.989082505666));
#70578=CARTESIAN_POINT('',(0.,-24.4259291680885,-29.1096888385212));
#70579=CARTESIAN_POINT('',(1.57538060255632,-25.4739497302129,-28.2302951713763));
#70580=CARTESIAN_POINT('Ctrl Pts',(1.57538060255632,-23.3779086059641,-29.989082505666));
#70581=CARTESIAN_POINT('Ctrl Pts',(1.62460345738085,-24.4259291681124,-29.1096888385011));
#70582=CARTESIAN_POINT('Ctrl Pts',(1.57538060255632,-25.4739497302129,-28.2302951713763));
#70583=CARTESIAN_POINT('',(1.9,-25.6899024992348,-28.0490892825384));
#70584=CARTESIAN_POINT('',(1.9,-25.6899024992348,-28.0490892825384));
#70585=CARTESIAN_POINT('',(4.5,-25.6899024992348,-28.0490892825384));
#70586=CARTESIAN_POINT('',(4.5,-25.6899024992348,-28.0490892825384));
#70587=CARTESIAN_POINT('',(4.5,-25.3068802776753,-28.3704830873816));
#70588=CARTESIAN_POINT('',(4.5,-25.3068802776753,-28.3704830873816));
#70589=CARTESIAN_POINT('',(10.9,-25.0004625004277,-28.6275981312563));
#70590=CARTESIAN_POINT('',(10.9,-25.0004625004277,-28.6275981312563));
#70591=CARTESIAN_POINT('',(11.9,-25.2302758333634,-28.4347618483503));
#70592=CARTESIAN_POINT('',(11.9,-25.2302758333634,-28.4347618483503));
#70593=CARTESIAN_POINT('',(12.6,-25.536693610611,-28.1776468044757));
#70594=CARTESIAN_POINT('',(12.6,-25.536693610611,-28.1776468044757));
#70595=CARTESIAN_POINT('',(13.2,-25.6899024992348,-28.0490892825384));
#70596=CARTESIAN_POINT('',(13.2,-25.6899024992348,-28.0490892825384));
#70597=CARTESIAN_POINT('',(21.8,-25.6899024992348,-28.0490892825384));
#70598=CARTESIAN_POINT('',(21.8,-25.6899024992348,-28.0490892825384));
#70599=CARTESIAN_POINT('',(22.4,-25.536693610611,-28.1776468044757));
#70600=CARTESIAN_POINT('',(22.4,-25.536693610611,-28.1776468044757));
#70601=CARTESIAN_POINT('',(23.1,-25.2302758333634,-28.4347618483503));
#70602=CARTESIAN_POINT('',(23.1,-25.2302758333634,-28.4347618483503));
#70603=CARTESIAN_POINT('',(24.1,-25.0004625004277,-28.6275981312563));
#70604=CARTESIAN_POINT('',(24.1,-25.0004625004277,-28.6275981312563));
#70605=CARTESIAN_POINT('',(30.5,-25.3068802776753,-28.3704830873816));
#70606=CARTESIAN_POINT('',(30.5,-25.3068802776753,-28.3704830873816));
#70607=CARTESIAN_POINT('',(30.5,-25.6899024992348,-28.0490892825384));
#70608=CARTESIAN_POINT('',(30.5,-25.6899024992348,-28.0490892825384));
#70609=CARTESIAN_POINT('',(33.1,-25.6899024992348,-28.0490892825384));
#70610=CARTESIAN_POINT('',(33.1,-25.6899024992348,-28.0490892825384));
#70611=CARTESIAN_POINT('',(35.,-24.4259291680885,-29.1096888385212));
#70612=CARTESIAN_POINT('Origin',(35.,-24.4259291680885,-29.1096888385212));
#70613=CARTESIAN_POINT('',(35.,-26.8018655926852,-33.3167260852698));
#70614=CARTESIAN_POINT('',(35.,-8.95315125918114,-1.71225837718511));
#70615=CARTESIAN_POINT('',(34.8617922858584,-26.7099230322464,-33.3938750538235));
#70616=CARTESIAN_POINT('',(33.5377160618333,-25.8290824872081,-34.132988030291));
#70617=CARTESIAN_POINT('',(34.4,-26.1673599741116,-33.234910440458));
#70618=CARTESIAN_POINT('Ctrl Pts',(34.4,-26.1673599741116,-33.234910440458));
#70619=CARTESIAN_POINT('Ctrl Pts',(34.6297825291012,-26.4376444612465,-33.3145607080718));
#70620=CARTESIAN_POINT('Ctrl Pts',(34.8617922858584,-26.7099230322464,-33.3938750538234));
#70621=CARTESIAN_POINT('',(33.322645308031,-25.4310730087083,-33.8016349549212));
#70622=CARTESIAN_POINT('Origin',(26.8550245390365,0.,0.));
#70623=CARTESIAN_POINT('',(33.0966075166785,-23.1273809239214,-30.1149569673582));
#70624=CARTESIAN_POINT('Origin',(17.5,-19.,-32.9089653438087));
#70625=CARTESIAN_POINT('',(33.1,-17.5710580837557,-33.7339653438087));
#70626=CARTESIAN_POINT('',(33.1,-17.5710580837557,-33.7339653438087));
#70627=CARTESIAN_POINT('',(30.5,-17.5710580837557,-33.7339653438087));
#70628=CARTESIAN_POINT('',(30.5,-17.5710580837557,-33.7339653438087));
#70629=CARTESIAN_POINT('',(30.5,-18.0040707856479,-33.4839653438087));
#70630=CARTESIAN_POINT('',(30.5,-18.0040707856479,-33.4839653438087));
#70631=CARTESIAN_POINT('',(24.1,-18.3504809471617,-33.2839653438087));
#70632=CARTESIAN_POINT('',(24.1,-18.3504809471617,-33.2839653438087));
#70633=CARTESIAN_POINT('',(23.1,-18.0906733260264,-33.4339653438087));
#70634=CARTESIAN_POINT('',(23.1,-18.0906733260264,-33.4339653438087));
#70635=CARTESIAN_POINT('',(22.4,-17.7442631645126,-33.6339653438087));
#70636=CARTESIAN_POINT('',(22.4,-17.7442631645126,-33.6339653438087));
#70637=CARTESIAN_POINT('',(21.8,-17.5710580837557,-33.7339653438087));
#70638=CARTESIAN_POINT('',(21.8,-17.5710580837557,-33.7339653438087));
#70639=CARTESIAN_POINT('',(13.2,-17.5710580837557,-33.7339653438087));
#70640=CARTESIAN_POINT('',(13.2,-17.5710580837557,-33.7339653438087));
#70641=CARTESIAN_POINT('',(12.6,-17.7442631645126,-33.6339653438087));
#70642=CARTESIAN_POINT('',(12.6,-17.7442631645126,-33.6339653438087));
#70643=CARTESIAN_POINT('',(11.9,-18.0906733260264,-33.4339653438087));
#70644=CARTESIAN_POINT('',(11.9,-18.0906733260264,-33.4339653438087));
#70645=CARTESIAN_POINT('',(10.9,-18.3504809471617,-33.2839653438087));
#70646=CARTESIAN_POINT('',(10.9,-18.3504809471617,-33.2839653438087));
#70647=CARTESIAN_POINT('',(4.5,-18.0040707856479,-33.4839653438087));
#70648=CARTESIAN_POINT('',(4.5,-18.0040707856479,-33.4839653438087));
#70649=CARTESIAN_POINT('',(4.5,-17.5710580837557,-33.7339653438087));
#70650=CARTESIAN_POINT('',(4.5,-17.5710580837557,-33.7339653438087));
#70651=CARTESIAN_POINT('',(1.9,-17.5710580837557,-33.7339653438087));
#70652=CARTESIAN_POINT('',(1.9,-17.5710580837557,-33.7339653438087));
#70653=CARTESIAN_POINT('',(1.57538060255633,-17.8151961173521,-33.5930121843923));
#70654=CARTESIAN_POINT('',(0.,-19.,-32.9089653438087));
#70655=CARTESIAN_POINT('',(1.57538060255632,-20.1848038826479,-32.224918503225));
#70656=CARTESIAN_POINT('Ctrl Pts',(1.57538060255633,-17.8151961173521,-33.5930121843923));
#70657=CARTESIAN_POINT('Ctrl Pts',(1.62460345738085,-19.000000000027,-32.9089653437931));
#70658=CARTESIAN_POINT('Ctrl Pts',(1.57538060255632,-20.1848038826479,-32.224918503225));
#70659=CARTESIAN_POINT('',(1.9,-20.4289419162443,-32.0839653438087));
#70660=CARTESIAN_POINT('',(1.9,-20.4289419162443,-32.0839653438087));
#70661=CARTESIAN_POINT('',(4.5,-20.4289419162443,-32.0839653438087));
#70662=CARTESIAN_POINT('',(4.5,-20.4289419162443,-32.0839653438087));
#70663=CARTESIAN_POINT('',(4.5,-19.9959292143521,-32.3339653438087));
#70664=CARTESIAN_POINT('',(4.5,-19.9959292143521,-32.3339653438087));
#70665=CARTESIAN_POINT('',(10.9,-19.6495190528383,-32.5339653438087));
#70666=CARTESIAN_POINT('',(10.9,-19.6495190528383,-32.5339653438087));
#70667=CARTESIAN_POINT('',(11.9,-19.9093266739737,-32.3839653438087));
#70668=CARTESIAN_POINT('',(11.9,-19.9093266739737,-32.3839653438087));
#70669=CARTESIAN_POINT('',(12.6,-20.2557368354875,-32.1839653438087));
#70670=CARTESIAN_POINT('',(12.6,-20.2557368354875,-32.1839653438087));
#70671=CARTESIAN_POINT('',(13.2,-20.4289419162443,-32.0839653438087));
#70672=CARTESIAN_POINT('',(13.2,-20.4289419162443,-32.0839653438087));
#70673=CARTESIAN_POINT('',(21.8,-20.4289419162443,-32.0839653438087));
#70674=CARTESIAN_POINT('',(21.8,-20.4289419162443,-32.0839653438087));
#70675=CARTESIAN_POINT('',(22.4,-20.2557368354875,-32.1839653438087));
#70676=CARTESIAN_POINT('',(22.4,-20.2557368354875,-32.1839653438087));
#70677=CARTESIAN_POINT('',(23.1,-19.9093266739737,-32.3839653438087));
#70678=CARTESIAN_POINT('',(23.1,-19.9093266739737,-32.3839653438087));
#70679=CARTESIAN_POINT('',(24.1,-19.6495190528383,-32.5339653438087));
#70680=CARTESIAN_POINT('',(24.1,-19.6495190528383,-32.5339653438087));
#70681=CARTESIAN_POINT('',(30.5,-19.9959292143521,-32.3339653438087));
#70682=CARTESIAN_POINT('',(30.5,-19.9959292143521,-32.3339653438087));
#70683=CARTESIAN_POINT('',(30.5,-20.4289419162443,-32.0839653438087));
#70684=CARTESIAN_POINT('',(30.5,-20.4289419162443,-32.0839653438087));
#70685=CARTESIAN_POINT('',(33.1,-20.4289419162443,-32.0839653438087));
#70686=CARTESIAN_POINT('',(33.1,-20.4289419162443,-32.0839653438087));
#70687=CARTESIAN_POINT('',(35.,-19.,-32.9089653438087));
#70688=CARTESIAN_POINT('Origin',(35.,-19.,-32.9089653438087));
#70689=CARTESIAN_POINT('',(35.,-20.6092962603321,-37.4646652720015));
#70690=CARTESIAN_POINT('',(35.,-9.89391142839378,-7.13086091745311));
#70691=CARTESIAN_POINT('',(34.8617922858584,-20.505353736182,-37.5246765162998));
#70692=CARTESIAN_POINT('',(33.5377160618333,-19.5095495168072,-38.099604350416));
#70693=CARTESIAN_POINT('',(34.4,-19.9986373454573,-37.2739118462884));
#70694=CARTESIAN_POINT('Ctrl Pts',(34.4,-19.9986373454573,-37.2739118462884));
#70695=CARTESIAN_POINT('Ctrl Pts',(34.6297825290997,-20.2509844800833,-37.3992864560058));
#70696=CARTESIAN_POINT('Ctrl Pts',(34.8617922858584,-20.505353736182,-37.5246765162998));
#70697=CARTESIAN_POINT('',(33.3226453080309,-19.1751255543105,-37.7041716521717));
#70698=CARTESIAN_POINT('Origin',(26.8550245390365,0.,0.));
#70699=CARTESIAN_POINT('',(33.0966075166785,-17.5466166428447,-33.6734706547313));
#70700=CARTESIAN_POINT('Origin',(17.5,-12.9967654463754,-35.7083195898645));
#70701=CARTESIAN_POINT('',(33.1,-11.4462726220787,-36.2726528263519));
#70702=CARTESIAN_POINT('',(33.1,-11.4462726220787,-36.2726528263519));
#70703=CARTESIAN_POINT('',(30.5,-11.4462726220787,-36.2726528263519));
#70704=CARTESIAN_POINT('',(30.5,-11.4462726220787,-36.2726528263519));
#70705=CARTESIAN_POINT('',(30.5,-11.9161189324716,-36.101642754689));
#70706=CARTESIAN_POINT('',(30.5,-11.9161189324716,-36.101642754689));
#70707=CARTESIAN_POINT('',(24.1,-12.291995980786,-35.9648346973588));
#70708=CARTESIAN_POINT('',(24.1,-12.291995980786,-35.9648346973588));
#70709=CARTESIAN_POINT('',(23.1,-12.0100881945502,-36.0674407403565));
#70710=CARTESIAN_POINT('',(23.1,-12.0100881945502,-36.0674407403565));
#70711=CARTESIAN_POINT('',(22.4,-11.6342111462359,-36.2042487976867));
#70712=CARTESIAN_POINT('',(22.4,-11.6342111462359,-36.2042487976867));
#70713=CARTESIAN_POINT('',(21.8,-11.4462726220787,-36.2726528263519));
#70714=CARTESIAN_POINT('',(21.8,-11.4462726220787,-36.2726528263519));
#70715=CARTESIAN_POINT('',(13.2,-11.4462726220787,-36.2726528263519));
#70716=CARTESIAN_POINT('',(13.2,-11.4462726220787,-36.2726528263519));
#70717=CARTESIAN_POINT('',(12.6,-11.6342111462359,-36.2042487976867));
#70718=CARTESIAN_POINT('',(12.6,-11.6342111462359,-36.2042487976867));
#70719=CARTESIAN_POINT('',(11.9,-12.0100881945502,-36.0674407403565));
#70720=CARTESIAN_POINT('',(11.9,-12.0100881945502,-36.0674407403565));
#70721=CARTESIAN_POINT('',(10.9,-12.291995980786,-35.9648346973588));
#70722=CARTESIAN_POINT('',(10.9,-12.291995980786,-35.9648346973588));
#70723=CARTESIAN_POINT('',(4.5,-11.9161189324716,-36.101642754689));
#70724=CARTESIAN_POINT('',(4.5,-11.9161189324716,-36.101642754689));
#70725=CARTESIAN_POINT('',(4.5,-11.4462726220787,-36.2726528263519));
#70726=CARTESIAN_POINT('',(4.5,-11.4462726220787,-36.2726528263519));
#70727=CARTESIAN_POINT('',(1.9,-11.4462726220787,-36.2726528263519));
#70728=CARTESIAN_POINT('',(1.9,-11.4462726220787,-36.2726528263519));
#70729=CARTESIAN_POINT('',(1.57538060255632,-11.7111779096387,-36.1762351867803));
#70730=CARTESIAN_POINT('',(0.,-12.9967654463754,-35.7083195898645));
#70731=CARTESIAN_POINT('',(1.57538060255632,-14.2823529831122,-35.2404039929487));
#70732=CARTESIAN_POINT('Ctrl Pts',(1.57538060255632,-11.7111779096387,-36.1762351867803));
#70733=CARTESIAN_POINT('Ctrl Pts',(1.62460345738085,-12.9967654464047,-35.7083195898538));
#70734=CARTESIAN_POINT('Ctrl Pts',(1.57538060255632,-14.2823529831122,-35.2404039929487));
#70735=CARTESIAN_POINT('',(1.9,-14.5472582706722,-35.1439863533772));
#70736=CARTESIAN_POINT('',(1.9,-14.5472582706722,-35.1439863533772));
#70737=CARTESIAN_POINT('',(4.5,-14.5472582706722,-35.1439863533772));
#70738=CARTESIAN_POINT('',(4.5,-14.5472582706722,-35.1439863533772));
#70739=CARTESIAN_POINT('',(4.5,-14.0774119602792,-35.31499642504));
#70740=CARTESIAN_POINT('',(4.5,-14.0774119602792,-35.31499642504));
#70741=CARTESIAN_POINT('',(10.9,-13.7015349119649,-35.4518044823703));
#70742=CARTESIAN_POINT('',(10.9,-13.7015349119649,-35.4518044823703));
#70743=CARTESIAN_POINT('',(11.9,-13.9834426982006,-35.3491984393726));
#70744=CARTESIAN_POINT('',(11.9,-13.9834426982006,-35.3491984393726));
#70745=CARTESIAN_POINT('',(12.6,-14.359319746515,-35.2123903820423));
#70746=CARTESIAN_POINT('',(12.6,-14.359319746515,-35.2123903820423));
#70747=CARTESIAN_POINT('',(13.2,-14.5472582706722,-35.1439863533772));
#70748=CARTESIAN_POINT('',(13.2,-14.5472582706722,-35.1439863533772));
#70749=CARTESIAN_POINT('',(21.8,-14.5472582706722,-35.1439863533772));
#70750=CARTESIAN_POINT('',(21.8,-14.5472582706722,-35.1439863533772));
#70751=CARTESIAN_POINT('',(22.4,-14.359319746515,-35.2123903820423));
#70752=CARTESIAN_POINT('',(22.4,-14.359319746515,-35.2123903820423));
#70753=CARTESIAN_POINT('',(23.1,-13.9834426982006,-35.3491984393726));
#70754=CARTESIAN_POINT('',(23.1,-13.9834426982006,-35.3491984393726));
#70755=CARTESIAN_POINT('',(24.1,-13.7015349119649,-35.4518044823703));
#70756=CARTESIAN_POINT('',(24.1,-13.7015349119649,-35.4518044823703));
#70757=CARTESIAN_POINT('',(30.5,-14.0774119602792,-35.31499642504));
#70758=CARTESIAN_POINT('',(30.5,-14.0774119602792,-35.31499642504));
#70759=CARTESIAN_POINT('',(30.5,-14.5472582706722,-35.1439863533772));
#70760=CARTESIAN_POINT('',(30.5,-14.5472582706722,-35.1439863533772));
#70761=CARTESIAN_POINT('',(33.1,-14.5472582706722,-35.1439863533772));
#70762=CARTESIAN_POINT('',(33.1,-14.5472582706722,-35.1439863533772));
#70763=CARTESIAN_POINT('',(35.,-12.9967654463754,-35.7083195898645));
#70764=CARTESIAN_POINT('Origin',(35.,-12.9967654463754,-35.7083195898645));
#70765=CARTESIAN_POINT('',(35.,-13.790523889916,-40.4742595624789));
#70766=CARTESIAN_POINT('',(35.,-9.22632453012935,-13.0695744862984));
#70767=CARTESIAN_POINT('',(34.8617922858584,-13.6777396430533,-40.515309671231));
#70768=CARTESIAN_POINT('',(33.5377160618333,-12.5972287566466,-40.9085834716836));
#70769=CARTESIAN_POINT('',(34.4,-13.22226624086,-40.1803643021789));
#70770=CARTESIAN_POINT('Ctrl Pts',(34.4,-13.22226624086,-40.1803643021789));
#70771=CARTESIAN_POINT('Ctrl Pts',(34.6297825290994,-13.4490085829866,-40.3476538099265));
#70772=CARTESIAN_POINT('Ctrl Pts',(34.8617922858584,-13.6777396430533,-40.515309671231));
#70773=CARTESIAN_POINT('',(33.3226453080309,-12.3365516130268,-40.4610861730024));
#70774=CARTESIAN_POINT('Origin',(26.8550245390365,0.,0.));
#70775=CARTESIAN_POINT('',(33.0966075166785,-11.4327072940916,-36.2088329758586));
#70776=CARTESIAN_POINT('Origin',(17.5,-6.59863075134335,-37.4226946144639));
#70777=CARTESIAN_POINT('',(33.1,-4.97369795887321,-37.7092141076143));
#70778=CARTESIAN_POINT('',(33.1,-4.97369795887321,-37.7092141076143));
#70779=CARTESIAN_POINT('',(30.5,-4.97369795887321,-37.7092141076143));
#70780=CARTESIAN_POINT('',(30.5,-4.97369795887321,-37.7092141076143));
#70781=CARTESIAN_POINT('',(30.5,-5.46610183537931,-37.6223900187809));
#70782=CARTESIAN_POINT('',(30.5,-5.46610183537931,-37.6223900187809));
#70783=CARTESIAN_POINT('',(24.1,-5.8600249365842,-37.5529307477141));
#70784=CARTESIAN_POINT('',(24.1,-5.8600249365842,-37.5529307477141));
#70785=CARTESIAN_POINT('',(23.1,-5.56458261068053,-37.6050252010142));
#70786=CARTESIAN_POINT('',(23.1,-5.56458261068053,-37.6050252010142));
#70787=CARTESIAN_POINT('',(22.4,-5.17065950947565,-37.674484472081));
#70788=CARTESIAN_POINT('',(22.4,-5.17065950947565,-37.674484472081));
#70789=CARTESIAN_POINT('',(21.8,-4.97369795887321,-37.7092141076143));
#70790=CARTESIAN_POINT('',(21.8,-4.97369795887321,-37.7092141076143));
#70791=CARTESIAN_POINT('',(13.2,-4.97369795887321,-37.7092141076143));
#70792=CARTESIAN_POINT('',(13.2,-4.97369795887321,-37.7092141076143));
#70793=CARTESIAN_POINT('',(12.6,-5.17065950947565,-37.674484472081));
#70794=CARTESIAN_POINT('',(12.6,-5.17065950947565,-37.674484472081));
#70795=CARTESIAN_POINT('',(11.9,-5.56458261068053,-37.6050252010142));
#70796=CARTESIAN_POINT('',(11.9,-5.56458261068053,-37.6050252010142));
#70797=CARTESIAN_POINT('',(10.9,-5.8600249365842,-37.5529307477141));
#70798=CARTESIAN_POINT('',(10.9,-5.8600249365842,-37.5529307477141));
#70799=CARTESIAN_POINT('',(4.5,-5.46610183537931,-37.6223900187809));
#70800=CARTESIAN_POINT('',(4.5,-5.46610183537931,-37.6223900187809));
#70801=CARTESIAN_POINT('',(4.5,-4.97369795887321,-37.7092141076143));
#70802=CARTESIAN_POINT('',(4.5,-4.97369795887321,-37.7092141076143));
#70803=CARTESIAN_POINT('',(1.9,-4.97369795887321,-37.7092141076143));
#70804=CARTESIAN_POINT('',(1.9,-4.97369795887321,-37.7092141076143));
#70805=CARTESIAN_POINT('',(1.57538060255632,-5.25132148728275,-37.6602615890763));
#70806=CARTESIAN_POINT('',(0.,-6.59863075134335,-37.4226946144639));
#70807=CARTESIAN_POINT('',(1.57538060255633,-7.94594001540395,-37.1851276398516));
#70808=CARTESIAN_POINT('Ctrl Pts',(1.57538060255632,-5.25132148728275,-37.6602615890763));
#70809=CARTESIAN_POINT('Ctrl Pts',(1.62460345738085,-6.59863075137406,-37.4226946144585));
#70810=CARTESIAN_POINT('Ctrl Pts',(1.57538060255633,-7.94594001540395,-37.1851276398516));
#70811=CARTESIAN_POINT('',(1.9,-8.2235635438135,-37.1361751213135));
#70812=CARTESIAN_POINT('',(1.9,-8.2235635438135,-37.1361751213135));
#70813=CARTESIAN_POINT('',(4.5,-8.2235635438135,-37.1361751213135));
#70814=CARTESIAN_POINT('',(4.5,-8.2235635438135,-37.1361751213135));
#70815=CARTESIAN_POINT('',(4.5,-7.73115966730739,-37.2229992101469));
#70816=CARTESIAN_POINT('',(4.5,-7.73115966730739,-37.2229992101469));
#70817=CARTESIAN_POINT('',(10.9,-7.33723656610251,-37.2924584812137));
#70818=CARTESIAN_POINT('',(10.9,-7.33723656610251,-37.2924584812137));
#70819=CARTESIAN_POINT('',(11.9,-7.63267889200617,-37.2403640279136));
#70820=CARTESIAN_POINT('',(11.9,-7.63267889200617,-37.2403640279136));
#70821=CARTESIAN_POINT('',(12.6,-8.02660199321105,-37.1709047568469));
#70822=CARTESIAN_POINT('',(12.6,-8.02660199321105,-37.1709047568469));
#70823=CARTESIAN_POINT('',(13.2,-8.2235635438135,-37.1361751213135));
#70824=CARTESIAN_POINT('',(13.2,-8.2235635438135,-37.1361751213135));
#70825=CARTESIAN_POINT('',(21.8,-8.2235635438135,-37.1361751213135));
#70826=CARTESIAN_POINT('',(21.8,-8.2235635438135,-37.1361751213135));
#70827=CARTESIAN_POINT('',(22.4,-8.02660199321105,-37.1709047568469));
#70828=CARTESIAN_POINT('',(22.4,-8.02660199321105,-37.1709047568469));
#70829=CARTESIAN_POINT('',(23.1,-7.63267889200617,-37.2403640279136));
#70830=CARTESIAN_POINT('',(23.1,-7.63267889200617,-37.2403640279136));
#70831=CARTESIAN_POINT('',(24.1,-7.33723656610251,-37.2924584812137));
#70832=CARTESIAN_POINT('',(24.1,-7.33723656610251,-37.2924584812137));
#70833=CARTESIAN_POINT('',(30.5,-7.73115966730739,-37.2229992101469));
#70834=CARTESIAN_POINT('',(30.5,-7.73115966730739,-37.2229992101469));
#70835=CARTESIAN_POINT('',(30.5,-8.2235635438135,-37.1361751213135));
#70836=CARTESIAN_POINT('',(30.5,-8.2235635438135,-37.1361751213135));
#70837=CARTESIAN_POINT('',(33.1,-8.2235635438135,-37.1361751213135));
#70838=CARTESIAN_POINT('',(33.1,-8.2235635438135,-37.1361751213135));
#70839=CARTESIAN_POINT('',(35.,-6.59863075134335,-37.4226946144639));
#70840=CARTESIAN_POINT('Origin',(35.,-6.59863075134335,-37.4226946144639));
#70841=CARTESIAN_POINT('',(35.,-6.55273342944652,-42.2540639571139));
#70842=CARTESIAN_POINT('',(35.,-6.77372590470163,-18.9913500169872));
#70843=CARTESIAN_POINT('',(34.8617922858584,-6.4345343521407,-42.2749056435377));
#70844=CARTESIAN_POINT('',(33.5377160618333,-5.30214757522046,-42.4745759849063));
#70845=CARTESIAN_POINT('',(34.4,-6.04414326732376,-41.8659567209931));
#70846=CARTESIAN_POINT('Ctrl Pts',(34.4,-6.04414326732376,-41.8659567209931));
#70847=CARTESIAN_POINT('Ctrl Pts',(34.6297825290996,-6.23839136562319,-42.0700781197309));
#70848=CARTESIAN_POINT('Ctrl Pts',(34.8617922858584,-6.4345343521407,-42.2749056435377));
#70849=CARTESIAN_POINT('',(33.3226453080309,-5.12313779357752,-41.9886110647639));
#70850=CARTESIAN_POINT('Origin',(26.8550245390365,0.,0.));
#70851=CARTESIAN_POINT('',(33.0966075166785,-4.97142091943645,-37.6440082295681));
#70852=CARTESIAN_POINT('Origin',(17.5,-6.98048675513991E-15,-38.));
#70853=CARTESIAN_POINT('',(33.1,1.64999999999999,-38.));
#70854=CARTESIAN_POINT('',(33.1,1.64999999999999,-38.));
#70855=CARTESIAN_POINT('',(30.5,1.64999999999999,-38.));
#70856=CARTESIAN_POINT('',(30.5,1.64999999999999,-38.));
#70857=CARTESIAN_POINT('',(30.5,1.14999999999999,-38.));
#70858=CARTESIAN_POINT('',(30.5,1.14999999999999,-38.));
#70859=CARTESIAN_POINT('',(24.1,0.749999999999993,-38.));
#70860=CARTESIAN_POINT('',(24.1,0.749999999999993,-38.));
#70861=CARTESIAN_POINT('',(23.1,1.04999999999999,-38.));
#70862=CARTESIAN_POINT('',(23.1,1.04999999999999,-38.));
#70863=CARTESIAN_POINT('',(22.4,1.44999999999999,-38.));
#70864=CARTESIAN_POINT('',(22.4,1.44999999999999,-38.));
#70865=CARTESIAN_POINT('',(21.8,1.64999999999999,-38.));
#70866=CARTESIAN_POINT('',(21.8,1.64999999999999,-38.));
#70867=CARTESIAN_POINT('',(13.2,1.64999999999999,-38.));
#70868=CARTESIAN_POINT('',(13.2,1.64999999999999,-38.));
#70869=CARTESIAN_POINT('',(12.6,1.44999999999999,-38.));
#70870=CARTESIAN_POINT('',(12.6,1.44999999999999,-38.));
#70871=CARTESIAN_POINT('',(11.9,1.04999999999999,-38.));
#70872=CARTESIAN_POINT('',(11.9,1.04999999999999,-38.));
#70873=CARTESIAN_POINT('',(10.9,0.749999999999993,-38.));
#70874=CARTESIAN_POINT('',(10.9,0.749999999999993,-38.));
#70875=CARTESIAN_POINT('',(4.5,1.14999999999999,-38.));
#70876=CARTESIAN_POINT('',(4.5,1.14999999999999,-38.));
#70877=CARTESIAN_POINT('',(4.5,1.64999999999999,-38.));
#70878=CARTESIAN_POINT('',(4.5,1.64999999999999,-38.));
#70879=CARTESIAN_POINT('',(1.9,1.64999999999999,-38.));
#70880=CARTESIAN_POINT('',(1.9,1.64999999999999,-38.));
#70881=CARTESIAN_POINT('',(1.57538060255632,1.36809368116733,-38.));
#70882=CARTESIAN_POINT('',(0.,-6.98048675513991E-15,-38.));
#70883=CARTESIAN_POINT('',(1.57538060255632,-1.36809368116734,-38.));
#70884=CARTESIAN_POINT('Ctrl Pts',(1.57538060255632,1.36809368116733,-38.));
#70885=CARTESIAN_POINT('Ctrl Pts',(1.62460345738085,-3.11864423174768E-11,
-38.));
#70886=CARTESIAN_POINT('Ctrl Pts',(1.57538060255632,-1.36809368116734,-38.));
#70887=CARTESIAN_POINT('',(1.9,-1.65000000000001,-38.));
#70888=CARTESIAN_POINT('',(1.9,-1.65000000000001,-38.));
#70889=CARTESIAN_POINT('',(4.5,-1.65000000000001,-38.));
#70890=CARTESIAN_POINT('',(4.5,-1.65000000000001,-38.));
#70891=CARTESIAN_POINT('',(4.5,-1.15000000000001,-38.));
#70892=CARTESIAN_POINT('',(4.5,-1.15000000000001,-38.));
#70893=CARTESIAN_POINT('',(10.9,-0.750000000000007,-38.));
#70894=CARTESIAN_POINT('',(10.9,-0.750000000000007,-38.));
#70895=CARTESIAN_POINT('',(11.9,-1.05000000000001,-38.));
#70896=CARTESIAN_POINT('',(11.9,-1.05000000000001,-38.));
#70897=CARTESIAN_POINT('',(12.6,-1.45000000000001,-38.));
#70898=CARTESIAN_POINT('',(12.6,-1.45000000000001,-38.));
#70899=CARTESIAN_POINT('',(13.2,-1.65000000000001,-38.));
#70900=CARTESIAN_POINT('',(13.2,-1.65000000000001,-38.));
#70901=CARTESIAN_POINT('',(21.8,-1.65000000000001,-38.));
#70902=CARTESIAN_POINT('',(21.8,-1.65000000000001,-38.));
#70903=CARTESIAN_POINT('',(22.4,-1.45000000000001,-38.));
#70904=CARTESIAN_POINT('',(22.4,-1.45000000000001,-38.));
#70905=CARTESIAN_POINT('',(23.1,-1.05000000000001,-38.));
#70906=CARTESIAN_POINT('',(23.1,-1.05000000000001,-38.));
#70907=CARTESIAN_POINT('',(24.1,-0.750000000000007,-38.));
#70908=CARTESIAN_POINT('',(24.1,-0.750000000000007,-38.));
#70909=CARTESIAN_POINT('',(30.5,-1.15000000000001,-38.));
#70910=CARTESIAN_POINT('',(30.5,-1.15000000000001,-38.));
#70911=CARTESIAN_POINT('',(30.5,-1.65000000000001,-38.));
#70912=CARTESIAN_POINT('',(30.5,-1.65000000000001,-38.));
#70913=CARTESIAN_POINT('',(33.1,-1.65000000000001,-38.));
#70914=CARTESIAN_POINT('',(33.1,-1.65000000000001,-38.));
#70915=CARTESIAN_POINT('',(35.,-6.98048675513991E-15,-38.));
#70916=CARTESIAN_POINT('Origin',(35.,-6.98048675513991E-15,-38.));
#70917=CARTESIAN_POINT('',(35.,0.884158520433528,-42.75));
#70918=CARTESIAN_POINT('',(35.,-2.54753088563723,-24.3137984568159));
#70919=CARTESIAN_POINT('',(34.8617922858584,1.0041810090302,-42.75));
#70920=CARTESIAN_POINT('',(33.5377160618333,2.15403667726254,-42.75));
#70921=CARTESIAN_POINT('',(34.4,1.31762794090604,-42.2794732300362));
#70922=CARTESIAN_POINT('Ctrl Pts',(34.4,1.31762794090604,-42.2794732300361));
#70923=CARTESIAN_POINT('Ctrl Pts',(34.6297825290971,1.16177621660823,-42.5142243943513));
#70924=CARTESIAN_POINT('Ctrl Pts',(34.8617922858584,1.0041810090302,-42.75));
#70925=CARTESIAN_POINT('',(33.322645308031,2.24593997529676,-42.240333256585));
#70926=CARTESIAN_POINT('Origin',(26.8550245390365,0.,0.));
#70927=CARTESIAN_POINT('',(33.0966075166785,1.64091956419533,-37.9353893420094));
#70928=CARTESIAN_POINT('Origin',(17.5,6.59863075134334,-37.4226946144639));
#70929=CARTESIAN_POINT('',(33.1,8.22356354381348,-37.1361751213135));
#70930=CARTESIAN_POINT('',(33.1,8.22356354381348,-37.1361751213135));
#70931=CARTESIAN_POINT('',(30.5,8.22356354381348,-37.1361751213135));
#70932=CARTESIAN_POINT('',(30.5,8.22356354381348,-37.1361751213135));
#70933=CARTESIAN_POINT('',(30.5,7.73115966730738,-37.2229992101469));
#70934=CARTESIAN_POINT('',(30.5,7.73115966730738,-37.2229992101469));
#70935=CARTESIAN_POINT('',(24.1,7.33723656610249,-37.2924584812137));
#70936=CARTESIAN_POINT('',(24.1,7.33723656610249,-37.2924584812137));
#70937=CARTESIAN_POINT('',(23.1,7.63267889200616,-37.2403640279136));
#70938=CARTESIAN_POINT('',(23.1,7.63267889200616,-37.2403640279136));
#70939=CARTESIAN_POINT('',(22.4,8.02660199321104,-37.1709047568469));
#70940=CARTESIAN_POINT('',(22.4,8.02660199321104,-37.1709047568469));
#70941=CARTESIAN_POINT('',(21.8,8.22356354381348,-37.1361751213135));
#70942=CARTESIAN_POINT('',(21.8,8.22356354381348,-37.1361751213135));
#70943=CARTESIAN_POINT('',(13.2,8.22356354381348,-37.1361751213135));
#70944=CARTESIAN_POINT('',(13.2,8.22356354381348,-37.1361751213135));
#70945=CARTESIAN_POINT('',(12.6,8.02660199321104,-37.1709047568469));
#70946=CARTESIAN_POINT('',(12.6,8.02660199321104,-37.1709047568469));
#70947=CARTESIAN_POINT('',(11.9,7.63267889200616,-37.2403640279136));
#70948=CARTESIAN_POINT('',(11.9,7.63267889200616,-37.2403640279136));
#70949=CARTESIAN_POINT('',(10.9,7.33723656610249,-37.2924584812137));
#70950=CARTESIAN_POINT('',(10.9,7.33723656610249,-37.2924584812137));
#70951=CARTESIAN_POINT('',(4.5,7.73115966730738,-37.2229992101469));
#70952=CARTESIAN_POINT('',(4.5,7.73115966730738,-37.2229992101469));
#70953=CARTESIAN_POINT('',(4.5,8.22356354381348,-37.1361751213135));
#70954=CARTESIAN_POINT('',(4.5,8.22356354381348,-37.1361751213135));
#70955=CARTESIAN_POINT('',(1.9,8.22356354381348,-37.1361751213135));
#70956=CARTESIAN_POINT('',(1.9,8.22356354381348,-37.1361751213135));
#70957=CARTESIAN_POINT('',(1.57538060255632,7.94594001540394,-37.1851276398516));
#70958=CARTESIAN_POINT('',(0.,6.59863075134334,-37.4226946144639));
#70959=CARTESIAN_POINT('',(1.57538060255633,5.25132148728273,-37.6602615890763));
#70960=CARTESIAN_POINT('Ctrl Pts',(1.57538060255632,7.94594001540394,-37.1851276398516));
#70961=CARTESIAN_POINT('Ctrl Pts',(1.62460345738085,6.59863075131263,-37.4226946144693));
#70962=CARTESIAN_POINT('Ctrl Pts',(1.57538060255633,5.25132148728273,-37.6602615890763));
#70963=CARTESIAN_POINT('',(1.9,4.9736979588732,-37.7092141076143));
#70964=CARTESIAN_POINT('',(1.9,4.9736979588732,-37.7092141076143));
#70965=CARTESIAN_POINT('',(4.5,4.9736979588732,-37.7092141076143));
#70966=CARTESIAN_POINT('',(4.5,4.9736979588732,-37.7092141076143));
#70967=CARTESIAN_POINT('',(4.5,5.4661018353793,-37.6223900187809));
#70968=CARTESIAN_POINT('',(4.5,5.4661018353793,-37.6223900187809));
#70969=CARTESIAN_POINT('',(10.9,5.86002493658418,-37.5529307477141));
#70970=CARTESIAN_POINT('',(10.9,5.86002493658418,-37.5529307477141));
#70971=CARTESIAN_POINT('',(11.9,5.56458261068052,-37.6050252010142));
#70972=CARTESIAN_POINT('',(11.9,5.56458261068052,-37.6050252010142));
#70973=CARTESIAN_POINT('',(12.6,5.17065950947564,-37.674484472081));
#70974=CARTESIAN_POINT('',(12.6,5.17065950947564,-37.674484472081));
#70975=CARTESIAN_POINT('',(13.2,4.9736979588732,-37.7092141076143));
#70976=CARTESIAN_POINT('',(13.2,4.9736979588732,-37.7092141076143));
#70977=CARTESIAN_POINT('',(21.8,4.9736979588732,-37.7092141076143));
#70978=CARTESIAN_POINT('',(21.8,4.9736979588732,-37.7092141076143));
#70979=CARTESIAN_POINT('',(22.4,5.17065950947564,-37.674484472081));
#70980=CARTESIAN_POINT('',(22.4,5.17065950947564,-37.674484472081));
#70981=CARTESIAN_POINT('',(23.1,5.56458261068052,-37.6050252010142));
#70982=CARTESIAN_POINT('',(23.1,5.56458261068052,-37.6050252010142));
#70983=CARTESIAN_POINT('',(24.1,5.86002493658418,-37.5529307477141));
#70984=CARTESIAN_POINT('',(24.1,5.86002493658418,-37.5529307477141));
#70985=CARTESIAN_POINT('',(30.5,5.4661018353793,-37.6223900187809));
#70986=CARTESIAN_POINT('',(30.5,5.4661018353793,-37.6223900187809));
#70987=CARTESIAN_POINT('',(30.5,4.9736979588732,-37.7092141076143));
#70988=CARTESIAN_POINT('',(30.5,4.9736979588732,-37.7092141076143));
#70989=CARTESIAN_POINT('',(33.1,4.9736979588732,-37.7092141076143));
#70990=CARTESIAN_POINT('',(33.1,4.9736979588732,-37.7092141076143));
#70991=CARTESIAN_POINT('',(35.,6.59863075134334,-37.4226946144639));
#70992=CARTESIAN_POINT('Origin',(35.,6.59863075134334,-37.4226946144639));
#70993=CARTESIAN_POINT('',(35.,8.294185761076,-41.9469989254299));
#70994=CARTESIAN_POINT('',(35.,3.24550057858058,-28.4754288467477));
#70995=CARTESIAN_POINT('',(34.8617922858584,8.41238483838183,-41.9261572390061));
#70996=CARTESIAN_POINT('',(33.5377160618333,9.54477161530206,-41.7264868976375));
#70997=CARTESIAN_POINT('',(34.4,8.63936369090331,-41.4083493394303));
#70998=CARTESIAN_POINT('Ctrl Pts',(34.4,8.63936369090331,-41.4083493394303));
#70999=CARTESIAN_POINT('Ctrl Pts',(34.6297825290999,8.5266438163816,-41.6665974739903));
#71000=CARTESIAN_POINT('Ctrl Pts',(34.8617922858584,8.41238483838183,-41.9261572390061));
#71001=CARTESIAN_POINT('',(33.322645308031,9.54677599452212,-41.2086042970448));
#71002=CARTESIAN_POINT('Origin',(26.8550245390365,0.,0.));
#71003=CARTESIAN_POINT('',(33.0966075166785,8.2034015372144,-37.0741228455271));
#71004=CARTESIAN_POINT('Origin',(17.5,12.9967654463754,-35.7083195898645));
#71005=CARTESIAN_POINT('',(33.1,14.5472582706721,-35.1439863533772));
#71006=CARTESIAN_POINT('',(33.1,14.5472582706721,-35.1439863533772));
#71007=CARTESIAN_POINT('',(30.5,14.5472582706721,-35.1439863533772));
#71008=CARTESIAN_POINT('',(30.5,14.5472582706721,-35.1439863533772));
#71009=CARTESIAN_POINT('',(30.5,14.0774119602792,-35.31499642504));
#71010=CARTESIAN_POINT('',(30.5,14.0774119602792,-35.31499642504));
#71011=CARTESIAN_POINT('',(24.1,13.7015349119648,-35.4518044823703));
#71012=CARTESIAN_POINT('',(24.1,13.7015349119648,-35.4518044823703));
#71013=CARTESIAN_POINT('',(23.1,13.9834426982006,-35.3491984393726));
#71014=CARTESIAN_POINT('',(23.1,13.9834426982006,-35.3491984393726));
#71015=CARTESIAN_POINT('',(22.4,14.359319746515,-35.2123903820423));
#71016=CARTESIAN_POINT('',(22.4,14.359319746515,-35.2123903820423));
#71017=CARTESIAN_POINT('',(21.8,14.5472582706721,-35.1439863533772));
#71018=CARTESIAN_POINT('',(21.8,14.5472582706721,-35.1439863533772));
#71019=CARTESIAN_POINT('',(13.2,14.5472582706721,-35.1439863533772));
#71020=CARTESIAN_POINT('',(13.2,14.5472582706721,-35.1439863533772));
#71021=CARTESIAN_POINT('',(12.6,14.359319746515,-35.2123903820423));
#71022=CARTESIAN_POINT('',(12.6,14.359319746515,-35.2123903820423));
#71023=CARTESIAN_POINT('',(11.9,13.9834426982006,-35.3491984393726));
#71024=CARTESIAN_POINT('',(11.9,13.9834426982006,-35.3491984393726));
#71025=CARTESIAN_POINT('',(10.9,13.7015349119648,-35.4518044823703));
#71026=CARTESIAN_POINT('',(10.9,13.7015349119648,-35.4518044823703));
#71027=CARTESIAN_POINT('',(4.5,14.0774119602792,-35.31499642504));
#71028=CARTESIAN_POINT('',(4.5,14.0774119602792,-35.31499642504));
#71029=CARTESIAN_POINT('',(4.5,14.5472582706721,-35.1439863533772));
#71030=CARTESIAN_POINT('',(4.5,14.5472582706721,-35.1439863533772));
#71031=CARTESIAN_POINT('',(1.9,14.5472582706721,-35.1439863533772));
#71032=CARTESIAN_POINT('',(1.9,14.5472582706721,-35.1439863533772));
#71033=CARTESIAN_POINT('',(1.57538060255632,14.2823529831122,-35.2404039929487));
#71034=CARTESIAN_POINT('',(0.,12.9967654463754,-35.7083195898645));
#71035=CARTESIAN_POINT('',(1.57538060255632,11.7111779096386,-36.1762351867803));
#71036=CARTESIAN_POINT('Ctrl Pts',(1.57538060255632,14.2823529831122,-35.2404039929487));
#71037=CARTESIAN_POINT('Ctrl Pts',(1.62460345738085,12.9967654463461,-35.7083195898752));
#71038=CARTESIAN_POINT('Ctrl Pts',(1.57538060255632,11.7111779096386,-36.1762351867803));
#71039=CARTESIAN_POINT('',(1.9,11.4462726220786,-36.2726528263519));
#71040=CARTESIAN_POINT('',(1.9,11.4462726220786,-36.2726528263519));
#71041=CARTESIAN_POINT('',(4.5,11.4462726220786,-36.2726528263519));
#71042=CARTESIAN_POINT('',(4.5,11.4462726220786,-36.2726528263519));
#71043=CARTESIAN_POINT('',(4.5,11.9161189324716,-36.101642754689));
#71044=CARTESIAN_POINT('',(4.5,11.9161189324716,-36.101642754689));
#71045=CARTESIAN_POINT('',(10.9,12.291995980786,-35.9648346973588));
#71046=CARTESIAN_POINT('',(10.9,12.291995980786,-35.9648346973588));
#71047=CARTESIAN_POINT('',(11.9,12.0100881945502,-36.0674407403565));
#71048=CARTESIAN_POINT('',(11.9,12.0100881945502,-36.0674407403565));
#71049=CARTESIAN_POINT('',(12.6,11.6342111462358,-36.2042487976867));
#71050=CARTESIAN_POINT('',(12.6,11.6342111462358,-36.2042487976867));
#71051=CARTESIAN_POINT('',(13.2,11.4462726220786,-36.2726528263519));
#71052=CARTESIAN_POINT('',(13.2,11.4462726220786,-36.2726528263519));
#71053=CARTESIAN_POINT('',(21.8,11.4462726220786,-36.2726528263519));
#71054=CARTESIAN_POINT('',(21.8,11.4462726220786,-36.2726528263519));
#71055=CARTESIAN_POINT('',(22.4,11.6342111462358,-36.2042487976867));
#71056=CARTESIAN_POINT('',(22.4,11.6342111462358,-36.2042487976867));
#71057=CARTESIAN_POINT('',(23.1,12.0100881945502,-36.0674407403565));
#71058=CARTESIAN_POINT('',(23.1,12.0100881945502,-36.0674407403565));
#71059=CARTESIAN_POINT('',(24.1,12.291995980786,-35.9648346973588));
#71060=CARTESIAN_POINT('',(24.1,12.291995980786,-35.9648346973588));
#71061=CARTESIAN_POINT('',(30.5,11.9161189324716,-36.101642754689));
#71062=CARTESIAN_POINT('',(30.5,11.9161189324716,-36.101642754689));
#71063=CARTESIAN_POINT('',(30.5,11.4462726220786,-36.2726528263519));
#71064=CARTESIAN_POINT('',(30.5,11.4462726220786,-36.2726528263519));
#71065=CARTESIAN_POINT('',(33.1,11.4462726220786,-36.2726528263519));
#71066=CARTESIAN_POINT('',(33.1,11.4462726220786,-36.2726528263519));
#71067=CARTESIAN_POINT('',(35.,12.9967654463754,-35.7083195898645));
#71068=CARTESIAN_POINT('Origin',(35.,12.9967654463754,-35.7083195898645));
#71069=CARTESIAN_POINT('',(35.,15.4521983644287,-39.8694595147163));
#71070=CARTESIAN_POINT('',(35.,10.2189962848885,-31.0009272294782));
#71071=CARTESIAN_POINT('',(34.8617922858584,15.5649826112914,-39.8284094059642));
#71072=CARTESIAN_POINT('',(33.5377160618333,16.6454934976981,-39.4351356055115));
#71073=CARTESIAN_POINT('',(34.4,15.6985967468815,-39.2790537077817));
#71074=CARTESIAN_POINT('Ctrl Pts',(34.4,15.6985967468815,-39.2790537077817));
#71075=CARTESIAN_POINT('Ctrl Pts',(34.6297825291022,15.6324336584855,-39.5529520736976));
#71076=CARTESIAN_POINT('Ctrl Pts',(34.8617922858584,15.5649826112914,-39.8284094059642));
#71077=CARTESIAN_POINT('',(33.3226453080309,16.5575380560557,-38.9247727484987));
#71078=CARTESIAN_POINT('Origin',(26.8550245390365,0.,0.));
#71079=CARTESIAN_POINT('',(33.0966075166785,14.5166273056467,-35.0863778867947));
#71080=CARTESIAN_POINT('Origin',(17.5,19.,-32.9089653438087));
#71081=CARTESIAN_POINT('',(33.1,20.4289419162443,-32.0839653438087));
#71082=CARTESIAN_POINT('',(33.1,20.4289419162443,-32.0839653438087));
#71083=CARTESIAN_POINT('',(30.5,20.4289419162443,-32.0839653438087));
#71084=CARTESIAN_POINT('',(30.5,20.4289419162443,-32.0839653438087));
#71085=CARTESIAN_POINT('',(30.5,19.9959292143521,-32.3339653438087));
#71086=CARTESIAN_POINT('',(30.5,19.9959292143521,-32.3339653438087));
#71087=CARTESIAN_POINT('',(24.1,19.6495190528383,-32.5339653438087));
#71088=CARTESIAN_POINT('',(24.1,19.6495190528383,-32.5339653438087));
#71089=CARTESIAN_POINT('',(23.1,19.9093266739737,-32.3839653438087));
#71090=CARTESIAN_POINT('',(23.1,19.9093266739737,-32.3839653438087));
#71091=CARTESIAN_POINT('',(22.4,20.2557368354874,-32.1839653438087));
#71092=CARTESIAN_POINT('',(22.4,20.2557368354874,-32.1839653438087));
#71093=CARTESIAN_POINT('',(21.8,20.4289419162443,-32.0839653438087));
#71094=CARTESIAN_POINT('',(21.8,20.4289419162443,-32.0839653438087));
#71095=CARTESIAN_POINT('',(13.2,20.4289419162443,-32.0839653438087));
#71096=CARTESIAN_POINT('',(13.2,20.4289419162443,-32.0839653438087));
#71097=CARTESIAN_POINT('',(12.6,20.2557368354874,-32.1839653438087));
#71098=CARTESIAN_POINT('',(12.6,20.2557368354874,-32.1839653438087));
#71099=CARTESIAN_POINT('',(11.9,19.9093266739737,-32.3839653438087));
#71100=CARTESIAN_POINT('',(11.9,19.9093266739737,-32.3839653438087));
#71101=CARTESIAN_POINT('',(10.9,19.6495190528383,-32.5339653438087));
#71102=CARTESIAN_POINT('',(10.9,19.6495190528383,-32.5339653438087));
#71103=CARTESIAN_POINT('',(4.5,19.9959292143521,-32.3339653438087));
#71104=CARTESIAN_POINT('',(4.5,19.9959292143521,-32.3339653438087));
#71105=CARTESIAN_POINT('',(4.5,20.4289419162443,-32.0839653438087));
#71106=CARTESIAN_POINT('',(4.5,20.4289419162443,-32.0839653438087));
#71107=CARTESIAN_POINT('',(1.9,20.4289419162443,-32.0839653438087));
#71108=CARTESIAN_POINT('',(1.9,20.4289419162443,-32.0839653438087));
#71109=CARTESIAN_POINT('',(1.57538060255632,20.1848038826479,-32.224918503225));
#71110=CARTESIAN_POINT('',(0.,19.,-32.9089653438087));
#71111=CARTESIAN_POINT('',(1.57538060255632,17.8151961173521,-33.5930121843923));
#71112=CARTESIAN_POINT('Ctrl Pts',(1.57538060255632,20.1848038826479,-32.224918503225));
#71113=CARTESIAN_POINT('Ctrl Pts',(1.62460345738085,18.999999999973,-32.9089653438243));
#71114=CARTESIAN_POINT('Ctrl Pts',(1.57538060255632,17.8151961173521,-33.5930121843923));
#71115=CARTESIAN_POINT('',(1.9,17.5710580837557,-33.7339653438087));
#71116=CARTESIAN_POINT('',(1.9,17.5710580837557,-33.7339653438087));
#71117=CARTESIAN_POINT('',(4.5,17.5710580837557,-33.7339653438087));
#71118=CARTESIAN_POINT('',(4.5,17.5710580837557,-33.7339653438087));
#71119=CARTESIAN_POINT('',(4.5,18.0040707856479,-33.4839653438087));
#71120=CARTESIAN_POINT('',(4.5,18.0040707856479,-33.4839653438087));
#71121=CARTESIAN_POINT('',(10.9,18.3504809471617,-33.2839653438087));
#71122=CARTESIAN_POINT('',(10.9,18.3504809471617,-33.2839653438087));
#71123=CARTESIAN_POINT('',(11.9,18.0906733260263,-33.4339653438087));
#71124=CARTESIAN_POINT('',(11.9,18.0906733260263,-33.4339653438087));
#71125=CARTESIAN_POINT('',(12.6,17.7442631645126,-33.6339653438087));
#71126=CARTESIAN_POINT('',(12.6,17.7442631645126,-33.6339653438087));
#71127=CARTESIAN_POINT('',(13.2,17.5710580837557,-33.7339653438087));
#71128=CARTESIAN_POINT('',(13.2,17.5710580837557,-33.7339653438087));
#71129=CARTESIAN_POINT('',(21.8,17.5710580837557,-33.7339653438087));
#71130=CARTESIAN_POINT('',(21.8,17.5710580837557,-33.7339653438087));
#71131=CARTESIAN_POINT('',(22.4,17.7442631645126,-33.6339653438087));
#71132=CARTESIAN_POINT('',(22.4,17.7442631645126,-33.6339653438087));
#71133=CARTESIAN_POINT('',(23.1,18.0906733260263,-33.4339653438087));
#71134=CARTESIAN_POINT('',(23.1,18.0906733260263,-33.4339653438087));
#71135=CARTESIAN_POINT('',(24.1,18.3504809471617,-33.2839653438087));
#71136=CARTESIAN_POINT('',(24.1,18.3504809471617,-33.2839653438087));
#71137=CARTESIAN_POINT('',(30.5,18.0040707856479,-33.4839653438087));
#71138=CARTESIAN_POINT('',(30.5,18.0040707856479,-33.4839653438087));
#71139=CARTESIAN_POINT('',(30.5,17.5710580837557,-33.7339653438087));
#71140=CARTESIAN_POINT('',(30.5,17.5710580837557,-33.7339653438087));
#71141=CARTESIAN_POINT('',(33.1,17.5710580837557,-33.7339653438087));
#71142=CARTESIAN_POINT('',(33.1,17.5710580837557,-33.7339653438087));
#71143=CARTESIAN_POINT('',(35.,19.,-32.9089653438087));
#71144=CARTESIAN_POINT('Origin',(35.,19.,-32.9089653438087));
#71145=CARTESIAN_POINT('',(35.,22.1407037396679,-36.580506751568));
#71146=CARTESIAN_POINT('',(35.,17.8440832811487,-31.5576770820153));
#71147=CARTESIAN_POINT('',(34.8617922858584,22.2446462638181,-36.5204955072696));
#71148=CARTESIAN_POINT('',(33.5377160618333,23.2404504831928,-35.9455676731535));
#71149=CARTESIAN_POINT('',(34.4,22.2808358845789,-35.9562839053824));
#71150=CARTESIAN_POINT('Ctrl Pts',(34.4,22.2808358845789,-35.9562839053824));
#71151=CARTESIAN_POINT('Ctrl Pts',(34.6297825291023,22.2632399142705,-36.2375102394025));
#71152=CARTESIAN_POINT('Ctrl Pts',(34.8617922858584,22.2446462638181,-36.5204955072696));
#71153=CARTESIAN_POINT('',(33.322645308031,23.0652077022745,-35.4582316768749));
#71154=CARTESIAN_POINT('Origin',(26.8550245390365,0.,0.));
#71155=CARTESIAN_POINT('',(33.0966075166785,20.3887726991648,-32.0325510905359));
#71156=CARTESIAN_POINT('Origin',(17.5,24.4259291680885,-29.1096888385212));
#71157=CARTESIAN_POINT('',(33.1,25.6899024992348,-28.0490892825384));
#71158=CARTESIAN_POINT('',(33.1,25.6899024992348,-28.0490892825384));
#71159=CARTESIAN_POINT('',(30.5,25.6899024992348,-28.0490892825384));
#71160=CARTESIAN_POINT('',(30.5,25.6899024992348,-28.0490892825384));
#71161=CARTESIAN_POINT('',(30.5,25.3068802776753,-28.3704830873817));
#71162=CARTESIAN_POINT('',(30.5,25.3068802776753,-28.3704830873817));
#71163=CARTESIAN_POINT('',(24.1,25.0004625004277,-28.6275981312563));
#71164=CARTESIAN_POINT('',(24.1,25.0004625004277,-28.6275981312563));
#71165=CARTESIAN_POINT('',(23.1,25.2302758333634,-28.4347618483503));
#71166=CARTESIAN_POINT('',(23.1,25.2302758333634,-28.4347618483503));
#71167=CARTESIAN_POINT('',(22.4,25.536693610611,-28.1776468044757));
#71168=CARTESIAN_POINT('',(22.4,25.536693610611,-28.1776468044757));
#71169=CARTESIAN_POINT('',(21.8,25.6899024992348,-28.0490892825384));
#71170=CARTESIAN_POINT('',(21.8,25.6899024992348,-28.0490892825384));
#71171=CARTESIAN_POINT('',(13.2,25.6899024992348,-28.0490892825384));
#71172=CARTESIAN_POINT('',(13.2,25.6899024992348,-28.0490892825384));
#71173=CARTESIAN_POINT('',(12.6,25.536693610611,-28.1776468044757));
#71174=CARTESIAN_POINT('',(12.6,25.536693610611,-28.1776468044757));
#71175=CARTESIAN_POINT('',(11.9,25.2302758333634,-28.4347618483503));
#71176=CARTESIAN_POINT('',(11.9,25.2302758333634,-28.4347618483503));
#71177=CARTESIAN_POINT('',(10.9,25.0004625004277,-28.6275981312563));
#71178=CARTESIAN_POINT('',(10.9,25.0004625004277,-28.6275981312563));
#71179=CARTESIAN_POINT('',(4.5,25.3068802776753,-28.3704830873817));
#71180=CARTESIAN_POINT('',(4.5,25.3068802776753,-28.3704830873817));
#71181=CARTESIAN_POINT('',(4.5,25.6899024992348,-28.0490892825384));
#71182=CARTESIAN_POINT('',(4.5,25.6899024992348,-28.0490892825384));
#71183=CARTESIAN_POINT('',(1.9,25.6899024992348,-28.0490892825384));
#71184=CARTESIAN_POINT('',(1.9,25.6899024992348,-28.0490892825384));
#71185=CARTESIAN_POINT('',(1.57538060255632,25.4739497302129,-28.2302951713764));
#71186=CARTESIAN_POINT('',(0.,24.4259291680885,-29.1096888385212));
#71187=CARTESIAN_POINT('',(1.57538060255632,23.3779086059641,-29.989082505666));
#71188=CARTESIAN_POINT('Ctrl Pts',(1.57538060255632,25.4739497302129,-28.2302951713764));
#71189=CARTESIAN_POINT('Ctrl Pts',(1.62460345738084,24.4259291680646,-29.1096888385412));
#71190=CARTESIAN_POINT('Ctrl Pts',(1.57538060255632,23.3779086059641,-29.989082505666));
#71191=CARTESIAN_POINT('',(1.9,23.1619558369422,-30.170288394504));
#71192=CARTESIAN_POINT('',(1.9,23.1619558369422,-30.170288394504));
#71193=CARTESIAN_POINT('',(4.5,23.1619558369422,-30.170288394504));
#71194=CARTESIAN_POINT('',(4.5,23.1619558369422,-30.170288394504));
#71195=CARTESIAN_POINT('',(4.5,23.5449780585017,-29.8488945896607));
#71196=CARTESIAN_POINT('',(4.5,23.5449780585017,-29.8488945896607));
#71197=CARTESIAN_POINT('',(10.9,23.8513958357493,-29.5917795457861));
#71198=CARTESIAN_POINT('',(10.9,23.8513958357493,-29.5917795457861));
#71199=CARTESIAN_POINT('',(11.9,23.6215825028136,-29.784615828692));
#71200=CARTESIAN_POINT('',(11.9,23.6215825028136,-29.784615828692));
#71201=CARTESIAN_POINT('',(12.6,23.315164725566,-30.0417308725667));
#71202=CARTESIAN_POINT('',(12.6,23.315164725566,-30.0417308725667));
#71203=CARTESIAN_POINT('',(13.2,23.1619558369422,-30.170288394504));
#71204=CARTESIAN_POINT('',(13.2,23.1619558369422,-30.170288394504));
#71205=CARTESIAN_POINT('',(21.8,23.1619558369422,-30.170288394504));
#71206=CARTESIAN_POINT('',(21.8,23.1619558369422,-30.170288394504));
#71207=CARTESIAN_POINT('',(22.4,23.315164725566,-30.0417308725667));
#71208=CARTESIAN_POINT('',(22.4,23.315164725566,-30.0417308725667));
#71209=CARTESIAN_POINT('',(23.1,23.6215825028136,-29.784615828692));
#71210=CARTESIAN_POINT('',(23.1,23.6215825028136,-29.784615828692));
#71211=CARTESIAN_POINT('',(24.1,23.8513958357493,-29.5917795457861));
#71212=CARTESIAN_POINT('',(24.1,23.8513958357493,-29.5917795457861));
#71213=CARTESIAN_POINT('',(30.5,23.5449780585017,-29.8488945896607));
#71214=CARTESIAN_POINT('',(30.5,23.5449780585017,-29.8488945896607));
#71215=CARTESIAN_POINT('',(30.5,23.1619558369422,-30.170288394504));
#71216=CARTESIAN_POINT('',(30.5,23.1619558369422,-30.170288394504));
#71217=CARTESIAN_POINT('',(33.1,23.1619558369422,-30.170288394504));
#71218=CARTESIAN_POINT('',(33.1,23.1619558369422,-30.170288394504));
#71219=CARTESIAN_POINT('',(35.,24.4259291680885,-29.1096888385212));
#71220=CARTESIAN_POINT('Origin',(35.,24.4259291680885,-29.1096888385212));
#71221=CARTESIAN_POINT('',(35.,28.156475035514,-32.1800738014028));
#71222=CARTESIAN_POINT('',(35.,25.5036906911557,-29.9967286690438));
#71223=CARTESIAN_POINT('',(34.8617922858584,28.2484175959528,-32.1029248328492));
#71224=CARTESIAN_POINT('',(33.5377160618333,29.129258140991,-31.3638118563816));
#71225=CARTESIAN_POINT('',(34.4,28.1860830985703,-31.5410006112756));
#71226=CARTESIAN_POINT('Ctrl Pts',(34.4,28.1860830985703,-31.5410006112756));
#71227=CARTESIAN_POINT('Ctrl Pts',(34.6297825290989,28.217588891003,-31.821009993544));
#71228=CARTESIAN_POINT('Ctrl Pts',(34.8617922858584,28.2484175959528,-32.1029248328492));
#71229=CARTESIAN_POINT('',(33.3226453080309,28.872052684018,-30.9143101784803));
#71230=CARTESIAN_POINT('Origin',(26.8550245390365,0.,0.));
#71231=CARTESIAN_POINT('',(33.0966075166785,25.6414155514355,-28.0054314386442));
#71232=CARTESIAN_POINT('Origin',(17.5,29.1096888385212,-24.4259291680885));
#71233=CARTESIAN_POINT('',(33.1,30.1702883945039,-23.1619558369422));
#71234=CARTESIAN_POINT('',(33.1,30.1702883945039,-23.1619558369422));
#71235=CARTESIAN_POINT('',(30.5,30.1702883945039,-23.1619558369422));
#71236=CARTESIAN_POINT('',(30.5,30.1702883945039,-23.1619558369422));
#71237=CARTESIAN_POINT('',(30.5,29.8488945896607,-23.5449780585017));
#71238=CARTESIAN_POINT('',(30.5,29.8488945896607,-23.5449780585017));
#71239=CARTESIAN_POINT('',(24.1,29.5917795457861,-23.8513958357493));
#71240=CARTESIAN_POINT('',(24.1,29.5917795457861,-23.8513958357493));
#71241=CARTESIAN_POINT('',(23.1,29.784615828692,-23.6215825028136));
#71242=CARTESIAN_POINT('',(23.1,29.784615828692,-23.6215825028136));
#71243=CARTESIAN_POINT('',(22.4,30.0417308725666,-23.315164725566));
#71244=CARTESIAN_POINT('',(22.4,30.0417308725666,-23.315164725566));
#71245=CARTESIAN_POINT('',(21.8,30.1702883945039,-23.1619558369422));
#71246=CARTESIAN_POINT('',(21.8,30.1702883945039,-23.1619558369422));
#71247=CARTESIAN_POINT('',(13.2,30.1702883945039,-23.1619558369422));
#71248=CARTESIAN_POINT('',(13.2,30.1702883945039,-23.1619558369422));
#71249=CARTESIAN_POINT('',(12.6,30.0417308725666,-23.315164725566));
#71250=CARTESIAN_POINT('',(12.6,30.0417308725666,-23.315164725566));
#71251=CARTESIAN_POINT('',(11.9,29.784615828692,-23.6215825028136));
#71252=CARTESIAN_POINT('',(11.9,29.784615828692,-23.6215825028136));
#71253=CARTESIAN_POINT('',(10.9,29.5917795457861,-23.8513958357493));
#71254=CARTESIAN_POINT('',(10.9,29.5917795457861,-23.8513958357493));
#71255=CARTESIAN_POINT('',(4.5,29.8488945896607,-23.5449780585017));
#71256=CARTESIAN_POINT('',(4.5,29.8488945896607,-23.5449780585017));
#71257=CARTESIAN_POINT('',(4.5,30.1702883945039,-23.1619558369422));
#71258=CARTESIAN_POINT('',(4.5,30.1702883945039,-23.1619558369422));
#71259=CARTESIAN_POINT('',(1.9,30.1702883945039,-23.1619558369422));
#71260=CARTESIAN_POINT('',(1.9,30.1702883945039,-23.1619558369422));
#71261=CARTESIAN_POINT('',(1.57538060255632,29.989082505666,-23.3779086059641));
#71262=CARTESIAN_POINT('',(0.,29.1096888385212,-24.4259291680885));
#71263=CARTESIAN_POINT('',(1.57538060255632,28.2302951713763,-25.4739497302129));
#71264=CARTESIAN_POINT('Ctrl Pts',(1.57538060255632,29.989082505666,-23.3779086059641));
#71265=CARTESIAN_POINT('Ctrl Pts',(1.62460345738085,29.1096888385011,-24.4259291681124));
#71266=CARTESIAN_POINT('Ctrl Pts',(1.57538060255632,28.2302951713763,-25.4739497302129));
#71267=CARTESIAN_POINT('',(1.9,28.0490892825384,-25.6899024992348));
#71268=CARTESIAN_POINT('',(1.9,28.0490892825384,-25.6899024992348));
#71269=CARTESIAN_POINT('',(4.5,28.0490892825384,-25.6899024992348));
#71270=CARTESIAN_POINT('',(4.5,28.0490892825384,-25.6899024992348));
#71271=CARTESIAN_POINT('',(4.5,28.3704830873816,-25.3068802776753));
#71272=CARTESIAN_POINT('',(4.5,28.3704830873816,-25.3068802776753));
#71273=CARTESIAN_POINT('',(10.9,28.6275981312562,-25.0004625004277));
#71274=CARTESIAN_POINT('',(10.9,28.6275981312562,-25.0004625004277));
#71275=CARTESIAN_POINT('',(11.9,28.4347618483503,-25.2302758333634));
#71276=CARTESIAN_POINT('',(11.9,28.4347618483503,-25.2302758333634));
#71277=CARTESIAN_POINT('',(12.6,28.1776468044757,-25.536693610611));
#71278=CARTESIAN_POINT('',(12.6,28.1776468044757,-25.536693610611));
#71279=CARTESIAN_POINT('',(13.2,28.0490892825384,-25.6899024992348));
#71280=CARTESIAN_POINT('',(13.2,28.0490892825384,-25.6899024992348));
#71281=CARTESIAN_POINT('',(21.8,28.0490892825384,-25.6899024992348));
#71282=CARTESIAN_POINT('',(21.8,28.0490892825384,-25.6899024992348));
#71283=CARTESIAN_POINT('',(22.4,28.1776468044757,-25.536693610611));
#71284=CARTESIAN_POINT('',(22.4,28.1776468044757,-25.536693610611));
#71285=CARTESIAN_POINT('',(23.1,28.4347618483503,-25.2302758333634));
#71286=CARTESIAN_POINT('',(23.1,28.4347618483503,-25.2302758333634));
#71287=CARTESIAN_POINT('',(24.1,28.6275981312562,-25.0004625004277));
#71288=CARTESIAN_POINT('',(24.1,28.6275981312562,-25.0004625004277));
#71289=CARTESIAN_POINT('',(30.5,28.3704830873816,-25.3068802776753));
#71290=CARTESIAN_POINT('',(30.5,28.3704830873816,-25.3068802776753));
#71291=CARTESIAN_POINT('',(30.5,28.0490892825384,-25.6899024992348));
#71292=CARTESIAN_POINT('',(30.5,28.0490892825384,-25.6899024992348));
#71293=CARTESIAN_POINT('',(33.1,28.0490892825384,-25.6899024992348));
#71294=CARTESIAN_POINT('',(33.1,28.0490892825384,-25.6899024992348));
#71295=CARTESIAN_POINT('',(35.,29.1096888385212,-24.4259291680885));
#71296=CARTESIAN_POINT('Origin',(35.,29.1096888385212,-24.4259291680885));
#71297=CARTESIAN_POINT('',(35.,33.3167260852698,-26.8018655926852));
#71298=CARTESIAN_POINT('',(35.,32.5577823964916,-26.3732499544995));
#71299=CARTESIAN_POINT('',(34.8617922858584,33.3938750538235,-26.7099230322464));
#71300=CARTESIAN_POINT('',(33.5377160618333,34.132988030291,-25.8290824872081));
#71301=CARTESIAN_POINT('',(34.4,33.234910440458,-26.1673599741116));
#71302=CARTESIAN_POINT('Ctrl Pts',(34.4,33.234910440458,-26.1673599741116));
#71303=CARTESIAN_POINT('Ctrl Pts',(34.629782529103,33.3145607080724,-26.4376444612486));
#71304=CARTESIAN_POINT('Ctrl Pts',(34.8617922858584,33.3938750538235,-26.7099230322464));
#71305=CARTESIAN_POINT('',(33.3226453080309,33.8016349549212,-25.4310730087083));
#71306=CARTESIAN_POINT('Origin',(26.8550245390365,0.,0.));
#71307=CARTESIAN_POINT('',(33.0966075166785,30.1149569673582,-23.1273809239214));
#71308=CARTESIAN_POINT('Origin',(17.5,32.9089653438087,-19.));
#71309=CARTESIAN_POINT('',(33.1,33.7339653438087,-17.5710580837557));
#71310=CARTESIAN_POINT('',(33.1,33.7339653438087,-17.5710580837557));
#71311=CARTESIAN_POINT('',(30.5,33.7339653438087,-17.5710580837557));
#71312=CARTESIAN_POINT('',(30.5,33.7339653438087,-17.5710580837557));
#71313=CARTESIAN_POINT('',(30.5,33.4839653438087,-18.0040707856479));
#71314=CARTESIAN_POINT('',(30.5,33.4839653438087,-18.0040707856479));
#71315=CARTESIAN_POINT('',(24.1,33.2839653438087,-18.3504809471617));
#71316=CARTESIAN_POINT('',(24.1,33.2839653438087,-18.3504809471617));
#71317=CARTESIAN_POINT('',(23.1,33.4339653438087,-18.0906733260264));
#71318=CARTESIAN_POINT('',(23.1,33.4339653438087,-18.0906733260264));
#71319=CARTESIAN_POINT('',(22.4,33.6339653438087,-17.7442631645126));
#71320=CARTESIAN_POINT('',(22.4,33.6339653438087,-17.7442631645126));
#71321=CARTESIAN_POINT('',(21.8,33.7339653438087,-17.5710580837557));
#71322=CARTESIAN_POINT('',(21.8,33.7339653438087,-17.5710580837557));
#71323=CARTESIAN_POINT('',(13.2,33.7339653438087,-17.5710580837557));
#71324=CARTESIAN_POINT('',(13.2,33.7339653438087,-17.5710580837557));
#71325=CARTESIAN_POINT('',(12.6,33.6339653438087,-17.7442631645126));
#71326=CARTESIAN_POINT('',(12.6,33.6339653438087,-17.7442631645126));
#71327=CARTESIAN_POINT('',(11.9,33.4339653438087,-18.0906733260264));
#71328=CARTESIAN_POINT('',(11.9,33.4339653438087,-18.0906733260264));
#71329=CARTESIAN_POINT('',(10.9,33.2839653438087,-18.3504809471617));
#71330=CARTESIAN_POINT('',(10.9,33.2839653438087,-18.3504809471617));
#71331=CARTESIAN_POINT('',(4.5,33.4839653438087,-18.0040707856479));
#71332=CARTESIAN_POINT('',(4.5,33.4839653438087,-18.0040707856479));
#71333=CARTESIAN_POINT('',(4.5,33.7339653438087,-17.5710580837557));
#71334=CARTESIAN_POINT('',(4.5,33.7339653438087,-17.5710580837557));
#71335=CARTESIAN_POINT('',(1.9,33.7339653438087,-17.5710580837557));
#71336=CARTESIAN_POINT('',(1.9,33.7339653438087,-17.5710580837557));
#71337=CARTESIAN_POINT('',(1.57538060255633,33.5930121843923,-17.8151961173521));
#71338=CARTESIAN_POINT('',(0.,32.9089653438087,-19.));
#71339=CARTESIAN_POINT('',(1.57538060255632,32.224918503225,-20.1848038826479));
#71340=CARTESIAN_POINT('Ctrl Pts',(1.57538060255633,33.5930121843923,-17.8151961173521));
#71341=CARTESIAN_POINT('Ctrl Pts',(1.62460345738085,32.9089653437931,-19.000000000027));
#71342=CARTESIAN_POINT('Ctrl Pts',(1.57538060255632,32.224918503225,-20.1848038826479));
#71343=CARTESIAN_POINT('',(1.9,32.0839653438087,-20.4289419162443));
#71344=CARTESIAN_POINT('',(1.9,32.0839653438087,-20.4289419162443));
#71345=CARTESIAN_POINT('',(4.5,32.0839653438087,-20.4289419162443));
#71346=CARTESIAN_POINT('',(4.5,32.0839653438087,-20.4289419162443));
#71347=CARTESIAN_POINT('',(4.5,32.3339653438087,-19.9959292143521));
#71348=CARTESIAN_POINT('',(4.5,32.3339653438087,-19.9959292143521));
#71349=CARTESIAN_POINT('',(10.9,32.5339653438087,-19.6495190528383));
#71350=CARTESIAN_POINT('',(10.9,32.5339653438087,-19.6495190528383));
#71351=CARTESIAN_POINT('',(11.9,32.3839653438087,-19.9093266739737));
#71352=CARTESIAN_POINT('',(11.9,32.3839653438087,-19.9093266739737));
#71353=CARTESIAN_POINT('',(12.6,32.1839653438087,-20.2557368354875));
#71354=CARTESIAN_POINT('',(12.6,32.1839653438087,-20.2557368354875));
#71355=CARTESIAN_POINT('',(13.2,32.0839653438087,-20.4289419162443));
#71356=CARTESIAN_POINT('',(13.2,32.0839653438087,-20.4289419162443));
#71357=CARTESIAN_POINT('',(21.8,32.0839653438087,-20.4289419162443));
#71358=CARTESIAN_POINT('',(21.8,32.0839653438087,-20.4289419162443));
#71359=CARTESIAN_POINT('',(22.4,32.1839653438087,-20.2557368354875));
#71360=CARTESIAN_POINT('',(22.4,32.1839653438087,-20.2557368354875));
#71361=CARTESIAN_POINT('',(23.1,32.3839653438087,-19.9093266739737));
#71362=CARTESIAN_POINT('',(23.1,32.3839653438087,-19.9093266739737));
#71363=CARTESIAN_POINT('',(24.1,32.5339653438087,-19.6495190528383));
#71364=CARTESIAN_POINT('',(24.1,32.5339653438087,-19.6495190528383));
#71365=CARTESIAN_POINT('',(30.5,32.3339653438087,-19.9959292143521));
#71366=CARTESIAN_POINT('',(30.5,32.3339653438087,-19.9959292143521));
#71367=CARTESIAN_POINT('',(30.5,32.0839653438087,-20.4289419162443));
#71368=CARTESIAN_POINT('',(30.5,32.0839653438087,-20.4289419162443));
#71369=CARTESIAN_POINT('',(33.1,32.0839653438087,-20.4289419162443));
#71370=CARTESIAN_POINT('',(33.1,32.0839653438087,-20.4289419162443));
#71371=CARTESIAN_POINT('',(35.,32.9089653438087,-19.));
#71372=CARTESIAN_POINT('Origin',(35.,32.9089653438087,-19.));
#71373=CARTESIAN_POINT('',(35.,37.4646652720015,-20.6092962603321));
#71374=CARTESIAN_POINT('',(35.,38.4119309417395,-20.943916872725));
#71375=CARTESIAN_POINT('',(34.8617922858584,37.5246765162998,-20.505353736182));
#71376=CARTESIAN_POINT('',(33.5377160618333,38.099604350416,-19.5095495168072));
#71377=CARTESIAN_POINT('',(34.4,37.2739118462884,-19.9986373454573));
#71378=CARTESIAN_POINT('Ctrl Pts',(34.4,37.2739118462884,-19.9986373454573));
#71379=CARTESIAN_POINT('Ctrl Pts',(34.6297825290997,37.3992864560058,-20.2509844800833));
#71380=CARTESIAN_POINT('Ctrl Pts',(34.8617922858584,37.5246765162998,-20.505353736182));
#71381=CARTESIAN_POINT('',(33.3226453080309,37.7041716521717,-19.1751255543105));
#71382=CARTESIAN_POINT('Origin',(26.8550245390365,0.,0.));
#71383=CARTESIAN_POINT('',(33.0966075166785,33.6734706547313,-17.5466166428447));
#71384=CARTESIAN_POINT('Origin',(17.5,35.7083195898645,-12.9967654463754));
#71385=CARTESIAN_POINT('',(33.1,36.2726528263519,-11.4462726220787));
#71386=CARTESIAN_POINT('',(33.1,36.2726528263519,-11.4462726220787));
#71387=CARTESIAN_POINT('',(30.5,36.2726528263519,-11.4462726220787));
#71388=CARTESIAN_POINT('',(30.5,36.2726528263519,-11.4462726220787));
#71389=CARTESIAN_POINT('',(30.5,36.101642754689,-11.9161189324716));
#71390=CARTESIAN_POINT('',(30.5,36.101642754689,-11.9161189324716));
#71391=CARTESIAN_POINT('',(24.1,35.9648346973588,-12.291995980786));
#71392=CARTESIAN_POINT('',(24.1,35.9648346973588,-12.291995980786));
#71393=CARTESIAN_POINT('',(23.1,36.0674407403565,-12.0100881945502));
#71394=CARTESIAN_POINT('',(23.1,36.0674407403565,-12.0100881945502));
#71395=CARTESIAN_POINT('',(22.4,36.2042487976867,-11.6342111462359));
#71396=CARTESIAN_POINT('',(22.4,36.2042487976867,-11.6342111462359));
#71397=CARTESIAN_POINT('',(21.8,36.2726528263519,-11.4462726220787));
#71398=CARTESIAN_POINT('',(21.8,36.2726528263519,-11.4462726220787));
#71399=CARTESIAN_POINT('',(13.2,36.2726528263519,-11.4462726220787));
#71400=CARTESIAN_POINT('',(13.2,36.2726528263519,-11.4462726220787));
#71401=CARTESIAN_POINT('',(12.6,36.2042487976867,-11.6342111462359));
#71402=CARTESIAN_POINT('',(12.6,36.2042487976867,-11.6342111462359));
#71403=CARTESIAN_POINT('',(11.9,36.0674407403565,-12.0100881945502));
#71404=CARTESIAN_POINT('',(11.9,36.0674407403565,-12.0100881945502));
#71405=CARTESIAN_POINT('',(10.9,35.9648346973588,-12.291995980786));
#71406=CARTESIAN_POINT('',(10.9,35.9648346973588,-12.291995980786));
#71407=CARTESIAN_POINT('',(4.5,36.101642754689,-11.9161189324716));
#71408=CARTESIAN_POINT('',(4.5,36.101642754689,-11.9161189324716));
#71409=CARTESIAN_POINT('',(4.5,36.2726528263519,-11.4462726220787));
#71410=CARTESIAN_POINT('',(4.5,36.2726528263519,-11.4462726220787));
#71411=CARTESIAN_POINT('',(1.9,36.2726528263519,-11.4462726220787));
#71412=CARTESIAN_POINT('',(1.9,36.2726528263519,-11.4462726220787));
#71413=CARTESIAN_POINT('',(1.57538060255633,36.1762351867803,-11.7111779096387));
#71414=CARTESIAN_POINT('',(0.,35.7083195898645,-12.9967654463754));
#71415=CARTESIAN_POINT('',(1.57538060255633,35.2404039929487,-14.2823529831122));
#71416=CARTESIAN_POINT('Ctrl Pts',(1.57538060255633,36.1762351867803,-11.7111779096387));
#71417=CARTESIAN_POINT('Ctrl Pts',(1.62460345738085,35.7083195898538,-12.9967654464047));
#71418=CARTESIAN_POINT('Ctrl Pts',(1.57538060255633,35.2404039929487,-14.2823529831122));
#71419=CARTESIAN_POINT('',(1.9,35.1439863533772,-14.5472582706722));
#71420=CARTESIAN_POINT('',(1.9,35.1439863533772,-14.5472582706722));
#71421=CARTESIAN_POINT('',(4.5,35.1439863533772,-14.5472582706722));
#71422=CARTESIAN_POINT('',(4.5,35.1439863533772,-14.5472582706722));
#71423=CARTESIAN_POINT('',(4.5,35.31499642504,-14.0774119602792));
#71424=CARTESIAN_POINT('',(4.5,35.31499642504,-14.0774119602792));
#71425=CARTESIAN_POINT('',(10.9,35.4518044823703,-13.7015349119649));
#71426=CARTESIAN_POINT('',(10.9,35.4518044823703,-13.7015349119649));
#71427=CARTESIAN_POINT('',(11.9,35.3491984393726,-13.9834426982006));
#71428=CARTESIAN_POINT('',(11.9,35.3491984393726,-13.9834426982006));
#71429=CARTESIAN_POINT('',(12.6,35.2123903820423,-14.359319746515));
#71430=CARTESIAN_POINT('',(12.6,35.2123903820423,-14.359319746515));
#71431=CARTESIAN_POINT('',(13.2,35.1439863533772,-14.5472582706722));
#71432=CARTESIAN_POINT('',(13.2,35.1439863533772,-14.5472582706722));
#71433=CARTESIAN_POINT('',(21.8,35.1439863533772,-14.5472582706722));
#71434=CARTESIAN_POINT('',(21.8,35.1439863533772,-14.5472582706722));
#71435=CARTESIAN_POINT('',(22.4,35.2123903820423,-14.359319746515));
#71436=CARTESIAN_POINT('',(22.4,35.2123903820423,-14.359319746515));
#71437=CARTESIAN_POINT('',(23.1,35.3491984393726,-13.9834426982006));
#71438=CARTESIAN_POINT('',(23.1,35.3491984393726,-13.9834426982006));
#71439=CARTESIAN_POINT('',(24.1,35.4518044823703,-13.7015349119649));
#71440=CARTESIAN_POINT('',(24.1,35.4518044823703,-13.7015349119649));
#71441=CARTESIAN_POINT('',(30.5,35.31499642504,-14.0774119602792));
#71442=CARTESIAN_POINT('',(30.5,35.31499642504,-14.0774119602792));
#71443=CARTESIAN_POINT('',(30.5,35.1439863533772,-14.5472582706722));
#71444=CARTESIAN_POINT('',(30.5,35.1439863533772,-14.5472582706722));
#71445=CARTESIAN_POINT('',(33.1,35.1439863533772,-14.5472582706722));
#71446=CARTESIAN_POINT('',(33.1,35.1439863533772,-14.5472582706722));
#71447=CARTESIAN_POINT('',(35.,35.7083195898645,-12.9967654463754));
#71448=CARTESIAN_POINT('Origin',(35.,35.7083195898645,-12.9967654463754));
#71449=CARTESIAN_POINT('',(35.,40.4742595624789,-13.790523889916));
#71450=CARTESIAN_POINT('',(35.,42.5812236707767,-14.1414348457417));
#71451=CARTESIAN_POINT('',(34.8617922858584,40.515309671231,-13.6777396430533));
#71452=CARTESIAN_POINT('',(33.5377160618333,40.9085834716836,-12.5972287566466));
#71453=CARTESIAN_POINT('',(34.4,40.1803643021789,-13.22226624086));
#71454=CARTESIAN_POINT('Ctrl Pts',(34.4,40.1803643021789,-13.22226624086));
#71455=CARTESIAN_POINT('Ctrl Pts',(34.6297825290978,40.3476538099254,-13.4490085829851));
#71456=CARTESIAN_POINT('Ctrl Pts',(34.8617922858584,40.515309671231,-13.6777396430533));
#71457=CARTESIAN_POINT('',(33.322645308031,40.4610861730024,-12.3365516130268));
#71458=CARTESIAN_POINT('Origin',(26.8550245390365,0.,0.));
#71459=CARTESIAN_POINT('',(33.0966075166785,36.2088329758586,-11.4327072940916));
#71460=CARTESIAN_POINT('Origin',(17.5,37.4226946144639,-6.59863075134336));
#71461=CARTESIAN_POINT('',(33.1,37.7092141076143,-4.97369795887321));
#71462=CARTESIAN_POINT('',(33.1,37.7092141076143,-4.97369795887321));
#71463=CARTESIAN_POINT('',(30.5,37.7092141076143,-4.97369795887321));
#71464=CARTESIAN_POINT('',(30.5,37.7092141076143,-4.97369795887321));
#71465=CARTESIAN_POINT('',(30.5,37.6223900187809,-5.46610183537932));
#71466=CARTESIAN_POINT('',(30.5,37.6223900187809,-5.46610183537932));
#71467=CARTESIAN_POINT('',(24.1,37.5529307477141,-5.8600249365842));
#71468=CARTESIAN_POINT('',(24.1,37.5529307477141,-5.8600249365842));
#71469=CARTESIAN_POINT('',(23.1,37.6050252010142,-5.56458261068054));
#71470=CARTESIAN_POINT('',(23.1,37.6050252010142,-5.56458261068054));
#71471=CARTESIAN_POINT('',(22.4,37.674484472081,-5.17065950947565));
#71472=CARTESIAN_POINT('',(22.4,37.674484472081,-5.17065950947565));
#71473=CARTESIAN_POINT('',(21.8,37.7092141076143,-4.97369795887321));
#71474=CARTESIAN_POINT('',(21.8,37.7092141076143,-4.97369795887321));
#71475=CARTESIAN_POINT('',(13.2,37.7092141076143,-4.97369795887321));
#71476=CARTESIAN_POINT('',(13.2,37.7092141076143,-4.97369795887321));
#71477=CARTESIAN_POINT('',(12.6,37.674484472081,-5.17065950947565));
#71478=CARTESIAN_POINT('',(12.6,37.674484472081,-5.17065950947565));
#71479=CARTESIAN_POINT('',(11.9,37.6050252010142,-5.56458261068054));
#71480=CARTESIAN_POINT('',(11.9,37.6050252010142,-5.56458261068054));
#71481=CARTESIAN_POINT('',(10.9,37.5529307477141,-5.8600249365842));
#71482=CARTESIAN_POINT('',(10.9,37.5529307477141,-5.8600249365842));
#71483=CARTESIAN_POINT('',(4.5,37.6223900187809,-5.46610183537932));
#71484=CARTESIAN_POINT('',(4.5,37.6223900187809,-5.46610183537932));
#71485=CARTESIAN_POINT('',(4.5,37.7092141076143,-4.97369795887321));
#71486=CARTESIAN_POINT('',(4.5,37.7092141076143,-4.97369795887321));
#71487=CARTESIAN_POINT('',(1.9,37.7092141076143,-4.97369795887321));
#71488=CARTESIAN_POINT('',(1.9,37.7092141076143,-4.97369795887321));
#71489=CARTESIAN_POINT('',(1.57538060255632,37.6602615890763,-5.25132148728275));
#71490=CARTESIAN_POINT('',(0.,37.4226946144639,-6.59863075134336));
#71491=CARTESIAN_POINT('',(1.57538060255632,37.1851276398516,-7.94594001540395));
#71492=CARTESIAN_POINT('Ctrl Pts',(1.57538060255632,37.6602615890763,-5.25132148728275));
#71493=CARTESIAN_POINT('Ctrl Pts',(1.62460345738085,37.4226946144585,-6.59863075137406));
#71494=CARTESIAN_POINT('Ctrl Pts',(1.57538060255632,37.1851276398516,-7.94594001540395));
#71495=CARTESIAN_POINT('',(1.9,37.1361751213135,-8.2235635438135));
#71496=CARTESIAN_POINT('',(1.9,37.1361751213135,-8.2235635438135));
#71497=CARTESIAN_POINT('',(4.5,37.1361751213135,-8.2235635438135));
#71498=CARTESIAN_POINT('',(4.5,37.1361751213135,-8.2235635438135));
#71499=CARTESIAN_POINT('',(4.5,37.2229992101469,-7.7311596673074));
#71500=CARTESIAN_POINT('',(4.5,37.2229992101469,-7.7311596673074));
#71501=CARTESIAN_POINT('',(10.9,37.2924584812137,-7.33723656610251));
#71502=CARTESIAN_POINT('',(10.9,37.2924584812137,-7.33723656610251));
#71503=CARTESIAN_POINT('',(11.9,37.2403640279136,-7.63267889200617));
#71504=CARTESIAN_POINT('',(11.9,37.2403640279136,-7.63267889200617));
#71505=CARTESIAN_POINT('',(12.6,37.1709047568469,-8.02660199321106));
#71506=CARTESIAN_POINT('',(12.6,37.1709047568469,-8.02660199321106));
#71507=CARTESIAN_POINT('',(13.2,37.1361751213135,-8.2235635438135));
#71508=CARTESIAN_POINT('',(13.2,37.1361751213135,-8.2235635438135));
#71509=CARTESIAN_POINT('',(21.8,37.1361751213135,-8.2235635438135));
#71510=CARTESIAN_POINT('',(21.8,37.1361751213135,-8.2235635438135));
#71511=CARTESIAN_POINT('',(22.4,37.1709047568469,-8.02660199321106));
#71512=CARTESIAN_POINT('',(22.4,37.1709047568469,-8.02660199321106));
#71513=CARTESIAN_POINT('',(23.1,37.2403640279136,-7.63267889200617));
#71514=CARTESIAN_POINT('',(23.1,37.2403640279136,-7.63267889200617));
#71515=CARTESIAN_POINT('',(24.1,37.2924584812137,-7.33723656610251));
#71516=CARTESIAN_POINT('',(24.1,37.2924584812137,-7.33723656610251));
#71517=CARTESIAN_POINT('',(30.5,37.2229992101469,-7.7311596673074));
#71518=CARTESIAN_POINT('',(30.5,37.2229992101469,-7.7311596673074));
#71519=CARTESIAN_POINT('',(30.5,37.1361751213135,-8.2235635438135));
#71520=CARTESIAN_POINT('',(30.5,37.1361751213135,-8.2235635438135));
#71521=CARTESIAN_POINT('',(33.1,37.1361751213135,-8.2235635438135));
#71522=CARTESIAN_POINT('',(33.1,37.1361751213135,-8.2235635438135));
#71523=CARTESIAN_POINT('',(35.,37.4226946144639,-6.59863075134336));
#71524=CARTESIAN_POINT('Origin',(35.,37.4226946144639,-6.59863075134336));
#71525=CARTESIAN_POINT('',(35.,42.2540639571139,-6.55273342944653));
#71526=CARTESIAN_POINT('',(35.,44.7420297840206,-6.52909810779604));
#71527=CARTESIAN_POINT('',(34.8617922858584,42.2749056435377,-6.4345343521407));
#71528=CARTESIAN_POINT('',(33.5377160618333,42.4745759849063,-5.30214757522046));
#71529=CARTESIAN_POINT('',(34.4,41.8659567209931,-6.04414326732376));
#71530=CARTESIAN_POINT('Ctrl Pts',(34.4,41.8659567209931,-6.04414326732376));
#71531=CARTESIAN_POINT('Ctrl Pts',(34.6297825290999,42.0700781197312,-6.23839136562344));
#71532=CARTESIAN_POINT('Ctrl Pts',(34.8617922858584,42.2749056435377,-6.4345343521407));
#71533=CARTESIAN_POINT('',(33.3226453080309,41.9886110647639,-5.12313779357752));
#71534=CARTESIAN_POINT('Origin',(26.8550245390365,0.,0.));
#71535=CARTESIAN_POINT('',(33.0966075166785,37.6440082295681,-4.97142091943645));
#71536=CARTESIAN_POINT('Origin',(0.8,0.,0.));
#71537=CARTESIAN_POINT('',(0.,38.9456055698919,-7.1693658572013));
#71538=CARTESIAN_POINT('',(2.77555756156289E-16,39.0489657041001,-6.5831814071929));
#71539=CARTESIAN_POINT('Origin',(0.,0.,0.));
#71540=CARTESIAN_POINT('Ctrl Pts',(1.57538060255632,37.1851276398516,-7.94594001540395));
#71541=CARTESIAN_POINT('Ctrl Pts',(0.801841055748964,38.0570140694246,-7.56742453339957));
#71542=CARTESIAN_POINT('Ctrl Pts',(-5.55111512312578E-16,38.9456055698919,
-7.1693658572013));
#71543=CARTESIAN_POINT('Ctrl Pts',(-1.38777878078145E-16,39.0489657041001,
-6.5831814071929));
#71544=CARTESIAN_POINT('Ctrl Pts',(0.801841055750455,38.350106913702,-5.90521241418052));
#71545=CARTESIAN_POINT('Ctrl Pts',(1.57538060255632,37.6602615890763,-5.25132148728275));
#71546=CARTESIAN_POINT('Origin',(0.8,0.,0.));
#71547=CARTESIAN_POINT('',(-1.38777878078145E-16,37.1089869948545,-13.8232805156997));
#71548=CARTESIAN_POINT('',(2.77555756156289E-16,37.3125667178958,-13.2639498235849));
#71549=CARTESIAN_POINT('Origin',(0.,0.,0.));
#71550=CARTESIAN_POINT('Ctrl Pts',(1.57538060255633,35.2404039929487,-14.2823529831122));
#71551=CARTESIAN_POINT('Ctrl Pts',(0.801841055749845,36.1647730322062,-14.0609894914273));
#71552=CARTESIAN_POINT('Ctrl Pts',(-2.77555756156289E-16,37.1089869948545,
-13.8232805156997));
#71553=CARTESIAN_POINT('Ctrl Pts',(9.71445146547012E-16,37.3125667178958,
-13.2639498235849));
#71554=CARTESIAN_POINT('Ctrl Pts',(0.801841055750823,36.742053243002,-12.4749251475649));
#71555=CARTESIAN_POINT('Ctrl Pts',(1.57538060255633,36.1762351867803,-11.7111779096387));
#71556=CARTESIAN_POINT('Origin',(0.8,0.,0.));
#71557=CARTESIAN_POINT('',(-6.93889390390723E-16,34.1448306280318,-20.0571817906459));
#71558=CARTESIAN_POINT('',(-5.55111512312578E-16,34.4424442730379,-19.5416998364696));
#71559=CARTESIAN_POINT('Origin',(0.,0.,0.));
#71560=CARTESIAN_POINT('Ctrl Pts',(1.57538060255632,32.224918503225,-20.1848038826479));
#71561=CARTESIAN_POINT('Ctrl Pts',(0.801841055749468,33.1736836666637,-20.1273183989615));
#71562=CARTESIAN_POINT('Ctrl Pts',(-1.11022302462516E-15,34.1448306280318,
-20.0571817906459));
#71563=CARTESIAN_POINT('Ctrl Pts',(-8.32667268468867E-16,34.4424442730379,
-19.5416998364696));
#71564=CARTESIAN_POINT('Ctrl Pts',(0.801841055749988,34.0176108768901,-18.6655935929584));
#71565=CARTESIAN_POINT('Ctrl Pts',(1.57538060255633,33.5930121843923,-17.8151961173521));
#71566=CARTESIAN_POINT('Origin',(0.8,0.,0.));
#71567=CARTESIAN_POINT('',(2.77555756156289E-16,30.1432008606945,-25.6816557463071));
#71568=CARTESIAN_POINT('',(-4.16333634234434E-16,30.5258055876616,-25.2256851884005));
#71569=CARTESIAN_POINT('Origin',(0.,0.,0.));
#71570=CARTESIAN_POINT('Ctrl Pts',(1.57538060255632,28.2302951713763,-25.4739497302129));
#71571=CARTESIAN_POINT('Ctrl Pts',(0.801841055749793,29.1746287096027,-25.5820889218578));
#71572=CARTESIAN_POINT('Ctrl Pts',(-1.11022302462516E-15,30.1432008606945,
-25.6816557463071));
#71573=CARTESIAN_POINT('Ctrl Pts',(-1.38777878078145E-16,30.5258055876616,
-25.2256851884005));
#71574=CARTESIAN_POINT('Ctrl Pts',(0.801841055749945,30.2595606180251,-24.2891174222752));
#71575=CARTESIAN_POINT('Ctrl Pts',(1.57538060255632,29.989082505666,-23.3779086059641));
#71576=CARTESIAN_POINT('Origin',(0.8,0.,0.));
#71577=CARTESIAN_POINT('',(-4.16333634234434E-16,25.2256851884005,-30.5258055876616));
#71578=CARTESIAN_POINT('',(4.16333634234434E-16,25.6816557463071,-30.1432008606945));
#71579=CARTESIAN_POINT('Origin',(0.,0.,0.));
#71580=CARTESIAN_POINT('Ctrl Pts',(1.57538060255632,23.3779086059641,-29.989082505666));
#71581=CARTESIAN_POINT('Ctrl Pts',(0.801841055749821,24.2891174222753,-30.2595606180251));
#71582=CARTESIAN_POINT('Ctrl Pts',(-2.77555756156289E-16,25.2256851884005,
-30.5258055876616));
#71583=CARTESIAN_POINT('Ctrl Pts',(6.93889390390723E-16,25.6816557463071,
-30.1432008606945));
#71584=CARTESIAN_POINT('Ctrl Pts',(0.80184105574966,25.5820889218578,-29.1746287096029));
#71585=CARTESIAN_POINT('Ctrl Pts',(1.57538060255632,25.4739497302129,-28.2302951713764));
#71586=CARTESIAN_POINT('Origin',(0.8,0.,0.));
#71587=CARTESIAN_POINT('',(-2.77555756156289E-16,19.5416998364696,-34.4424442730379));
#71588=CARTESIAN_POINT('',(1.38777878078145E-16,20.0571817906459,-34.1448306280319));
#71589=CARTESIAN_POINT('Origin',(0.,0.,0.));
#71590=CARTESIAN_POINT('Ctrl Pts',(1.57538060255632,17.8151961173521,-33.5930121843923));
#71591=CARTESIAN_POINT('Ctrl Pts',(0.801841055750877,18.6655935929574,-34.0176108768897));
#71592=CARTESIAN_POINT('Ctrl Pts',(-2.77555756156289E-16,19.5416998364696,
-34.4424442730379));
#71593=CARTESIAN_POINT('Ctrl Pts',(1.38777878078145E-16,20.0571817906459,
-34.1448306280319));
#71594=CARTESIAN_POINT('Ctrl Pts',(0.801841055749399,20.1273183989615,-33.1736836666638));
#71595=CARTESIAN_POINT('Ctrl Pts',(1.57538060255632,20.1848038826479,-32.224918503225));
#71596=CARTESIAN_POINT('Origin',(0.8,0.,0.));
#71597=CARTESIAN_POINT('',(-1.38777878078145E-16,13.2639498235848,-37.3125667178958));
#71598=CARTESIAN_POINT('',(-2.77555756156289E-16,13.8232805156996,-37.1089869948545));
#71599=CARTESIAN_POINT('Origin',(0.,0.,0.));
#71600=CARTESIAN_POINT('Ctrl Pts',(1.57538060255632,11.7111779096386,-36.1762351867803));
#71601=CARTESIAN_POINT('Ctrl Pts',(0.801841055749469,12.4749251475662,-36.7420532430029));
#71602=CARTESIAN_POINT('Ctrl Pts',(1.38777878078145E-16,13.2639498235848,
-37.3125667178958));
#71603=CARTESIAN_POINT('Ctrl Pts',(4.16333634234434E-16,13.8232805156996,
-37.1089869948545));
#71604=CARTESIAN_POINT('Ctrl Pts',(0.801841055749681,14.0609894914272,-36.1647730322064));
#71605=CARTESIAN_POINT('Ctrl Pts',(1.57538060255632,14.2823529831122,-35.2404039929487));
#71606=CARTESIAN_POINT('Origin',(0.8,0.,0.));
#71607=CARTESIAN_POINT('',(1.38777878078145E-16,6.58318140719289,-39.0489657041002));
#71608=CARTESIAN_POINT('',(1.38777878078145E-16,7.16936585720128,-38.9456055698919));
#71609=CARTESIAN_POINT('Origin',(0.,0.,0.));
#71610=CARTESIAN_POINT('Ctrl Pts',(1.57538060255633,5.25132148728273,-37.6602615890763));
#71611=CARTESIAN_POINT('Ctrl Pts',(0.801841055749878,5.90521241418099,-38.3501069137025));
#71612=CARTESIAN_POINT('Ctrl Pts',(1.38777878078145E-16,6.58318140719289,
-39.0489657041002));
#71613=CARTESIAN_POINT('Ctrl Pts',(0.,7.16936585720128,-38.9456055698919));
#71614=CARTESIAN_POINT('Ctrl Pts',(0.80184105575087,7.5674245334005,-38.0570140694225));
#71615=CARTESIAN_POINT('Ctrl Pts',(1.57538060255632,7.94594001540394,-37.1851276398516));
#71616=CARTESIAN_POINT('Origin',(0.8,0.,0.));
#71617=CARTESIAN_POINT('',(-2.77555756156289E-16,-0.297613645006075,-39.5988816271155));
#71618=CARTESIAN_POINT('',(-2.77555756156289E-16,0.297613645006066,-39.5988816271155));
#71619=CARTESIAN_POINT('Origin',(0.,0.,0.));
#71620=CARTESIAN_POINT('Ctrl Pts',(1.57538060255632,-1.36809368116734,-38.));
#71621=CARTESIAN_POINT('Ctrl Pts',(0.801841055749771,-0.843927210226931,
-38.7929119919201));
#71622=CARTESIAN_POINT('Ctrl Pts',(-4.16333634234434E-16,-0.297613645006074,
-39.5988816271155));
#71623=CARTESIAN_POINT('Ctrl Pts',(-1.38777878078145E-16,0.29761364500606,
-39.5988816271155));
#71624=CARTESIAN_POINT('Ctrl Pts',(0.801841055750365,0.843927210227319,
-38.7929119919195));
#71625=CARTESIAN_POINT('Ctrl Pts',(1.57538060255632,1.36809368116733,-38.));
#71626=CARTESIAN_POINT('Origin',(0.8,0.,0.));
#71627=CARTESIAN_POINT('',(6.93889390390723E-16,-7.16936585720129,-38.9456055698919));
#71628=CARTESIAN_POINT('',(-2.77555756156289E-16,-6.5831814071929,-39.0489657041002));
#71629=CARTESIAN_POINT('Origin',(0.,0.,0.));
#71630=CARTESIAN_POINT('Ctrl Pts',(1.57538060255633,-7.94594001540395,-37.1851276398516));
#71631=CARTESIAN_POINT('Ctrl Pts',(0.80184105574994,-7.56742453340005,-38.0570140694235));
#71632=CARTESIAN_POINT('Ctrl Pts',(-2.77555756156289E-16,-7.16936585720129,
-38.9456055698919));
#71633=CARTESIAN_POINT('Ctrl Pts',(-2.77555756156289E-16,-6.5831814071929,
-39.0489657041001));
#71634=CARTESIAN_POINT('Ctrl Pts',(0.80184105575081,-5.90521241418022,-38.3501069137017));
#71635=CARTESIAN_POINT('Ctrl Pts',(1.57538060255632,-5.25132148728275,-37.6602615890763));
#71636=CARTESIAN_POINT('Origin',(0.8,0.,0.));
#71637=CARTESIAN_POINT('',(1.38777878078145E-16,-13.8232805156997,-37.1089869948545));
#71638=CARTESIAN_POINT('',(1.38777878078145E-16,-13.2639498235849,-37.3125667178958));
#71639=CARTESIAN_POINT('Origin',(0.,0.,0.));
#71640=CARTESIAN_POINT('Ctrl Pts',(1.57538060255632,-14.2823529831122,-35.2404039929487));
#71641=CARTESIAN_POINT('Ctrl Pts',(0.801841055750031,-14.0609894914273,
-36.1647730322059));
#71642=CARTESIAN_POINT('Ctrl Pts',(-1.38777878078145E-16,-13.8232805156997,
-37.1089869948545));
#71643=CARTESIAN_POINT('Ctrl Pts',(9.71445146547012E-16,-13.2639498235849,
-37.3125667178958));
#71644=CARTESIAN_POINT('Ctrl Pts',(0.801841055748983,-12.4749251475667,
-36.7420532430033));
#71645=CARTESIAN_POINT('Ctrl Pts',(1.57538060255632,-11.7111779096387,-36.1762351867803));
#71646=CARTESIAN_POINT('Origin',(0.8,0.,0.));
#71647=CARTESIAN_POINT('',(-1.2490009027033E-15,-20.0571817906459,-34.1448306280318));
#71648=CARTESIAN_POINT('',(-6.93889390390723E-16,-19.5416998364696,-34.4424442730379));
#71649=CARTESIAN_POINT('Origin',(0.,0.,0.));
#71650=CARTESIAN_POINT('Ctrl Pts',(1.57538060255632,-20.1848038826479,-32.224918503225));
#71651=CARTESIAN_POINT('Ctrl Pts',(0.801841055749729,-20.1273183989615,
-33.1736836666634));
#71652=CARTESIAN_POINT('Ctrl Pts',(-6.93889390390723E-16,-20.0571817906459,
-34.1448306280318));
#71653=CARTESIAN_POINT('Ctrl Pts',(-5.55111512312578E-16,-19.5416998364696,
-34.4424442730379));
#71654=CARTESIAN_POINT('Ctrl Pts',(0.801841055748299,-18.6655935929602,
-34.017610876891));
#71655=CARTESIAN_POINT('Ctrl Pts',(1.57538060255633,-17.8151961173521,-33.5930121843923));
#71656=CARTESIAN_POINT('Origin',(0.8,0.,0.));
#71657=CARTESIAN_POINT('',(1.2490009027033E-15,-25.6816557463071,-30.1432008606945));
#71658=CARTESIAN_POINT('',(-4.16333634234434E-16,-25.2256851884005,-30.5258055876616));
#71659=CARTESIAN_POINT('Origin',(0.,0.,0.));
#71660=CARTESIAN_POINT('Ctrl Pts',(1.57538060255632,-25.4739497302129,-28.2302951713763));
#71661=CARTESIAN_POINT('Ctrl Pts',(0.801841055750148,-25.5820889218578,
-29.1746287096023));
#71662=CARTESIAN_POINT('Ctrl Pts',(2.77555756156289E-16,-25.6816557463071,
-30.1432008606945));
#71663=CARTESIAN_POINT('Ctrl Pts',(1.38777878078145E-16,-25.2256851884005,
-30.5258055876616));
#71664=CARTESIAN_POINT('Ctrl Pts',(0.801841055749258,-24.289117422276,-30.2595606180253));
#71665=CARTESIAN_POINT('Ctrl Pts',(1.57538060255632,-23.3779086059641,-29.989082505666));
#71666=CARTESIAN_POINT('Origin',(0.8,0.,0.));
#71667=CARTESIAN_POINT('',(-4.16333634234434E-16,-30.5258055876616,-25.2256851884005));
#71668=CARTESIAN_POINT('',(1.2490009027033E-15,-30.1432008606945,-25.6816557463071));
#71669=CARTESIAN_POINT('Origin',(0.,0.,0.));
#71670=CARTESIAN_POINT('Ctrl Pts',(1.57538060255632,-29.989082505666,-23.3779086059641));
#71671=CARTESIAN_POINT('Ctrl Pts',(0.801841055748062,-30.2595606180257,
-24.2891174222774));
#71672=CARTESIAN_POINT('Ctrl Pts',(-1.11022302462516E-15,-30.5258055876616,
-25.2256851884005));
#71673=CARTESIAN_POINT('Ctrl Pts',(6.93889390390723E-16,-30.1432008606945,
-25.6816557463071));
#71674=CARTESIAN_POINT('Ctrl Pts',(0.801841055750156,-29.1746287096023,
-25.5820889218578));
#71675=CARTESIAN_POINT('Ctrl Pts',(1.57538060255632,-28.2302951713764,-25.4739497302129));
#71676=CARTESIAN_POINT('Origin',(0.8,0.,0.));
#71677=CARTESIAN_POINT('',(-9.71445146547012E-16,-34.4424442730379,-19.5416998364696));
#71678=CARTESIAN_POINT('',(-9.71445146547012E-16,-34.1448306280319,-20.0571817906459));
#71679=CARTESIAN_POINT('Origin',(0.,0.,0.));
#71680=CARTESIAN_POINT('Ctrl Pts',(1.57538060255633,-33.5930121843923,-17.8151961173521));
#71681=CARTESIAN_POINT('Ctrl Pts',(0.801841055749805,-34.0176108768902,
-18.6655935929586));
#71682=CARTESIAN_POINT('Ctrl Pts',(0.,-34.4424442730379,-19.5416998364696));
#71683=CARTESIAN_POINT('Ctrl Pts',(6.93889390390723E-16,-34.1448306280319,
-20.0571817906459));
#71684=CARTESIAN_POINT('Ctrl Pts',(0.801841055748204,-33.1736836666653,
-20.1273183989614));
#71685=CARTESIAN_POINT('Ctrl Pts',(1.57538060255633,-32.224918503225,-20.1848038826479));
#71686=CARTESIAN_POINT('Origin',(0.8,0.,0.));
#71687=CARTESIAN_POINT('',(-1.38777878078145E-16,-37.3125667178958,-13.2639498235848));
#71688=CARTESIAN_POINT('',(-4.16333634234434E-16,-37.1089869948545,-13.8232805156996));
#71689=CARTESIAN_POINT('Origin',(0.,0.,0.));
#71690=CARTESIAN_POINT('Ctrl Pts',(1.57538060255633,-36.1762351867803,-11.7111779096386));
#71691=CARTESIAN_POINT('Ctrl Pts',(0.801841055749638,-36.7420532430028,
-12.474925147566));
#71692=CARTESIAN_POINT('Ctrl Pts',(2.77555756156289E-16,-37.3125667178958,
-13.2639498235848));
#71693=CARTESIAN_POINT('Ctrl Pts',(-6.93889390390723E-16,-37.1089869948545,
-13.8232805156996));
#71694=CARTESIAN_POINT('Ctrl Pts',(0.801841055748945,-36.1647730322072,
-14.060989491427));
#71695=CARTESIAN_POINT('Ctrl Pts',(1.57538060255633,-35.2404039929487,-14.2823529831122));
#71696=CARTESIAN_POINT('Origin',(0.8,0.,0.));
#71697=CARTESIAN_POINT('',(0.,-39.0489657041002,-6.58318140719289));
#71698=CARTESIAN_POINT('',(-1.38777878078145E-16,-38.9456055698919,-7.16936585720128));
#71699=CARTESIAN_POINT('Origin',(0.,0.,0.));
#71700=CARTESIAN_POINT('Ctrl Pts',(1.57538060255633,-37.6602615890763,-5.25132148728274));
#71701=CARTESIAN_POINT('Ctrl Pts',(0.801841055749013,-38.3501069137033,
-5.90521241418173));
#71702=CARTESIAN_POINT('Ctrl Pts',(-5.55111512312578E-16,-39.0489657041002,
-6.58318140719289));
#71703=CARTESIAN_POINT('Ctrl Pts',(2.77555756156289E-16,-38.9456055698919,
-7.16936585720128));
#71704=CARTESIAN_POINT('Ctrl Pts',(0.801841055749582,-38.0570140694239,
-7.56742453339987));
#71705=CARTESIAN_POINT('Ctrl Pts',(1.57538060255632,-37.1851276398516,-7.94594001540395));
#71706=CARTESIAN_POINT('Origin',(0.8,0.,0.));
#71707=CARTESIAN_POINT('',(0.,-39.5988816271155,0.297613645006073));
#71708=CARTESIAN_POINT('',(1.38777878078145E-16,-39.5988816271155,-0.29761364500606));
#71709=CARTESIAN_POINT('Origin',(0.,0.,0.));
#71710=CARTESIAN_POINT('Ctrl Pts',(1.57538060255633,-38.,1.36809368116734));
#71711=CARTESIAN_POINT('Ctrl Pts',(0.801841055749649,-38.7929119919202,
0.843927210226842));
#71712=CARTESIAN_POINT('Ctrl Pts',(-1.38777878078145E-16,-39.5988816271155,
0.29761364500607));
#71713=CARTESIAN_POINT('Ctrl Pts',(-1.38777878078145E-16,-39.5988816271155,
-0.297613645006064));
#71714=CARTESIAN_POINT('Ctrl Pts',(0.801841055749106,-38.7929119919208,
-0.843927210226466));
#71715=CARTESIAN_POINT('Ctrl Pts',(1.57538060255632,-38.,-1.36809368116733));
#71716=CARTESIAN_POINT('Origin',(0.8,0.,0.));
#71717=CARTESIAN_POINT('',(-1.38777878078145E-16,-38.9456055698919,7.16936585720131));
#71718=CARTESIAN_POINT('',(2.77555756156289E-16,-39.0489657041001,6.58318140719291));
#71719=CARTESIAN_POINT('Origin',(0.,0.,0.));
#71720=CARTESIAN_POINT('Ctrl Pts',(1.57538060255632,-37.1851276398516,7.94594001540397));
#71721=CARTESIAN_POINT('Ctrl Pts',(0.801841055749284,-38.0570140694243,
7.56742453339975));
#71722=CARTESIAN_POINT('Ctrl Pts',(0.,-38.9456055698919,7.16936585720131));
#71723=CARTESIAN_POINT('Ctrl Pts',(0.,-39.0489657041001,6.58318140719291));
#71724=CARTESIAN_POINT('Ctrl Pts',(0.80184105575133,-38.3501069137012,5.90521241417979));
#71725=CARTESIAN_POINT('Ctrl Pts',(1.57538060255632,-37.6602615890763,5.25132148728276));
#71726=CARTESIAN_POINT('Origin',(0.8,0.,0.));
#71727=CARTESIAN_POINT('',(1.38777878078145E-16,-37.1089869948545,13.8232805156996));
#71728=CARTESIAN_POINT('',(1.38777878078145E-16,-37.3125667178958,13.2639498235848));
#71729=CARTESIAN_POINT('Origin',(0.,0.,0.));
#71730=CARTESIAN_POINT('Ctrl Pts',(1.57538060255633,-35.2404039929487,14.2823529831122));
#71731=CARTESIAN_POINT('Ctrl Pts',(0.8018410557497,-36.1647730322063,14.0609894914272));
#71732=CARTESIAN_POINT('Ctrl Pts',(1.38777878078145E-16,-37.1089869948545,
13.8232805156996));
#71733=CARTESIAN_POINT('Ctrl Pts',(9.71445146547012E-16,-37.3125667178958,
13.2639498235848));
#71734=CARTESIAN_POINT('Ctrl Pts',(0.801841055750097,-36.7420532430025,
12.4749251475656));
#71735=CARTESIAN_POINT('Ctrl Pts',(1.57538060255632,-36.1762351867803,11.7111779096386));
#71736=CARTESIAN_POINT('Origin',(0.8,0.,0.));
#71737=CARTESIAN_POINT('',(1.52655665885959E-15,-34.1448306280319,20.0571817906459));
#71738=CARTESIAN_POINT('',(-4.16333634234434E-16,-34.4424442730379,19.5416998364696));
#71739=CARTESIAN_POINT('Origin',(0.,0.,0.));
#71740=CARTESIAN_POINT('Ctrl Pts',(1.57538060255632,-32.224918503225,20.1848038826479));
#71741=CARTESIAN_POINT('Ctrl Pts',(0.801841055750799,-33.1736836666621,
20.1273183989616));
#71742=CARTESIAN_POINT('Ctrl Pts',(6.93889390390723E-16,-34.1448306280319,
20.0571817906459));
#71743=CARTESIAN_POINT('Ctrl Pts',(-2.77555756156289E-16,-34.4424442730379,
19.5416998364696));
#71744=CARTESIAN_POINT('Ctrl Pts',(0.801841055749465,-34.0176108768904,
18.6655935929589));
#71745=CARTESIAN_POINT('Ctrl Pts',(1.57538060255632,-33.5930121843923,17.8151961173521));
#71746=CARTESIAN_POINT('Origin',(0.8,0.,0.));
#71747=CARTESIAN_POINT('',(1.2490009027033E-15,-30.1432008606945,25.6816557463071));
#71748=CARTESIAN_POINT('',(-1.38777878078145E-16,-30.5258055876616,25.2256851884005));
#71749=CARTESIAN_POINT('Origin',(0.,0.,0.));
#71750=CARTESIAN_POINT('Ctrl Pts',(1.57538060255632,-28.2302951713763,25.4739497302129));
#71751=CARTESIAN_POINT('Ctrl Pts',(0.801841055750152,-29.1746287096023,
25.5820889218578));
#71752=CARTESIAN_POINT('Ctrl Pts',(1.38777878078145E-16,-30.1432008606945,
25.6816557463071));
#71753=CARTESIAN_POINT('Ctrl Pts',(1.38777878078145E-16,-30.5258055876616,
25.2256851884005));
#71754=CARTESIAN_POINT('Ctrl Pts',(0.80184105574948,-30.2595606180252,24.2891174222757));
#71755=CARTESIAN_POINT('Ctrl Pts',(1.57538060255632,-29.989082505666,23.3779086059641));
#71756=CARTESIAN_POINT('Origin',(0.8,0.,0.));
#71757=CARTESIAN_POINT('',(2.77555756156289E-16,-25.2256851884005,30.5258055876616));
#71758=CARTESIAN_POINT('',(-6.93889390390723E-16,-25.6816557463071,30.1432008606945));
#71759=CARTESIAN_POINT('Origin',(0.,0.,0.));
#71760=CARTESIAN_POINT('Ctrl Pts',(1.57538060255632,-23.3779086059641,29.989082505666));
#71761=CARTESIAN_POINT('Ctrl Pts',(0.801841055750737,-24.2891174222742,
30.2595606180248));
#71762=CARTESIAN_POINT('Ctrl Pts',(-1.52655665885959E-15,-25.2256851884005,
30.5258055876616));
#71763=CARTESIAN_POINT('Ctrl Pts',(1.38777878078145E-16,-25.6816557463071,
30.1432008606945));
#71764=CARTESIAN_POINT('Ctrl Pts',(0.801841055749893,-25.5820889218578,
29.1746287096026));
#71765=CARTESIAN_POINT('Ctrl Pts',(1.57538060255633,-25.4739497302129,28.2302951713764));
#71766=CARTESIAN_POINT('Origin',(0.8,0.,0.));
#71767=CARTESIAN_POINT('',(0.,-19.5416998364696,34.4424442730379));
#71768=CARTESIAN_POINT('',(2.08166817117217E-15,-20.0571817906459,34.1448306280319));
#71769=CARTESIAN_POINT('Origin',(0.,0.,0.));
#71770=CARTESIAN_POINT('Ctrl Pts',(1.57538060255632,-17.8151961173521,33.5930121843923));
#71771=CARTESIAN_POINT('Ctrl Pts',(0.801841055749172,-18.6655935929592,
34.0176108768906));
#71772=CARTESIAN_POINT('Ctrl Pts',(1.38777878078145E-16,-19.5416998364696,
34.4424442730379));
#71773=CARTESIAN_POINT('Ctrl Pts',(8.32667268468867E-16,-20.0571817906459,
34.1448306280319));
#71774=CARTESIAN_POINT('Ctrl Pts',(0.801841055749073,-20.1273183989614,
33.1736836666642));
#71775=CARTESIAN_POINT('Ctrl Pts',(1.57538060255632,-20.1848038826479,32.224918503225));
#71776=CARTESIAN_POINT('Origin',(0.8,0.,0.));
#71777=CARTESIAN_POINT('',(4.16333634234434E-16,-13.2639498235848,37.3125667178958));
#71778=CARTESIAN_POINT('',(-1.38777878078145E-16,-13.8232805156996,37.1089869948545));
#71779=CARTESIAN_POINT('Origin',(0.,0.,0.));
#71780=CARTESIAN_POINT('Ctrl Pts',(1.57538060255632,-11.7111779096386,36.1762351867803));
#71781=CARTESIAN_POINT('Ctrl Pts',(0.801841055748783,-12.4749251475669,
36.7420532430035));
#71782=CARTESIAN_POINT('Ctrl Pts',(5.55111512312578E-16,-13.2639498235848,
37.3125667178958));
#71783=CARTESIAN_POINT('Ctrl Pts',(1.38777878078145E-16,-13.8232805156996,
37.1089869948545));
#71784=CARTESIAN_POINT('Ctrl Pts',(0.801841055750372,-14.0609894914274,
36.1647730322055));
#71785=CARTESIAN_POINT('Ctrl Pts',(1.57538060255632,-14.2823529831122,35.2404039929487));
#71786=CARTESIAN_POINT('Origin',(0.8,0.,0.));
#71787=CARTESIAN_POINT('',(1.38777878078145E-16,-6.5831814071929,39.0489657041001));
#71788=CARTESIAN_POINT('',(-5.55111512312578E-16,-7.16936585720129,38.9456055698919));
#71789=CARTESIAN_POINT('Origin',(0.,0.,0.));
#71790=CARTESIAN_POINT('Ctrl Pts',(1.57538060255632,-5.25132148728275,37.6602615890763));
#71791=CARTESIAN_POINT('Ctrl Pts',(0.801841055749745,-5.90521241418111,
38.3501069137026));
#71792=CARTESIAN_POINT('Ctrl Pts',(4.16333634234434E-16,-6.5831814071929,
39.0489657041001));
#71793=CARTESIAN_POINT('Ctrl Pts',(5.55111512312578E-16,-7.16936585720129,
38.9456055698919));
#71794=CARTESIAN_POINT('Ctrl Pts',(0.801841055751039,-7.5674245334006,38.0570140694223));
#71795=CARTESIAN_POINT('Ctrl Pts',(1.57538060255632,-7.94594001540396,37.1851276398516));
#71796=CARTESIAN_POINT('Origin',(0.8,0.,0.));
#71797=CARTESIAN_POINT('',(1.38777878078145E-16,0.297613645006065,39.5988816271155));
#71798=CARTESIAN_POINT('',(0.,-0.297613645006066,39.5988816271155));
#71799=CARTESIAN_POINT('Origin',(0.,0.,0.));
#71800=CARTESIAN_POINT('Ctrl Pts',(1.57538060255633,1.36809368116734,38.));
#71801=CARTESIAN_POINT('Ctrl Pts',(0.801841055749075,0.843927210226451,
38.7929119919208));
#71802=CARTESIAN_POINT('Ctrl Pts',(-2.77555756156289E-16,0.297613645006067,
39.5988816271155));
#71803=CARTESIAN_POINT('Ctrl Pts',(0.,-0.297613645006065,39.5988816271155));
#71804=CARTESIAN_POINT('Ctrl Pts',(0.801841055749647,-0.84392721022684,
38.7929119919202));
#71805=CARTESIAN_POINT('Ctrl Pts',(1.57538060255632,-1.36809368116733,38.));
#71806=CARTESIAN_POINT('Origin',(0.8,0.,0.));
#71807=CARTESIAN_POINT('',(1.38777878078145E-16,7.16936585720129,38.9456055698919));
#71808=CARTESIAN_POINT('',(-1.38777878078145E-16,6.5831814071929,39.0489657041002));
#71809=CARTESIAN_POINT('Origin',(0.,0.,0.));
#71810=CARTESIAN_POINT('Ctrl Pts',(1.57538060255632,7.94594001540395,37.1851276398516));
#71811=CARTESIAN_POINT('Ctrl Pts',(0.801841055750375,7.56742453340027,38.0570140694231));
#71812=CARTESIAN_POINT('Ctrl Pts',(-5.55111512312578E-16,7.1693658572013,
38.9456055698919));
#71813=CARTESIAN_POINT('Ctrl Pts',(0.,6.5831814071929,39.0489657041001));
#71814=CARTESIAN_POINT('Ctrl Pts',(0.801841055750716,5.9052124141803,38.3501069137018));
#71815=CARTESIAN_POINT('Ctrl Pts',(1.57538060255632,5.25132148728276,37.6602615890763));
#71816=CARTESIAN_POINT('Origin',(0.8,0.,0.));
#71817=CARTESIAN_POINT('',(-2.77555756156289E-16,13.8232805156996,37.1089869948545));
#71818=CARTESIAN_POINT('',(1.38777878078145E-16,13.2639498235848,37.3125667178958));
#71819=CARTESIAN_POINT('Origin',(0.,0.,0.));
#71820=CARTESIAN_POINT('Ctrl Pts',(1.57538060255633,14.2823529831122,35.2404039929487));
#71821=CARTESIAN_POINT('Ctrl Pts',(0.801841055750263,14.0609894914274,36.1647730322056));
#71822=CARTESIAN_POINT('Ctrl Pts',(1.38777878078145E-16,13.8232805156996,
37.1089869948545));
#71823=CARTESIAN_POINT('Ctrl Pts',(5.55111512312578E-16,13.2639498235848,
37.3125667178958));
#71824=CARTESIAN_POINT('Ctrl Pts',(0.801841055750114,12.4749251475656,36.7420532430025));
#71825=CARTESIAN_POINT('Ctrl Pts',(1.57538060255632,11.7111779096386,36.1762351867803));
#71826=CARTESIAN_POINT('Origin',(0.8,0.,0.));
#71827=CARTESIAN_POINT('',(0.,20.0571817906459,34.1448306280319));
#71828=CARTESIAN_POINT('',(-2.77555756156289E-16,19.5416998364696,34.4424442730379));
#71829=CARTESIAN_POINT('Origin',(0.,0.,0.));
#71830=CARTESIAN_POINT('Ctrl Pts',(1.57538060255632,20.1848038826479,32.224918503225));
#71831=CARTESIAN_POINT('Ctrl Pts',(0.801841055749837,20.1273183989615,33.1736836666633));
#71832=CARTESIAN_POINT('Ctrl Pts',(5.55111512312578E-16,20.0571817906459,
34.1448306280319));
#71833=CARTESIAN_POINT('Ctrl Pts',(0.,19.5416998364696,34.4424442730379));
#71834=CARTESIAN_POINT('Ctrl Pts',(0.801841055750045,18.6655935929583,34.0176108768901));
#71835=CARTESIAN_POINT('Ctrl Pts',(1.57538060255632,17.8151961173521,33.5930121843923));
#71836=CARTESIAN_POINT('Origin',(0.8,0.,0.));
#71837=CARTESIAN_POINT('',(-1.38777878078145E-16,25.6816557463071,30.1432008606945));
#71838=CARTESIAN_POINT('',(4.16333634234434E-16,25.2256851884005,30.5258055876616));
#71839=CARTESIAN_POINT('Origin',(0.,0.,0.));
#71840=CARTESIAN_POINT('Ctrl Pts',(1.57538060255632,25.4739497302129,28.2302951713764));
#71841=CARTESIAN_POINT('Ctrl Pts',(0.801841055750649,25.5820889218577,29.1746287096017));
#71842=CARTESIAN_POINT('Ctrl Pts',(-9.71445146547012E-16,25.6816557463071,
30.1432008606945));
#71843=CARTESIAN_POINT('Ctrl Pts',(4.16333634234434E-16,25.2256851884005,
30.5258055876616));
#71844=CARTESIAN_POINT('Ctrl Pts',(0.801841055749584,24.2891174222756,30.2595606180252));
#71845=CARTESIAN_POINT('Ctrl Pts',(1.57538060255632,23.3779086059641,29.989082505666));
#71846=CARTESIAN_POINT('Origin',(0.8,0.,0.));
#71847=CARTESIAN_POINT('',(0.,30.5258055876616,25.2256851884005));
#71848=CARTESIAN_POINT('',(8.32667268468867E-16,30.1432008606945,25.6816557463071));
#71849=CARTESIAN_POINT('Origin',(0.,0.,0.));
#71850=CARTESIAN_POINT('Ctrl Pts',(1.57538060255632,29.989082505666,23.3779086059641));
#71851=CARTESIAN_POINT('Ctrl Pts',(0.801841055748062,30.2595606180257,24.2891174222774));
#71852=CARTESIAN_POINT('Ctrl Pts',(-1.11022302462516E-15,30.5258055876616,
25.2256851884005));
#71853=CARTESIAN_POINT('Ctrl Pts',(6.93889390390723E-16,30.1432008606945,
25.6816557463071));
#71854=CARTESIAN_POINT('Ctrl Pts',(0.801841055750156,29.1746287096023,25.5820889218578));
#71855=CARTESIAN_POINT('Ctrl Pts',(1.57538060255632,28.2302951713764,25.4739497302129));
#71856=CARTESIAN_POINT('Origin',(0.8,0.,0.));
#71857=CARTESIAN_POINT('',(2.77555756156289E-16,34.4424442730379,19.5416998364696));
#71858=CARTESIAN_POINT('',(1.38777878078145E-16,34.1448306280319,20.0571817906459));
#71859=CARTESIAN_POINT('Origin',(0.,0.,0.));
#71860=CARTESIAN_POINT('Ctrl Pts',(1.57538060255632,33.5930121843923,17.8151961173521));
#71861=CARTESIAN_POINT('Ctrl Pts',(0.801841055749312,34.0176108768905,18.6655935929591));
#71862=CARTESIAN_POINT('Ctrl Pts',(2.77555756156289E-16,34.4424442730379,
19.5416998364696));
#71863=CARTESIAN_POINT('Ctrl Pts',(-8.32667268468867E-16,34.1448306280319,
20.0571817906459));
#71864=CARTESIAN_POINT('Ctrl Pts',(0.801841055749606,33.1736836666635,20.1273183989615));
#71865=CARTESIAN_POINT('Ctrl Pts',(1.57538060255632,32.224918503225,20.1848038826479));
#71866=CARTESIAN_POINT('Origin',(0.8,0.,0.));
#71867=CARTESIAN_POINT('',(-2.77555756156289E-16,37.3125667178958,13.2639498235848));
#71868=CARTESIAN_POINT('',(-1.38777878078145E-16,37.1089869948545,13.8232805156996));
#71869=CARTESIAN_POINT('Origin',(0.,0.,0.));
#71870=CARTESIAN_POINT('Ctrl Pts',(1.57538060255632,36.1762351867803,11.7111779096386));
#71871=CARTESIAN_POINT('Ctrl Pts',(0.801841055749034,36.7420532430033,12.4749251475666));
#71872=CARTESIAN_POINT('Ctrl Pts',(5.55111512312578E-16,37.3125667178958,
13.2639498235848));
#71873=CARTESIAN_POINT('Ctrl Pts',(1.38777878078145E-16,37.1089869948545,
13.8232805156996));
#71874=CARTESIAN_POINT('Ctrl Pts',(0.801841055750194,36.1647730322057,14.0609894914274));
#71875=CARTESIAN_POINT('Ctrl Pts',(1.57538060255633,35.2404039929487,14.2823529831122));
#71876=CARTESIAN_POINT('Origin',(0.8,0.,0.));
#71877=CARTESIAN_POINT('',(-2.77555756156289E-16,39.0489657041001,6.5831814071929));
#71878=CARTESIAN_POINT('',(0.,38.9456055698919,7.16936585720129));
#71879=CARTESIAN_POINT('Origin',(0.,0.,0.));
#71880=CARTESIAN_POINT('Ctrl Pts',(1.57538060255632,37.6602615890763,5.25132148728275));
#71881=CARTESIAN_POINT('Ctrl Pts',(0.801841055750208,38.3501069137022,5.90521241418072));
#71882=CARTESIAN_POINT('Ctrl Pts',(-4.16333634234434E-16,39.0489657041001,
6.5831814071929));
#71883=CARTESIAN_POINT('Ctrl Pts',(5.55111512312578E-16,38.9456055698919,
7.16936585720129));
#71884=CARTESIAN_POINT('Ctrl Pts',(0.801841055749313,38.0570140694242,7.56742453339975));
#71885=CARTESIAN_POINT('Ctrl Pts',(1.57538060255632,37.1851276398516,7.94594001540396));
#71886=CARTESIAN_POINT('Origin',(0.8,0.,0.));
#71887=CARTESIAN_POINT('',(4.16333634234434E-16,39.5988816271155,-0.297613645006065));
#71888=CARTESIAN_POINT('',(-1.38777878078145E-16,39.5988816271155,0.297613645006066));
#71889=CARTESIAN_POINT('Origin',(0.,0.,0.));
#71890=CARTESIAN_POINT('Ctrl Pts',(1.57538060255632,38.,-1.36809368116733));
#71891=CARTESIAN_POINT('Ctrl Pts',(0.801841055749355,38.7929119919205,-0.843927210226636));
#71892=CARTESIAN_POINT('Ctrl Pts',(-2.77555756156289E-16,39.5988816271155,
-0.297613645006065));
#71893=CARTESIAN_POINT('Ctrl Pts',(0.,39.5988816271155,0.297613645006068));
#71894=CARTESIAN_POINT('Ctrl Pts',(0.801841055750186,38.7929119919197,0.843927210227206));
#71895=CARTESIAN_POINT('Ctrl Pts',(1.57538060255633,38.,1.36809368116734));
#71896=CARTESIAN_POINT('Origin',(0.,38.,0.));
#71897=CARTESIAN_POINT('',(0.,42.75,-0.884158520433537));
#71898=CARTESIAN_POINT('',(0.,37.5167436681065,0.0899526743993834));
#71899=CARTESIAN_POINT('',(0.13820771414163,42.75,-1.00418100903022));
#71900=CARTESIAN_POINT('',(1.46228393816674,42.75,-2.15403667726254));
#71901=CARTESIAN_POINT('',(0.600000000000001,42.2794732300361,-1.31762794090604));
#71902=CARTESIAN_POINT('Ctrl Pts',(0.600000000000001,42.2794732300362,-1.31762794090604));
#71903=CARTESIAN_POINT('Ctrl Pts',(0.370217470899393,42.5142243943549,-1.16177621660585));
#71904=CARTESIAN_POINT('Ctrl Pts',(0.13820771414163,42.75,-1.00418100903022));
#71905=CARTESIAN_POINT('',(1.67735469196904,42.240333256585,-2.24593997529677));
#71906=CARTESIAN_POINT('Origin',(8.1449754609635,0.,0.));
#71907=CARTESIAN_POINT('',(1.90339248332146,37.9353893420094,-1.64091956419534));
#71908=CARTESIAN_POINT('Origin',(0.,37.4226946144639,6.59863075134335));
#71909=CARTESIAN_POINT('',(0.,42.2540639571139,6.55273342944652));
#71910=CARTESIAN_POINT('',(0.,37.2427065776832,6.60034061210452));
#71911=CARTESIAN_POINT('',(0.138207714141617,42.2749056435377,6.4345343521407));
#71912=CARTESIAN_POINT('',(1.46228393816674,42.4745759849063,5.30214757522046));
#71913=CARTESIAN_POINT('',(0.600000000000001,41.8659567209931,6.04414326732376));
#71914=CARTESIAN_POINT('Ctrl Pts',(0.6,41.8659567209931,6.04414326732376));
#71915=CARTESIAN_POINT('Ctrl Pts',(0.370217470897594,42.0700781197334,6.23839136562556));
#71916=CARTESIAN_POINT('Ctrl Pts',(0.138207714141617,42.2749056435377,6.4345343521407));
#71917=CARTESIAN_POINT('',(1.67735469196904,41.9886110647639,5.12313779357752));
#71918=CARTESIAN_POINT('Origin',(8.1449754609635,0.,0.));
#71919=CARTESIAN_POINT('',(1.90339248332146,37.6440082295681,4.97142091943645));
#71920=CARTESIAN_POINT('Origin',(0.,35.7083195898645,12.9967654463754));
#71921=CARTESIAN_POINT('',(0.,40.4742595624789,13.790523889916));
#71922=CARTESIAN_POINT('',(0.,35.2836459493057,12.9260368409209));
#71923=CARTESIAN_POINT('',(0.138207714141626,40.515309671231,13.6777396430533));
#71924=CARTESIAN_POINT('',(1.46228393816674,40.9085834716837,12.5972287566465));
#71925=CARTESIAN_POINT('',(0.600000000000001,40.1803643021789,13.22226624086));
#71926=CARTESIAN_POINT('Ctrl Pts',(0.600000000000002,40.1803643021789,13.22226624086));
#71927=CARTESIAN_POINT('Ctrl Pts',(0.37021747089599,40.3476538099299,13.4490085829912));
#71928=CARTESIAN_POINT('Ctrl Pts',(0.138207714141626,40.515309671231,13.6777396430533));
#71929=CARTESIAN_POINT('',(1.67735469196904,40.4610861730024,12.3365516130268));
#71930=CARTESIAN_POINT('Origin',(8.1449754609635,0.,0.));
#71931=CARTESIAN_POINT('',(1.90339248332146,36.2088329758587,11.4327072940915));
#71932=CARTESIAN_POINT('Origin',(0.,32.9089653438087,19.));
#71933=CARTESIAN_POINT('',(0.,37.4646652720015,20.6092962603321));
#71934=CARTESIAN_POINT('',(0.,31.7439889350152,18.5884732955206));
#71935=CARTESIAN_POINT('',(0.138207714141626,37.5246765162999,20.5053537361819));
#71936=CARTESIAN_POINT('',(1.46228393816674,38.099604350416,19.5095495168072));
#71937=CARTESIAN_POINT('',(0.600000000000001,37.2739118462884,19.9986373454573));
#71938=CARTESIAN_POINT('Ctrl Pts',(0.600000000000003,37.2739118462884,19.9986373454573));
#71939=CARTESIAN_POINT('Ctrl Pts',(0.370217470897655,37.3992864560072,20.2509844800861));
#71940=CARTESIAN_POINT('Ctrl Pts',(0.138207714141626,37.5246765162998,20.5053537361819));
#71941=CARTESIAN_POINT('',(1.67735469196904,37.7041716521717,19.1751255543105));
#71942=CARTESIAN_POINT('Origin',(8.1449754609635,0.,0.));
#71943=CARTESIAN_POINT('',(1.90339248332146,33.6734706547313,17.5466166428447));
#71944=CARTESIAN_POINT('Origin',(0.,29.1096888385212,24.4259291680885));
#71945=CARTESIAN_POINT('',(0.,33.3167260852698,26.8018655926851));
#71946=CARTESIAN_POINT('',(0.,26.8714229747626,23.1618620629671));
#71947=CARTESIAN_POINT('',(0.138207714141623,33.3938750538235,26.7099230322464));
#71948=CARTESIAN_POINT('',(1.46228393816674,34.132988030291,25.8290824872081));
#71949=CARTESIAN_POINT('',(0.600000000000001,33.234910440458,26.1673599741116));
#71950=CARTESIAN_POINT('Ctrl Pts',(0.600000000000003,33.234910440458,26.1673599741116));
#71951=CARTESIAN_POINT('Ctrl Pts',(0.370217470903501,33.3145607080702,26.437644461241));
#71952=CARTESIAN_POINT('Ctrl Pts',(0.138207714141623,33.3938750538235,26.7099230322464));
#71953=CARTESIAN_POINT('',(1.67735469196904,33.8016349549212,25.4310730087083));
#71954=CARTESIAN_POINT('Origin',(8.1449754609635,0.,0.));
#71955=CARTESIAN_POINT('',(1.90339248332146,30.1149569673582,23.1273809239214));
#71956=CARTESIAN_POINT('Origin',(0.,24.4259291680885,29.1096888385212));
#71957=CARTESIAN_POINT('',(0.,28.156475035514,32.1800738014028));
#71958=CARTESIAN_POINT('',(0.,21.0324673783039,26.3167372379398));
#71959=CARTESIAN_POINT('',(0.138207714141625,28.2484175959528,32.1029248328492));
#71960=CARTESIAN_POINT('',(1.46228393816674,29.129258140991,31.3638118563816));
#71961=CARTESIAN_POINT('',(0.600000000000001,28.1860830985703,31.5410006112756));
#71962=CARTESIAN_POINT('Ctrl Pts',(0.600000000000002,28.1860830985703,31.5410006112756));
#71963=CARTESIAN_POINT('Ctrl Pts',(0.370217470900064,28.2175888910031,31.8210099935453));
#71964=CARTESIAN_POINT('Ctrl Pts',(0.138207714141625,28.2484175959528,32.1029248328492));
#71965=CARTESIAN_POINT('',(1.67735469196904,28.872052684018,30.9143101784803));
#71966=CARTESIAN_POINT('Origin',(8.1449754609635,0.,0.));
#71967=CARTESIAN_POINT('',(1.90339248332146,25.6414155514355,28.0054314386442));
#71968=CARTESIAN_POINT('Origin',(0.,19.,32.9089653438087));
#71969=CARTESIAN_POINT('',(0.,22.1407037396679,36.580506751568));
#71970=CARTESIAN_POINT('',(0.,14.6749862528265,27.8529433888201));
#71971=CARTESIAN_POINT('',(0.138207714141622,22.2446462638181,36.5204955072696));
#71972=CARTESIAN_POINT('',(1.46228393816674,23.2404504831928,35.9455676731535));
#71973=CARTESIAN_POINT('',(0.600000000000001,22.2808358845789,35.9562839053824));
#71974=CARTESIAN_POINT('Ctrl Pts',(0.600000000000003,22.2808358845789,35.9562839053824));
#71975=CARTESIAN_POINT('Ctrl Pts',(0.370217470897647,22.2632399142705,36.2375102394026));
#71976=CARTESIAN_POINT('Ctrl Pts',(0.138207714141622,22.2446462638181,36.5204955072696));
#71977=CARTESIAN_POINT('',(1.67735469196904,23.0652077022745,35.4582316768749));
#71978=CARTESIAN_POINT('Origin',(8.1449754609635,0.,0.));
#71979=CARTESIAN_POINT('',(1.90339248332146,20.3887726991648,32.0325510905359));
#71980=CARTESIAN_POINT('Origin',(0.,12.9967654463754,35.7083195898645));
#71981=CARTESIAN_POINT('',(0.,15.4521983644287,39.8694595147163));
#71982=CARTESIAN_POINT('',(0.,8.28196006949682,27.7182968336373));
#71983=CARTESIAN_POINT('',(0.138207714141624,15.5649826112914,39.8284094059642));
#71984=CARTESIAN_POINT('',(1.46228393816674,16.6454934976982,39.4351356055115));
#71985=CARTESIAN_POINT('',(0.600000000000001,15.6985967468815,39.2790537077817));
#71986=CARTESIAN_POINT('Ctrl Pts',(0.600000000000003,15.6985967468815,39.2790537077817));
#71987=CARTESIAN_POINT('Ctrl Pts',(0.37021747089523,15.6324336584848,39.5529520737006));
#71988=CARTESIAN_POINT('Ctrl Pts',(0.138207714141624,15.5649826112914,39.8284094059641));
#71989=CARTESIAN_POINT('',(1.67735469196904,16.5575380560557,38.9247727484987));
#71990=CARTESIAN_POINT('Origin',(8.14497546096349,0.,0.));
#71991=CARTESIAN_POINT('',(1.90339248332146,14.5166273056467,35.0863778867947));
#71992=CARTESIAN_POINT('Origin',(0.,6.59863075134336,37.4226946144639));
#71993=CARTESIAN_POINT('',(0.,8.29418576107603,41.9469989254299));
#71994=CARTESIAN_POINT('',(0.,2.32185498719982,26.0108354204645));
#71995=CARTESIAN_POINT('',(0.138207714141621,8.41238483838185,41.9261572390061));
#71996=CARTESIAN_POINT('',(1.46228393816674,9.54477161530209,41.7264868976375));
#71997=CARTESIAN_POINT('',(0.600000000000001,8.63936369090333,41.4083493394303));
#71998=CARTESIAN_POINT('Ctrl Pts',(0.600000000000004,8.63936369090333,41.4083493394303));
#71999=CARTESIAN_POINT('Ctrl Pts',(0.370217470893892,8.5266438163786,41.6665974739972));
#72000=CARTESIAN_POINT('Ctrl Pts',(0.138207714141621,8.41238483838185,41.9261572390061));
#72001=CARTESIAN_POINT('',(1.67735469196904,9.54677599452213,41.2086042970448));
#72002=CARTESIAN_POINT('Origin',(8.1449754609635,0.,0.));
#72003=CARTESIAN_POINT('',(1.90339248332146,8.20340153721441,37.0741228455271));
#72004=CARTESIAN_POINT('Origin',(0.,2.32682891837997E-15,38.));
#72005=CARTESIAN_POINT('',(0.,0.884158520433539,42.75));
#72006=CARTESIAN_POINT('',(0.,-2.79868590723512,22.9645083408252));
#72007=CARTESIAN_POINT('',(0.138207714141629,1.00418100903022,42.75));
#72008=CARTESIAN_POINT('',(1.46228393816674,2.15403667726255,42.75));
#72009=CARTESIAN_POINT('',(0.600000000000001,1.31762794090604,42.2794732300361));
#72010=CARTESIAN_POINT('Ctrl Pts',(0.600000000000004,1.31762794090604,42.2794732300361));
#72011=CARTESIAN_POINT('Ctrl Pts',(0.37021747089638,1.1617762166038,42.5142243943579));
#72012=CARTESIAN_POINT('Ctrl Pts',(0.138207714141629,1.00418100903022,42.75));
#72013=CARTESIAN_POINT('',(1.67735469196904,2.24593997529677,42.240333256585));
#72014=CARTESIAN_POINT('Origin',(8.1449754609635,0.,0.));
#72015=CARTESIAN_POINT('',(1.90339248332146,1.64091956419534,37.9353893420094));
#72016=CARTESIAN_POINT('Origin',(0.,-6.59863075134335,37.4226946144639));
#72017=CARTESIAN_POINT('',(0.,-6.55273342944652,42.2540639571139));
#72018=CARTESIAN_POINT('',(0.,-6.77440269836428,18.9201075126787));
#72019=CARTESIAN_POINT('',(0.138207714141616,-6.4345343521407,42.2749056435377));
#72020=CARTESIAN_POINT('',(1.46228393816674,-5.30214757522046,42.4745759849063));
#72021=CARTESIAN_POINT('',(0.600000000000001,-6.04414326732376,41.8659567209931));
#72022=CARTESIAN_POINT('Ctrl Pts',(0.600000000000004,-6.04414326732376,
41.8659567209931));
#72023=CARTESIAN_POINT('Ctrl Pts',(0.370217470895893,-6.23839136562701,
42.0700781197349));
#72024=CARTESIAN_POINT('Ctrl Pts',(0.138207714141616,-6.4345343521407,42.2749056435377));
#72025=CARTESIAN_POINT('',(1.67735469196904,-5.12313779357752,41.9886110647639));
#72026=CARTESIAN_POINT('Origin',(8.1449754609635,0.,0.));
#72027=CARTESIAN_POINT('',(1.90339248332146,-4.97142091943645,37.6440082295681));
#72028=CARTESIAN_POINT('Origin',(0.,-12.9967654463754,35.7083195898645));
#72029=CARTESIAN_POINT('',(0.,-13.790523889916,40.4742595624789));
#72030=CARTESIAN_POINT('',(0.,-9.42874680865831,14.2849724911192));
#72031=CARTESIAN_POINT('',(0.138207714141626,-13.6777396430533,40.515309671231));
#72032=CARTESIAN_POINT('',(1.46228393816674,-12.5972287566465,40.9085834716837));
#72033=CARTESIAN_POINT('',(0.600000000000001,-13.22226624086,40.1803643021789));
#72034=CARTESIAN_POINT('Ctrl Pts',(0.600000000000004,-13.22226624086,40.1803643021789));
#72035=CARTESIAN_POINT('Ctrl Pts',(0.370217470891807,-13.4490085829953,
40.3476538099329));
#72036=CARTESIAN_POINT('Ctrl Pts',(0.138207714141626,-13.6777396430533,
40.515309671231));
#72037=CARTESIAN_POINT('',(1.67735469196904,-12.3365516130268,40.4610861730024));
#72038=CARTESIAN_POINT('Origin',(8.1449754609635,0.,0.));
#72039=CARTESIAN_POINT('',(1.90339248332146,-11.4327072940915,36.2088329758587));
#72040=CARTESIAN_POINT('Origin',(0.,-19.,32.9089653438087));
#72041=CARTESIAN_POINT('',(0.,-20.6092962603321,37.4646652720015));
#72042=CARTESIAN_POINT('',(0.,-10.7259694216695,9.48630449465761));
#72043=CARTESIAN_POINT('',(0.138207714141623,-20.5053537361819,37.5246765162999));
#72044=CARTESIAN_POINT('',(1.46228393816674,-19.5095495168072,38.099604350416));
#72045=CARTESIAN_POINT('',(0.600000000000001,-19.9986373454573,37.2739118462884));
#72046=CARTESIAN_POINT('Ctrl Pts',(0.600000000000005,-19.9986373454573,
37.2739118462884));
#72047=CARTESIAN_POINT('Ctrl Pts',(0.370217470900507,-20.250984480083,37.3992864560057));
#72048=CARTESIAN_POINT('Ctrl Pts',(0.138207714141623,-20.5053537361819,
37.5246765162998));
#72049=CARTESIAN_POINT('',(1.67735469196904,-19.1751255543105,37.7041716521717));
#72050=CARTESIAN_POINT('Origin',(8.1449754609635,0.,0.));
#72051=CARTESIAN_POINT('',(1.90339248332146,-17.5466166428447,33.6734706547313));
#72052=CARTESIAN_POINT('Origin',(0.,-24.4259291680885,29.1096888385212));
#72053=CARTESIAN_POINT('',(0.,-26.8018655926851,33.3167260852698));
#72054=CARTESIAN_POINT('',(0.,-10.7667918374521,4.92364626871755));
#72055=CARTESIAN_POINT('',(0.138207714141626,-26.7099230322463,33.3938750538235));
#72056=CARTESIAN_POINT('',(1.46228393816674,-25.8290824872081,34.132988030291));
#72057=CARTESIAN_POINT('',(0.600000000000001,-26.1673599741116,33.234910440458));
#72058=CARTESIAN_POINT('Ctrl Pts',(0.600000000000004,-26.1673599741116,
33.234910440458));
#72059=CARTESIAN_POINT('Ctrl Pts',(0.370217470899579,-26.4376444612456,
33.3145607080715));
#72060=CARTESIAN_POINT('Ctrl Pts',(0.138207714141626,-26.7099230322463,
33.3938750538235));
#72061=CARTESIAN_POINT('',(1.67735469196904,-25.4310730087083,33.8016349549212));
#72062=CARTESIAN_POINT('Origin',(8.1449754609635,0.,0.));
#72063=CARTESIAN_POINT('',(1.90339248332146,-23.1273809239214,30.1149569673582));
#72064=CARTESIAN_POINT('Origin',(0.,-29.1096888385212,24.4259291680885));
#72065=CARTESIAN_POINT('',(0.,-32.1800738014028,28.156475035514));
#72066=CARTESIAN_POINT('',(0.,-9.76844254625099,0.92613767654611));
#72067=CARTESIAN_POINT('',(0.138207714141625,-32.1029248328492,28.2484175959528));
#72068=CARTESIAN_POINT('',(1.46228393816674,-31.3638118563816,29.129258140991));
#72069=CARTESIAN_POINT('',(0.600000000000001,-31.5410006112756,28.1860830985703));
#72070=CARTESIAN_POINT('Ctrl Pts',(0.600000000000004,-31.5410006112756,
28.1860830985703));
#72071=CARTESIAN_POINT('Ctrl Pts',(0.370217470900199,-31.8210099935451,
28.2175888910031));
#72072=CARTESIAN_POINT('Ctrl Pts',(0.138207714141625,-32.1029248328492,
28.2484175959528));
#72073=CARTESIAN_POINT('',(1.67735469196904,-30.9143101784803,28.872052684018));
#72074=CARTESIAN_POINT('Origin',(8.1449754609635,0.,0.));
#72075=CARTESIAN_POINT('',(1.90339248332146,-28.0054314386442,25.6414155514355));
#72076=CARTESIAN_POINT('Origin',(0.,-32.9089653438087,19.));
#72077=CARTESIAN_POINT('',(0.,-36.580506751568,22.1407037396679));
#72078=CARTESIAN_POINT('',(0.,-8.03170628213326,-2.28046286024977));
#72079=CARTESIAN_POINT('',(0.138207714141621,-36.5204955072697,22.244646263818));
#72080=CARTESIAN_POINT('',(1.46228393816674,-35.9455676731535,23.2404504831928));
#72081=CARTESIAN_POINT('',(0.600000000000001,-35.9562839053824,22.2808358845789));
#72082=CARTESIAN_POINT('Ctrl Pts',(0.600000000000004,-35.9562839053824,
22.2808358845789));
#72083=CARTESIAN_POINT('Ctrl Pts',(0.370217470899393,-36.2375102394005,
22.2632399142707));
#72084=CARTESIAN_POINT('Ctrl Pts',(0.138207714141621,-36.5204955072697,
22.244646263818));
#72085=CARTESIAN_POINT('',(1.67735469196904,-35.4582316768749,23.0652077022745));
#72086=CARTESIAN_POINT('Origin',(8.1449754609635,0.,0.));
#72087=CARTESIAN_POINT('',(1.90339248332146,-32.0325510905359,20.3887726991648));
#72088=CARTESIAN_POINT('Origin',(0.,-35.7083195898645,12.9967654463754));
#72089=CARTESIAN_POINT('',(0.,-39.8694595147163,15.4521983644287));
#72090=CARTESIAN_POINT('',(0.,-5.89916452186253,-4.59321757154364));
#72091=CARTESIAN_POINT('',(0.138207714141621,-39.8284094059642,15.5649826112914));
#72092=CARTESIAN_POINT('',(1.46228393816674,-39.4351356055115,16.6454934976982));
#72093=CARTESIAN_POINT('',(0.600000000000001,-39.2790537077817,15.6985967468815));
#72094=CARTESIAN_POINT('Ctrl Pts',(0.600000000000005,-39.2790537077817,
15.6985967468815));
#72095=CARTESIAN_POINT('Ctrl Pts',(0.370217470897566,-39.5529520736978,
15.6324336584854));
#72096=CARTESIAN_POINT('Ctrl Pts',(0.138207714141621,-39.8284094059642,
15.5649826112914));
#72097=CARTESIAN_POINT('',(1.67735469196904,-38.9247727484987,16.5575380560557));
#72098=CARTESIAN_POINT('Origin',(8.1449754609635,0.,0.));
#72099=CARTESIAN_POINT('',(1.90339248332146,-35.0863778867947,14.5166273056467));
#72100=CARTESIAN_POINT('Origin',(0.,-37.4226946144639,6.59863075134337));
#72101=CARTESIAN_POINT('',(0.,-41.9469989254299,8.29418576107604));
#72102=CARTESIAN_POINT('',(0.,-3.70983076103834,-6.03580125637146));
#72103=CARTESIAN_POINT('',(0.138207714141622,-41.9261572390061,8.41238483838186));
#72104=CARTESIAN_POINT('',(1.46228393816674,-41.7264868976375,9.5447716153021));
#72105=CARTESIAN_POINT('',(0.600000000000001,-41.4083493394303,8.63936369090334));
#72106=CARTESIAN_POINT('Ctrl Pts',(0.600000000000005,-41.4083493394303,
8.63936369090334));
#72107=CARTESIAN_POINT('Ctrl Pts',(0.370217470898631,-41.6665974739919,
8.52664381638094));
#72108=CARTESIAN_POINT('Ctrl Pts',(0.138207714141622,-41.9261572390061,
8.41238483838186));
#72109=CARTESIAN_POINT('',(1.67735469196904,-41.2086042970448,9.54677599452215));
#72110=CARTESIAN_POINT('Origin',(8.1449754609635,0.,0.));
#72111=CARTESIAN_POINT('',(1.90339248332146,-37.074122845527,8.20340153721442));
#72112=CARTESIAN_POINT('Origin',(0.,-38.,4.65365783675994E-15));
#72113=CARTESIAN_POINT('',(0.,-42.75,0.884158520433542));
#72114=CARTESIAN_POINT('',(0.,-1.75577510798945,-6.74645057995377));
#72115=CARTESIAN_POINT('',(0.13820771414162,-42.75,1.00418100903021));
#72116=CARTESIAN_POINT('',(1.46228393816674,-42.75,2.15403667726255));
#72117=CARTESIAN_POINT('',(0.600000000000001,-42.2794732300361,1.31762794090605));
#72118=CARTESIAN_POINT('Ctrl Pts',(0.600000000000006,-42.2794732300361,
1.31762794090605));
#72119=CARTESIAN_POINT('Ctrl Pts',(0.370217470900961,-42.5142243943533,
1.16177621660692));
#72120=CARTESIAN_POINT('Ctrl Pts',(0.13820771414162,-42.75,1.00418100903021));
#72121=CARTESIAN_POINT('',(1.67735469196904,-42.240333256585,2.24593997529678));
#72122=CARTESIAN_POINT('Origin',(8.1449754609635,0.,0.));
#72123=CARTESIAN_POINT('',(1.90339248332146,-37.9353893420094,1.64091956419534));
#72124=CARTESIAN_POINT('Origin',(0.,-37.4226946144639,-6.59863075134334));
#72125=CARTESIAN_POINT('',(0.,-42.2540639571139,-6.55273342944651));
#72126=CARTESIAN_POINT('',(0.,-0.246045426418917,-6.95180363335973));
#72127=CARTESIAN_POINT('',(0.138207714141624,-42.2749056435377,-6.43453435214068));
#72128=CARTESIAN_POINT('',(1.46228393816674,-42.4745759849063,-5.30214757522045));
#72129=CARTESIAN_POINT('',(0.600000000000001,-41.8659567209931,-6.04414326732375));
#72130=CARTESIAN_POINT('Ctrl Pts',(0.600000000000006,-41.8659567209931,
-6.04414326732374));
#72131=CARTESIAN_POINT('Ctrl Pts',(0.370217470894059,-42.0700781197365,
-6.23839136562854));
#72132=CARTESIAN_POINT('Ctrl Pts',(0.138207714141624,-42.2749056435377,
-6.43453435214068));
#72133=CARTESIAN_POINT('',(1.67735469196904,-41.9886110647639,-5.1231377935775));
#72134=CARTESIAN_POINT('Origin',(8.1449754609635,0.,0.));
#72135=CARTESIAN_POINT('',(1.90339248332146,-37.6440082295681,-4.97142091943644));
#72136=CARTESIAN_POINT('Origin',(0.,-35.7083195898645,-12.9967654463754));
#72137=CARTESIAN_POINT('',(0.,-40.4742595624789,-13.790523889916));
#72138=CARTESIAN_POINT('',(0.,0.717737476618173,-6.93007335047185));
#72139=CARTESIAN_POINT('',(0.138207714141626,-40.515309671231,-13.6777396430533));
#72140=CARTESIAN_POINT('',(1.46228393816674,-40.9085834716837,-12.5972287566465));
#72141=CARTESIAN_POINT('',(0.600000000000001,-40.1803643021789,-13.22226624086));
#72142=CARTESIAN_POINT('Ctrl Pts',(0.600000000000006,-40.1803643021789,
-13.22226624086));
#72143=CARTESIAN_POINT('Ctrl Pts',(0.370217470897712,-40.3476538099286,
-13.4490085829895));
#72144=CARTESIAN_POINT('Ctrl Pts',(0.138207714141626,-40.515309671231,-13.6777396430533));
#72145=CARTESIAN_POINT('',(1.67735469196904,-40.4610861730024,-12.3365516130268));
#72146=CARTESIAN_POINT('Origin',(8.1449754609635,0.,0.));
#72147=CARTESIAN_POINT('',(1.90339248332146,-36.2088329758587,-11.4327072940915));
#72148=CARTESIAN_POINT('Origin',(0.,-32.9089653438087,-19.));
#72149=CARTESIAN_POINT('',(0.,-37.4646652720015,-20.6092962603321));
#72150=CARTESIAN_POINT('',(0.,1.15119163149133,-6.96828498131187));
#72151=CARTESIAN_POINT('',(0.138207714141633,-37.5246765162999,-20.5053537361819));
#72152=CARTESIAN_POINT('',(1.46228393816674,-38.099604350416,-19.5095495168072));
#72153=CARTESIAN_POINT('',(0.600000000000001,-37.2739118462884,-19.9986373454573));
#72154=CARTESIAN_POINT('Ctrl Pts',(0.600000000000006,-37.2739118462884,
-19.9986373454572));
#72155=CARTESIAN_POINT('Ctrl Pts',(0.370217470897372,-37.3992864560074,
-20.2509844800864));
#72156=CARTESIAN_POINT('Ctrl Pts',(0.138207714141633,-37.5246765162999,
-20.5053537361819));
#72157=CARTESIAN_POINT('',(1.67735469196904,-37.7041716521717,-19.1751255543105));
#72158=CARTESIAN_POINT('Origin',(8.1449754609635,0.,0.));
#72159=CARTESIAN_POINT('',(1.90339248332146,-33.6734706547313,-17.5466166428447));
#72160=CARTESIAN_POINT('Origin',(0.,-29.1096888385212,-24.4259291680885));
#72161=CARTESIAN_POINT('',(0.,-33.3167260852698,-26.8018655926851));
#72162=CARTESIAN_POINT('',(0.,1.18128350576745,-7.31901513140711));
#72163=CARTESIAN_POINT('',(0.138207714141623,-33.3938750538235,-26.7099230322464));
#72164=CARTESIAN_POINT('',(1.46228393816674,-34.132988030291,-25.8290824872081));
#72165=CARTESIAN_POINT('',(0.600000000000001,-33.234910440458,-26.1673599741116));
#72166=CARTESIAN_POINT('Ctrl Pts',(0.600000000000006,-33.234910440458,-26.1673599741116));
#72167=CARTESIAN_POINT('Ctrl Pts',(0.370217470902497,-33.3145607080705,
-26.4376444612422));
#72168=CARTESIAN_POINT('Ctrl Pts',(0.138207714141623,-33.3938750538235,
-26.7099230322464));
#72169=CARTESIAN_POINT('',(1.67735469196904,-33.8016349549212,-25.4310730087083));
#72170=CARTESIAN_POINT('Origin',(8.1449754609635,0.,0.));
#72171=CARTESIAN_POINT('',(1.90339248332146,-30.1149569673582,-23.1273809239214));
#72172=CARTESIAN_POINT('Origin',(0.,-24.4259291680885,-29.1096888385212));
#72173=CARTESIAN_POINT('',(0.,-28.156475035514,-32.1800738014028));
#72174=CARTESIAN_POINT('',(0.,1.02556763176512,-8.16211284449324));
#72175=CARTESIAN_POINT('',(0.138207714141625,-28.2484175959528,-32.1029248328492));
#72176=CARTESIAN_POINT('',(1.46228393816674,-29.129258140991,-31.3638118563816));
#72177=CARTESIAN_POINT('',(0.600000000000001,-28.1860830985703,-31.5410006112756));
#72178=CARTESIAN_POINT('Ctrl Pts',(0.600000000000006,-28.1860830985703,
-31.5410006112756));
#72179=CARTESIAN_POINT('Ctrl Pts',(0.370217470901873,-28.2175888910029,
-31.8210099935431));
#72180=CARTESIAN_POINT('Ctrl Pts',(0.138207714141625,-28.2484175959528,
-32.1029248328492));
#72181=CARTESIAN_POINT('',(1.67735469196904,-28.872052684018,-30.9143101784803));
#72182=CARTESIAN_POINT('Origin',(8.1449754609635,0.,0.));
#72183=CARTESIAN_POINT('',(1.90339248332146,-25.6414155514355,-28.0054314386442));
#72184=CARTESIAN_POINT('Origin',(0.,-19.,-32.9089653438087));
#72185=CARTESIAN_POINT('',(0.,-22.1407037396679,-36.580506751568));
#72186=CARTESIAN_POINT('',(0.,0.959225753562968,-9.57625716905698));
#72187=CARTESIAN_POINT('',(0.138207714141625,-22.2446462638181,-36.5204955072696));
#72188=CARTESIAN_POINT('',(1.46228393816674,-23.2404504831928,-35.9455676731535));
#72189=CARTESIAN_POINT('',(0.600000000000001,-22.2808358845789,-35.9562839053824));
#72190=CARTESIAN_POINT('Ctrl Pts',(0.600000000000006,-22.2808358845789,
-35.9562839053824));
#72191=CARTESIAN_POINT('Ctrl Pts',(0.37021747090221,-22.2632399142709,-36.237510239397));
#72192=CARTESIAN_POINT('Ctrl Pts',(0.138207714141625,-22.2446462638181,
-36.5204955072696));
#72193=CARTESIAN_POINT('',(1.67735469196904,-23.0652077022745,-35.4582316768749));
#72194=CARTESIAN_POINT('Origin',(8.14497546096349,0.,0.));
#72195=CARTESIAN_POINT('',(1.90339248332146,-20.3887726991648,-32.0325510905359));
#72196=CARTESIAN_POINT('Origin',(0.,-12.9967654463754,-35.7083195898645));
#72197=CARTESIAN_POINT('',(0.,-15.4521983644287,-39.8694595147163));
#72198=CARTESIAN_POINT('',(0.,1.27408525976888,-11.5239868808221));
#72199=CARTESIAN_POINT('',(0.138207714141625,-15.5649826112914,-39.8284094059641));
#72200=CARTESIAN_POINT('',(1.46228393816674,-16.6454934976982,-39.4351356055115));
#72201=CARTESIAN_POINT('',(0.600000000000001,-15.6985967468815,-39.2790537077817));
#72202=CARTESIAN_POINT('Ctrl Pts',(0.600000000000006,-15.6985967468815,
-39.2790537077817));
#72203=CARTESIAN_POINT('Ctrl Pts',(0.370217470897549,-15.6324336584855,
-39.5529520736978));
#72204=CARTESIAN_POINT('Ctrl Pts',(0.138207714141625,-15.5649826112914,
-39.8284094059641));
#72205=CARTESIAN_POINT('',(1.67735469196904,-16.5575380560557,-38.9247727484987));
#72206=CARTESIAN_POINT('Origin',(8.1449754609635,0.,0.));
#72207=CARTESIAN_POINT('',(1.90339248332146,-14.5166273056467,-35.0863778867947));
#72208=CARTESIAN_POINT('Origin',(0.,-6.59863075134335,-37.4226946144639));
#72209=CARTESIAN_POINT('',(0.,-8.29418576107602,-41.9469989254299));
#72210=CARTESIAN_POINT('',(0.,2.23479659694533,-13.8521745174671));
#72211=CARTESIAN_POINT('',(0.138207714141623,-8.41238483838184,-41.9261572390061));
#72212=CARTESIAN_POINT('',(1.46228393816674,-9.54477161530208,-41.7264868976375));
#72213=CARTESIAN_POINT('',(0.600000000000001,-8.63936369090332,-41.4083493394303));
#72214=CARTESIAN_POINT('Ctrl Pts',(0.600000000000007,-8.63936369090333,
-41.4083493394303));
#72215=CARTESIAN_POINT('Ctrl Pts',(0.370217470894352,-8.52664381637882,
-41.6665974739967));
#72216=CARTESIAN_POINT('Ctrl Pts',(0.138207714141623,-8.41238483838184,
-41.9261572390061));
#72217=CARTESIAN_POINT('',(1.67735469196904,-9.54677599452213,-41.2086042970448));
#72218=CARTESIAN_POINT('Origin',(8.1449754609635,0.,0.));
#72219=CARTESIAN_POINT('',(1.90339248332146,-8.20340153721441,-37.0741228455271));
#72220=CARTESIAN_POINT('Origin',(0.,-6.98048675513991E-15,-38.));
#72221=CARTESIAN_POINT('',(0.,-0.884158520433544,-42.75));
#72222=CARTESIAN_POINT('',(0.,4.03771734711804,-16.3080104352708));
#72223=CARTESIAN_POINT('',(0.138207714141621,-1.00418100903022,-42.75));
#72224=CARTESIAN_POINT('',(1.46228393816674,-2.15403667726255,-42.75));
#72225=CARTESIAN_POINT('',(0.600000000000001,-1.31762794090605,-42.2794732300361));
#72226=CARTESIAN_POINT('Ctrl Pts',(0.600000000000007,-1.31762794090605,
-42.2794732300361));
#72227=CARTESIAN_POINT('Ctrl Pts',(0.37021747090171,-1.16177621660743,-42.5142243943525));
#72228=CARTESIAN_POINT('Ctrl Pts',(0.138207714141621,-1.00418100903022,
-42.75));
#72229=CARTESIAN_POINT('',(1.67735469196904,-2.24593997529678,-42.240333256585));
#72230=CARTESIAN_POINT('Origin',(8.1449754609635,0.,0.));
#72231=CARTESIAN_POINT('',(1.90339248332146,-1.64091956419534,-37.9353893420094));
#72232=CARTESIAN_POINT('Origin',(0.,6.59863075134334,-37.4226946144639));
#72233=CARTESIAN_POINT('',(0.,6.5527334294465,-42.2540639571139));
#72234=CARTESIAN_POINT('',(0.,6.77774154709997,-18.5686444914235));
#72235=CARTESIAN_POINT('',(0.138207714141623,6.43453435214068,-42.2749056435377));
#72236=CARTESIAN_POINT('',(1.46228393816674,5.30214757522045,-42.4745759849063));
#72237=CARTESIAN_POINT('',(0.600000000000001,6.04414326732375,-41.8659567209931));
#72238=CARTESIAN_POINT('Ctrl Pts',(0.600000000000007,6.04414326732374,-41.8659567209931));
#72239=CARTESIAN_POINT('Ctrl Pts',(0.370217470894012,6.23839136562858,-42.0700781197365));
#72240=CARTESIAN_POINT('Ctrl Pts',(0.138207714141623,6.43453435214068,-42.2749056435377));
#72241=CARTESIAN_POINT('',(1.67735469196904,5.1231377935775,-41.9886110647639));
#72242=CARTESIAN_POINT('Origin',(8.1449754609635,0.,0.));
#72243=CARTESIAN_POINT('',(1.90339248332146,4.97142091943644,-37.6440082295681));
#72244=CARTESIAN_POINT('Origin',(0.,12.9967654463754,-35.7083195898645));
#72245=CARTESIAN_POINT('',(0.,13.7905238899159,-40.4742595624789));
#72246=CARTESIAN_POINT('',(0.,10.4273633827345,-20.2809359815683));
#72247=CARTESIAN_POINT('',(0.138207714141626,13.6777396430533,-40.515309671231));
#72248=CARTESIAN_POINT('',(1.46228393816674,12.5972287566465,-40.9085834716837));
#72249=CARTESIAN_POINT('',(0.600000000000001,13.22226624086,-40.1803643021789));
#72250=CARTESIAN_POINT('Ctrl Pts',(0.600000000000008,13.22226624086,-40.1803643021789));
#72251=CARTESIAN_POINT('Ctrl Pts',(0.370217470897429,13.4490085829897,-40.3476538099288));
#72252=CARTESIAN_POINT('Ctrl Pts',(0.138207714141626,13.6777396430533,-40.515309671231));
#72253=CARTESIAN_POINT('',(1.67735469196904,12.3365516130267,-40.4610861730024));
#72254=CARTESIAN_POINT('Origin',(8.1449754609635,0.,0.));
#72255=CARTESIAN_POINT('',(1.90339248332146,11.4327072940915,-36.2088329758587));
#72256=CARTESIAN_POINT('Origin',(0.,19.,-32.9089653438087));
#72257=CARTESIAN_POINT('',(0.,20.6092962603321,-37.4646652720015));
#72258=CARTESIAN_POINT('',(0.,14.8307888551629,-21.1064928088663));
#72259=CARTESIAN_POINT('',(0.138207714141623,20.505353736182,-37.5246765162999));
#72260=CARTESIAN_POINT('',(1.46228393816674,19.5095495168072,-38.099604350416));
#72261=CARTESIAN_POINT('',(0.600000000000001,19.9986373454573,-37.2739118462884));
#72262=CARTESIAN_POINT('Ctrl Pts',(0.600000000000008,19.9986373454573,-37.2739118462884));
#72263=CARTESIAN_POINT('Ctrl Pts',(0.370217470899336,20.2509844800843,-37.3992864560063));
#72264=CARTESIAN_POINT('Ctrl Pts',(0.138207714141623,20.505353736182,-37.5246765162999));
#72265=CARTESIAN_POINT('',(1.67735469196904,19.1751255543105,-37.7041716521717));
#72266=CARTESIAN_POINT('Origin',(8.1449754609635,0.,0.));
#72267=CARTESIAN_POINT('',(1.90339248332146,17.5466166428447,-33.6734706547313));
#72268=CARTESIAN_POINT('Origin',(0.,24.4259291680885,-29.1096888385212));
#72269=CARTESIAN_POINT('',(0.,26.8018655926851,-33.3167260852698));
#72270=CARTESIAN_POINT('',(0.,19.7140853569221,-20.7664932002776));
#72271=CARTESIAN_POINT('',(0.138207714141623,26.7099230322463,-33.3938750538235));
#72272=CARTESIAN_POINT('',(1.46228393816674,25.8290824872081,-34.132988030291));
#72273=CARTESIAN_POINT('',(0.600000000000001,26.1673599741116,-33.234910440458));
#72274=CARTESIAN_POINT('Ctrl Pts',(0.600000000000008,26.1673599741116,-33.234910440458));
#72275=CARTESIAN_POINT('Ctrl Pts',(0.370217470904163,26.4376444612402,-33.3145607080699));
#72276=CARTESIAN_POINT('Ctrl Pts',(0.138207714141623,26.7099230322463,-33.3938750538235));
#72277=CARTESIAN_POINT('',(1.67735469196904,25.4310730087083,-33.8016349549212));
#72278=CARTESIAN_POINT('Origin',(8.1449754609635,0.,0.));
#72279=CARTESIAN_POINT('',(1.90339248332146,23.1273809239214,-30.1149569673582));
#72280=CARTESIAN_POINT('Origin',(0.,29.1096888385212,-24.4259291680885));
#72281=CARTESIAN_POINT('',(0.,32.1800738014028,-28.156475035514));
#72282=CARTESIAN_POINT('',(0.,24.710407536182,-19.0807620699926));
#72283=CARTESIAN_POINT('',(0.13820771414163,32.1029248328491,-28.2484175959528));
#72284=CARTESIAN_POINT('',(1.46228393816674,31.3638118563816,-29.129258140991));
#72285=CARTESIAN_POINT('',(0.600000000000001,31.5410006112756,-28.1860830985703));
#72286=CARTESIAN_POINT('Ctrl Pts',(0.600000000000009,31.5410006112756,-28.1860830985703));
#72287=CARTESIAN_POINT('Ctrl Pts',(0.370217470894748,31.8210099935517,-28.2175888910039));
#72288=CARTESIAN_POINT('Ctrl Pts',(0.13820771414163,32.1029248328491,-28.2484175959528));
#72289=CARTESIAN_POINT('',(1.67735469196904,30.9143101784803,-28.872052684018));
#72290=CARTESIAN_POINT('Origin',(8.1449754609635,0.,0.));
#72291=CARTESIAN_POINT('',(1.90339248332146,28.0054314386442,-25.6414155514355));
#72292=CARTESIAN_POINT('Origin',(0.,32.9089653438087,-19.));
#72293=CARTESIAN_POINT('',(0.,36.580506751568,-22.1407037396679));
#72294=CARTESIAN_POINT('',(0.,29.3974942757438,-15.9962233595133));
#72295=CARTESIAN_POINT('',(0.138207714141626,36.5204955072696,-22.2446462638181));
#72296=CARTESIAN_POINT('',(1.46228393816674,35.9455676731535,-23.2404504831928));
#72297=CARTESIAN_POINT('',(0.600000000000001,35.9562839053824,-22.2808358845789));
#72298=CARTESIAN_POINT('Ctrl Pts',(0.600000000000009,35.9562839053824,-22.2808358845789));
#72299=CARTESIAN_POINT('Ctrl Pts',(0.370217470898111,36.237510239402,-22.2632399142706));
#72300=CARTESIAN_POINT('Ctrl Pts',(0.138207714141626,36.5204955072696,-22.2446462638181));
#72301=CARTESIAN_POINT('',(1.67735469196904,35.4582316768749,-23.0652077022745));
#72302=CARTESIAN_POINT('Origin',(8.1449754609635,0.,0.));
#72303=CARTESIAN_POINT('',(1.90339248332146,32.0325510905359,-20.3887726991648));
#72304=CARTESIAN_POINT('Origin',(0.,35.7083195898645,-12.9967654463754));
#72305=CARTESIAN_POINT('',(0.,39.8694595147163,-15.4521983644287));
#72306=CARTESIAN_POINT('',(0.,33.3431191925968,-11.6010923812716));
#72307=CARTESIAN_POINT('',(0.138207714141623,39.8284094059641,-15.5649826112914));
#72308=CARTESIAN_POINT('',(1.46228393816674,39.4351356055115,-16.6454934976982));
#72309=CARTESIAN_POINT('',(0.600000000000001,39.2790537077817,-15.6985967468815));
#72310=CARTESIAN_POINT('Ctrl Pts',(0.600000000000009,39.2790537077817,-15.6985967468815));
#72311=CARTESIAN_POINT('Ctrl Pts',(0.370217470896577,39.552952073699,-15.6324336584852));
#72312=CARTESIAN_POINT('Ctrl Pts',(0.138207714141623,39.8284094059641,-15.5649826112914));
#72313=CARTESIAN_POINT('',(1.67735469196904,38.9247727484987,-16.5575380560557));
#72314=CARTESIAN_POINT('Origin',(8.1449754609635,0.,0.));
#72315=CARTESIAN_POINT('',(1.90339248332146,35.0863778867947,-14.5166273056467));
#72316=CARTESIAN_POINT('Origin',(0.,37.4226946144639,-6.59863075134336));
#72317=CARTESIAN_POINT('',(0.,41.9469989254299,-8.29418576107603));
#72318=CARTESIAN_POINT('',(0.,36.1531791768932,-6.12285964662596));
#72319=CARTESIAN_POINT('',(0.138207714141624,41.9261572390061,-8.41238483838185));
#72320=CARTESIAN_POINT('',(1.46228393816674,41.7264868976375,-9.54477161530208));
#72321=CARTESIAN_POINT('',(0.600000000000001,41.4083493394303,-8.63936369090333));
#72322=CARTESIAN_POINT('Ctrl Pts',(0.600000000000009,41.4083493394303,-8.63936369090333));
#72323=CARTESIAN_POINT('Ctrl Pts',(0.370217470894459,41.6665974739965,-8.52664381637888));
#72324=CARTESIAN_POINT('Ctrl Pts',(0.138207714141624,41.9261572390061,-8.41238483838185));
#72325=CARTESIAN_POINT('',(1.67735469196904,41.2086042970448,-9.54677599452213));
#72326=CARTESIAN_POINT('Origin',(8.1449754609635,0.,0.));
#72327=CARTESIAN_POINT('',(1.90339248332146,37.0741228455271,-8.20340153721441));
#72328=CARTESIAN_POINT('Origin',(35.,52.,0.));
#72329=CARTESIAN_POINT('',(35.,42.75,-0.884158520433536));
#72330=CARTESIAN_POINT('',(35.,44.9140105592676,-1.28696449396714));
#72331=CARTESIAN_POINT('',(35.,42.75,0.));
#72332=CARTESIAN_POINT('Origin',(35.,52.,0.));
#72333=CARTESIAN_POINT('',(35.,42.2540639571139,6.55273342944652));
#72334=CARTESIAN_POINT('',(35.,44.8929942217219,6.52766396709994));
#72335=CARTESIAN_POINT('',(35.,42.8845273710551,2.97719773202758));
#72336=CARTESIAN_POINT('Origin',(35.,52.,0.));
#72337=CARTESIAN_POINT('',(35.,40.4742595624789,13.790523889916));
#72338=CARTESIAN_POINT('',(35.,42.7301436553725,14.1662371923646));
#72339=CARTESIAN_POINT('',(35.,43.2132817780509,6.26512220124733));
#72340=CARTESIAN_POINT('Origin',(35.,52.,0.));
#72341=CARTESIAN_POINT('',(35.,37.4646652720015,20.6092962603321));
#72342=CARTESIAN_POINT('',(35.,38.554281614855,20.9942020999154));
#72343=CARTESIAN_POINT('',(35.,43.5225860117848,10.1166697508023));
#72344=CARTESIAN_POINT('Origin',(35.,52.,0.));
#72345=CARTESIAN_POINT('',(35.,33.3167260852698,26.8018655926851));
#72346=CARTESIAN_POINT('',(35.,32.689238504957,26.4474901710748));
#72347=CARTESIAN_POINT('',(35.,43.4909736336662,14.6766695249408));
#72348=CARTESIAN_POINT('Origin',(35.,52.,0.));
#72349=CARTESIAN_POINT('',(35.,28.156475035514,32.1800738014028));
#72350=CARTESIAN_POINT('',(35.,25.6202580076353,30.0926681235906));
#72351=CARTESIAN_POINT('',(35.,42.7365966237696,19.9458991541776));
#72352=CARTESIAN_POINT('Origin',(35.,52.,0.));
#72353=CARTESIAN_POINT('',(35.,22.1407037396679,36.580506751568));
#72354=CARTESIAN_POINT('',(35.,17.9422199667173,31.672400702755));
#72355=CARTESIAN_POINT('',(35.,40.875,25.764255762587));
#72356=CARTESIAN_POINT('Origin',(35.,52.,0.));
#72357=CARTESIAN_POINT('',(35.,15.4521983644287,39.8694595147163));
#72358=CARTESIAN_POINT('',(35.,10.2957205060146,31.1309491972475));
#72359=CARTESIAN_POINT('',(35.,37.5799388877191,31.8156206126726));
#72360=CARTESIAN_POINT('Origin',(35.,52.,0.));
#72361=CARTESIAN_POINT('',(35.,8.29418576107603,41.9469989254299));
#72362=CARTESIAN_POINT('',(35.,3.29848110862957,28.6167985098503));
#72363=CARTESIAN_POINT('',(35.,32.6394636654781,37.6542695780382));
#72364=CARTESIAN_POINT('Origin',(35.,52.,0.));
#72365=CARTESIAN_POINT('',(35.,0.884158520433538,42.75));
#72366=CARTESIAN_POINT('',(35.,-2.51990383326145,24.4622203695749));
#72367=CARTESIAN_POINT('',(35.,26.,42.75));
#72368=CARTESIAN_POINT('Origin',(35.,52.,0.));
#72369=CARTESIAN_POINT('',(35.,-6.55273342944652,42.2540639571139));
#72370=CARTESIAN_POINT('',(35.,-6.77229176400553,19.1423144546885));
#72371=CARTESIAN_POINT('',(35.,17.7925444749555,46.5467933045056));
#72372=CARTESIAN_POINT('Origin',(35.,52.,0.));
#72373=CARTESIAN_POINT('',(35.,-13.790523889916,40.4742595624789));
#72374=CARTESIAN_POINT('',(35.,-9.25112687675228,13.2184944708942));
#72375=CARTESIAN_POINT('',(35.,8.33721663337438,48.5280984645226));
#72376=CARTESIAN_POINT('Origin',(35.,52.,0.));
#72377=CARTESIAN_POINT('',(35.,-20.6092962603321,37.4646652720015));
#72378=CARTESIAN_POINT('',(35.,-9.94419665558418,7.27321159056857));
#72379=CARTESIAN_POINT('',(35.,-1.87499999999998,48.2809162609825));
#72380=CARTESIAN_POINT('Origin',(35.,52.,0.));
#72381=CARTESIAN_POINT('',(35.,-26.8018655926851,33.3167260852698));
#72382=CARTESIAN_POINT('',(35.,-9.02739147575637,1.84371448565053));
#72383=CARTESIAN_POINT('',(35.,-12.2217440044295,45.550900732495));
#72384=CARTESIAN_POINT('Origin',(35.,52.,0.));
#72385=CARTESIAN_POINT('',(35.,-32.1800738014028,28.156475035514));
#72386=CARTESIAN_POINT('',(35.,-6.8356053136496,-2.63728643807825));
#72387=CARTESIAN_POINT('',(35.,-22.0058262530064,40.2816711032583));
#72388=CARTESIAN_POINT('Origin',(35.,52.,0.));
#72389=CARTESIAN_POINT('',(35.,-36.580506751568,22.1407037396679));
#72390=CARTESIAN_POINT('',(35.,-3.8155269311951,-5.88705986787639));
#72391=CARTESIAN_POINT('',(35.,-30.5225860117848,32.6333302491977));
#72392=CARTESIAN_POINT('Origin',(35.,52.,0.));
#72393=CARTESIAN_POINT('',(35.,-39.8694595147163,15.4521983644287));
#72394=CARTESIAN_POINT('',(35.,-0.466222705023521,-7.79912374625847));
#72395=CARTESIAN_POINT('',(35.,-37.1304372991443,22.9776000530974));
#72396=CARTESIAN_POINT('Origin',(35.,52.,0.));
#72397=CARTESIAN_POINT('',(35.,-41.9469989254299,8.29418576107603));
#72398=CARTESIAN_POINT('',(35.,2.72515398447831,-8.44741415260574));
#72399=CARTESIAN_POINT('',(35.,-41.3165355114887,11.869721458495));
#72400=CARTESIAN_POINT('Origin',(35.,52.,0.));
#72401=CARTESIAN_POINT('',(35.,-42.75,0.884158520433541));
#72402=CARTESIAN_POINT('',(35.,5.34464795765368,-8.06811364356874));
#72403=CARTESIAN_POINT('',(35.,-42.75,8.41944674413805E-15));
#72404=CARTESIAN_POINT('Origin',(35.,52.,0.));
#72405=CARTESIAN_POINT('',(35.,-42.2540639571139,-6.55273342944651));
#72406=CARTESIAN_POINT('',(35.,7.10231334221714,-7.02161199697211));
#72407=CARTESIAN_POINT('',(35.,-41.3165355114887,-11.8697214584949));
#72408=CARTESIAN_POINT('Origin',(35.,52.,0.));
#72409=CARTESIAN_POINT('',(35.,-40.4742595624789,-13.790523889916));
#72410=CARTESIAN_POINT('',(35.,7.86639521349345,-5.73947769227399));
#72411=CARTESIAN_POINT('',(35.,-37.1304372991443,-22.9776000530973));
#72412=CARTESIAN_POINT('Origin',(35.,52.,0.));
#72413=CARTESIAN_POINT('',(35.,-37.4646652720015,-20.6092962603321));
#72414=CARTESIAN_POINT('',(35.,7.67678296510018,-4.66312663129778));
#72415=CARTESIAN_POINT('',(35.,-30.5225860117848,-32.6333302491977));
#72416=CARTESIAN_POINT('Origin',(35.,52.,0.));
#72417=CARTESIAN_POINT('',(35.,-33.3167260852698,-26.8018655926851));
#72418=CARTESIAN_POINT('',(35.,6.73618681903107,-4.18186745644989));
#72419=CARTESIAN_POINT('',(35.,-22.0058262530064,-40.2816711032583));
#72420=CARTESIAN_POINT('Origin',(35.,52.,0.));
#72421=CARTESIAN_POINT('',(35.,-28.156475035514,-32.1800738014028));
#72422=CARTESIAN_POINT('',(35.,5.38022362813726,-4.57806086793601));
#72423=CARTESIAN_POINT('',(35.,-12.2217440044295,-45.550900732495));
#72424=CARTESIAN_POINT('Origin',(35.,52.,0.));
#72425=CARTESIAN_POINT('',(35.,-22.1407037396679,-36.580506751568));
#72426=CARTESIAN_POINT('',(35.,4.03018609631655,-5.98624709660142));
#72427=CARTESIAN_POINT('',(35.,-1.87500000000003,-48.2809162609824));
#72428=CARTESIAN_POINT('Origin',(35.,52.,0.));
#72429=CARTESIAN_POINT('',(35.,-15.4521983644287,-39.8694595147163));
#72430=CARTESIAN_POINT('',(35.,3.13439725403449,-8.37137845275046));
#72431=CARTESIAN_POINT('',(35.,8.33721663337434,-48.5280984645226));
#72432=CARTESIAN_POINT('Origin',(35.,52.,0.));
#72433=CARTESIAN_POINT('',(35.,-8.29418576107602,-41.9469989254299));
#72434=CARTESIAN_POINT('',(35.,3.10546165827712,-11.5289507542864));
#72435=CARTESIAN_POINT('',(35.,17.7925444749555,-46.5467933045056));
#72436=CARTESIAN_POINT('Origin',(35.,52.,0.));
#72437=CARTESIAN_POINT('',(35.,-0.884158520433544,-42.75));
#72438=CARTESIAN_POINT('',(35.,4.26124531634016,-15.107142232039));
#72439=CARTESIAN_POINT('',(35.,26.,-42.75));
#72440=CARTESIAN_POINT('Origin',(35.,52.,0.));
#72441=CARTESIAN_POINT('',(35.,6.55273342944651,-42.2540639571139));
#72442=CARTESIAN_POINT('',(35.,6.7769842000665,-18.6483664248163));
#72443=CARTESIAN_POINT('',(35.,32.6394636654781,-37.6542695780382));
#72444=CARTESIAN_POINT('Origin',(35.,52.,0.));
#72445=CARTESIAN_POINT('',(35.,13.7905238899159,-40.4742595624789));
#72446=CARTESIAN_POINT('',(35.,10.6545880078863,-21.6452539709848));
#72447=CARTESIAN_POINT('',(35.,37.579938887719,-31.8156206126726));
#72448=CARTESIAN_POINT('Origin',(35.,52.,0.));
#72449=CARTESIAN_POINT('',(35.,20.6092962603321,-37.4646652720015));
#72450=CARTESIAN_POINT('',(35.,15.713132075629,-23.6042870591862));
#72451=CARTESIAN_POINT('',(35.,40.875,-25.764255762587));
#72452=CARTESIAN_POINT('Origin',(35.,52.,0.));
#72453=CARTESIAN_POINT('',(35.,26.8018655926851,-33.3167260852698));
#72454=CARTESIAN_POINT('',(35.,21.6019661517683,-24.1093372002754));
#72455=CARTESIAN_POINT('',(35.,42.7365966237696,-19.9458991541776));
#72456=CARTESIAN_POINT('Origin',(35.,52.,0.));
#72457=CARTESIAN_POINT('',(35.,32.1800738014028,-28.156475035514));
#72458=CARTESIAN_POINT('',(35.,27.835123677877,-22.8773208175763));
#72459=CARTESIAN_POINT('',(35.,43.4909736336662,-14.6766695249409));
#72460=CARTESIAN_POINT('Origin',(35.,52.,0.));
#72461=CARTESIAN_POINT('',(35.,36.580506751568,-22.1407037396679));
#72462=CARTESIAN_POINT('',(35.,33.8431208681613,-19.7990937382771));
#72463=CARTESIAN_POINT('',(35.,43.5225860117848,-10.1166697508023));
#72464=CARTESIAN_POINT('Origin',(35.,52.,0.));
#72465=CARTESIAN_POINT('',(35.,39.8694595147163,-15.4521983644287));
#72466=CARTESIAN_POINT('',(35.,39.0361049449744,-14.9604469982386));
#72467=CARTESIAN_POINT('',(35.,43.2132817780509,-6.26512220124734));
#72468=CARTESIAN_POINT('Origin',(35.,52.,0.));
#72469=CARTESIAN_POINT('',(35.,41.9469989254299,-8.29418576107602));
#72470=CARTESIAN_POINT('',(35.,42.870903248615,-8.64043360295818));
#72471=CARTESIAN_POINT('',(35.,42.8845273710551,-2.97719773202758));
#72472=CARTESIAN_POINT('Origin',(33.1,37.1361751213135,-8.2235635438135));
#72473=CARTESIAN_POINT('',(33.3226453080309,41.2086042970448,-9.54677599452213));
#72474=CARTESIAN_POINT('',(33.0964948753266,37.0720625104951,-8.20273209378168));
#72475=CARTESIAN_POINT('',(34.4,41.4083493394303,-8.63936369090333));
#72476=CARTESIAN_POINT('Origin',(26.8550245390365,0.,0.));
#72477=CARTESIAN_POINT('',(34.8617922858584,41.9261572390061,-8.41238483838185));
#72478=CARTESIAN_POINT('Ctrl Pts',(34.8617922858584,41.9261572390061,-8.41238483838185));
#72479=CARTESIAN_POINT('Ctrl Pts',(34.6297825291011,41.6665974739915,-8.52664381638108));
#72480=CARTESIAN_POINT('Ctrl Pts',(34.4,41.4083493394303,-8.63936369090333));
#72481=CARTESIAN_POINT('',(35.4377160618333,42.013006390788,-7.91983882283194));
#72482=CARTESIAN_POINT('Origin',(33.1,35.1439863533772,-14.5472582706722));
#72483=CARTESIAN_POINT('',(33.3226453080309,38.9247727484987,-16.5575380560557));
#72484=CARTESIAN_POINT('',(33.0964948753266,35.0844651005135,-14.5156102591403));
#72485=CARTESIAN_POINT('',(34.4,39.2790537077817,-15.6985967468815));
#72486=CARTESIAN_POINT('Origin',(26.8550245390365,0.,0.));
#72487=CARTESIAN_POINT('',(34.8617922858584,39.8284094059641,-15.5649826112914));
#72488=CARTESIAN_POINT('Ctrl Pts',(34.8617922858584,39.8284094059641,-15.5649826112914));
#72489=CARTESIAN_POINT('Ctrl Pts',(34.6297825291059,39.5529520737019,-15.6324336584845));
#72490=CARTESIAN_POINT('Ctrl Pts',(34.4,39.2790537077817,-15.6985967468815));
#72491=CARTESIAN_POINT('',(35.4377160618333,39.9994688419988,-15.0950006734014));
#72492=CARTESIAN_POINT('Origin',(33.1,32.0839653438087,-20.4289419162443));
#72493=CARTESIAN_POINT('',(33.3226453080309,35.4582316768749,-23.0652077022745));
#72494=CARTESIAN_POINT('',(33.0964948753266,32.0308439720488,-20.3874389520281));
#72495=CARTESIAN_POINT('',(34.4,35.9562839053824,-22.2808358845789));
#72496=CARTESIAN_POINT('Origin',(26.8550245390365,0.,0.));
#72497=CARTESIAN_POINT('',(34.8617922858584,36.5204955072696,-22.2446462638181));
#72498=CARTESIAN_POINT('Ctrl Pts',(34.8617922858584,36.5204955072696,-22.2446462638181));
#72499=CARTESIAN_POINT('Ctrl Pts',(34.6297825291007,36.2375102394006,-22.2632399142707));
#72500=CARTESIAN_POINT('Ctrl Pts',(34.4,35.9562839053824,-22.2808358845789));
#72501=CARTESIAN_POINT('',(35.4377160618333,36.7705676731535,-21.8115085669485));
#72502=CARTESIAN_POINT('Origin',(33.1,28.0490892825384,-25.6899024992348));
#72503=CARTESIAN_POINT('',(33.3226453080309,30.9143101784803,-28.872052684018));
#72504=CARTESIAN_POINT('',(33.0964948753266,28.0039818578826,-25.6398056289004));
#72505=CARTESIAN_POINT('',(34.4,31.5410006112756,-28.1860830985704));
#72506=CARTESIAN_POINT('Origin',(26.8550245390365,0.,0.));
#72507=CARTESIAN_POINT('',(34.8617922858584,32.1029248328491,-28.2484175959528));
#72508=CARTESIAN_POINT('Ctrl Pts',(34.8617922858584,32.1029248328491,-28.2484175959528));
#72509=CARTESIAN_POINT('Ctrl Pts',(34.629782529101,31.8210099935466,-28.2175888910033));
#72510=CARTESIAN_POINT('Ctrl Pts',(34.4,31.5410006112756,-28.1860830985704));
#72511=CARTESIAN_POINT('',(35.4377160618333,32.4244114123644,-27.8652848098447));
#72512=CARTESIAN_POINT('Origin',(33.1,23.1619558369422,-30.170288394504));
#72513=CARTESIAN_POINT('',(33.3226453080309,25.4310730087083,-33.8016349549212));
#72514=CARTESIAN_POINT('',(33.0964948753266,23.1262329256631,-30.1131197861062));
#72515=CARTESIAN_POINT('',(34.4,26.1673599741116,-33.234910440458));
#72516=CARTESIAN_POINT('Origin',(26.8550245390365,0.,0.));
#72517=CARTESIAN_POINT('',(34.8617922858584,26.7099230322463,-33.3938750538235));
#72518=CARTESIAN_POINT('Ctrl Pts',(34.8617922858584,26.7099230322463,-33.3938750538235));
#72519=CARTESIAN_POINT('Ctrl Pts',(34.6297825291025,26.4376444612481,-33.3145607080723));
#72520=CARTESIAN_POINT('Ctrl Pts',(34.4,26.1673599741116,-33.234910440458));
#72521=CARTESIAN_POINT('',(35.4377160618333,27.0930558183544,-33.0723884743082));
#72522=CARTESIAN_POINT('Origin',(33.1,17.5710580837557,-33.7339653438087));
#72523=CARTESIAN_POINT('',(33.3226453080309,19.1751255543105,-37.7041716521717));
#72524=CARTESIAN_POINT('',(33.0964948753266,17.5458051084359,-33.6714620365851));
#72525=CARTESIAN_POINT('',(34.4,19.9986373454573,-37.2739118462884));
#72526=CARTESIAN_POINT('Origin',(26.8550245390365,0.,0.));
#72527=CARTESIAN_POINT('',(34.8617922858584,20.505353736182,-37.5246765162999));
#72528=CARTESIAN_POINT('Ctrl Pts',(34.8617922858584,20.505353736182,-37.5246765162999));
#72529=CARTESIAN_POINT('Ctrl Pts',(34.6297825291059,20.25098448009,-37.3992864560092));
#72530=CARTESIAN_POINT('Ctrl Pts',(34.4,19.9986373454573,-37.2739118462884));
#72531=CARTESIAN_POINT('',(35.4377160618333,20.9384914330515,-37.274604350416));
#72532=CARTESIAN_POINT('Origin',(33.1,11.4462726220786,-36.2726528263519));
#72533=CARTESIAN_POINT('',(33.3226453080309,12.3365516130267,-40.4610861730024));
#72534=CARTESIAN_POINT('',(33.0964948753266,11.4322568815947,-36.2067139516643));
#72535=CARTESIAN_POINT('',(34.4,13.22226624086,-40.1803643021789));
#72536=CARTESIAN_POINT('Origin',(26.8550245390365,0.,0.));
#72537=CARTESIAN_POINT('',(34.8617922858584,13.6777396430533,-40.515309671231));
#72538=CARTESIAN_POINT('Ctrl Pts',(34.8617922858584,13.6777396430533,-40.515309671231));
#72539=CARTESIAN_POINT('Ctrl Pts',(34.6297825291018,13.449008582989,-40.3476538099283));
#72540=CARTESIAN_POINT('Ctrl Pts',(34.4,13.22226624086,-40.1803643021789));
#72541=CARTESIAN_POINT('',(35.4377160618333,14.1477215809433,-40.3442502351963));
#72542=CARTESIAN_POINT('Origin',(33.1,4.9736979588732,-37.7092141076143));
#72543=CARTESIAN_POINT('',(33.3226453080309,5.1231377935775,-41.9886110647639));
#72544=CARTESIAN_POINT('',(33.0964948753266,4.97134531440727,-37.6418431848034));
#72545=CARTESIAN_POINT('',(34.4,6.04414326732375,-41.8659567209931));
#72546=CARTESIAN_POINT('Origin',(26.8550245390365,0.,0.));
#72547=CARTESIAN_POINT('',(34.8617922858584,6.43453435214068,-42.2749056435377));
#72548=CARTESIAN_POINT('Ctrl Pts',(34.8617922858584,6.43453435214068,-42.2749056435377));
#72549=CARTESIAN_POINT('Ctrl Pts',(34.6297825291057,6.23839136562832,-42.0700781197363));
#72550=CARTESIAN_POINT('Ctrl Pts',(34.4,6.04414326732374,-41.8659567209931));
#72551=CARTESIAN_POINT('',(35.4377160618333,6.92708036769059,-42.1880564917558));
#72552=CARTESIAN_POINT('Origin',(33.1,-1.65000000000001,-38.));
#72553=CARTESIAN_POINT('',(33.3226453080309,-2.24593997529678,-42.240333256585));
#72554=CARTESIAN_POINT('',(33.0964948753266,-1.64061806453627,-37.933244060464));
#72555=CARTESIAN_POINT('',(34.4,-1.31762794090605,-42.2794732300362));
#72556=CARTESIAN_POINT('Origin',(26.8550245390365,0.,0.));
#72557=CARTESIAN_POINT('',(34.8617922858584,-1.00418100903022,-42.75));
#72558=CARTESIAN_POINT('Ctrl Pts',(34.8617922858584,-1.00418100903022,-42.75));
#72559=CARTESIAN_POINT('Ctrl Pts',(34.6297825291027,-1.16177621660441,-42.514224394357));
#72560=CARTESIAN_POINT('Ctrl Pts',(34.4,-1.31762794090605,-42.2794732300361));
#72561=CARTESIAN_POINT('',(35.4377160618333,-0.504036677262553,-42.75));
#72562=CARTESIAN_POINT('Origin',(33.1,-8.2235635438135,-37.1361751213135));
#72563=CARTESIAN_POINT('',(33.3226453080309,-9.54677599452213,-41.2086042970448));
#72564=CARTESIAN_POINT('',(33.0964948753266,-8.20273209378168,-37.0720625104951));
#72565=CARTESIAN_POINT('',(34.4,-8.63936369090332,-41.4083493394303));
#72566=CARTESIAN_POINT('Origin',(26.8550245390365,0.,0.));
#72567=CARTESIAN_POINT('',(34.8617922858584,-8.41238483838184,-41.9261572390061));
#72568=CARTESIAN_POINT('Ctrl Pts',(34.8617922858584,-8.41238483838184,-41.9261572390061));
#72569=CARTESIAN_POINT('Ctrl Pts',(34.6297825291012,-8.526643816381,-41.6665974739917));
#72570=CARTESIAN_POINT('Ctrl Pts',(34.4,-8.63936369090332,-41.4083493394303));
#72571=CARTESIAN_POINT('',(35.4377160618333,-7.91983882283194,-42.013006390788));
#72572=CARTESIAN_POINT('Origin',(33.1,-14.5472582706722,-35.1439863533772));
#72573=CARTESIAN_POINT('',(33.3226453080309,-16.5575380560557,-38.9247727484987));
#72574=CARTESIAN_POINT('',(33.0964948753266,-14.5156102591403,-35.0844651005135));
#72575=CARTESIAN_POINT('',(34.4,-15.6985967468815,-39.2790537077817));
#72576=CARTESIAN_POINT('Origin',(26.8550245390365,0.,0.));
#72577=CARTESIAN_POINT('',(34.8617922858584,-15.5649826112914,-39.8284094059641));
#72578=CARTESIAN_POINT('Ctrl Pts',(34.8617922858584,-15.5649826112914,-39.8284094059641));
#72579=CARTESIAN_POINT('Ctrl Pts',(34.6297825291,-15.6324336584862,-39.552952073695));
#72580=CARTESIAN_POINT('Ctrl Pts',(34.4,-15.6985967468815,-39.2790537077817));
#72581=CARTESIAN_POINT('',(35.4377160618333,-15.0950006734014,-39.9994688419988));
#72582=CARTESIAN_POINT('Origin',(33.1,-20.4289419162443,-32.0839653438087));
#72583=CARTESIAN_POINT('',(33.3226453080309,-23.0652077022745,-35.4582316768749));
#72584=CARTESIAN_POINT('',(33.0964948753266,-20.3874389520281,-32.0308439720488));
#72585=CARTESIAN_POINT('',(34.4,-22.2808358845789,-35.9562839053824));
#72586=CARTESIAN_POINT('Origin',(26.8550245390365,0.,0.));
#72587=CARTESIAN_POINT('',(34.8617922858584,-22.2446462638181,-36.5204955072696));
#72588=CARTESIAN_POINT('Ctrl Pts',(34.8617922858584,-22.2446462638181,-36.5204955072696));
#72589=CARTESIAN_POINT('Ctrl Pts',(34.629782529101,-22.2632399142707,-36.237510239401));
#72590=CARTESIAN_POINT('Ctrl Pts',(34.4,-22.2808358845789,-35.9562839053824));
#72591=CARTESIAN_POINT('',(35.4377160618333,-21.8115085669485,-36.7705676731535));
#72592=CARTESIAN_POINT('Origin',(33.1,-25.6899024992348,-28.0490892825384));
#72593=CARTESIAN_POINT('',(33.3226453080309,-28.872052684018,-30.9143101784803));
#72594=CARTESIAN_POINT('',(33.0964948753266,-25.6398056289004,-28.0039818578826));
#72595=CARTESIAN_POINT('',(34.4,-28.1860830985704,-31.5410006112756));
#72596=CARTESIAN_POINT('Origin',(26.8550245390365,0.,0.));
#72597=CARTESIAN_POINT('',(34.8617922858584,-28.2484175959528,-32.1029248328491));
#72598=CARTESIAN_POINT('Ctrl Pts',(34.8617922858584,-28.2484175959528,-32.1029248328491));
#72599=CARTESIAN_POINT('Ctrl Pts',(34.6297825291016,-28.2175888910034,-31.8210099935474));
#72600=CARTESIAN_POINT('Ctrl Pts',(34.4,-28.1860830985703,-31.5410006112756));
#72601=CARTESIAN_POINT('',(35.4377160618333,-27.8652848098447,-32.4244114123644));
#72602=CARTESIAN_POINT('Origin',(33.1,-30.170288394504,-23.1619558369422));
#72603=CARTESIAN_POINT('',(33.3226453080309,-33.8016349549212,-25.4310730087083));
#72604=CARTESIAN_POINT('',(33.0964948753266,-30.1131197861062,-23.1262329256631));
#72605=CARTESIAN_POINT('',(34.4,-33.234910440458,-26.1673599741116));
#72606=CARTESIAN_POINT('Origin',(26.8550245390365,0.,0.));
#72607=CARTESIAN_POINT('',(34.8617922858584,-33.3938750538235,-26.7099230322464));
#72608=CARTESIAN_POINT('Ctrl Pts',(34.8617922858584,-33.3938750538235,-26.7099230322464));
#72609=CARTESIAN_POINT('Ctrl Pts',(34.6297825291001,-33.3145607080714,-26.4376444612452));
#72610=CARTESIAN_POINT('Ctrl Pts',(34.4,-33.234910440458,-26.1673599741116));
#72611=CARTESIAN_POINT('',(35.4377160618333,-33.0723884743082,-27.0930558183544));
#72612=CARTESIAN_POINT('Origin',(33.1,-33.7339653438087,-17.5710580837557));
#72613=CARTESIAN_POINT('',(33.3226453080309,-37.7041716521717,-19.1751255543105));
#72614=CARTESIAN_POINT('',(33.0964948753266,-33.6714620365851,-17.5458051084359));
#72615=CARTESIAN_POINT('',(34.4,-37.2739118462885,-19.9986373454573));
#72616=CARTESIAN_POINT('Origin',(26.8550245390365,0.,0.));
#72617=CARTESIAN_POINT('',(34.8617922858584,-37.5246765162999,-20.5053537361819));
#72618=CARTESIAN_POINT('Ctrl Pts',(34.8617922858584,-37.5246765162999,-20.5053537361819));
#72619=CARTESIAN_POINT('Ctrl Pts',(34.6297825291016,-37.3992864560069,-20.2509844800853));
#72620=CARTESIAN_POINT('Ctrl Pts',(34.4,-37.2739118462884,-19.9986373454572));
#72621=CARTESIAN_POINT('',(35.4377160618333,-37.274604350416,-20.9384914330515));
#72622=CARTESIAN_POINT('Origin',(33.1,-36.2726528263519,-11.4462726220787));
#72623=CARTESIAN_POINT('',(33.3226453080309,-40.4610861730024,-12.3365516130268));
#72624=CARTESIAN_POINT('',(33.0964948753266,-36.2067139516643,-11.4322568815947));
#72625=CARTESIAN_POINT('',(34.4,-40.1803643021789,-13.22226624086));
#72626=CARTESIAN_POINT('Origin',(26.8550245390365,0.,0.));
#72627=CARTESIAN_POINT('',(34.8617922858584,-40.515309671231,-13.6777396430533));
#72628=CARTESIAN_POINT('Ctrl Pts',(34.8617922858584,-40.515309671231,-13.6777396430533));
#72629=CARTESIAN_POINT('Ctrl Pts',(34.6297825291007,-40.3476538099275,-13.4490085829879));
#72630=CARTESIAN_POINT('Ctrl Pts',(34.4,-40.1803643021789,-13.22226624086));
#72631=CARTESIAN_POINT('',(35.4377160618333,-40.3442502351963,-14.1477215809433));
#72632=CARTESIAN_POINT('Origin',(33.1,-37.7092141076143,-4.9736979588732));
#72633=CARTESIAN_POINT('',(33.3226453080309,-41.9886110647639,-5.12313779357751));
#72634=CARTESIAN_POINT('',(33.0964948753266,-37.6418431848034,-4.97134531440727));
#72635=CARTESIAN_POINT('',(34.4,-41.8659567209931,-6.04414326732375));
#72636=CARTESIAN_POINT('Origin',(26.8550245390365,0.,0.));
#72637=CARTESIAN_POINT('',(34.8617922858584,-42.2749056435377,-6.43453435214069));
#72638=CARTESIAN_POINT('Ctrl Pts',(34.8617922858584,-42.2749056435377,-6.43453435214069));
#72639=CARTESIAN_POINT('Ctrl Pts',(34.6297825291043,-42.0700781197351,-6.23839136562716));
#72640=CARTESIAN_POINT('Ctrl Pts',(34.4,-41.8659567209931,-6.04414326732375));
#72641=CARTESIAN_POINT('',(35.4377160618333,-42.1880564917558,-6.92708036769059));
#72642=CARTESIAN_POINT('Origin',(33.1,-38.,1.65));
#72643=CARTESIAN_POINT('',(33.3226453080309,-42.240333256585,2.24593997529678));
#72644=CARTESIAN_POINT('',(33.0964948753266,-37.933244060464,1.64061806453627));
#72645=CARTESIAN_POINT('',(34.4,-42.2794732300362,1.31762794090605));
#72646=CARTESIAN_POINT('Origin',(26.8550245390365,0.,0.));
#72647=CARTESIAN_POINT('',(34.8617922858584,-42.75,1.00418100903022));
#72648=CARTESIAN_POINT('Ctrl Pts',(34.8617922858584,-42.75,1.00418100903022));
#72649=CARTESIAN_POINT('Ctrl Pts',(34.629782529102,-42.5142243943562,1.16177621660493));
#72650=CARTESIAN_POINT('Ctrl Pts',(34.4,-42.2794732300361,1.31762794090605));
#72651=CARTESIAN_POINT('',(35.4377160618333,-42.75,0.50403667726255));
#72652=CARTESIAN_POINT('Origin',(33.1,-37.1361751213135,8.22356354381351));
#72653=CARTESIAN_POINT('',(33.3226453080309,-41.2086042970448,9.54677599452215));
#72654=CARTESIAN_POINT('',(33.0964948753266,-37.072062510495,8.20273209378169));
#72655=CARTESIAN_POINT('',(34.4,-41.4083493394303,8.63936369090334));
#72656=CARTESIAN_POINT('Origin',(26.8550245390365,0.,0.));
#72657=CARTESIAN_POINT('',(34.8617922858584,-41.926157239006,8.41238483838188));
#72658=CARTESIAN_POINT('Ctrl Pts',(34.8617922858584,-41.926157239006,8.41238483838188));
#72659=CARTESIAN_POINT('Ctrl Pts',(34.6297825290997,-41.66659747399,8.52664381638178));
#72660=CARTESIAN_POINT('Ctrl Pts',(34.4,-41.4083493394303,8.63936369090334));
#72661=CARTESIAN_POINT('',(35.4377160618333,-42.013006390788,7.91983882283195));
#72662=CARTESIAN_POINT('Origin',(33.1,-35.1439863533772,14.5472582706722));
#72663=CARTESIAN_POINT('',(33.3226453080309,-38.9247727484987,16.5575380560557));
#72664=CARTESIAN_POINT('',(33.0964948753266,-35.0844651005135,14.5156102591403));
#72665=CARTESIAN_POINT('',(34.4,-39.2790537077817,15.6985967468815));
#72666=CARTESIAN_POINT('Origin',(26.8550245390365,0.,0.));
#72667=CARTESIAN_POINT('',(34.8617922858584,-39.8284094059642,15.5649826112914));
#72668=CARTESIAN_POINT('Ctrl Pts',(34.8617922858584,-39.8284094059642,15.5649826112914));
#72669=CARTESIAN_POINT('Ctrl Pts',(34.6297825291024,-39.5529520736977,15.6324336584855));
#72670=CARTESIAN_POINT('Ctrl Pts',(34.4,-39.2790537077817,15.6985967468815));
#72671=CARTESIAN_POINT('',(35.4377160618333,-39.9994688419988,15.0950006734014));
#72672=CARTESIAN_POINT('Origin',(33.1,-32.0839653438087,20.4289419162443));
#72673=CARTESIAN_POINT('',(33.3226453080309,-35.4582316768749,23.0652077022745));
#72674=CARTESIAN_POINT('',(33.0964948753266,-32.0308439720488,20.387438952028));
#72675=CARTESIAN_POINT('',(34.4,-35.9562839053824,22.2808358845789));
#72676=CARTESIAN_POINT('Origin',(26.8550245390365,0.,0.));
#72677=CARTESIAN_POINT('',(34.8617922858584,-36.5204955072696,22.2446462638181));
#72678=CARTESIAN_POINT('Ctrl Pts',(34.8617922858584,-36.5204955072696,22.2446462638181));
#72679=CARTESIAN_POINT('Ctrl Pts',(34.6297825291014,-36.2375102394014,22.2632399142706));
#72680=CARTESIAN_POINT('Ctrl Pts',(34.4,-35.9562839053824,22.2808358845789));
#72681=CARTESIAN_POINT('',(35.4377160618333,-36.7705676731535,21.8115085669485));
#72682=CARTESIAN_POINT('Origin',(33.1,-28.0490892825384,25.6899024992348));
#72683=CARTESIAN_POINT('',(33.3226453080309,-30.9143101784803,28.872052684018));
#72684=CARTESIAN_POINT('',(33.0964948753266,-28.0039818578826,25.6398056289004));
#72685=CARTESIAN_POINT('',(34.4,-31.5410006112756,28.1860830985704));
#72686=CARTESIAN_POINT('Origin',(26.8550245390365,0.,0.));
#72687=CARTESIAN_POINT('',(34.8617922858584,-32.1029248328491,28.2484175959528));
#72688=CARTESIAN_POINT('Ctrl Pts',(34.8617922858584,-32.1029248328491,28.2484175959528));
#72689=CARTESIAN_POINT('Ctrl Pts',(34.6297825291016,-31.8210099935474,28.2175888910034));
#72690=CARTESIAN_POINT('Ctrl Pts',(34.4,-31.5410006112756,28.1860830985703));
#72691=CARTESIAN_POINT('',(35.4377160618333,-32.4244114123644,27.8652848098447));
#72692=CARTESIAN_POINT('Origin',(33.1,-23.1619558369422,30.170288394504));
#72693=CARTESIAN_POINT('',(33.3226453080309,-25.4310730087083,33.8016349549212));
#72694=CARTESIAN_POINT('',(33.0964948753266,-23.1262329256631,30.1131197861062));
#72695=CARTESIAN_POINT('',(34.4,-26.1673599741116,33.234910440458));
#72696=CARTESIAN_POINT('Origin',(26.8550245390365,0.,0.));
#72697=CARTESIAN_POINT('',(34.8617922858584,-26.7099230322463,33.3938750538235));
#72698=CARTESIAN_POINT('Ctrl Pts',(34.8617922858584,-26.7099230322463,33.3938750538235));
#72699=CARTESIAN_POINT('Ctrl Pts',(34.6297825290984,-26.4376444612432,33.3145607080708));
#72700=CARTESIAN_POINT('Ctrl Pts',(34.4,-26.1673599741116,33.234910440458));
#72701=CARTESIAN_POINT('',(35.4377160618333,-27.0930558183544,33.0723884743082));
#72702=CARTESIAN_POINT('Origin',(33.1,-17.5710580837557,33.7339653438087));
#72703=CARTESIAN_POINT('',(33.3226453080309,-19.1751255543105,37.7041716521717));
#72704=CARTESIAN_POINT('',(33.0964948753266,-17.5458051084359,33.6714620365851));
#72705=CARTESIAN_POINT('',(34.4,-19.9986373454573,37.2739118462884));
#72706=CARTESIAN_POINT('Origin',(26.8550245390365,0.,0.));
#72707=CARTESIAN_POINT('',(34.8617922858584,-20.5053537361819,37.5246765162999));
#72708=CARTESIAN_POINT('Ctrl Pts',(34.8617922858584,-20.5053537361819,37.5246765162999));
#72709=CARTESIAN_POINT('Ctrl Pts',(34.6297825291036,-20.2509844800875,37.3992864560079));
#72710=CARTESIAN_POINT('Ctrl Pts',(34.4,-19.9986373454573,37.2739118462884));
#72711=CARTESIAN_POINT('',(35.4377160618333,-20.9384914330515,37.274604350416));
#72712=CARTESIAN_POINT('Origin',(33.1,-11.4462726220787,36.2726528263519));
#72713=CARTESIAN_POINT('',(33.3226453080309,-12.3365516130268,40.4610861730024));
#72714=CARTESIAN_POINT('',(33.0964948753266,-11.4322568815947,36.2067139516643));
#72715=CARTESIAN_POINT('',(34.4,-13.22226624086,40.1803643021789));
#72716=CARTESIAN_POINT('Origin',(26.8550245390365,0.,0.));
#72717=CARTESIAN_POINT('',(34.8617922858584,-13.6777396430533,40.515309671231));
#72718=CARTESIAN_POINT('Ctrl Pts',(34.8617922858584,-13.6777396430533,40.515309671231));
#72719=CARTESIAN_POINT('Ctrl Pts',(34.6297825290975,-13.4490085829847,40.3476538099251));
#72720=CARTESIAN_POINT('Ctrl Pts',(34.4,-13.22226624086,40.1803643021789));
#72721=CARTESIAN_POINT('',(35.4377160618333,-14.1477215809433,40.3442502351963));
#72722=CARTESIAN_POINT('Origin',(33.1,-4.97369795887321,37.7092141076143));
#72723=CARTESIAN_POINT('',(33.3226453080309,-5.12313779357752,41.9886110647639));
#72724=CARTESIAN_POINT('',(33.0964948753266,-4.97134531440728,37.6418431848034));
#72725=CARTESIAN_POINT('',(34.4,-6.04414326732376,41.8659567209931));
#72726=CARTESIAN_POINT('Origin',(26.8550245390365,0.,0.));
#72727=CARTESIAN_POINT('',(34.8617922858584,-6.4345343521407,42.2749056435377));
#72728=CARTESIAN_POINT('Ctrl Pts',(34.8617922858584,-6.4345343521407,42.2749056435377));
#72729=CARTESIAN_POINT('Ctrl Pts',(34.629782529103,-6.23839136562604,42.0700781197339));
#72730=CARTESIAN_POINT('Ctrl Pts',(34.4,-6.04414326732376,41.8659567209931));
#72731=CARTESIAN_POINT('',(35.4377160618333,-6.9270803676906,42.1880564917558));
#72732=CARTESIAN_POINT('Origin',(33.1,1.65,38.));
#72733=CARTESIAN_POINT('',(33.3226453080309,2.24593997529677,42.240333256585));
#72734=CARTESIAN_POINT('',(33.0964948753266,1.64061806453627,37.933244060464));
#72735=CARTESIAN_POINT('',(34.4,1.31762794090604,42.2794732300362));
#72736=CARTESIAN_POINT('Origin',(26.8550245390365,0.,0.));
#72737=CARTESIAN_POINT('',(34.8617922858584,1.00418100903021,42.75));
#72738=CARTESIAN_POINT('Ctrl Pts',(34.8617922858584,1.00418100903021,42.75));
#72739=CARTESIAN_POINT('Ctrl Pts',(34.629782529099,1.16177621660694,42.5142243943532));
#72740=CARTESIAN_POINT('Ctrl Pts',(34.4,1.31762794090604,42.2794732300361));
#72741=CARTESIAN_POINT('',(35.4377160618333,0.504036677262548,42.75));
#72742=CARTESIAN_POINT('Origin',(33.1,8.2235635438135,37.1361751213135));
#72743=CARTESIAN_POINT('',(33.3226453080309,9.54677599452214,41.2086042970448));
#72744=CARTESIAN_POINT('',(33.0964948753266,8.20273209378168,37.0720625104951));
#72745=CARTESIAN_POINT('',(34.4,8.63936369090333,41.4083493394303));
#72746=CARTESIAN_POINT('Origin',(26.8550245390365,0.,0.));
#72747=CARTESIAN_POINT('',(34.8617922858584,8.41238483838185,41.9261572390061));
#72748=CARTESIAN_POINT('Ctrl Pts',(34.8617922858584,8.41238483838185,41.9261572390061));
#72749=CARTESIAN_POINT('Ctrl Pts',(34.6297825291019,8.52664381638067,41.6665974739925));
#72750=CARTESIAN_POINT('Ctrl Pts',(34.4,8.63936369090333,41.4083493394303));
#72751=CARTESIAN_POINT('',(35.4377160618333,7.91983882283194,42.013006390788));
#72752=CARTESIAN_POINT('Origin',(33.1,14.5472582706722,35.1439863533772));
#72753=CARTESIAN_POINT('',(33.3226453080309,16.5575380560557,38.9247727484987));
#72754=CARTESIAN_POINT('',(33.0964948753266,14.5156102591403,35.0844651005135));
#72755=CARTESIAN_POINT('',(34.4,15.6985967468815,39.2790537077817));
#72756=CARTESIAN_POINT('Origin',(26.8550245390365,0.,0.));
#72757=CARTESIAN_POINT('',(34.8617922858584,15.5649826112914,39.8284094059642));
#72758=CARTESIAN_POINT('Ctrl Pts',(34.8617922858584,15.5649826112914,39.8284094059641));
#72759=CARTESIAN_POINT('Ctrl Pts',(34.6297825291034,15.6324336584852,39.5529520736989));
#72760=CARTESIAN_POINT('Ctrl Pts',(34.4,15.6985967468815,39.2790537077817));
#72761=CARTESIAN_POINT('',(35.4377160618333,15.0950006734014,39.9994688419988));
#72762=CARTESIAN_POINT('Origin',(33.1,20.4289419162443,32.0839653438087));
#72763=CARTESIAN_POINT('',(33.3226453080309,23.0652077022745,35.4582316768749));
#72764=CARTESIAN_POINT('',(33.0964948753266,20.3874389520281,32.0308439720488));
#72765=CARTESIAN_POINT('',(34.4,22.2808358845789,35.9562839053824));
#72766=CARTESIAN_POINT('Origin',(26.8550245390365,0.,0.));
#72767=CARTESIAN_POINT('',(34.8617922858584,22.2446462638181,36.5204955072696));
#72768=CARTESIAN_POINT('Ctrl Pts',(34.8617922858584,22.2446462638181,36.5204955072696));
#72769=CARTESIAN_POINT('Ctrl Pts',(34.6297825291015,22.2632399142706,36.2375102394016));
#72770=CARTESIAN_POINT('Ctrl Pts',(34.4,22.2808358845789,35.9562839053824));
#72771=CARTESIAN_POINT('',(35.4377160618333,21.8115085669485,36.7705676731535));
#72772=CARTESIAN_POINT('Origin',(33.1,25.6899024992348,28.0490892825384));
#72773=CARTESIAN_POINT('',(33.3226453080309,28.872052684018,30.9143101784803));
#72774=CARTESIAN_POINT('',(33.0964948753266,25.6398056289004,28.0039818578826));
#72775=CARTESIAN_POINT('',(34.4,28.1860830985703,31.5410006112756));
#72776=CARTESIAN_POINT('Origin',(26.8550245390365,0.,0.));
#72777=CARTESIAN_POINT('',(34.8617922858584,28.2484175959528,32.1029248328492));
#72778=CARTESIAN_POINT('Ctrl Pts',(34.8617922858584,28.2484175959528,32.1029248328492));
#72779=CARTESIAN_POINT('Ctrl Pts',(34.6297825291063,28.217588891004,31.821009993553));
#72780=CARTESIAN_POINT('Ctrl Pts',(34.4,28.1860830985703,31.5410006112756));
#72781=CARTESIAN_POINT('',(35.4377160618333,27.8652848098447,32.4244114123644));
#72782=CARTESIAN_POINT('Origin',(33.1,30.170288394504,23.1619558369422));
#72783=CARTESIAN_POINT('',(33.3226453080309,33.8016349549212,25.4310730087083));
#72784=CARTESIAN_POINT('',(33.0964948753266,30.1131197861062,23.1262329256631));
#72785=CARTESIAN_POINT('',(34.4,33.234910440458,26.1673599741116));
#72786=CARTESIAN_POINT('Origin',(26.8550245390365,0.,0.));
#72787=CARTESIAN_POINT('',(34.8617922858584,33.3938750538235,26.7099230322464));
#72788=CARTESIAN_POINT('Ctrl Pts',(34.8617922858584,33.3938750538235,26.7099230322464));
#72789=CARTESIAN_POINT('Ctrl Pts',(34.6297825291001,33.3145607080714,26.4376444612452));
#72790=CARTESIAN_POINT('Ctrl Pts',(34.4,33.234910440458,26.1673599741116));
#72791=CARTESIAN_POINT('',(35.4377160618333,33.0723884743082,27.0930558183544));
#72792=CARTESIAN_POINT('Origin',(33.1,33.7339653438087,17.5710580837557));
#72793=CARTESIAN_POINT('',(33.3226453080309,37.7041716521717,19.1751255543105));
#72794=CARTESIAN_POINT('',(33.0964948753266,33.6714620365851,17.5458051084359));
#72795=CARTESIAN_POINT('',(34.4,37.2739118462884,19.9986373454573));
#72796=CARTESIAN_POINT('Origin',(26.8550245390365,0.,0.));
#72797=CARTESIAN_POINT('',(34.8617922858584,37.5246765162999,20.5053537361819));
#72798=CARTESIAN_POINT('Ctrl Pts',(34.8617922858584,37.5246765162999,20.5053537361819));
#72799=CARTESIAN_POINT('Ctrl Pts',(34.6297825291027,37.3992864560074,20.2509844800865));
#72800=CARTESIAN_POINT('Ctrl Pts',(34.4,37.2739118462884,19.9986373454573));
#72801=CARTESIAN_POINT('',(35.4377160618333,37.274604350416,20.9384914330515));
#72802=CARTESIAN_POINT('Origin',(33.1,36.2726528263519,11.4462726220787));
#72803=CARTESIAN_POINT('',(33.3226453080309,40.4610861730024,12.3365516130268));
#72804=CARTESIAN_POINT('',(33.0964948753266,36.2067139516643,11.4322568815947));
#72805=CARTESIAN_POINT('',(34.4,40.1803643021789,13.22226624086));
#72806=CARTESIAN_POINT('Origin',(26.8550245390365,0.,0.));
#72807=CARTESIAN_POINT('',(34.8617922858584,40.515309671231,13.6777396430533));
#72808=CARTESIAN_POINT('Ctrl Pts',(34.8617922858584,40.515309671231,13.6777396430533));
#72809=CARTESIAN_POINT('Ctrl Pts',(34.6297825290994,40.3476538099265,13.4490085829866));
#72810=CARTESIAN_POINT('Ctrl Pts',(34.4,40.1803643021789,13.22226624086));
#72811=CARTESIAN_POINT('',(35.4377160618333,40.3442502351963,14.1477215809433));
#72812=CARTESIAN_POINT('Origin',(33.1,37.7092141076143,4.97369795887321));
#72813=CARTESIAN_POINT('',(33.3226453080309,41.9886110647639,5.12313779357752));
#72814=CARTESIAN_POINT('',(33.0964948753266,37.6418431848034,4.97134531440728));
#72815=CARTESIAN_POINT('',(34.4,41.8659567209931,6.04414326732376));
#72816=CARTESIAN_POINT('Origin',(26.8550245390365,0.,0.));
#72817=CARTESIAN_POINT('',(34.8617922858584,42.2749056435377,6.4345343521407));
#72818=CARTESIAN_POINT('Ctrl Pts',(34.8617922858584,42.2749056435377,6.4345343521407));
#72819=CARTESIAN_POINT('Ctrl Pts',(34.629782529104,42.0700781197348,6.23839136562689));
#72820=CARTESIAN_POINT('Ctrl Pts',(34.4,41.8659567209931,6.04414326732376));
#72821=CARTESIAN_POINT('',(35.4377160618333,42.1880564917558,6.9270803676906));
#72822=CARTESIAN_POINT('Origin',(17.5,42.75,0.));
#72823=CARTESIAN_POINT('',(34.8617922858584,42.75,-1.00418100903021));
#72824=CARTESIAN_POINT('',(35.4377160618333,42.75,-0.504036677262545));
#72825=CARTESIAN_POINT('Ctrl Pts',(34.8617922858584,42.75,1.00418100903022));
#72826=CARTESIAN_POINT('Ctrl Pts',(34.8382109660634,42.75,1.80411241501588E-15));
#72827=CARTESIAN_POINT('Ctrl Pts',(34.8617922858584,42.75,-1.00418100903021));
#72828=CARTESIAN_POINT('Origin',(0.,37.,0.));
#72829=CARTESIAN_POINT('',(0.,42.75,0.884158520433536));
#72830=CARTESIAN_POINT('',(0.,37.6651655808655,-0.062325622023615));
#72831=CARTESIAN_POINT('',(0.,42.75,0.));
#72832=CARTESIAN_POINT('Origin',(0.,37.,0.));
#72833=CARTESIAN_POINT('',(0.,41.9469989254299,8.29418576107602));
#72834=CARTESIAN_POINT('',(0.,36.2945488399958,6.17584017667492));
#72835=CARTESIAN_POINT('',(0.,42.6583746990022,4.25977326949884));
#72836=CARTESIAN_POINT('Origin',(0.,37.,0.));
#72837=CARTESIAN_POINT('',(0.,39.8694595147163,15.4521983644287));
#72838=CARTESIAN_POINT('',(0.,33.4731411603662,11.6778166023976));
#72839=CARTESIAN_POINT('',(0.,42.335948439747,8.67557573757185));
#72840=CARTESIAN_POINT('Origin',(0.,37.,0.));
#72841=CARTESIAN_POINT('',(0.,36.580506751568,22.1407037396679));
#72842=CARTESIAN_POINT('',(0.,29.5122178964835,16.0943600450819));
#72843=CARTESIAN_POINT('',(0.,41.6475860117848,13.3642650149939));
#72844=CARTESIAN_POINT('Origin',(0.,37.,0.));
#72845=CARTESIAN_POINT('',(0.,32.1800738014028,28.156475035514));
#72846=CARTESIAN_POINT('',(0.,24.8063469907288,19.1973293864723));
#72847=CARTESIAN_POINT('',(0.,40.3921542999172,18.3696985987366));
#72848=CARTESIAN_POINT('Origin',(0.,37.,0.));
#72849=CARTESIAN_POINT('',(0.,26.8018655926851,33.3167260852698));
#72850=CARTESIAN_POINT('',(0.,19.7883255734973,20.897949308743));
#72851=CARTESIAN_POINT('',(0.,38.3354159575187,23.6389282279734));
#72852=CARTESIAN_POINT('Origin',(0.,37.,0.));
#72853=CARTESIAN_POINT('',(0.,20.6092962603321,37.4646652720015));
#72854=CARTESIAN_POINT('',(0.,14.8810740823533,21.2488434819817));
#72855=CARTESIAN_POINT('',(0.,35.25,29.0118510267787));
#72856=CARTESIAN_POINT('Origin',(0.,37.,0.));
#72857=CARTESIAN_POINT('',(0.,13.790523889916,40.4742595624789));
#72858=CARTESIAN_POINT('',(0.,10.4521657293574,20.4298559661641));
#72859=CARTESIAN_POINT('',(0.,30.9572722260229,34.2260741489971));
#72860=CARTESIAN_POINT('Origin',(0.,37.,0.));
#72861=CARTESIAN_POINT('',(0.,6.55273342944653,42.2540639571139));
#72862=CARTESIAN_POINT('',(0.,6.77630740640388,18.7196089291248));
#72863=CARTESIAN_POINT('',(0.,25.3656163375309,38.9368451155095));
#72864=CARTESIAN_POINT('Origin',(0.,37.,0.));
#72865=CARTESIAN_POINT('',(0.,-0.884158520433534,42.75));
#72866=CARTESIAN_POINT('',(0.,4.01009029474227,16.4564323480298));
#72867=CARTESIAN_POINT('',(0.,18.5,42.75));
#72868=CARTESIAN_POINT('Origin',(0.,37.,0.));
#72869=CARTESIAN_POINT('',(0.,-8.29418576107602,41.9469989254299));
#72870=CARTESIAN_POINT('',(0.,2.18181606689636,13.9935441805696));
#72871=CARTESIAN_POINT('',(0.,10.5186971470084,45.2642177670343));
#72872=CARTESIAN_POINT('Origin',(0.,37.,0.));
#72873=CARTESIAN_POINT('',(0.,-15.4521983644287,39.8694595147163));
#72874=CARTESIAN_POINT('',(0.,1.19736103864281,11.6540088485914));
#72875=CARTESIAN_POINT('',(0.,1.71454997167821,46.1176449281981));
#72876=CARTESIAN_POINT('Origin',(0.,37.,0.));
#72877=CARTESIAN_POINT('',(0.,-22.1407037396679,36.580506751568));
#72878=CARTESIAN_POINT('',(0.,0.861089067994371,9.69098078979665));
#72879=CARTESIAN_POINT('',(0.,-7.49999999999998,45.0333209967908));
#72880=CARTESIAN_POINT('Origin',(0.,37.,0.));
#72881=CARTESIAN_POINT('',(0.,-28.156475035514,32.1800738014028));
#72882=CARTESIAN_POINT('',(0.,0.909000315285454,8.25805229904004));
#72883=CARTESIAN_POINT('',(0.,-16.6229246706804,41.8578716586992));
#72884=CARTESIAN_POINT('Origin',(0.,37.,0.));
#72885=CARTESIAN_POINT('',(0.,-33.3167260852698,26.8018655926852));
#72886=CARTESIAN_POINT('',(0.,1.04982739730203,7.39325534798233));
#72887=CARTESIAN_POINT('',(0.,-25.1046455867554,36.5886420294625));
#72888=CARTESIAN_POINT('Origin',(0.,37.,0.));
#72889=CARTESIAN_POINT('',(0.,-37.4646652720015,20.6092962603321));
#72890=CARTESIAN_POINT('',(0.,1.00884095837589,7.01857020850226));
#72891=CARTESIAN_POINT('',(0.,-32.3975860117848,29.3857349850061));
#72892=CARTESIAN_POINT('Origin',(0.,37.,0.));
#72893=CARTESIAN_POINT('',(0.,-40.4742595624789,13.790523889916));
#72894=CARTESIAN_POINT('',(0.,0.568817492022398,6.95487569709476));
#72895=CARTESIAN_POINT('',(0.,-38.0077706374481,20.5671465167728));
#72896=CARTESIAN_POINT('Origin',(0.,37.,0.));
#72897=CARTESIAN_POINT('',(0.,-42.2540639571139,6.55273342944654));
#72898=CARTESIAN_POINT('',(0.,-0.39700986412022,6.95036949266363));
#72899=CARTESIAN_POINT('',(0.,-41.5426881835415,10.5871459210237));
#72900=CARTESIAN_POINT('Origin',(0.,37.,0.));
#72901=CARTESIAN_POINT('',(0.,-42.75,-0.884158520433531));
#72902=CARTESIAN_POINT('',(0.,-1.90419702074843,6.718823527578));
#72903=CARTESIAN_POINT('',(0.,-42.75,7.50096164477754E-15));
#72904=CARTESIAN_POINT('Origin',(0.,37.,0.));
#72905=CARTESIAN_POINT('',(0.,-41.9469989254299,-8.29418576107601));
#72906=CARTESIAN_POINT('',(0.,-3.85120042414092,5.98282072632249));
#72907=CARTESIAN_POINT('',(0.,-41.5426881835416,-10.5871459210237));
#72908=CARTESIAN_POINT('Origin',(0.,37.,0.));
#72909=CARTESIAN_POINT('',(0.,-39.8694595147163,-15.4521983644287));
#72910=CARTESIAN_POINT('',(0.,-6.02918648963184,4.51649335041757));
#72911=CARTESIAN_POINT('',(0.,-38.0077706374481,-20.5671465167728));
#72912=CARTESIAN_POINT('Origin',(0.,37.,0.));
#72913=CARTESIAN_POINT('',(0.,-36.580506751568,-22.1407037396679));
#72914=CARTESIAN_POINT('',(0.,-8.14642990287292,2.18232617468118));
#72915=CARTESIAN_POINT('',(0.,-32.3975860117848,-29.385734985006));
#72916=CARTESIAN_POINT('Origin',(0.,37.,0.));
#72917=CARTESIAN_POINT('',(0.,-32.1800738014028,-28.156475035514));
#72918=CARTESIAN_POINT('',(0.,-9.86438200079779,-1.04270499302577));
#72919=CARTESIAN_POINT('',(0.,-25.1046455867554,-36.5886420294625));
#72920=CARTESIAN_POINT('Origin',(0.,37.,0.));
#72921=CARTESIAN_POINT('',(0.,-26.8018655926852,-33.3167260852698));
#72922=CARTESIAN_POINT('',(0.,-10.8410320540273,-5.05510237718296));
#72923=CARTESIAN_POINT('',(0.,-16.6229246706805,-41.8578716586992));
#72924=CARTESIAN_POINT('Origin',(0.,37.,0.));
#72925=CARTESIAN_POINT('',(0.,-20.6092962603321,-37.4646652720015));
#72926=CARTESIAN_POINT('',(0.,-10.7762546488599,-9.62865516777302));
#72927=CARTESIAN_POINT('',(0.,-7.50000000000002,-45.0333209967908));
#72928=CARTESIAN_POINT('Origin',(0.,37.,0.));
#72929=CARTESIAN_POINT('',(0.,-13.790523889916,-40.4742595624789));
#72930=CARTESIAN_POINT('',(0.,-9.45354915528123,-14.4338924757149));
#72931=CARTESIAN_POINT('',(0.,1.71454997167818,-46.1176449281981));
#72932=CARTESIAN_POINT('Origin',(0.,37.,0.));
#72933=CARTESIAN_POINT('',(0.,-6.55273342944652,-42.2540639571139));
#72934=CARTESIAN_POINT('',(0.,-6.77296855766818,-19.07107195038));
#72935=CARTESIAN_POINT('',(0.,10.5186971470084,-45.2642177670343));
#72936=CARTESIAN_POINT('Origin',(0.,37.,0.));
#72937=CARTESIAN_POINT('',(0.,0.884158520433529,-42.75));
#72938=CARTESIAN_POINT('',(0.,-2.77105885485935,-23.1129302535842));
#72939=CARTESIAN_POINT('',(0.,18.5,-42.75));
#72940=CARTESIAN_POINT('Origin',(0.,37.,0.));
#72941=CARTESIAN_POINT('',(0.,8.294185761076,-41.9469989254299));
#72942=CARTESIAN_POINT('',(0.,2.37483551724878,-26.1522050835671));
#72943=CARTESIAN_POINT('',(0.,25.3656163375309,-38.9368451155095));
#72944=CARTESIAN_POINT('Origin',(0.,37.,0.));
#72945=CARTESIAN_POINT('',(0.,15.4521983644287,-39.8694595147163));
#72946=CARTESIAN_POINT('',(0.,8.35868429062286,-27.8483188014066));
#72947=CARTESIAN_POINT('',(0.,30.9572722260229,-34.2260741489971));
#72948=CARTESIAN_POINT('Origin',(0.,37.,0.));
#72949=CARTESIAN_POINT('',(0.,22.1407037396679,-36.580506751568));
#72950=CARTESIAN_POINT('',(0.,14.7731229383951,-27.9676670095597));
#72951=CARTESIAN_POINT('',(0.,35.25,-29.0118510267787));
#72952=CARTESIAN_POINT('Origin',(0.,37.,0.));
#72953=CARTESIAN_POINT('',(0.,28.156475035514,-32.1800738014028));
#72954=CARTESIAN_POINT('',(0.,21.1490346947835,-26.4126766924866));
#72955=CARTESIAN_POINT('',(0.,38.3354159575187,-23.6389282279734));
#72956=CARTESIAN_POINT('Origin',(0.,37.,0.));
#72957=CARTESIAN_POINT('',(0.,33.3167260852698,-26.8018655926852));
#72958=CARTESIAN_POINT('',(0.,27.002879083228,-23.2361022795424));
#72959=CARTESIAN_POINT('',(0.,40.3921542999172,-18.3696985987366));
#72960=CARTESIAN_POINT('Origin',(0.,37.,0.));
#72961=CARTESIAN_POINT('',(0.,37.4646652720015,-20.6092962603321));
#72962=CARTESIAN_POINT('',(0.,31.8863396081306,-18.638758522711));
#72963=CARTESIAN_POINT('',(0.,41.6475860117848,-13.364265014994));
#72964=CARTESIAN_POINT('Origin',(0.,37.,0.));
#72965=CARTESIAN_POINT('',(0.,40.4742595624789,-13.790523889916));
#72966=CARTESIAN_POINT('',(0.,35.4325659339014,-12.9508391875439));
#72967=CARTESIAN_POINT('',(0.,42.335948439747,-8.67557573757187));
#72968=CARTESIAN_POINT('Origin',(0.,37.,0.));
#72969=CARTESIAN_POINT('',(0.,42.2540639571139,-6.55273342944652));
#72970=CARTESIAN_POINT('',(0.,37.3936710153845,-6.59890647140843));
#72971=CARTESIAN_POINT('',(0.,42.6583746990022,-4.25977326949884));
#72972=CARTESIAN_POINT('Origin',(17.5,42.1005314412719,-7.42345959526127));
#72973=CARTESIAN_POINT('',(0.138207714141615,42.2749056435377,-6.43453435214071));
#72974=CARTESIAN_POINT('',(-0.437716061833263,42.1880564917558,-6.92708036769061));
#72975=CARTESIAN_POINT('Ctrl Pts',(0.138207714141624,41.9261572390061,-8.41238483838185));
#72976=CARTESIAN_POINT('Ctrl Pts',(0.16178903393654,42.1005314412719,-7.42345959526128));
#72977=CARTESIAN_POINT('Ctrl Pts',(0.138207714141615,42.2749056435377,-6.43453435214071));
#72978=CARTESIAN_POINT('Origin',(17.5,40.1718595385976,-14.6213611271724));
#72979=CARTESIAN_POINT('',(0.13820771414162,40.515309671231,-13.6777396430533));
#72980=CARTESIAN_POINT('',(-0.437716061833263,40.3442502351963,-14.1477215809433));
#72981=CARTESIAN_POINT('Ctrl Pts',(0.138207714141623,39.8284094059641,-15.5649826112914));
#72982=CARTESIAN_POINT('Ctrl Pts',(0.161789033936545,40.1718595385976,-14.6213611271724));
#72983=CARTESIAN_POINT('Ctrl Pts',(0.13820771414162,40.515309671231,-13.6777396430533));
#72984=CARTESIAN_POINT('Origin',(17.5,37.0225860117847,-21.375));
#72985=CARTESIAN_POINT('',(0.138207714141623,37.5246765162998,-20.505353736182));
#72986=CARTESIAN_POINT('',(-0.437716061833263,37.274604350416,-20.9384914330516));
#72987=CARTESIAN_POINT('Ctrl Pts',(0.138207714141626,36.5204955072696,-22.2446462638181));
#72988=CARTESIAN_POINT('Ctrl Pts',(0.161789033936547,37.0225860117847,-21.375));
#72989=CARTESIAN_POINT('Ctrl Pts',(0.138207714141623,37.5246765162998,-20.505353736182));
#72990=CARTESIAN_POINT('Origin',(17.5,32.7483999433363,-27.4791703140996));
#72991=CARTESIAN_POINT('',(0.138207714141626,33.3938750538235,-26.7099230322464));
#72992=CARTESIAN_POINT('',(-0.437716061833263,33.0723884743082,-27.0930558183544));
#72993=CARTESIAN_POINT('Ctrl Pts',(0.13820771414163,32.1029248328491,-28.2484175959528));
#72994=CARTESIAN_POINT('Ctrl Pts',(0.16178903393655,32.7483999433363,-27.4791703140996));
#72995=CARTESIAN_POINT('Ctrl Pts',(0.138207714141626,33.3938750538235,-26.7099230322464));
#72996=CARTESIAN_POINT('Origin',(17.5,27.4791703140995,-32.7483999433363));
#72997=CARTESIAN_POINT('',(0.138207714141627,28.2484175959528,-32.1029248328492));
#72998=CARTESIAN_POINT('',(-0.437716061833263,27.8652848098447,-32.4244114123644));
#72999=CARTESIAN_POINT('Ctrl Pts',(0.138207714141623,26.7099230322463,-33.3938750538235));
#73000=CARTESIAN_POINT('Ctrl Pts',(0.161789033936551,27.4791703140995,-32.7483999433363));
#73001=CARTESIAN_POINT('Ctrl Pts',(0.138207714141627,28.2484175959528,-32.1029248328492));
#73002=CARTESIAN_POINT('Origin',(17.5,21.375,-37.0225860117847));
#73003=CARTESIAN_POINT('',(0.138207714141627,22.2446462638181,-36.5204955072696));
#73004=CARTESIAN_POINT('',(-0.437716061833263,21.8115085669485,-36.7705676731535));
#73005=CARTESIAN_POINT('Ctrl Pts',(0.138207714141623,20.505353736182,-37.5246765162999));
#73006=CARTESIAN_POINT('Ctrl Pts',(0.16178903393655,21.375,-37.0225860117847));
#73007=CARTESIAN_POINT('Ctrl Pts',(0.138207714141627,22.2446462638181,-36.5204955072696));
#73008=CARTESIAN_POINT('Origin',(17.5,14.6213611271723,-40.1718595385976));
#73009=CARTESIAN_POINT('',(0.138207714141622,15.5649826112913,-39.8284094059642));
#73010=CARTESIAN_POINT('',(-0.437716061833263,15.0950006734014,-39.9994688419989));
#73011=CARTESIAN_POINT('Ctrl Pts',(0.138207714141626,13.6777396430533,-40.515309671231));
#73012=CARTESIAN_POINT('Ctrl Pts',(0.161789033936545,14.6213611271723,-40.1718595385976));
#73013=CARTESIAN_POINT('Ctrl Pts',(0.138207714141622,15.5649826112913,-39.8284094059642));
#73014=CARTESIAN_POINT('Origin',(17.5,7.42345959526125,-42.1005314412719));
#73015=CARTESIAN_POINT('',(0.138207714141623,8.41238483838183,-41.9261572390061));
#73016=CARTESIAN_POINT('',(-0.437716061833263,7.91983882283192,-42.013006390788));
#73017=CARTESIAN_POINT('Ctrl Pts',(0.138207714141623,6.43453435214068,-42.2749056435377));
#73018=CARTESIAN_POINT('Ctrl Pts',(0.161789033936546,7.42345959526126,-42.1005314412719));
#73019=CARTESIAN_POINT('Ctrl Pts',(0.138207714141623,8.41238483838183,-41.9261572390061));
#73020=CARTESIAN_POINT('Origin',(17.5,-7.8530475995324E-15,-42.75));
#73021=CARTESIAN_POINT('',(0.138207714141622,1.0041810090302,-42.75));
#73022=CARTESIAN_POINT('',(-0.437716061833263,0.504036677262537,-42.75));
#73023=CARTESIAN_POINT('Ctrl Pts',(0.138207714141621,-1.00418100903022,
-42.75));
#73024=CARTESIAN_POINT('Ctrl Pts',(0.161789033936545,-7.49400541621981E-15,
-42.75));
#73025=CARTESIAN_POINT('Ctrl Pts',(0.138207714141622,1.0041810090302,-42.75));
#73026=CARTESIAN_POINT('Origin',(17.5,-7.42345959526127,-42.1005314412719));
#73027=CARTESIAN_POINT('',(0.138207714141622,-6.4345343521407,-42.2749056435377));
#73028=CARTESIAN_POINT('',(-0.437716061833263,-6.9270803676906,-42.1880564917558));
#73029=CARTESIAN_POINT('Ctrl Pts',(0.138207714141623,-8.41238483838184,
-41.9261572390061));
#73030=CARTESIAN_POINT('Ctrl Pts',(0.161789033936548,-7.42345959526127,
-42.1005314412719));
#73031=CARTESIAN_POINT('Ctrl Pts',(0.138207714141622,-6.4345343521407,-42.2749056435377));
#73032=CARTESIAN_POINT('Origin',(17.5,-14.6213611271724,-40.1718595385976));
#73033=CARTESIAN_POINT('',(0.138207714141628,-13.6777396430533,-40.515309671231));
#73034=CARTESIAN_POINT('',(-0.437716061833263,-14.1477215809433,-40.3442502351963));
#73035=CARTESIAN_POINT('Ctrl Pts',(0.138207714141625,-15.5649826112914,
-39.8284094059641));
#73036=CARTESIAN_POINT('Ctrl Pts',(0.161789033936553,-14.6213611271724,
-40.1718595385976));
#73037=CARTESIAN_POINT('Ctrl Pts',(0.138207714141628,-13.6777396430533,
-40.515309671231));
#73038=CARTESIAN_POINT('Origin',(17.5,-21.375,-37.0225860117847));
#73039=CARTESIAN_POINT('',(0.138207714141623,-20.505353736182,-37.5246765162998));
#73040=CARTESIAN_POINT('',(-0.437716061833263,-20.9384914330516,-37.274604350416));
#73041=CARTESIAN_POINT('Ctrl Pts',(0.138207714141625,-22.2446462638181,
-36.5204955072696));
#73042=CARTESIAN_POINT('Ctrl Pts',(0.161789033936547,-21.375,-37.0225860117847));
#73043=CARTESIAN_POINT('Ctrl Pts',(0.138207714141623,-20.505353736182,-37.5246765162998));
#73044=CARTESIAN_POINT('Origin',(17.5,-27.4791703140996,-32.7483999433363));
#73045=CARTESIAN_POINT('',(0.138207714141625,-26.7099230322463,-33.3938750538235));
#73046=CARTESIAN_POINT('',(-0.437716061833263,-27.0930558183544,-33.0723884743082));
#73047=CARTESIAN_POINT('Ctrl Pts',(0.138207714141625,-28.2484175959528,
-32.1029248328492));
#73048=CARTESIAN_POINT('Ctrl Pts',(0.161789033936547,-27.4791703140996,
-32.7483999433363));
#73049=CARTESIAN_POINT('Ctrl Pts',(0.138207714141625,-26.7099230322464,
-33.3938750538235));
#73050=CARTESIAN_POINT('Origin',(17.5,-32.7483999433363,-27.4791703140996));
#73051=CARTESIAN_POINT('',(0.138207714141624,-32.1029248328492,-28.2484175959528));
#73052=CARTESIAN_POINT('',(-0.437716061833263,-32.4244114123644,-27.8652848098447));
#73053=CARTESIAN_POINT('Ctrl Pts',(0.138207714141623,-33.3938750538235,
-26.7099230322464));
#73054=CARTESIAN_POINT('Ctrl Pts',(0.161789033936548,-32.7483999433363,
-27.4791703140996));
#73055=CARTESIAN_POINT('Ctrl Pts',(0.138207714141624,-32.1029248328492,
-28.2484175959527));
#73056=CARTESIAN_POINT('Origin',(17.5,-37.0225860117848,-21.375));
#73057=CARTESIAN_POINT('',(0.138207714141622,-36.5204955072697,-22.244646263818));
#73058=CARTESIAN_POINT('',(-0.437716061833263,-36.7705676731535,-21.8115085669484));
#73059=CARTESIAN_POINT('Ctrl Pts',(0.138207714141633,-37.5246765162999,
-20.5053537361819));
#73060=CARTESIAN_POINT('Ctrl Pts',(0.161789033936547,-37.0225860117848,
-21.375));
#73061=CARTESIAN_POINT('Ctrl Pts',(0.138207714141622,-36.5204955072697,
-22.244646263818));
#73062=CARTESIAN_POINT('Origin',(17.5,-40.1718595385976,-14.6213611271723));
#73063=CARTESIAN_POINT('',(0.138207714141633,-39.8284094059642,-15.5649826112914));
#73064=CARTESIAN_POINT('',(-0.437716061833263,-39.9994688419988,-15.0950006734014));
#73065=CARTESIAN_POINT('Ctrl Pts',(0.138207714141626,-40.515309671231,-13.6777396430533));
#73066=CARTESIAN_POINT('Ctrl Pts',(0.161789033936555,-40.1718595385976,
-14.6213611271723));
#73067=CARTESIAN_POINT('Ctrl Pts',(0.138207714141633,-39.8284094059642,
-15.5649826112914));
#73068=CARTESIAN_POINT('Origin',(17.5,-42.1005314412719,-7.42345959526126));
#73069=CARTESIAN_POINT('',(0.138207714141624,-41.9261572390061,-8.41238483838183));
#73070=CARTESIAN_POINT('',(-0.437716061833263,-42.013006390788,-7.91983882283192));
#73071=CARTESIAN_POINT('Ctrl Pts',(0.138207714141624,-42.2749056435377,
-6.43453435214068));
#73072=CARTESIAN_POINT('Ctrl Pts',(0.161789033936547,-42.1005314412719,
-7.42345959526126));
#73073=CARTESIAN_POINT('Ctrl Pts',(0.138207714141624,-41.9261572390061,
-8.41238483838183));
#73074=CARTESIAN_POINT('Origin',(17.5,-42.75,5.23536506635493E-15));
#73075=CARTESIAN_POINT('',(0.138207714141623,-42.75,-1.00418100903021));
#73076=CARTESIAN_POINT('',(-0.437716061833263,-42.75,-0.50403667726254));
#73077=CARTESIAN_POINT('',(0.149999999999998,-42.75,-5.05935899139558E-15));
#73078=CARTESIAN_POINT('Ctrl Pts',(0.149999999999998,-42.75,-4.88335291643624E-15));
#73079=CARTESIAN_POINT('Ctrl Pts',(0.149999999999999,-42.75,-0.502021265003248));
#73080=CARTESIAN_POINT('Ctrl Pts',(0.138207714141623,-42.75,-1.00418100903021));
#73081=CARTESIAN_POINT('Ctrl Pts',(0.13820771414162,-42.75,1.00418100903021));
#73082=CARTESIAN_POINT('Ctrl Pts',(0.149999999999998,-42.75,0.502021265003246));
#73083=CARTESIAN_POINT('Ctrl Pts',(0.149999999999998,-42.75,-4.88335291643624E-15));
#73084=CARTESIAN_POINT('Origin',(17.5,-42.1005314412719,7.42345959526129));
#73085=CARTESIAN_POINT('',(0.138207714141624,-42.2749056435377,6.43453435214071));
#73086=CARTESIAN_POINT('',(-0.437716061833263,-42.1880564917558,6.92708036769062));
#73087=CARTESIAN_POINT('Ctrl Pts',(0.138207714141622,-41.926157239006,8.41238483838185));
#73088=CARTESIAN_POINT('Ctrl Pts',(0.161789033936547,-42.1005314412719,
7.42345959526129));
#73089=CARTESIAN_POINT('Ctrl Pts',(0.138207714141624,-42.2749056435377,
6.43453435214071));
#73090=CARTESIAN_POINT('Origin',(17.5,-40.1718595385976,14.6213611271723));
#73091=CARTESIAN_POINT('',(0.138207714141621,-40.515309671231,13.6777396430533));
#73092=CARTESIAN_POINT('',(-0.437716061833263,-40.3442502351963,14.1477215809433));
#73093=CARTESIAN_POINT('Ctrl Pts',(0.138207714141621,-39.8284094059642,
15.5649826112914));
#73094=CARTESIAN_POINT('Ctrl Pts',(0.161789033936546,-40.1718595385976,
14.6213611271723));
#73095=CARTESIAN_POINT('Ctrl Pts',(0.138207714141621,-40.515309671231,13.6777396430533));
#73096=CARTESIAN_POINT('Origin',(17.5,-37.0225860117848,21.375));
#73097=CARTESIAN_POINT('',(0.138207714141623,-37.5246765162999,20.5053537361819));
#73098=CARTESIAN_POINT('',(-0.437716061833263,-37.274604350416,20.9384914330515));
#73099=CARTESIAN_POINT('Ctrl Pts',(0.138207714141621,-36.5204955072697,
22.244646263818));
#73100=CARTESIAN_POINT('Ctrl Pts',(0.161789033936545,-37.0225860117848,
21.375));
#73101=CARTESIAN_POINT('Ctrl Pts',(0.138207714141623,-37.5246765162999,
20.5053537361819));
#73102=CARTESIAN_POINT('Origin',(17.5,-32.7483999433363,27.4791703140996));
#73103=CARTESIAN_POINT('',(0.138207714141626,-33.3938750538235,26.7099230322464));
#73104=CARTESIAN_POINT('',(-0.437716061833263,-33.0723884743082,27.0930558183544));
#73105=CARTESIAN_POINT('Ctrl Pts',(0.138207714141625,-32.1029248328492,
28.2484175959528));
#73106=CARTESIAN_POINT('Ctrl Pts',(0.161789033936548,-32.7483999433363,
27.4791703140996));
#73107=CARTESIAN_POINT('Ctrl Pts',(0.138207714141626,-33.3938750538235,
26.7099230322464));
#73108=CARTESIAN_POINT('Origin',(17.5,-27.4791703140996,32.7483999433363));
#73109=CARTESIAN_POINT('',(0.13820771414163,-28.2484175959528,32.1029248328492));
#73110=CARTESIAN_POINT('',(-0.437716061833263,-27.8652848098447,32.4244114123644));
#73111=CARTESIAN_POINT('Ctrl Pts',(0.138207714141626,-26.7099230322463,
33.3938750538235));
#73112=CARTESIAN_POINT('Ctrl Pts',(0.161789033936555,-27.4791703140996,
32.7483999433363));
#73113=CARTESIAN_POINT('Ctrl Pts',(0.13820771414163,-28.2484175959528,32.1029248328492));
#73114=CARTESIAN_POINT('Origin',(17.5,-21.375,37.0225860117848));
#73115=CARTESIAN_POINT('',(0.138207714141625,-22.244646263818,36.5204955072697));
#73116=CARTESIAN_POINT('',(-0.437716061833263,-21.8115085669485,36.7705676731535));
#73117=CARTESIAN_POINT('Ctrl Pts',(0.138207714141623,-20.5053537361819,
37.5246765162999));
#73118=CARTESIAN_POINT('Ctrl Pts',(0.161789033936548,-21.375,37.0225860117848));
#73119=CARTESIAN_POINT('Ctrl Pts',(0.138207714141625,-22.244646263818,36.5204955072697));
#73120=CARTESIAN_POINT('Origin',(17.5,-14.6213611271723,40.1718595385976));
#73121=CARTESIAN_POINT('',(0.138207714141622,-15.5649826112914,39.8284094059642));
#73122=CARTESIAN_POINT('',(-0.437716061833263,-15.0950006734014,39.9994688419988));
#73123=CARTESIAN_POINT('Ctrl Pts',(0.138207714141626,-13.6777396430533,
40.515309671231));
#73124=CARTESIAN_POINT('Ctrl Pts',(0.161789033936544,-14.6213611271723,
40.1718595385976));
#73125=CARTESIAN_POINT('Ctrl Pts',(0.138207714141622,-15.5649826112914,
39.8284094059642));
#73126=CARTESIAN_POINT('Origin',(17.5,-7.42345959526127,42.1005314412719));
#73127=CARTESIAN_POINT('',(0.138207714141624,-8.41238483838185,41.9261572390061));
#73128=CARTESIAN_POINT('',(-0.437716061833263,-7.91983882283194,42.013006390788));
#73129=CARTESIAN_POINT('Ctrl Pts',(0.138207714141616,-6.4345343521407,42.2749056435377));
#73130=CARTESIAN_POINT('Ctrl Pts',(0.161789033936548,-7.42345959526127,
42.1005314412719));
#73131=CARTESIAN_POINT('Ctrl Pts',(0.138207714141624,-8.41238483838185,
41.9261572390061));
#73132=CARTESIAN_POINT('Origin',(17.5,2.61768253317747E-15,42.75));
#73133=CARTESIAN_POINT('',(0.13820771414162,-1.0041810090302,42.75));
#73134=CARTESIAN_POINT('',(-0.437716061833263,-0.504036677262543,42.75));
#73135=CARTESIAN_POINT('Ctrl Pts',(0.138207714141629,1.00418100903022,42.75));
#73136=CARTESIAN_POINT('Ctrl Pts',(0.161789033936545,7.49400541621981E-15,
42.75));
#73137=CARTESIAN_POINT('Ctrl Pts',(0.13820771414162,-1.0041810090302,42.75));
#73138=CARTESIAN_POINT('Origin',(17.5,7.42345959526128,42.1005314412719));
#73139=CARTESIAN_POINT('',(0.138207714141615,6.43453435214071,42.2749056435377));
#73140=CARTESIAN_POINT('',(-0.437716061833263,6.92708036769061,42.1880564917558));
#73141=CARTESIAN_POINT('Ctrl Pts',(0.138207714141621,8.41238483838185,41.9261572390061));
#73142=CARTESIAN_POINT('Ctrl Pts',(0.161789033936541,7.42345959526128,42.1005314412719));
#73143=CARTESIAN_POINT('Ctrl Pts',(0.138207714141615,6.43453435214071,42.2749056435377));
#73144=CARTESIAN_POINT('Origin',(17.5,14.6213611271723,40.1718595385976));
#73145=CARTESIAN_POINT('',(0.138207714141621,13.6777396430533,40.515309671231));
#73146=CARTESIAN_POINT('',(-0.437716061833263,14.1477215809433,40.3442502351963));
#73147=CARTESIAN_POINT('Ctrl Pts',(0.138207714141624,15.5649826112914,39.8284094059642));
#73148=CARTESIAN_POINT('Ctrl Pts',(0.161789033936547,14.6213611271723,40.1718595385976));
#73149=CARTESIAN_POINT('Ctrl Pts',(0.138207714141621,13.6777396430533,40.515309671231));
#73150=CARTESIAN_POINT('Origin',(17.5,21.375,37.0225860117847));
#73151=CARTESIAN_POINT('',(0.138207714141623,20.505353736182,37.5246765162999));
#73152=CARTESIAN_POINT('',(-0.437716061833263,20.9384914330515,37.274604350416));
#73153=CARTESIAN_POINT('Ctrl Pts',(0.138207714141622,22.2446462638181,36.5204955072696));
#73154=CARTESIAN_POINT('Ctrl Pts',(0.161789033936545,21.375,37.0225860117847));
#73155=CARTESIAN_POINT('Ctrl Pts',(0.138207714141623,20.505353736182,37.5246765162999));
#73156=CARTESIAN_POINT('Origin',(17.5,27.4791703140996,32.7483999433363));
#73157=CARTESIAN_POINT('',(0.138207714141625,26.7099230322463,33.3938750538235));
#73158=CARTESIAN_POINT('',(-0.437716061833263,27.0930558183544,33.0723884743082));
#73159=CARTESIAN_POINT('Ctrl Pts',(0.138207714141625,28.2484175959528,32.1029248328492));
#73160=CARTESIAN_POINT('Ctrl Pts',(0.16178903393655,27.4791703140995,32.7483999433363));
#73161=CARTESIAN_POINT('Ctrl Pts',(0.138207714141625,26.7099230322463,33.3938750538235));
#73162=CARTESIAN_POINT('Origin',(17.5,32.7483999433363,27.4791703140996));
#73163=CARTESIAN_POINT('',(0.138207714141624,32.1029248328492,28.2484175959528));
#73164=CARTESIAN_POINT('',(-0.437716061833263,32.4244114123644,27.8652848098447));
#73165=CARTESIAN_POINT('Ctrl Pts',(0.138207714141623,33.3938750538235,26.7099230322464));
#73166=CARTESIAN_POINT('Ctrl Pts',(0.161789033936548,32.7483999433363,27.4791703140996));
#73167=CARTESIAN_POINT('Ctrl Pts',(0.138207714141624,32.1029248328492,28.2484175959527));
#73168=CARTESIAN_POINT('Origin',(17.5,37.0225860117848,21.375));
#73169=CARTESIAN_POINT('',(0.138207714141628,36.5204955072696,22.244646263818));
#73170=CARTESIAN_POINT('',(-0.437716061833263,36.7705676731535,21.8115085669485));
#73171=CARTESIAN_POINT('Ctrl Pts',(0.138207714141626,37.5246765162999,20.5053537361819));
#73172=CARTESIAN_POINT('Ctrl Pts',(0.161789033936552,37.0225860117848,21.375));
#73173=CARTESIAN_POINT('Ctrl Pts',(0.138207714141628,36.5204955072696,22.2446462638181));
#73174=CARTESIAN_POINT('Origin',(17.5,40.1718595385976,14.6213611271723));
#73175=CARTESIAN_POINT('',(0.138207714141622,39.8284094059642,15.5649826112914));
#73176=CARTESIAN_POINT('',(-0.437716061833263,39.9994688419988,15.0950006734014));
#73177=CARTESIAN_POINT('Ctrl Pts',(0.138207714141626,40.515309671231,13.6777396430533));
#73178=CARTESIAN_POINT('Ctrl Pts',(0.161789033936544,40.1718595385976,14.6213611271723));
#73179=CARTESIAN_POINT('Ctrl Pts',(0.138207714141622,39.8284094059642,15.5649826112914));
#73180=CARTESIAN_POINT('Origin',(17.5,42.1005314412719,7.42345959526127));
#73181=CARTESIAN_POINT('',(0.138207714141622,41.9261572390061,8.41238483838184));
#73182=CARTESIAN_POINT('',(-0.437716061833263,42.013006390788,7.91983882283194));
#73183=CARTESIAN_POINT('Ctrl Pts',(0.138207714141617,42.2749056435377,6.4345343521407));
#73184=CARTESIAN_POINT('Ctrl Pts',(0.161789033936546,42.1005314412719,7.42345959526127));
#73185=CARTESIAN_POINT('Ctrl Pts',(0.138207714141622,41.9261572390061,8.41238483838184));
#73186=CARTESIAN_POINT('Origin',(17.5,42.75,0.));
#73187=CARTESIAN_POINT('',(0.138207714141622,42.75,1.00418100903021));
#73188=CARTESIAN_POINT('',(-0.437716061833263,42.75,0.504036677262545));
#73189=CARTESIAN_POINT('Ctrl Pts',(0.13820771414163,42.75,-1.00418100903022));
#73190=CARTESIAN_POINT('Ctrl Pts',(0.161789033936547,42.75,-1.80411241501588E-15));
#73191=CARTESIAN_POINT('Ctrl Pts',(0.138207714141622,42.75,1.00418100903021));
#73192=CARTESIAN_POINT('Origin',(33.1,37.7092141076143,-4.97369795887321));
#73193=CARTESIAN_POINT('',(29.9040600247032,41.9886110647639,-5.12313779357752));
#73194=CARTESIAN_POINT('',(17.5,41.9886110647639,-5.12313779357752));
#73195=CARTESIAN_POINT('',(30.5247014514712,37.5318349744051,-4.96750374304977));
#73196=CARTESIAN_POINT('Origin',(30.5,37.7092141076143,-4.97369795887321));
#73197=CARTESIAN_POINT('',(29.9005519666592,41.9206753505941,-5.65216579287046));
#73198=CARTESIAN_POINT('Origin',(35.8405517186909,0.,0.));
#73199=CARTESIAN_POINT('',(30.4955273645547,37.6544606275072,-5.46749010626366));
#73200=CARTESIAN_POINT('Origin',(30.5,37.6223900187809,-5.46610183537932));
#73201=CARTESIAN_POINT('',(24.1697957402248,41.8715390397407,-6.00534915250319));
#73202=CARTESIAN_POINT('Origin',(97.7155570771054,0.,0.));
#73203=CARTESIAN_POINT('',(24.1012882089558,37.6326386190063,-5.86270716268919));
#73204=CARTESIAN_POINT('Origin',(24.1,37.5529307477141,-5.8600249365842));
#73205=CARTESIAN_POINT('',(23.3381365738089,41.9060788618227,-5.75938837262207));
#73206=CARTESIAN_POINT('Origin',(8.01433437672608,0.,0.));
#73207=CARTESIAN_POINT('',(23.1004586919557,37.6133097693334,-5.56495784004782));
#73208=CARTESIAN_POINT('Origin',(23.1,37.6050252010142,-5.56458261068054));
#73209=CARTESIAN_POINT('',(22.6451513366954,41.9578594516632,-5.3691740737731));
#73210=CARTESIAN_POINT('Origin',(14.1732738814488,0.,0.));
#73211=CARTESIAN_POINT('',(22.399682944576,37.6689447622493,-5.17040276961776));
#73212=CARTESIAN_POINT('Origin',(22.4,37.674484472081,-5.17065950947565));
#73213=CARTESIAN_POINT('',(21.896707744792,41.9886110647639,-5.12313779357752));
#73214=CARTESIAN_POINT('Origin',(9.86169260701005,0.,0.));
#73215=CARTESIAN_POINT('',(21.7998387845652,37.7020801925101,-4.97344883706828));
#73216=CARTESIAN_POINT('Origin',(21.8,37.7092141076143,-4.97369795887321));
#73217=CARTESIAN_POINT('',(13.103292255208,41.9886110647639,-5.12313779357752));
#73218=CARTESIAN_POINT('',(17.5,41.9886110647639,-5.12313779357752));
#73219=CARTESIAN_POINT('',(13.2021921742626,37.6122086000507,-4.97031045190415));
#73220=CARTESIAN_POINT('Origin',(13.2,37.7092141076143,-4.97369795887321));
#73221=CARTESIAN_POINT('',(12.3548486633046,41.9578594516632,-5.3691740737731));
#73222=CARTESIAN_POINT('Origin',(25.13830739299,0.,0.));
#73223=CARTESIAN_POINT('',(12.6002487187375,37.6701387661531,-5.17045810616099));
#73224=CARTESIAN_POINT('Origin',(12.6,37.674484472081,-5.17065950947565));
#73225=CARTESIAN_POINT('',(11.6618634261911,41.9060788618227,-5.75938837262207));
#73226=CARTESIAN_POINT('Origin',(20.8267261185512,0.,0.));
#73227=CARTESIAN_POINT('',(11.8996457869536,37.6114227454796,-5.56487237189312));
#73228=CARTESIAN_POINT('Origin',(11.9,37.6050252010142,-5.56458261068054));
#73229=CARTESIAN_POINT('',(10.8302042597752,41.8715390397407,-6.00534915250319));
#73230=CARTESIAN_POINT('Origin',(26.9856656232739,0.,0.));
#73231=CARTESIAN_POINT('',(10.899790263986,37.565908154163,-5.86046163546711));
#73232=CARTESIAN_POINT('Origin',(10.9,37.5529307477141,-5.8600249365842));
#73233=CARTESIAN_POINT('',(5.09944803334083,41.9206753505941,-5.65216579287046));
#73234=CARTESIAN_POINT('Origin',(-62.7155570771055,0.,0.));
#73235=CARTESIAN_POINT('',(4.55736144060343,38.0336947942479,-5.48390637564378));
#73236=CARTESIAN_POINT('Origin',(4.5,37.6223900187809,-5.46610183537932));
#73237=CARTESIAN_POINT('',(5.09593997529677,41.9886110647639,-5.12313779357752));
#73238=CARTESIAN_POINT('Origin',(-0.840551718690872,0.,0.));
#73239=CARTESIAN_POINT('',(4.49524972087093,37.6751027358433,-4.97250676352255));
#73240=CARTESIAN_POINT('Origin',(4.5,37.7092141076143,-4.97369795887321));
#73241=CARTESIAN_POINT('',(1.67735469196905,41.9886110647639,-5.12313779357752));
#73242=CARTESIAN_POINT('',(17.5,41.9886110647639,-5.12313779357752));
#73243=CARTESIAN_POINT('',(1.90350512467335,37.6418431848034,-4.97134531440729));
#73244=CARTESIAN_POINT('Origin',(1.9,37.7092141076143,-4.97369795887321));
#73245=CARTESIAN_POINT('',(0.600000000000001,41.8659567209931,-6.04414326732376));
#73246=CARTESIAN_POINT('Origin',(8.14497546096349,0.,0.));
#73247=CARTESIAN_POINT('Ctrl Pts',(0.138207714141615,42.2749056435377,-6.43453435214071));
#73248=CARTESIAN_POINT('Ctrl Pts',(0.370217470893695,42.0700781197368,-6.23839136562887));
#73249=CARTESIAN_POINT('Ctrl Pts',(0.600000000000008,41.8659567209931,-6.04414326732376));
#73250=CARTESIAN_POINT('Origin',(1.9,37.1361751213135,-8.2235635438135));
#73251=CARTESIAN_POINT('',(5.09593997529677,41.2086042970448,-9.54677599452213));
#73252=CARTESIAN_POINT('',(17.5,41.2086042970448,-9.54677599452213));
#73253=CARTESIAN_POINT('',(4.47529854852883,36.9673747121716,-8.16871696615113));
#73254=CARTESIAN_POINT('Origin',(4.5,37.1361751213135,-8.2235635438135));
#73255=CARTESIAN_POINT('',(5.09944803334083,41.325703839893,-9.02641690470011));
#73256=CARTESIAN_POINT('Origin',(-0.840551718690874,0.,0.));
#73257=CARTESIAN_POINT('',(4.50447263544529,37.253610541118,-7.74082391359485));
#73258=CARTESIAN_POINT('Origin',(4.5,37.2229992101469,-7.7311596673074));
#73259=CARTESIAN_POINT('',(10.8302042597752,41.4003266344532,-8.6777274997883));
#73260=CARTESIAN_POINT('Origin',(-62.7155570771054,0.,0.));
#73261=CARTESIAN_POINT('',(10.8987117910442,37.3682767550424,-7.36197779558791));
#73262=CARTESIAN_POINT('Origin',(10.9,37.2924584812137,-7.33723656610251));
#73263=CARTESIAN_POINT('',(11.6618634261911,41.3486599091995,-8.92066834454427));
#73264=CARTESIAN_POINT('Origin',(26.9856656232739,0.,0.));
#73265=CARTESIAN_POINT('',(11.8995413080444,37.2482773116316,-7.63515978098257));
#73266=CARTESIAN_POINT('Origin',(11.9,37.2403640279136,-7.63267889200617));
#73267=CARTESIAN_POINT('',(12.3548486633046,41.2638565969525,-9.30505984645652));
#73268=CARTESIAN_POINT('Origin',(20.8267261185512,0.,0.));
#73269=CARTESIAN_POINT('',(12.600317055424,37.1656113221937,-8.02494855741037));
#73270=CARTESIAN_POINT('Origin',(12.6,37.1709047568469,-8.02660199321106));
#73271=CARTESIAN_POINT('',(13.103292255208,41.2086042970448,-9.54677599452213));
#73272=CARTESIAN_POINT('Origin',(25.13830739299,0.,0.));
#73273=CARTESIAN_POINT('',(13.2001612154348,37.1293862292573,-8.22135769906884));
#73274=CARTESIAN_POINT('Origin',(13.2,37.1361751213135,-8.2235635438135));
#73275=CARTESIAN_POINT('',(21.896707744792,41.2086042970448,-9.54677599452213));
#73276=CARTESIAN_POINT('',(17.5,41.2086042970448,-9.54677599452213));
#73277=CARTESIAN_POINT('',(21.7978078257374,37.0438611660612,-8.19356892151487));
#73278=CARTESIAN_POINT('Origin',(21.8,37.1361751213135,-8.2235635438135));
#73279=CARTESIAN_POINT('',(22.6451513366954,41.2638565969525,-9.30505984645652));
#73280=CARTESIAN_POINT('Origin',(9.86169260701005,0.,0.));
#73281=CARTESIAN_POINT('',(22.3997512812625,37.1667522450638,-8.02530493145534));
#73282=CARTESIAN_POINT('Origin',(22.4,37.1709047568469,-8.02660199321106));
#73283=CARTESIAN_POINT('',(23.3381365738089,41.3486599091995,-8.92066834454427));
#73284=CARTESIAN_POINT('Origin',(14.1732738814488,0.,0.));
#73285=CARTESIAN_POINT('',(23.1003542130464,37.2464748574103,-7.6345946946079));
#73286=CARTESIAN_POINT('Origin',(23.1,37.2403640279136,-7.63267889200617));
#73287=CARTESIAN_POINT('',(24.1697957402248,41.4003266344532,-8.6777274997883));
#73288=CARTESIAN_POINT('Origin',(8.01433437672608,0.,0.));
#73289=CARTESIAN_POINT('',(24.100209736014,37.3048026141052,-7.34126473779837));
#73290=CARTESIAN_POINT('Origin',(24.1,37.2924584812137,-7.33723656610251));
#73291=CARTESIAN_POINT('',(29.9005519666592,41.325703839893,-9.02641690470011));
#73292=CARTESIAN_POINT('Origin',(97.7155570771055,0.,0.));
#73293=CARTESIAN_POINT('',(30.4426385593966,37.6155887839604,-7.85510339046017));
#73294=CARTESIAN_POINT('Origin',(30.5,37.2229992101469,-7.7311596673074));
#73295=CARTESIAN_POINT('',(29.9040600247032,41.2086042970448,-9.54677599452213));
#73296=CARTESIAN_POINT('Origin',(35.8405517186909,0.,0.));
#73297=CARTESIAN_POINT('',(30.5047502791291,37.1037135041708,-8.21301612503228));
#73298=CARTESIAN_POINT('Origin',(30.5,37.1361751213135,-8.2235635438135));
#73299=CARTESIAN_POINT('',(17.5,41.2086042970448,-9.54677599452213));
#73300=CARTESIAN_POINT('Origin',(17.5,42.1005314412719,-7.42345959526127));
#73301=CARTESIAN_POINT('Ctrl Pts',(34.8617922858584,42.2749056435377,-6.4345343521407));
#73302=CARTESIAN_POINT('Ctrl Pts',(34.8382109660635,42.1005314412719,-7.42345959526127));
#73303=CARTESIAN_POINT('Ctrl Pts',(34.8617922858584,41.9261572390061,-8.41238483838185));
#73304=CARTESIAN_POINT('Origin',(34.7,0.,0.));
#73305=CARTESIAN_POINT('',(35.,-42.9,-5.25373476834215E-15));
#73306=CARTESIAN_POINT('Origin',(35.,0.,0.));
#73307=CARTESIAN_POINT('',(34.85,-42.75,-5.28447809747245E-15));
#73308=CARTESIAN_POINT('',(34.7,-42.6,-5.21699536436772E-15));
#73309=CARTESIAN_POINT('Ctrl Pts',(34.85,-42.75,-5.33359112858996E-15));
#73310=CARTESIAN_POINT('Ctrl Pts',(34.85,-42.75,0.50202126500325));
#73311=CARTESIAN_POINT('Ctrl Pts',(34.8617922858584,-42.75,1.00418100903022));
#73312=CARTESIAN_POINT('Origin',(34.4,0.,0.));
#73313=CARTESIAN_POINT('Ctrl Pts',(34.8617922858584,-42.2749056435377,6.43453435214071));
#73314=CARTESIAN_POINT('Ctrl Pts',(34.8382109660634,-42.1005314412719,7.42345959526129));
#73315=CARTESIAN_POINT('Ctrl Pts',(34.8617922858584,-41.926157239006,8.41238483838188));
#73316=CARTESIAN_POINT('Origin',(34.4,0.,0.));
#73317=CARTESIAN_POINT('Ctrl Pts',(34.8617922858584,-40.515309671231,13.6777396430533));
#73318=CARTESIAN_POINT('Ctrl Pts',(34.8382109660634,-40.1718595385976,14.6213611271723));
#73319=CARTESIAN_POINT('Ctrl Pts',(34.8617922858584,-39.8284094059642,15.5649826112914));
#73320=CARTESIAN_POINT('Origin',(34.4,0.,0.));
#73321=CARTESIAN_POINT('Ctrl Pts',(34.8617922858584,-37.5246765162999,20.5053537361819));
#73322=CARTESIAN_POINT('Ctrl Pts',(34.8382109660634,-37.0225860117847,21.375));
#73323=CARTESIAN_POINT('Ctrl Pts',(34.8617922858584,-36.5204955072696,22.2446462638181));
#73324=CARTESIAN_POINT('Origin',(34.4,0.,0.));
#73325=CARTESIAN_POINT('Ctrl Pts',(34.8617922858584,-33.3938750538235,26.7099230322464));
#73326=CARTESIAN_POINT('Ctrl Pts',(34.8382109660634,-32.7483999433363,27.4791703140996));
#73327=CARTESIAN_POINT('Ctrl Pts',(34.8617922858584,-32.1029248328491,28.2484175959528));
#73328=CARTESIAN_POINT('Origin',(34.4,0.,0.));
#73329=CARTESIAN_POINT('Ctrl Pts',(34.8617922858584,-28.2484175959528,32.1029248328492));
#73330=CARTESIAN_POINT('Ctrl Pts',(34.8382109660634,-27.4791703140996,32.7483999433363));
#73331=CARTESIAN_POINT('Ctrl Pts',(34.8617922858584,-26.7099230322463,33.3938750538235));
#73332=CARTESIAN_POINT('Origin',(34.4,0.,0.));
#73333=CARTESIAN_POINT('Ctrl Pts',(34.8617922858584,-22.244646263818,36.5204955072697));
#73334=CARTESIAN_POINT('Ctrl Pts',(34.8382109660635,-21.375,37.0225860117848));
#73335=CARTESIAN_POINT('Ctrl Pts',(34.8617922858584,-20.5053537361819,37.5246765162999));
#73336=CARTESIAN_POINT('Origin',(34.4,0.,0.));
#73337=CARTESIAN_POINT('Ctrl Pts',(34.8617922858584,-15.5649826112914,39.8284094059642));
#73338=CARTESIAN_POINT('Ctrl Pts',(34.8382109660635,-14.6213611271723,40.1718595385976));
#73339=CARTESIAN_POINT('Ctrl Pts',(34.8617922858584,-13.6777396430533,40.515309671231));
#73340=CARTESIAN_POINT('Origin',(34.4,0.,0.));
#73341=CARTESIAN_POINT('Ctrl Pts',(34.8617922858584,-8.41238483838184,41.9261572390061));
#73342=CARTESIAN_POINT('Ctrl Pts',(34.8382109660634,-7.42345959526127,42.1005314412719));
#73343=CARTESIAN_POINT('Ctrl Pts',(34.8617922858584,-6.4345343521407,42.2749056435377));
#73344=CARTESIAN_POINT('Origin',(34.4,0.,0.));
#73345=CARTESIAN_POINT('Ctrl Pts',(34.8617922858584,-1.0041810090302,42.75));
#73346=CARTESIAN_POINT('Ctrl Pts',(34.8382109660635,4.30211422042248E-15,
42.75));
#73347=CARTESIAN_POINT('Ctrl Pts',(34.8617922858584,1.00418100903021,42.75));
#73348=CARTESIAN_POINT('Origin',(34.4,0.,0.));
#73349=CARTESIAN_POINT('Ctrl Pts',(34.8617922858584,6.4345343521407,42.2749056435377));
#73350=CARTESIAN_POINT('Ctrl Pts',(34.8382109660634,7.42345959526127,42.1005314412719));
#73351=CARTESIAN_POINT('Ctrl Pts',(34.8617922858584,8.41238483838185,41.9261572390061));
#73352=CARTESIAN_POINT('Origin',(34.4,0.,0.));
#73353=CARTESIAN_POINT('Ctrl Pts',(34.8617922858584,13.6777396430533,40.515309671231));
#73354=CARTESIAN_POINT('Ctrl Pts',(34.8382109660634,14.6213611271723,40.1718595385976));
#73355=CARTESIAN_POINT('Ctrl Pts',(34.8617922858584,15.5649826112914,39.8284094059642));
#73356=CARTESIAN_POINT('Origin',(34.4,0.,0.));
#73357=CARTESIAN_POINT('Ctrl Pts',(34.8617922858584,20.5053537361819,37.5246765162999));
#73358=CARTESIAN_POINT('Ctrl Pts',(34.8382109660634,21.375,37.0225860117847));
#73359=CARTESIAN_POINT('Ctrl Pts',(34.8617922858584,22.2446462638181,36.5204955072696));
#73360=CARTESIAN_POINT('Origin',(34.4,0.,0.));
#73361=CARTESIAN_POINT('Ctrl Pts',(34.8617922858584,26.7099230322463,33.3938750538235));
#73362=CARTESIAN_POINT('Ctrl Pts',(34.8382109660634,27.4791703140995,32.7483999433363));
#73363=CARTESIAN_POINT('Ctrl Pts',(34.8617922858584,28.2484175959528,32.1029248328492));
#73364=CARTESIAN_POINT('Origin',(34.4,0.,0.));
#73365=CARTESIAN_POINT('Ctrl Pts',(34.8617922858584,32.1029248328492,28.2484175959528));
#73366=CARTESIAN_POINT('Ctrl Pts',(34.8382109660634,32.7483999433363,27.4791703140995));
#73367=CARTESIAN_POINT('Ctrl Pts',(34.8617922858584,33.3938750538235,26.7099230322464));
#73368=CARTESIAN_POINT('Origin',(34.4,0.,0.));
#73369=CARTESIAN_POINT('Ctrl Pts',(34.8617922858584,36.5204955072696,22.244646263818));
#73370=CARTESIAN_POINT('Ctrl Pts',(34.8382109660634,37.0225860117847,21.375));
#73371=CARTESIAN_POINT('Ctrl Pts',(34.8617922858584,37.5246765162998,20.5053537361819));
#73372=CARTESIAN_POINT('Origin',(34.4,0.,0.));
#73373=CARTESIAN_POINT('Ctrl Pts',(34.8617922858584,39.8284094059642,15.5649826112914));
#73374=CARTESIAN_POINT('Ctrl Pts',(34.8382109660635,40.1718595385976,14.6213611271723));
#73375=CARTESIAN_POINT('Ctrl Pts',(34.8617922858584,40.515309671231,13.6777396430533));
#73376=CARTESIAN_POINT('Origin',(34.4,0.,0.));
#73377=CARTESIAN_POINT('Ctrl Pts',(34.8617922858584,41.9261572390061,8.41238483838185));
#73378=CARTESIAN_POINT('Ctrl Pts',(34.8382109660634,42.1005314412719,7.42345959526127));
#73379=CARTESIAN_POINT('Ctrl Pts',(34.8617922858584,42.2749056435377,6.4345343521407));
#73380=CARTESIAN_POINT('Origin',(34.4,0.,0.));
#73381=CARTESIAN_POINT('',(34.4,42.2794732300362,-1.31762794090604));
#73382=CARTESIAN_POINT('Ctrl Pts',(34.8617922858584,42.75,-1.00418100903021));
#73383=CARTESIAN_POINT('Ctrl Pts',(34.6297825290987,42.5142243943529,-1.16177621660715));
#73384=CARTESIAN_POINT('Ctrl Pts',(34.4,42.2794732300361,-1.31762794090604));
#73385=CARTESIAN_POINT('Origin',(34.4,0.,0.));
#73386=CARTESIAN_POINT('Origin',(34.4,0.,0.));
#73387=CARTESIAN_POINT('Ctrl Pts',(34.8617922858584,40.515309671231,-13.6777396430533));
#73388=CARTESIAN_POINT('Ctrl Pts',(34.8382109660634,40.1718595385976,-14.6213611271724));
#73389=CARTESIAN_POINT('Ctrl Pts',(34.8617922858584,39.8284094059641,-15.5649826112914));
#73390=CARTESIAN_POINT('Origin',(34.4,0.,0.));
#73391=CARTESIAN_POINT('Ctrl Pts',(34.8617922858584,37.5246765162999,-20.505353736182));
#73392=CARTESIAN_POINT('Ctrl Pts',(34.8382109660634,37.0225860117847,-21.375));
#73393=CARTESIAN_POINT('Ctrl Pts',(34.8617922858584,36.5204955072696,-22.2446462638181));
#73394=CARTESIAN_POINT('Origin',(34.4,0.,0.));
#73395=CARTESIAN_POINT('Ctrl Pts',(34.8617922858584,33.3938750538235,-26.7099230322464));
#73396=CARTESIAN_POINT('Ctrl Pts',(34.8382109660635,32.7483999433363,-27.4791703140996));
#73397=CARTESIAN_POINT('Ctrl Pts',(34.8617922858584,32.1029248328491,-28.2484175959528));
#73398=CARTESIAN_POINT('Origin',(34.4,0.,0.));
#73399=CARTESIAN_POINT('Ctrl Pts',(34.8617922858584,28.2484175959528,-32.1029248328492));
#73400=CARTESIAN_POINT('Ctrl Pts',(34.8382109660634,27.4791703140995,-32.7483999433363));
#73401=CARTESIAN_POINT('Ctrl Pts',(34.8617922858584,26.7099230322463,-33.3938750538235));
#73402=CARTESIAN_POINT('Origin',(34.4,0.,0.));
#73403=CARTESIAN_POINT('Ctrl Pts',(34.8617922858584,22.2446462638181,-36.5204955072696));
#73404=CARTESIAN_POINT('Ctrl Pts',(34.8382109660635,21.375,-37.0225860117847));
#73405=CARTESIAN_POINT('Ctrl Pts',(34.8617922858584,20.505353736182,-37.5246765162999));
#73406=CARTESIAN_POINT('Origin',(34.4,0.,0.));
#73407=CARTESIAN_POINT('Ctrl Pts',(34.8617922858584,15.5649826112914,-39.8284094059642));
#73408=CARTESIAN_POINT('Ctrl Pts',(34.8382109660634,14.6213611271723,-40.1718595385976));
#73409=CARTESIAN_POINT('Ctrl Pts',(34.8617922858584,13.6777396430533,-40.515309671231));
#73410=CARTESIAN_POINT('Origin',(34.4,0.,0.));
#73411=CARTESIAN_POINT('Ctrl Pts',(34.8617922858584,8.41238483838183,-41.9261572390061));
#73412=CARTESIAN_POINT('Ctrl Pts',(34.8382109660635,7.42345959526126,-42.1005314412719));
#73413=CARTESIAN_POINT('Ctrl Pts',(34.8617922858584,6.43453435214068,-42.2749056435377));
#73414=CARTESIAN_POINT('Origin',(34.4,0.,0.));
#73415=CARTESIAN_POINT('Ctrl Pts',(34.8617922858584,1.0041810090302,-42.75));
#73416=CARTESIAN_POINT('Ctrl Pts',(34.8382109660634,-8.74300631892311E-15,
-42.75));
#73417=CARTESIAN_POINT('Ctrl Pts',(34.8617922858584,-1.00418100903022,-42.75));
#73418=CARTESIAN_POINT('Origin',(34.4,0.,0.));
#73419=CARTESIAN_POINT('Ctrl Pts',(34.8617922858584,-6.4345343521407,-42.2749056435377));
#73420=CARTESIAN_POINT('Ctrl Pts',(34.8382109660634,-7.42345959526127,-42.1005314412719));
#73421=CARTESIAN_POINT('Ctrl Pts',(34.8617922858584,-8.41238483838184,-41.9261572390061));
#73422=CARTESIAN_POINT('Origin',(34.4,0.,0.));
#73423=CARTESIAN_POINT('Ctrl Pts',(34.8617922858584,-13.6777396430533,-40.515309671231));
#73424=CARTESIAN_POINT('Ctrl Pts',(34.8382109660634,-14.6213611271724,-40.1718595385976));
#73425=CARTESIAN_POINT('Ctrl Pts',(34.8617922858584,-15.5649826112914,-39.8284094059641));
#73426=CARTESIAN_POINT('Origin',(34.4,0.,0.));
#73427=CARTESIAN_POINT('Ctrl Pts',(34.8617922858584,-20.505353736182,-37.5246765162999));
#73428=CARTESIAN_POINT('Ctrl Pts',(34.8382109660634,-21.375,-37.0225860117847));
#73429=CARTESIAN_POINT('Ctrl Pts',(34.8617922858584,-22.2446462638181,-36.5204955072696));
#73430=CARTESIAN_POINT('Origin',(34.4,0.,0.));
#73431=CARTESIAN_POINT('Ctrl Pts',(34.8617922858584,-26.7099230322464,-33.3938750538235));
#73432=CARTESIAN_POINT('Ctrl Pts',(34.8382109660634,-27.4791703140996,-32.7483999433363));
#73433=CARTESIAN_POINT('Ctrl Pts',(34.8617922858584,-28.2484175959528,-32.1029248328491));
#73434=CARTESIAN_POINT('Origin',(34.4,0.,0.));
#73435=CARTESIAN_POINT('Ctrl Pts',(34.8617922858584,-32.1029248328492,-28.2484175959528));
#73436=CARTESIAN_POINT('Ctrl Pts',(34.8382109660634,-32.7483999433363,-27.4791703140995));
#73437=CARTESIAN_POINT('Ctrl Pts',(34.8617922858584,-33.3938750538235,-26.7099230322464));
#73438=CARTESIAN_POINT('Origin',(34.4,0.,0.));
#73439=CARTESIAN_POINT('Ctrl Pts',(34.8617922858584,-36.5204955072697,-22.244646263818));
#73440=CARTESIAN_POINT('Ctrl Pts',(34.8382109660634,-37.0225860117848,-21.375));
#73441=CARTESIAN_POINT('Ctrl Pts',(34.8617922858584,-37.5246765162999,-20.5053537361819));
#73442=CARTESIAN_POINT('Origin',(34.4,0.,0.));
#73443=CARTESIAN_POINT('Ctrl Pts',(34.8617922858584,-39.8284094059642,-15.5649826112914));
#73444=CARTESIAN_POINT('Ctrl Pts',(34.8382109660635,-40.1718595385976,-14.6213611271723));
#73445=CARTESIAN_POINT('Ctrl Pts',(34.8617922858584,-40.515309671231,-13.6777396430533));
#73446=CARTESIAN_POINT('Origin',(34.4,0.,0.));
#73447=CARTESIAN_POINT('Ctrl Pts',(34.8617922858584,-41.9261572390061,-8.41238483838183));
#73448=CARTESIAN_POINT('Ctrl Pts',(34.8382109660635,-42.1005314412719,-7.42345959526126));
#73449=CARTESIAN_POINT('Ctrl Pts',(34.8617922858584,-42.2749056435377,-6.43453435214069));
#73450=CARTESIAN_POINT('Origin',(34.4,0.,0.));
#73451=CARTESIAN_POINT('Ctrl Pts',(34.8617922858584,-42.75,-1.0041810090302));
#73452=CARTESIAN_POINT('Ctrl Pts',(34.85,-42.75,-0.502021265003246));
#73453=CARTESIAN_POINT('Ctrl Pts',(34.85,-42.75,-5.33359112858996E-15));
#73454=CARTESIAN_POINT('Origin',(17.5,0.,0.));
#73455=CARTESIAN_POINT('',(0.600000000000001,40.1803643021789,-13.22226624086));
#73456=CARTESIAN_POINT('Origin',(0.600000000000001,0.,0.));
#73457=CARTESIAN_POINT('',(1.67735469196905,40.4610861730024,-12.3365516130268));
#73458=CARTESIAN_POINT('Origin',(8.14497546096349,0.,0.));
#73459=CARTESIAN_POINT('',(5.09593997529677,40.4610861730024,-12.3365516130268));
#73460=CARTESIAN_POINT('',(17.5,40.4610861730024,-12.3365516130268));
#73461=CARTESIAN_POINT('',(5.09944803334083,40.3023178069695,-12.8457455753269));
#73462=CARTESIAN_POINT('Origin',(-0.840551718690872,0.,0.));
#73463=CARTESIAN_POINT('',(10.8302042597752,40.1925983403041,-13.1850308552912));
#73464=CARTESIAN_POINT('Origin',(-62.7155570771055,0.,0.));
#73465=CARTESIAN_POINT('',(11.6618634261911,40.2693240660821,-12.9488045494888));
#73466=CARTESIAN_POINT('Origin',(26.9856656232739,0.,0.));
#73467=CARTESIAN_POINT('',(12.3548486633046,40.3880779943072,-12.5735100877104));
#73468=CARTESIAN_POINT('Origin',(20.8267261185512,0.,0.));
#73469=CARTESIAN_POINT('',(13.103292255208,40.4610861730024,-12.3365516130268));
#73470=CARTESIAN_POINT('Origin',(25.13830739299,0.,0.));
#73471=CARTESIAN_POINT('',(21.896707744792,40.4610861730024,-12.3365516130268));
#73472=CARTESIAN_POINT('',(17.5,40.4610861730024,-12.3365516130268));
#73473=CARTESIAN_POINT('',(22.6451513366954,40.3880779943072,-12.5735100877104));
#73474=CARTESIAN_POINT('Origin',(9.86169260701006,0.,0.));
#73475=CARTESIAN_POINT('',(23.3381365738089,40.2693240660821,-12.9488045494888));
#73476=CARTESIAN_POINT('Origin',(14.1732738814488,0.,0.));
#73477=CARTESIAN_POINT('',(24.1697957402248,40.1925983403041,-13.1850308552912));
#73478=CARTESIAN_POINT('Origin',(8.01433437672608,0.,0.));
#73479=CARTESIAN_POINT('',(29.9005519666592,40.3023178069695,-12.8457455753269));
#73480=CARTESIAN_POINT('Origin',(97.7155570771054,0.,0.));
#73481=CARTESIAN_POINT('',(29.9040600247032,40.4610861730024,-12.3365516130268));
#73482=CARTESIAN_POINT('Origin',(35.8405517186909,0.,0.));
#73483=CARTESIAN_POINT('',(17.5,40.4610861730024,-12.3365516130268));
#73484=CARTESIAN_POINT('Origin',(33.1,36.2726528263519,-11.4462726220787));
#73485=CARTESIAN_POINT('',(30.5247014514712,36.0990440950346,-11.409370947074));
#73486=CARTESIAN_POINT('Origin',(30.5,36.2726528263519,-11.4462726220787));
#73487=CARTESIAN_POINT('',(30.4955273645547,36.1329850680974,-11.9230551151638));
#73488=CARTESIAN_POINT('Origin',(30.5,36.101642754689,-11.9161189324716));
#73489=CARTESIAN_POINT('',(24.1012882089558,36.0428658633082,-12.3084785844451));
#73490=CARTESIAN_POINT('Origin',(24.1,35.9648346973588,-12.291995980786));
#73491=CARTESIAN_POINT('',(23.1004586919557,36.0755342895717,-12.0118963235317));
#73492=CARTESIAN_POINT('Origin',(23.1,36.0674407403565,-12.0100881945502));
#73493=CARTESIAN_POINT('',(22.399682944576,36.1988378309035,-11.6329963463162));
#73494=CARTESIAN_POINT('Origin',(22.4,36.2042487976867,-11.6342111462359));
#73495=CARTESIAN_POINT('',(21.7998387845652,36.2656705509953,-11.4447884936363));
#73496=CARTESIAN_POINT('Origin',(21.8,36.2726528263519,-11.4462726220787));
#73497=CARTESIAN_POINT('',(13.2021921742626,36.1777092848303,-11.4260917493401));
#73498=CARTESIAN_POINT('Origin',(13.2,36.2726528263519,-11.4462726220787));
#73499=CARTESIAN_POINT('',(12.6002487187375,36.2000040861152,-11.633258178775));
#73500=CARTESIAN_POINT('Origin',(12.6,36.2042487976867,-11.6342111462359));
#73501=CARTESIAN_POINT('',(11.8996457869536,36.0736907752397,-12.0114844755769));
#73502=CARTESIAN_POINT('Origin',(11.9,36.0674407403565,-12.0100881945502));
#73503=CARTESIAN_POINT('',(10.899790263986,35.9775391158784,-12.2946795482123));
#73504=CARTESIAN_POINT('Origin',(10.9,35.9648346973588,-12.291995980786));
#73505=CARTESIAN_POINT('',(4.55736144060343,36.5036071604488,-12.0050753064885));
#73506=CARTESIAN_POINT('Origin',(4.5,36.101642754689,-11.9161189324716));
#73507=CARTESIAN_POINT('',(4.49524972087093,36.2392665318678,-11.4391761461162));
#73508=CARTESIAN_POINT('Origin',(4.5,36.2726528263519,-11.4462726220787));
#73509=CARTESIAN_POINT('',(1.90350512467335,36.2067139516643,-11.4322568815947));
#73510=CARTESIAN_POINT('Origin',(1.9,36.2726528263519,-11.4462726220787));
#73511=CARTESIAN_POINT('Ctrl Pts',(0.13820771414162,40.515309671231,-13.6777396430533));
#73512=CARTESIAN_POINT('Ctrl Pts',(0.370217470898406,40.3476538099281,-13.4490085829888));
#73513=CARTESIAN_POINT('Ctrl Pts',(0.600000000000009,40.1803643021789,-13.22226624086));
#73514=CARTESIAN_POINT('Origin',(1.9,35.1439863533772,-14.5472582706722));
#73515=CARTESIAN_POINT('',(5.09593997529677,38.9247727484987,-16.5575380560557));
#73516=CARTESIAN_POINT('',(17.5,38.9247727484987,-16.5575380560557));
#73517=CARTESIAN_POINT('',(4.47529854852883,34.987274410005,-14.4639330523272));
#73518=CARTESIAN_POINT('Origin',(4.5,35.1439863533772,-14.5472582706722));
#73519=CARTESIAN_POINT('',(5.09944803334083,39.1304526938498,-16.0654185122698));
#73520=CARTESIAN_POINT('Origin',(-0.840551718690874,0.,0.));
#73521=CARTESIAN_POINT('',(4.50447263544529,35.343464522354,-14.0922449867892));
#73522=CARTESIAN_POINT('Origin',(4.5,35.31499642504,-14.0774119602792));
#73523=CARTESIAN_POINT('',(10.8302042597752,39.2644910802189,-15.7349845952073));
#73524=CARTESIAN_POINT('Origin',(-62.7155570771055,0.,0.));
#73525=CARTESIAN_POINT('',(10.8987117910442,35.5221746368434,-13.7390659716653));
#73526=CARTESIAN_POINT('Origin',(10.9,35.4518044823703,-13.7015349119649));
#73527=CARTESIAN_POINT('',(11.6618634261911,39.1714230536436,-15.96526278996));
#73528=CARTESIAN_POINT('Origin',(26.9856656232739,0.,0.));
#73529=CARTESIAN_POINT('',(11.8995413080444,35.35656070068,-13.9872600241959));
#73530=CARTESIAN_POINT('Origin',(11.9,35.3491984393726,-13.9834426982006));
#73531=CARTESIAN_POINT('',(12.3548486633046,39.0211592104439,-16.3290885806033));
#73532=CARTESIAN_POINT('Origin',(20.8267261185512,0.,0.));
#73533=CARTESIAN_POINT('',(12.600317055424,35.2074644826695,-14.3567722348383));
#73534=CARTESIAN_POINT('Origin',(12.6,35.2123903820423,-14.359319746515));
#73535=CARTESIAN_POINT('',(13.103292255208,38.9247727484987,-16.5575380560557));
#73536=CARTESIAN_POINT('Origin',(25.13830739299,0.,0.));
#73537=CARTESIAN_POINT('',(13.2001612154348,35.137683640766,-14.5439070589318));
#73538=CARTESIAN_POINT('Origin',(13.2,35.1439863533772,-14.5472582706722));
#73539=CARTESIAN_POINT('',(21.896707744792,38.9247727484987,-16.5575380560557));
#73540=CARTESIAN_POINT('',(17.5,38.9247727484987,-16.5575380560557));
#73541=CARTESIAN_POINT('',(21.7978078257374,35.0582833660355,-14.501689183981));
#73542=CARTESIAN_POINT('Origin',(21.8,35.1439863533772,-14.5472582706722));
#73543=CARTESIAN_POINT('',(22.6451513366954,39.0211592104439,-16.3290885806033));
#73544=CARTESIAN_POINT('Origin',(9.86169260701006,0.,0.));
#73545=CARTESIAN_POINT('',(22.3997512812625,35.208526188654,-14.357321313938));
#73546=CARTESIAN_POINT('Origin',(22.4,35.2123903820423,-14.359319746515));
#73547=CARTESIAN_POINT('',(23.3381365738089,39.1714230536436,-15.96526278996));
#73548=CARTESIAN_POINT('Origin',(14.1732738814488,0.,0.));
#73549=CARTESIAN_POINT('',(23.1003542130464,35.3548837560077,-13.9863905298622));
#73550=CARTESIAN_POINT('Origin',(23.1,35.3491984393726,-13.9834426982006));
#73551=CARTESIAN_POINT('',(24.1697957402248,39.2644910802189,-15.7349845952073));
#73552=CARTESIAN_POINT('Origin',(8.01433437672606,0.,0.));
#73553=CARTESIAN_POINT('',(24.100209736014,35.4632615954716,-13.7076454228629));
#73554=CARTESIAN_POINT('Origin',(24.1,35.4518044823703,-13.7015349119649));
#73555=CARTESIAN_POINT('',(29.9005519666592,39.1304526938498,-16.0654185122698));
#73556=CARTESIAN_POINT('Origin',(97.7155570771054,0.,0.));
#73557=CARTESIAN_POINT('',(30.4426385593966,35.6800990794245,-14.267645163841));
#73558=CARTESIAN_POINT('Origin',(30.5,35.31499642504,-14.0774119602792));
#73559=CARTESIAN_POINT('',(29.9040600247032,38.9247727484987,-16.5575380560557));
#73560=CARTESIAN_POINT('Origin',(35.8405517186909,0.,0.));
#73561=CARTESIAN_POINT('',(30.5047502791291,35.1138494411902,-14.5312341902212));
#73562=CARTESIAN_POINT('Origin',(30.5,35.1439863533772,-14.5472582706722));
#73563=CARTESIAN_POINT('',(17.5,38.9247727484987,-16.5575380560557));
#73564=CARTESIAN_POINT('Origin',(17.5,40.1718595385976,-14.6213611271724));
#73565=CARTESIAN_POINT('Origin',(17.5,0.,0.));
#73566=CARTESIAN_POINT('',(0.600000000000001,37.2739118462884,-19.9986373454573));
#73567=CARTESIAN_POINT('Origin',(0.600000000000001,0.,0.));
#73568=CARTESIAN_POINT('',(1.67735469196905,37.7041716521717,-19.1751255543105));
#73569=CARTESIAN_POINT('Origin',(8.14497546096349,0.,0.));
#73570=CARTESIAN_POINT('',(5.09593997529677,37.7041716521717,-19.1751255543105));
#73571=CARTESIAN_POINT('',(17.5,37.7041716521717,-19.1751255543105));
#73572=CARTESIAN_POINT('',(5.09944803334083,37.459394730737,-19.6490138787379));
#73573=CARTESIAN_POINT('Origin',(-0.840551718690872,0.,0.));
#73574=CARTESIAN_POINT('',(10.8302042597752,37.2924258787336,-19.9640920674886));
#73575=CARTESIAN_POINT('Origin',(-62.7155570771055,0.,0.));
#73576=CARTESIAN_POINT('',(11.6618634261911,37.4090062358548,-19.7447778525305));
#73577=CARTESIAN_POINT('Origin',(26.9856656232739,0.,0.));
#73578=CARTESIAN_POINT('',(12.3548486633046,37.5911252244478,-19.3958063601357));
#73579=CARTESIAN_POINT('Origin',(20.8267261185512,0.,0.));
#73580=CARTESIAN_POINT('',(13.103292255208,37.7041716521717,-19.1751255543105));
#73581=CARTESIAN_POINT('Origin',(25.13830739299,0.,0.));
#73582=CARTESIAN_POINT('',(21.896707744792,37.7041716521717,-19.1751255543105));
#73583=CARTESIAN_POINT('',(17.5,37.7041716521717,-19.1751255543105));
#73584=CARTESIAN_POINT('',(22.6451513366954,37.5911252244478,-19.3958063601357));
#73585=CARTESIAN_POINT('Origin',(9.86169260701006,0.,0.));
#73586=CARTESIAN_POINT('',(23.3381365738089,37.4090062358548,-19.7447778525305));
#73587=CARTESIAN_POINT('Origin',(14.1732738814488,0.,0.));
#73588=CARTESIAN_POINT('',(24.1697957402248,37.2924258787336,-19.9640920674886));
#73589=CARTESIAN_POINT('Origin',(8.01433437672609,0.,0.));
#73590=CARTESIAN_POINT('',(29.9005519666592,37.459394730737,-19.6490138787379));
#73591=CARTESIAN_POINT('Origin',(97.7155570771054,0.,0.));
#73592=CARTESIAN_POINT('',(29.9040600247032,37.7041716521717,-19.1751255543105));
#73593=CARTESIAN_POINT('Origin',(35.8405517186909,0.,0.));
#73594=CARTESIAN_POINT('',(17.5,37.7041716521717,-19.1751255543105));
#73595=CARTESIAN_POINT('Origin',(33.1,33.7339653438087,-17.5710580837557));
#73596=CARTESIAN_POINT('',(30.5247014514712,33.5694020278342,-17.5045701882916));
#73597=CARTESIAN_POINT('Origin',(30.5,33.7339653438087,-17.5710580837557));
#73598=CARTESIAN_POINT('',(30.4955273645547,33.5136270415661,-18.0163441277467));
#73599=CARTESIAN_POINT('Origin',(30.5,33.4839653438087,-18.0040707856479));
#73600=CARTESIAN_POINT('',(24.1012882089558,33.3579488669236,-18.3802631128034));
#73601=CARTESIAN_POINT('Origin',(24.1,33.2839653438087,-18.3504809471617));
#73602=CARTESIAN_POINT('',(23.1004586919557,33.4416219555226,-18.0938594155378));
#73603=CARTESIAN_POINT('Origin',(23.1,33.4339653438087,-18.0906733260264));
#73604=CARTESIAN_POINT('',(22.399682944576,33.6288475295615,-17.742127215612));
#73605=CARTESIAN_POINT('Origin',(22.4,33.6339653438087,-17.7442631645126));
#73606=CARTESIAN_POINT('',(21.7998387845652,33.7273468611033,-17.5683840431675));
#73607=CARTESIAN_POINT('Origin',(21.8,33.7339653438087,-17.5710580837557));
#73608=CARTESIAN_POINT('',(13.2021921742626,33.6439685797945,-17.5346970308537));
#73609=CARTESIAN_POINT('Origin',(13.2,33.7339653438087,-17.5710580837557));
#73610=CARTESIAN_POINT('',(12.6002487187375,33.6299506000067,-17.7425875883397));
#73611=CARTESIAN_POINT('Origin',(12.6,33.6339653438087,-17.7442631645126));
#73612=CARTESIAN_POINT('',(11.8996457869536,33.4398779649625,-18.0931337015746));
#73613=CARTESIAN_POINT('Origin',(11.9,33.4339653438087,-18.0906733260264));
#73614=CARTESIAN_POINT('',(10.899790263986,33.2960107570711,-18.3553298442931));
#73615=CARTESIAN_POINT('Origin',(10.9,33.2839653438087,-18.3504809471617));
#73616=CARTESIAN_POINT('',(4.55736144060343,33.8643758947959,-18.1614760990067));
#73617=CARTESIAN_POINT('Origin',(4.5,33.4839653438087,-18.0040707856479));
#73618=CARTESIAN_POINT('',(4.49524972087093,33.7023185522751,-17.5582719500126));
#73619=CARTESIAN_POINT('Origin',(4.5,33.7339653438087,-17.5710580837557));
#73620=CARTESIAN_POINT('',(1.90350512467335,33.6714620365851,-17.5458051084359));
#73621=CARTESIAN_POINT('Origin',(1.9,33.7339653438087,-17.5710580837557));
#73622=CARTESIAN_POINT('Ctrl Pts',(0.138207714141623,37.5246765162998,-20.505353736182));
#73623=CARTESIAN_POINT('Ctrl Pts',(0.370217470896568,37.3992864560078,-20.2509844800873));
#73624=CARTESIAN_POINT('Ctrl Pts',(0.600000000000009,37.2739118462884,-19.9986373454573));
#73625=CARTESIAN_POINT('Origin',(1.9,32.0839653438087,-20.4289419162443));
#73626=CARTESIAN_POINT('',(5.09593997529677,35.4582316768749,-23.0652077022745));
#73627=CARTESIAN_POINT('',(17.5,35.4582316768749,-23.0652077022745));
#73628=CARTESIAN_POINT('',(4.47529854852883,31.9441034793054,-20.3196698518115));
#73629=CARTESIAN_POINT('Origin',(4.5,32.0839653438087,-20.4289419162443));
#73630=CARTESIAN_POINT('',(5.09944803334083,35.7462425436685,-22.6162805078382));
#73631=CARTESIAN_POINT('Origin',(-0.840551718690874,0.,0.));
#73632=CARTESIAN_POINT('',(4.50447263544529,32.3594252187343,-20.01548032708));
#73633=CARTESIAN_POINT('Origin',(4.5,32.3339653438087,-19.9959292143521));
#73634=CARTESIAN_POINT('',(10.8302042597752,35.9356238333033,-22.3141421459872));
#73635=CARTESIAN_POINT('Origin',(-62.7155570771054,0.,0.));
#73636=CARTESIAN_POINT('',(10.8987117910442,32.5967492173915,-19.6986995804965));
#73637=CARTESIAN_POINT('Origin',(10.9,32.5339653438087,-19.6495190528383));
#73638=CARTESIAN_POINT('',(11.6618634261911,35.8039823302991,-22.5247608043155));
#73639=CARTESIAN_POINT('Origin',(26.9856656232739,0.,0.));
#73640=CARTESIAN_POINT('',(11.8995413080444,32.3905528841213,-19.9143644494692));
#73641=CARTESIAN_POINT('Origin',(11.9,32.3839653438087,-19.9093266739737));
#73642=CARTESIAN_POINT('',(12.3548486633046,35.5928236469852,-22.856966221146));
#73643=CARTESIAN_POINT('Origin',(20.8267261185512,0.,0.));
#73644=CARTESIAN_POINT('',(12.600317055424,32.179556650676,-20.2523726527879));
#73645=CARTESIAN_POINT('Origin',(12.6,32.1839653438087,-20.2557368354875));
#73646=CARTESIAN_POINT('',(13.103292255208,35.4582316768749,-23.0652077022745));
#73647=CARTESIAN_POINT('Origin',(25.13830739299,0.,0.));
#73648=CARTESIAN_POINT('',(13.2001612154348,32.0783403153759,-20.4245471623811));
#73649=CARTESIAN_POINT('Origin',(13.2,32.0839653438087,-20.4289419162443));
#73650=CARTESIAN_POINT('',(21.896707744792,35.4582316768749,-23.0652077022745));
#73651=CARTESIAN_POINT('',(17.5,35.4582316768749,-23.0652077022745));
#73652=CARTESIAN_POINT('',(21.7978078257374,32.0074773662801,-20.3691829588007));
#73653=CARTESIAN_POINT('Origin',(21.8,32.0839653438087,-20.4289419162443));
#73654=CARTESIAN_POINT('',(22.6451513366954,35.5928236469852,-22.856966221146));
#73655=CARTESIAN_POINT('Origin',(9.86169260701005,0.,0.));
#73656=CARTESIAN_POINT('',(22.3997512812625,32.180506880376,-20.2530977534517));
#73657=CARTESIAN_POINT('Origin',(22.4,32.1839653438087,-20.2557368354875));
#73658=CARTESIAN_POINT('',(23.3381365738089,35.8039823302991,-22.5247608043155));
#73659=CARTESIAN_POINT('Origin',(14.1732738814488,0.,0.));
#73660=CARTESIAN_POINT('',(23.1003542130464,32.3890524021132,-19.9132169663217));
#73661=CARTESIAN_POINT('Origin',(23.1,32.3839653438087,-19.9093266739737));
#73662=CARTESIAN_POINT('',(24.1697957402248,35.9356238333033,-22.3141421459872));
#73663=CARTESIAN_POINT('Origin',(8.01433437672607,0.,0.));
#73664=CARTESIAN_POINT('',(24.100209736014,32.544187318536,-19.657526238157));
#73665=CARTESIAN_POINT('Origin',(24.1,32.5339653438087,-19.6495190528383));
#73666=CARTESIAN_POINT('',(29.9005519666592,35.7462425436685,-22.6162805078382));
#73667=CARTESIAN_POINT('Origin',(97.7155570771054,0.,0.));
#73668=CARTESIAN_POINT('',(30.4426385593966,32.6604876193616,-20.2466717586954));
#73669=CARTESIAN_POINT('Origin',(30.5,32.3339653438087,-19.9959292143521));
#73670=CARTESIAN_POINT('',(29.9040600247032,35.4582316768749,-23.0652077022745));
#73671=CARTESIAN_POINT('Origin',(35.8405517186909,0.,0.));
#73672=CARTESIAN_POINT('',(30.5047502791291,32.0570688314042,-20.4079280576996));
#73673=CARTESIAN_POINT('Origin',(30.5,32.0839653438087,-20.4289419162443));
#73674=CARTESIAN_POINT('',(17.5,35.4582316768749,-23.0652077022745));
#73675=CARTESIAN_POINT('Origin',(17.5,37.0225860117847,-21.375));
#73676=CARTESIAN_POINT('Origin',(17.5,0.,0.));
#73677=CARTESIAN_POINT('',(0.600000000000001,33.234910440458,-26.1673599741116));
#73678=CARTESIAN_POINT('Origin',(0.600000000000001,0.,0.));
#73679=CARTESIAN_POINT('',(1.67735469196904,33.8016349549212,-25.4310730087083));
#73680=CARTESIAN_POINT('Origin',(8.14497546096349,0.,0.));
#73681=CARTESIAN_POINT('',(5.09593997529677,33.8016349549212,-25.4310730087083));
#73682=CARTESIAN_POINT('',(17.5,33.8016349549212,-25.4310730087083));
#73683=CARTESIAN_POINT('',(5.09944803334083,33.4782869009793,-25.8552568383243));
#73684=CARTESIAN_POINT('Origin',(-0.840551718690872,0.,0.));
#73685=CARTESIAN_POINT('',(10.8302042597752,33.2591419277157,-26.1365544445335));
#73686=CARTESIAN_POINT('Origin',(-62.7155570771055,0.,0.));
#73687=CARTESIAN_POINT('',(11.6618634261911,33.4120346810215,-25.9408160718628));
#73688=CARTESIAN_POINT('Origin',(26.9856656232739,0.,0.));
#73689=CARTESIAN_POINT('',(12.3548486633046,33.6519851366708,-25.6287708710599));
#73690=CARTESIAN_POINT('Origin',(20.8267261185512,0.,0.));
#73691=CARTESIAN_POINT('',(13.103292255208,33.8016349549212,-25.4310730087083));
#73692=CARTESIAN_POINT('Origin',(25.13830739299,0.,0.));
#73693=CARTESIAN_POINT('',(21.896707744792,33.8016349549212,-25.4310730087083));
#73694=CARTESIAN_POINT('',(17.5,33.8016349549212,-25.4310730087083));
#73695=CARTESIAN_POINT('',(22.6451513366954,33.6519851366708,-25.6287708710599));
#73696=CARTESIAN_POINT('Origin',(9.86169260701004,0.,0.));
#73697=CARTESIAN_POINT('',(23.3381365738089,33.4120346810215,-25.9408160718628));
#73698=CARTESIAN_POINT('Origin',(14.1732738814488,0.,0.));
#73699=CARTESIAN_POINT('',(24.1697957402248,33.2591419277157,-26.1365544445335));
#73700=CARTESIAN_POINT('Origin',(8.01433437672609,0.,0.));
#73701=CARTESIAN_POINT('',(29.9005519666592,33.4782869009793,-25.8552568383243));
#73702=CARTESIAN_POINT('Origin',(97.7155570771054,0.,0.));
#73703=CARTESIAN_POINT('',(29.9040600247032,33.8016349549212,-25.4310730087083));
#73704=CARTESIAN_POINT('Origin',(35.8405517186909,0.,0.));
#73705=CARTESIAN_POINT('',(17.5,33.8016349549212,-25.4310730087083));
#73706=CARTESIAN_POINT('Origin',(33.1,30.1702883945039,-23.1619558369422));
#73707=CARTESIAN_POINT('',(30.5247014514712,30.0197706669552,-23.0679019220779));
#73708=CARTESIAN_POINT('Origin',(30.5,30.1702883945039,-23.1619558369422));
#73709=CARTESIAN_POINT('',(30.4955273645547,29.8759744160903,-23.562215640718));
#73710=CARTESIAN_POINT('Origin',(30.5,29.8488945896607,-23.5449780585017));
#73711=CARTESIAN_POINT('',(24.1012882089558,29.6594674741542,-23.893572647341));
#73712=CARTESIAN_POINT('Origin',(24.1,29.5917795457861,-23.8513958357493));
#73713=CARTESIAN_POINT('',(23.1004586919557,29.7916028606322,-23.6260497451375));
#73714=CARTESIAN_POINT('Origin',(23.1,29.784615828692,-23.6215825028136));
#73715=CARTESIAN_POINT('',(22.399682944576,30.0370617130518,-23.3121725274111));
#73716=CARTESIAN_POINT('Origin',(22.4,30.0417308725666,-23.315164725566));
#73717=CARTESIAN_POINT('',(21.7998387845652,30.1642348036977,-23.1581731335784));
#73718=CARTESIAN_POINT('Origin',(21.8,30.1702883945039,-23.1619558369422));
#73719=CARTESIAN_POINT('',(13.2021921742626,30.0879729141313,-23.1105194160696));
#73720=CARTESIAN_POINT('Origin',(13.2,30.1702883945039,-23.1619558369422));
#73721=CARTESIAN_POINT('',(12.6002487187375,30.038068082493,-23.3128174522151));
#73722=CARTESIAN_POINT('Origin',(12.6,30.0417308725666,-23.315164725566));
#73723=CARTESIAN_POINT('',(11.8996457869536,29.7900113841146,-23.6250322156174));
#73724=CARTESIAN_POINT('Origin',(11.9,29.784615828692,-23.6215825028136));
#73725=CARTESIAN_POINT('',(10.899790263986,29.6027999600046,-23.8582627313001));
#73726=CARTESIAN_POINT('Origin',(10.9,29.5917795457861,-23.8513958357493));
#73727=CARTESIAN_POINT('',(4.55736144060343,30.1961927037808,-23.7660496304069));
#73728=CARTESIAN_POINT('Origin',(4.5,29.8488945896607,-23.5449780585017));
#73729=CARTESIAN_POINT('',(4.49524972087093,30.1413426776676,-23.1438685456221));
#73730=CARTESIAN_POINT('Origin',(4.5,30.1702883945039,-23.1619558369422));
#73731=CARTESIAN_POINT('',(1.90350512467335,30.1131197861062,-23.1262329256631));
#73732=CARTESIAN_POINT('Origin',(1.9,30.1702883945039,-23.1619558369422));
#73733=CARTESIAN_POINT('Ctrl Pts',(0.138207714141626,33.3938750538235,-26.7099230322464));
#73734=CARTESIAN_POINT('Ctrl Pts',(0.370217470894619,33.3145607080732,-26.4376444612514));
#73735=CARTESIAN_POINT('Ctrl Pts',(0.600000000000007,33.234910440458,-26.1673599741116));
#73736=CARTESIAN_POINT('Origin',(1.9,28.0490892825384,-25.6899024992348));
#73737=CARTESIAN_POINT('',(5.09593997529677,30.9143101784803,-28.872052684018));
#73738=CARTESIAN_POINT('',(17.5,30.9143101784803,-28.872052684018));
#73739=CARTESIAN_POINT('',(4.47529854852883,27.9303271288835,-25.5580037650976));
#73740=CARTESIAN_POINT('Origin',(4.5,28.0490892825384,-25.6899024992348));
#73741=CARTESIAN_POINT('',(5.09944803334083,31.2759009022694,-28.4799582645661));
#73742=CARTESIAN_POINT('Origin',(-0.840551718690874,0.,0.));
#73743=CARTESIAN_POINT('',(4.50447263544529,28.3921611545025,-25.3305554259542));
#73744=CARTESIAN_POINT('Origin',(4.5,28.3704830873816,-25.3068802776753));
#73745=CARTESIAN_POINT('',(10.8302042597752,31.5148708405159,-28.2152957791621));
#73746=CARTESIAN_POINT('Origin',(-62.7155570771054,0.,0.));
#73747=CARTESIAN_POINT('',(10.8987117910442,28.6808880677203,-25.0597981705973));
#73748=CARTESIAN_POINT('Origin',(10.9,28.6275981312562,-25.0004625004277));
#73749=CARTESIAN_POINT('',(11.6618634261911,31.3486557215378,-28.3998553597108));
#73750=CARTESIAN_POINT('Origin',(26.9856656232739,0.,0.));
#73751=CARTESIAN_POINT('',(11.8995413080444,28.4403745085892,-25.2363809880999));
#73752=CARTESIAN_POINT('Origin',(11.9,28.4347618483503,-25.2302758333634));
#73753=CARTESIAN_POINT('',(12.3548486633046,31.0830181478507,-28.6903465092421));
#73754=CARTESIAN_POINT('Origin',(20.8267261185512,0.,0.));
#73755=CARTESIAN_POINT('',(12.600317055424,28.1738892734931,-25.5326149758776));
#73756=CARTESIAN_POINT('Origin',(12.6,28.1776468044757,-25.536693610611));
#73757=CARTESIAN_POINT('',(13.103292255208,30.9143101784803,-28.872052684018));
#73758=CARTESIAN_POINT('Origin',(25.13830739299,0.,0.));
#73759=CARTESIAN_POINT('',(13.2001612154348,28.0443128519265,-25.684597735621));
#73760=CARTESIAN_POINT('Origin',(13.2,28.0490892825384,-25.6899024992348));
#73761=CARTESIAN_POINT('',(21.896707744792,30.9143101784803,-28.872052684018));
#73762=CARTESIAN_POINT('',(17.5,30.9143101784803,-28.872052684018));
#73763=CARTESIAN_POINT('',(21.7978078257374,27.9841403633154,-25.6177694167212));
#73764=CARTESIAN_POINT('Origin',(21.8,28.0490892825384,-25.6899024992348));
#73765=CARTESIAN_POINT('',(22.6451513366954,31.0830181478507,-28.6903465092421));
#73766=CARTESIAN_POINT('Origin',(9.86169260701004,0.,0.));
#73767=CARTESIAN_POINT('',(22.3997512812625,28.1746991546599,-25.5334940662887));
#73768=CARTESIAN_POINT('Origin',(22.4,28.1776468044757,-25.536693610611));
#73769=CARTESIAN_POINT('',(23.3381365738089,31.3486557215378,-28.3998553597108));
#73770=CARTESIAN_POINT('Origin',(14.1732738814488,0.,0.));
#73771=CARTESIAN_POINT('',(23.1003542130464,28.4390960806318,-25.2349903818335));
#73772=CARTESIAN_POINT('Origin',(23.1,28.4347618483503,-25.2302758333634));
#73773=CARTESIAN_POINT('',(24.1697957402248,31.5148708405159,-28.2152957791621));
#73774=CARTESIAN_POINT('Origin',(8.01433437672607,0.,0.));
#73775=CARTESIAN_POINT('',(24.100209736014,28.63627437808,-25.0101230658929));
#73776=CARTESIAN_POINT('Origin',(24.1,28.6275981312562,-25.0004625004277));
#73777=CARTESIAN_POINT('',(29.9005519666592,31.2759009022694,-28.4799582645661));
#73778=CARTESIAN_POINT('Origin',(97.7155570771054,0.,0.));
#73779=CARTESIAN_POINT('',(30.4426385593966,28.6485037699886,-25.610513477472));
#73780=CARTESIAN_POINT('Origin',(30.5,28.3704830873816,-25.3068802776753));
#73781=CARTESIAN_POINT('',(29.9040600247032,30.9143101784803,-28.872052684018));
#73782=CARTESIAN_POINT('Origin',(35.8405517186909,0.,0.));
#73783=CARTESIAN_POINT('',(30.5047502791291,28.0262504068355,-25.6645373580546));
#73784=CARTESIAN_POINT('Origin',(30.5,28.0490892825384,-25.6899024992348));
#73785=CARTESIAN_POINT('',(17.5,30.9143101784803,-28.872052684018));
#73786=CARTESIAN_POINT('Origin',(17.5,32.7483999433363,-27.4791703140996));
#73787=CARTESIAN_POINT('Origin',(17.5,0.,0.));
#73788=CARTESIAN_POINT('',(0.600000000000001,28.1860830985703,-31.5410006112756));
#73789=CARTESIAN_POINT('Origin',(0.600000000000001,0.,0.));
#73790=CARTESIAN_POINT('',(1.67735469196904,28.872052684018,-30.9143101784803));
#73791=CARTESIAN_POINT('Origin',(8.14497546096349,0.,0.));
#73792=CARTESIAN_POINT('',(5.09593997529677,28.872052684018,-30.9143101784803));
#73793=CARTESIAN_POINT('',(17.5,28.872052684018,-30.9143101784803));
#73794=CARTESIAN_POINT('',(5.09944803334083,28.4799582645661,-31.2759009022694));
#73795=CARTESIAN_POINT('Origin',(-0.840551718690872,0.,0.));
#73796=CARTESIAN_POINT('',(10.8302042597752,28.2152957791621,-31.5148708405159));
#73797=CARTESIAN_POINT('Origin',(-62.7155570771055,0.,0.));
#73798=CARTESIAN_POINT('',(11.6618634261911,28.3998553597108,-31.3486557215378));
#73799=CARTESIAN_POINT('Origin',(26.9856656232739,0.,0.));
#73800=CARTESIAN_POINT('',(12.3548486633046,28.6903465092421,-31.0830181478507));
#73801=CARTESIAN_POINT('Origin',(20.8267261185512,0.,0.));
#73802=CARTESIAN_POINT('',(13.103292255208,28.872052684018,-30.9143101784803));
#73803=CARTESIAN_POINT('Origin',(25.13830739299,0.,0.));
#73804=CARTESIAN_POINT('',(21.896707744792,28.872052684018,-30.9143101784803));
#73805=CARTESIAN_POINT('',(17.5,28.872052684018,-30.9143101784803));
#73806=CARTESIAN_POINT('',(22.6451513366954,28.6903465092421,-31.0830181478507));
#73807=CARTESIAN_POINT('Origin',(9.86169260701007,0.,0.));
#73808=CARTESIAN_POINT('',(23.3381365738089,28.3998553597108,-31.3486557215378));
#73809=CARTESIAN_POINT('Origin',(14.1732738814488,0.,0.));
#73810=CARTESIAN_POINT('',(24.1697957402248,28.2152957791621,-31.5148708405159));
#73811=CARTESIAN_POINT('Origin',(8.01433437672609,0.,0.));
#73812=CARTESIAN_POINT('',(29.9005519666592,28.4799582645661,-31.2759009022694));
#73813=CARTESIAN_POINT('Origin',(97.7155570771054,0.,0.));
#73814=CARTESIAN_POINT('',(29.9040600247032,28.872052684018,-30.9143101784803));
#73815=CARTESIAN_POINT('Origin',(35.8405517186909,0.,0.));
#73816=CARTESIAN_POINT('',(17.5,28.872052684018,-30.9143101784803));
#73817=CARTESIAN_POINT('Origin',(33.1,25.6899024992348,-28.0490892825384));
#73818=CARTESIAN_POINT('',(30.5247014514712,25.5580037650976,-27.9303271288835));
#73819=CARTESIAN_POINT('Origin',(30.5,25.6899024992348,-28.0490892825384));
#73820=CARTESIAN_POINT('',(30.4955273645547,25.3305554259542,-28.3921611545025));
#73821=CARTESIAN_POINT('Origin',(30.5,25.3068802776753,-28.3704830873817));
#73822=CARTESIAN_POINT('',(24.1012882089558,25.0597981705973,-28.6808880677203));
#73823=CARTESIAN_POINT('Origin',(24.1,25.0004625004277,-28.6275981312563));
#73824=CARTESIAN_POINT('',(23.1004586919557,25.2363809880999,-28.4403745085892));
#73825=CARTESIAN_POINT('Origin',(23.1,25.2302758333634,-28.4347618483503));
#73826=CARTESIAN_POINT('',(22.399682944576,25.5326149758775,-28.1738892734932));
#73827=CARTESIAN_POINT('Origin',(22.4,25.536693610611,-28.1776468044757));
#73828=CARTESIAN_POINT('',(21.7998387845652,25.684597735621,-28.0443128519265));
#73829=CARTESIAN_POINT('Origin',(21.8,25.6899024992348,-28.0490892825384));
#73830=CARTESIAN_POINT('',(13.2021921742626,25.6177694167211,-27.9841403633154));
#73831=CARTESIAN_POINT('Origin',(13.2,25.6899024992348,-28.0490892825384));
#73832=CARTESIAN_POINT('',(12.6002487187375,25.5334940662887,-28.1746991546599));
#73833=CARTESIAN_POINT('Origin',(12.6,25.536693610611,-28.1776468044757));
#73834=CARTESIAN_POINT('',(11.8996457869536,25.2349903818335,-28.4390960806318));
#73835=CARTESIAN_POINT('Origin',(11.9,25.2302758333634,-28.4347618483503));
#73836=CARTESIAN_POINT('',(10.899790263986,25.0101230658929,-28.63627437808));
#73837=CARTESIAN_POINT('Origin',(10.9,25.0004625004277,-28.6275981312563));
#73838=CARTESIAN_POINT('',(4.55736144060343,25.610513477472,-28.6485037699886));
#73839=CARTESIAN_POINT('Origin',(4.5,25.3068802776753,-28.3704830873817));
#73840=CARTESIAN_POINT('',(4.49524972087093,25.6645373580546,-28.0262504068355));
#73841=CARTESIAN_POINT('Origin',(4.5,25.6899024992348,-28.0490892825384));
#73842=CARTESIAN_POINT('',(1.90350512467335,25.6398056289004,-28.0039818578826));
#73843=CARTESIAN_POINT('Origin',(1.9,25.6899024992348,-28.0490892825384));
#73844=CARTESIAN_POINT('Ctrl Pts',(0.138207714141627,28.2484175959528,-32.1029248328492));
#73845=CARTESIAN_POINT('Ctrl Pts',(0.370217470896185,28.2175888910037,-31.82100999355));
#73846=CARTESIAN_POINT('Ctrl Pts',(0.600000000000008,28.1860830985703,-31.5410006112756));
#73847=CARTESIAN_POINT('Origin',(1.9,23.1619558369422,-30.170288394504));
#73848=CARTESIAN_POINT('',(5.09593997529677,25.4310730087083,-33.8016349549212));
#73849=CARTESIAN_POINT('',(17.5,25.4310730087083,-33.8016349549212));
#73850=CARTESIAN_POINT('',(4.47529854852883,23.0679019220779,-30.0197706669552));
#73851=CARTESIAN_POINT('Origin',(4.5,23.1619558369422,-30.170288394504));
#73852=CARTESIAN_POINT('',(5.09944803334083,25.8552568383243,-33.4782869009794));
#73853=CARTESIAN_POINT('Origin',(-0.840551718690874,0.,0.));
#73854=CARTESIAN_POINT('',(4.50447263544529,23.562215640718,-29.8759744160904));
#73855=CARTESIAN_POINT('Origin',(4.5,23.5449780585017,-29.8488945896607));
#73856=CARTESIAN_POINT('',(10.8302042597752,26.1365544445334,-33.2591419277157));
#73857=CARTESIAN_POINT('Origin',(-62.7155570771056,0.,0.));
#73858=CARTESIAN_POINT('',(10.8987117910442,23.893572647341,-29.6594674741542));
#73859=CARTESIAN_POINT('Origin',(10.9,23.8513958357493,-29.5917795457861));
#73860=CARTESIAN_POINT('',(11.6618634261911,25.9408160718628,-33.4120346810215));
#73861=CARTESIAN_POINT('Origin',(26.9856656232739,0.,0.));
#73862=CARTESIAN_POINT('',(11.8995413080444,23.6260497451375,-29.7916028606322));
#73863=CARTESIAN_POINT('Origin',(11.9,23.6215825028136,-29.784615828692));
#73864=CARTESIAN_POINT('',(12.3548486633046,25.6287708710599,-33.6519851366708));
#73865=CARTESIAN_POINT('Origin',(20.8267261185512,0.,0.));
#73866=CARTESIAN_POINT('',(12.600317055424,23.312172527411,-30.0370617130518));
#73867=CARTESIAN_POINT('Origin',(12.6,23.315164725566,-30.0417308725667));
#73868=CARTESIAN_POINT('',(13.103292255208,25.4310730087083,-33.8016349549212));
#73869=CARTESIAN_POINT('Origin',(25.13830739299,0.,0.));
#73870=CARTESIAN_POINT('',(13.2001612154348,23.1581731335784,-30.1642348036977));
#73871=CARTESIAN_POINT('Origin',(13.2,23.1619558369422,-30.170288394504));
#73872=CARTESIAN_POINT('',(21.896707744792,25.4310730087083,-33.8016349549212));
#73873=CARTESIAN_POINT('',(17.5,25.4310730087083,-33.8016349549212));
#73874=CARTESIAN_POINT('',(21.7978078257374,23.1105194160696,-30.0879729141313));
#73875=CARTESIAN_POINT('Origin',(21.8,23.1619558369422,-30.170288394504));
#73876=CARTESIAN_POINT('',(22.6451513366954,25.6287708710599,-33.6519851366708));
#73877=CARTESIAN_POINT('Origin',(9.86169260701005,0.,0.));
#73878=CARTESIAN_POINT('',(22.3997512812625,23.3128174522151,-30.0380680824931));
#73879=CARTESIAN_POINT('Origin',(22.4,23.315164725566,-30.0417308725667));
#73880=CARTESIAN_POINT('',(23.3381365738089,25.9408160718628,-33.4120346810215));
#73881=CARTESIAN_POINT('Origin',(14.1732738814488,0.,0.));
#73882=CARTESIAN_POINT('',(23.1003542130464,23.6250322156174,-29.7900113841146));
#73883=CARTESIAN_POINT('Origin',(23.1,23.6215825028136,-29.784615828692));
#73884=CARTESIAN_POINT('',(24.1697957402248,26.1365544445334,-33.2591419277157));
#73885=CARTESIAN_POINT('Origin',(8.01433437672607,0.,0.));
#73886=CARTESIAN_POINT('',(24.100209736014,23.8582627313001,-29.6027999600046));
#73887=CARTESIAN_POINT('Origin',(24.1,23.8513958357493,-29.5917795457861));
#73888=CARTESIAN_POINT('',(29.9005519666592,25.8552568383243,-33.4782869009794));
#73889=CARTESIAN_POINT('Origin',(97.7155570771055,0.,0.));
#73890=CARTESIAN_POINT('',(30.4426385593966,23.7660496304069,-30.1961927037808));
#73891=CARTESIAN_POINT('Origin',(30.5,23.5449780585017,-29.8488945896607));
#73892=CARTESIAN_POINT('',(29.9040600247032,25.4310730087083,-33.8016349549212));
#73893=CARTESIAN_POINT('Origin',(35.8405517186909,0.,0.));
#73894=CARTESIAN_POINT('',(30.5047502791291,23.1438685456221,-30.1413426776677));
#73895=CARTESIAN_POINT('Origin',(30.5,23.1619558369422,-30.170288394504));
#73896=CARTESIAN_POINT('',(17.5,25.4310730087083,-33.8016349549212));
#73897=CARTESIAN_POINT('Origin',(17.5,27.4791703140995,-32.7483999433363));
#73898=CARTESIAN_POINT('Origin',(17.5,0.,0.));
#73899=CARTESIAN_POINT('',(0.600000000000001,22.2808358845789,-35.9562839053824));
#73900=CARTESIAN_POINT('Origin',(0.600000000000001,0.,0.));
#73901=CARTESIAN_POINT('',(1.67735469196904,23.0652077022745,-35.4582316768749));
#73902=CARTESIAN_POINT('Origin',(8.14497546096349,0.,0.));
#73903=CARTESIAN_POINT('',(5.09593997529677,23.0652077022745,-35.4582316768749));
#73904=CARTESIAN_POINT('',(17.5,23.0652077022745,-35.4582316768749));
#73905=CARTESIAN_POINT('',(5.09944803334083,22.6162805078382,-35.7462425436685));
#73906=CARTESIAN_POINT('Origin',(-0.840551718690872,0.,0.));
#73907=CARTESIAN_POINT('',(10.8302042597752,22.3141421459872,-35.9356238333033));
#73908=CARTESIAN_POINT('Origin',(-62.7155570771055,0.,0.));
#73909=CARTESIAN_POINT('',(11.6618634261911,22.5247608043155,-35.8039823302991));
#73910=CARTESIAN_POINT('Origin',(26.9856656232739,0.,0.));
#73911=CARTESIAN_POINT('',(12.3548486633046,22.856966221146,-35.5928236469852));
#73912=CARTESIAN_POINT('Origin',(20.8267261185512,0.,0.));
#73913=CARTESIAN_POINT('',(13.103292255208,23.0652077022745,-35.4582316768749));
#73914=CARTESIAN_POINT('Origin',(25.13830739299,0.,0.));
#73915=CARTESIAN_POINT('',(21.896707744792,23.0652077022745,-35.4582316768749));
#73916=CARTESIAN_POINT('',(17.5,23.0652077022745,-35.4582316768749));
#73917=CARTESIAN_POINT('',(22.6451513366954,22.856966221146,-35.5928236469852));
#73918=CARTESIAN_POINT('Origin',(9.86169260701005,0.,0.));
#73919=CARTESIAN_POINT('',(23.3381365738089,22.5247608043155,-35.8039823302992));
#73920=CARTESIAN_POINT('Origin',(14.1732738814488,0.,0.));
#73921=CARTESIAN_POINT('',(24.1697957402248,22.3141421459872,-35.9356238333033));
#73922=CARTESIAN_POINT('Origin',(8.01433437672609,0.,0.));
#73923=CARTESIAN_POINT('',(29.9005519666592,22.6162805078382,-35.7462425436685));
#73924=CARTESIAN_POINT('Origin',(97.7155570771054,0.,0.));
#73925=CARTESIAN_POINT('',(29.9040600247032,23.0652077022745,-35.4582316768749));
#73926=CARTESIAN_POINT('Origin',(35.8405517186909,0.,0.));
#73927=CARTESIAN_POINT('',(17.5,23.0652077022745,-35.4582316768749));
#73928=CARTESIAN_POINT('Origin',(33.1,20.4289419162443,-32.0839653438087));
#73929=CARTESIAN_POINT('',(30.5247014514712,20.3196698518115,-31.9441034793054));
#73930=CARTESIAN_POINT('Origin',(30.5,20.4289419162443,-32.0839653438087));
#73931=CARTESIAN_POINT('',(30.4955273645547,20.01548032708,-32.3594252187343));
#73932=CARTESIAN_POINT('Origin',(30.5,19.9959292143521,-32.3339653438087));
#73933=CARTESIAN_POINT('',(24.1012882089558,19.6986995804965,-32.5967492173916));
#73934=CARTESIAN_POINT('Origin',(24.1,19.6495190528383,-32.5339653438087));
#73935=CARTESIAN_POINT('',(23.1004586919557,19.9143644494692,-32.3905528841213));
#73936=CARTESIAN_POINT('Origin',(23.1,19.9093266739737,-32.3839653438087));
#73937=CARTESIAN_POINT('',(22.399682944576,20.2523726527879,-32.1795566506761));
#73938=CARTESIAN_POINT('Origin',(22.4,20.2557368354874,-32.1839653438087));
#73939=CARTESIAN_POINT('',(21.7998387845652,20.4245471623811,-32.0783403153759));
#73940=CARTESIAN_POINT('Origin',(21.8,20.4289419162443,-32.0839653438087));
#73941=CARTESIAN_POINT('',(13.2021921742626,20.3691829588007,-32.0074773662801));
#73942=CARTESIAN_POINT('Origin',(13.2,20.4289419162443,-32.0839653438087));
#73943=CARTESIAN_POINT('',(12.6002487187375,20.2530977534517,-32.180506880376));
#73944=CARTESIAN_POINT('Origin',(12.6,20.2557368354874,-32.1839653438087));
#73945=CARTESIAN_POINT('',(11.8996457869536,19.9132169663217,-32.3890524021132));
#73946=CARTESIAN_POINT('Origin',(11.9,19.9093266739737,-32.3839653438087));
#73947=CARTESIAN_POINT('',(10.899790263986,19.657526238157,-32.544187318536));
#73948=CARTESIAN_POINT('Origin',(10.9,19.6495190528383,-32.5339653438087));
#73949=CARTESIAN_POINT('',(4.55736144060343,20.2466717586954,-32.6604876193617));
#73950=CARTESIAN_POINT('Origin',(4.5,19.9959292143521,-32.3339653438087));
#73951=CARTESIAN_POINT('',(4.49524972087093,20.4079280576996,-32.0570688314042));
#73952=CARTESIAN_POINT('Origin',(4.5,20.4289419162443,-32.0839653438087));
#73953=CARTESIAN_POINT('',(1.90350512467335,20.3874389520281,-32.0308439720488));
#73954=CARTESIAN_POINT('Origin',(1.9,20.4289419162443,-32.0839653438087));
#73955=CARTESIAN_POINT('Ctrl Pts',(0.138207714141627,22.2446462638181,-36.5204955072696));
#73956=CARTESIAN_POINT('Ctrl Pts',(0.370217470898034,22.2632399142706,-36.2375102394021));
#73957=CARTESIAN_POINT('Ctrl Pts',(0.600000000000007,22.2808358845789,-35.9562839053824));
#73958=CARTESIAN_POINT('Origin',(1.9,17.5710580837557,-33.7339653438087));
#73959=CARTESIAN_POINT('',(5.09593997529677,19.1751255543105,-37.7041716521717));
#73960=CARTESIAN_POINT('',(17.5,19.1751255543105,-37.7041716521717));
#73961=CARTESIAN_POINT('',(4.47529854852883,17.5045701882916,-33.5694020278343));
#73962=CARTESIAN_POINT('Origin',(4.5,17.5710580837557,-33.7339653438087));
#73963=CARTESIAN_POINT('',(5.09944803334083,19.6490138787379,-37.459394730737));
#73964=CARTESIAN_POINT('Origin',(-0.840551718690874,0.,0.));
#73965=CARTESIAN_POINT('',(4.50447263544529,18.0163441277467,-33.5136270415661));
#73966=CARTESIAN_POINT('Origin',(4.5,18.0040707856479,-33.4839653438087));
#73967=CARTESIAN_POINT('',(10.8302042597752,19.9640920674886,-37.2924258787336));
#73968=CARTESIAN_POINT('Origin',(-62.7155570771054,0.,0.));
#73969=CARTESIAN_POINT('',(10.8987117910442,18.3802631128034,-33.3579488669236));
#73970=CARTESIAN_POINT('Origin',(10.9,18.3504809471617,-33.2839653438087));
#73971=CARTESIAN_POINT('',(11.6618634261911,19.7447778525305,-37.4090062358548));
#73972=CARTESIAN_POINT('Origin',(26.9856656232739,0.,0.));
#73973=CARTESIAN_POINT('',(11.8995413080444,18.0938594155378,-33.4416219555226));
#73974=CARTESIAN_POINT('Origin',(11.9,18.0906733260263,-33.4339653438087));
#73975=CARTESIAN_POINT('',(12.3548486633046,19.3958063601357,-37.5911252244478));
#73976=CARTESIAN_POINT('Origin',(20.8267261185512,0.,0.));
#73977=CARTESIAN_POINT('',(12.600317055424,17.742127215612,-33.6288475295615));
#73978=CARTESIAN_POINT('Origin',(12.6,17.7442631645126,-33.6339653438087));
#73979=CARTESIAN_POINT('',(13.103292255208,19.1751255543105,-37.7041716521717));
#73980=CARTESIAN_POINT('Origin',(25.13830739299,0.,0.));
#73981=CARTESIAN_POINT('',(13.2001612154348,17.5683840431675,-33.7273468611033));
#73982=CARTESIAN_POINT('Origin',(13.2,17.5710580837557,-33.7339653438087));
#73983=CARTESIAN_POINT('',(21.896707744792,19.1751255543105,-37.7041716521717));
#73984=CARTESIAN_POINT('',(17.5,19.1751255543105,-37.7041716521717));
#73985=CARTESIAN_POINT('',(21.7978078257374,17.5346970308537,-33.6439685797945));
#73986=CARTESIAN_POINT('Origin',(21.8,17.5710580837557,-33.7339653438087));
#73987=CARTESIAN_POINT('',(22.6451513366954,19.3958063601357,-37.5911252244478));
#73988=CARTESIAN_POINT('Origin',(9.86169260701005,0.,0.));
#73989=CARTESIAN_POINT('',(22.3997512812625,17.7425875883397,-33.6299506000067));
#73990=CARTESIAN_POINT('Origin',(22.4,17.7442631645126,-33.6339653438087));
#73991=CARTESIAN_POINT('',(23.3381365738089,19.7447778525305,-37.4090062358548));
#73992=CARTESIAN_POINT('Origin',(14.1732738814488,0.,0.));
#73993=CARTESIAN_POINT('',(23.1003542130464,18.0931337015746,-33.4398779649625));
#73994=CARTESIAN_POINT('Origin',(23.1,18.0906733260263,-33.4339653438087));
#73995=CARTESIAN_POINT('',(24.1697957402248,19.9640920674886,-37.2924258787336));
#73996=CARTESIAN_POINT('Origin',(8.01433437672608,0.,0.));
#73997=CARTESIAN_POINT('',(24.100209736014,18.3553298442931,-33.2960107570711));
#73998=CARTESIAN_POINT('Origin',(24.1,18.3504809471617,-33.2839653438087));
#73999=CARTESIAN_POINT('',(29.9005519666592,19.6490138787379,-37.459394730737));
#74000=CARTESIAN_POINT('Origin',(97.7155570771054,0.,0.));
#74001=CARTESIAN_POINT('',(30.4426385593966,18.1614760990067,-33.864375894796));
#74002=CARTESIAN_POINT('Origin',(30.5,18.0040707856479,-33.4839653438087));
#74003=CARTESIAN_POINT('',(29.9040600247032,19.1751255543105,-37.7041716521717));
#74004=CARTESIAN_POINT('Origin',(35.8405517186909,0.,0.));
#74005=CARTESIAN_POINT('',(30.5047502791291,17.5582719500126,-33.7023185522751));
#74006=CARTESIAN_POINT('Origin',(30.5,17.5710580837557,-33.7339653438087));
#74007=CARTESIAN_POINT('',(17.5,19.1751255543105,-37.7041716521717));
#74008=CARTESIAN_POINT('Origin',(17.5,21.375,-37.0225860117847));
#74009=CARTESIAN_POINT('Origin',(17.5,0.,0.));
#74010=CARTESIAN_POINT('',(0.600000000000001,15.6985967468814,-39.2790537077817));
#74011=CARTESIAN_POINT('Origin',(0.600000000000001,0.,0.));
#74012=CARTESIAN_POINT('',(1.67735469196904,16.5575380560557,-38.9247727484987));
#74013=CARTESIAN_POINT('Origin',(8.14497546096349,0.,0.));
#74014=CARTESIAN_POINT('',(5.09593997529677,16.5575380560557,-38.9247727484987));
#74015=CARTESIAN_POINT('',(17.5,16.5575380560557,-38.9247727484987));
#74016=CARTESIAN_POINT('',(5.09944803334083,16.0654185122698,-39.1304526938498));
#74017=CARTESIAN_POINT('Origin',(-0.840551718690872,0.,0.));
#74018=CARTESIAN_POINT('',(10.8302042597752,15.7349845952072,-39.2644910802189));
#74019=CARTESIAN_POINT('Origin',(-62.7155570771055,0.,0.));
#74020=CARTESIAN_POINT('',(11.6618634261911,15.9652627899599,-39.1714230536436));
#74021=CARTESIAN_POINT('Origin',(26.9856656232739,0.,0.));
#74022=CARTESIAN_POINT('',(12.3548486633046,16.3290885806033,-39.0211592104439));
#74023=CARTESIAN_POINT('Origin',(20.8267261185512,0.,0.));
#74024=CARTESIAN_POINT('',(13.103292255208,16.5575380560557,-38.9247727484987));
#74025=CARTESIAN_POINT('Origin',(25.13830739299,0.,0.));
#74026=CARTESIAN_POINT('',(21.896707744792,16.5575380560557,-38.9247727484987));
#74027=CARTESIAN_POINT('',(17.5,16.5575380560557,-38.9247727484987));
#74028=CARTESIAN_POINT('',(22.6451513366954,16.3290885806033,-39.0211592104439));
#74029=CARTESIAN_POINT('Origin',(9.86169260701006,0.,0.));
#74030=CARTESIAN_POINT('',(23.3381365738089,15.9652627899599,-39.1714230536436));
#74031=CARTESIAN_POINT('Origin',(14.1732738814488,0.,0.));
#74032=CARTESIAN_POINT('',(24.1697957402248,15.7349845952072,-39.2644910802189));
#74033=CARTESIAN_POINT('Origin',(8.01433437672609,0.,0.));
#74034=CARTESIAN_POINT('',(29.9005519666592,16.0654185122698,-39.1304526938498));
#74035=CARTESIAN_POINT('Origin',(97.7155570771054,0.,0.));
#74036=CARTESIAN_POINT('',(29.9040600247032,16.5575380560557,-38.9247727484987));
#74037=CARTESIAN_POINT('Origin',(35.8405517186909,0.,0.));
#74038=CARTESIAN_POINT('',(17.5,16.5575380560557,-38.9247727484987));
#74039=CARTESIAN_POINT('Origin',(33.1,14.5472582706721,-35.1439863533772));
#74040=CARTESIAN_POINT('',(30.5247014514712,14.4639330523271,-34.987274410005));
#74041=CARTESIAN_POINT('Origin',(30.5,14.5472582706721,-35.1439863533772));
#74042=CARTESIAN_POINT('',(30.4955273645547,14.0922449867892,-35.343464522354));
#74043=CARTESIAN_POINT('Origin',(30.5,14.0774119602792,-35.31499642504));
#74044=CARTESIAN_POINT('',(24.1012882089558,13.7390659716653,-35.5221746368434));
#74045=CARTESIAN_POINT('Origin',(24.1,13.7015349119648,-35.4518044823703));
#74046=CARTESIAN_POINT('',(23.1004586919557,13.9872600241959,-35.35656070068));
#74047=CARTESIAN_POINT('Origin',(23.1,13.9834426982006,-35.3491984393726));
#74048=CARTESIAN_POINT('',(22.399682944576,14.3567722348382,-35.2074644826695));
#74049=CARTESIAN_POINT('Origin',(22.4,14.359319746515,-35.2123903820423));
#74050=CARTESIAN_POINT('',(21.7998387845652,14.5439070589317,-35.137683640766));
#74051=CARTESIAN_POINT('Origin',(21.8,14.5472582706721,-35.1439863533772));
#74052=CARTESIAN_POINT('',(13.2021921742626,14.501689183981,-35.0582833660355));
#74053=CARTESIAN_POINT('Origin',(13.2,14.5472582706721,-35.1439863533772));
#74054=CARTESIAN_POINT('',(12.6002487187375,14.3573213139379,-35.208526188654));
#74055=CARTESIAN_POINT('Origin',(12.6,14.359319746515,-35.2123903820423));
#74056=CARTESIAN_POINT('',(11.8996457869536,13.9863905298622,-35.3548837560077));
#74057=CARTESIAN_POINT('Origin',(11.9,13.9834426982006,-35.3491984393726));
#74058=CARTESIAN_POINT('',(10.899790263986,13.7076454228628,-35.4632615954717));
#74059=CARTESIAN_POINT('Origin',(10.9,13.7015349119648,-35.4518044823703));
#74060=CARTESIAN_POINT('',(4.55736144060343,14.267645163841,-35.6800990794246));
#74061=CARTESIAN_POINT('Origin',(4.5,14.0774119602792,-35.31499642504));
#74062=CARTESIAN_POINT('',(4.49524972087093,14.5312341902212,-35.1138494411902));
#74063=CARTESIAN_POINT('Origin',(4.5,14.5472582706721,-35.1439863533772));
#74064=CARTESIAN_POINT('',(1.90350512467335,14.5156102591402,-35.0844651005135));
#74065=CARTESIAN_POINT('Origin',(1.9,14.5472582706721,-35.1439863533772));
#74066=CARTESIAN_POINT('Ctrl Pts',(0.138207714141622,15.5649826112913,-39.8284094059642));
#74067=CARTESIAN_POINT('Ctrl Pts',(0.370217470896767,15.6324336584852,-39.5529520736987));
#74068=CARTESIAN_POINT('Ctrl Pts',(0.600000000000007,15.6985967468815,-39.2790537077817));
#74069=CARTESIAN_POINT('Origin',(1.9,11.4462726220786,-36.2726528263519));
#74070=CARTESIAN_POINT('',(5.09593997529677,12.3365516130267,-40.4610861730024));
#74071=CARTESIAN_POINT('',(17.5,12.3365516130267,-40.4610861730024));
#74072=CARTESIAN_POINT('',(4.47529854852883,11.409370947074,-36.0990440950346));
#74073=CARTESIAN_POINT('Origin',(4.5,11.4462726220786,-36.2726528263519));
#74074=CARTESIAN_POINT('',(5.09944803334083,12.8457455753269,-40.3023178069695));
#74075=CARTESIAN_POINT('Origin',(-0.840551718690874,0.,0.));
#74076=CARTESIAN_POINT('',(4.50447263544529,11.9230551151638,-36.1329850680974));
#74077=CARTESIAN_POINT('Origin',(4.5,11.9161189324716,-36.101642754689));
#74078=CARTESIAN_POINT('',(10.8302042597752,13.1850308552911,-40.1925983403042));
#74079=CARTESIAN_POINT('Origin',(-62.7155570771054,0.,0.));
#74080=CARTESIAN_POINT('',(10.8987117910442,12.3084785844451,-36.0428658633082));
#74081=CARTESIAN_POINT('Origin',(10.9,12.291995980786,-35.9648346973588));
#74082=CARTESIAN_POINT('',(11.6618634261911,12.9488045494887,-40.2693240660821));
#74083=CARTESIAN_POINT('Origin',(26.9856656232739,0.,0.));
#74084=CARTESIAN_POINT('',(11.8995413080444,12.0118963235316,-36.0755342895718));
#74085=CARTESIAN_POINT('Origin',(11.9,12.0100881945502,-36.0674407403565));
#74086=CARTESIAN_POINT('',(12.3548486633046,12.5735100877104,-40.3880779943072));
#74087=CARTESIAN_POINT('Origin',(20.8267261185512,0.,0.));
#74088=CARTESIAN_POINT('',(12.600317055424,11.6329963463162,-36.1988378309035));
#74089=CARTESIAN_POINT('Origin',(12.6,11.6342111462358,-36.2042487976867));
#74090=CARTESIAN_POINT('',(13.103292255208,12.3365516130267,-40.4610861730024));
#74091=CARTESIAN_POINT('Origin',(25.13830739299,0.,0.));
#74092=CARTESIAN_POINT('',(13.2001612154348,11.4447884936362,-36.2656705509953));
#74093=CARTESIAN_POINT('Origin',(13.2,11.4462726220786,-36.2726528263519));
#74094=CARTESIAN_POINT('',(21.896707744792,12.3365516130267,-40.4610861730024));
#74095=CARTESIAN_POINT('',(17.5,12.3365516130267,-40.4610861730024));
#74096=CARTESIAN_POINT('',(21.7978078257374,11.42609174934,-36.1777092848303));
#74097=CARTESIAN_POINT('Origin',(21.8,11.4462726220786,-36.2726528263519));
#74098=CARTESIAN_POINT('',(22.6451513366954,12.5735100877104,-40.3880779943072));
#74099=CARTESIAN_POINT('Origin',(9.86169260701006,0.,0.));
#74100=CARTESIAN_POINT('',(22.3997512812625,11.633258178775,-36.2000040861152));
#74101=CARTESIAN_POINT('Origin',(22.4,11.6342111462358,-36.2042487976867));
#74102=CARTESIAN_POINT('',(23.3381365738089,12.9488045494887,-40.2693240660821));
#74103=CARTESIAN_POINT('Origin',(14.1732738814488,0.,0.));
#74104=CARTESIAN_POINT('',(23.1003542130464,12.0114844755768,-36.0736907752397));
#74105=CARTESIAN_POINT('Origin',(23.1,12.0100881945502,-36.0674407403565));
#74106=CARTESIAN_POINT('',(24.1697957402248,13.1850308552911,-40.1925983403042));
#74107=CARTESIAN_POINT('Origin',(8.01433437672607,0.,0.));
#74108=CARTESIAN_POINT('',(24.100209736014,12.2946795482123,-35.9775391158784));
#74109=CARTESIAN_POINT('Origin',(24.1,12.291995980786,-35.9648346973588));
#74110=CARTESIAN_POINT('',(29.9005519666592,12.8457455753269,-40.3023178069695));
#74111=CARTESIAN_POINT('Origin',(97.7155570771054,0.,0.));
#74112=CARTESIAN_POINT('',(30.4426385593966,12.0050753064884,-36.5036071604488));
#74113=CARTESIAN_POINT('Origin',(30.5,11.9161189324716,-36.101642754689));
#74114=CARTESIAN_POINT('',(29.9040600247032,12.3365516130267,-40.4610861730024));
#74115=CARTESIAN_POINT('Origin',(35.8405517186909,0.,0.));
#74116=CARTESIAN_POINT('',(30.5047502791291,11.4391761461162,-36.2392665318678));
#74117=CARTESIAN_POINT('Origin',(30.5,11.4462726220786,-36.2726528263519));
#74118=CARTESIAN_POINT('',(17.5,12.3365516130267,-40.4610861730024));
#74119=CARTESIAN_POINT('Origin',(17.5,14.6213611271723,-40.1718595385976));
#74120=CARTESIAN_POINT('Origin',(17.5,0.,0.));
#74121=CARTESIAN_POINT('',(0.600000000000001,8.63936369090331,-41.4083493394303));
#74122=CARTESIAN_POINT('Origin',(0.600000000000001,0.,0.));
#74123=CARTESIAN_POINT('',(1.67735469196904,9.54677599452212,-41.2086042970448));
#74124=CARTESIAN_POINT('Origin',(8.14497546096349,0.,0.));
#74125=CARTESIAN_POINT('',(5.09593997529677,9.54677599452211,-41.2086042970448));
#74126=CARTESIAN_POINT('',(17.5,9.54677599452211,-41.2086042970448));
#74127=CARTESIAN_POINT('',(5.09944803334083,9.02641690470009,-41.325703839893));
#74128=CARTESIAN_POINT('Origin',(-0.840551718690872,0.,0.));
#74129=CARTESIAN_POINT('',(10.8302042597752,8.67772749978828,-41.4003266344532));
#74130=CARTESIAN_POINT('Origin',(-62.7155570771055,0.,0.));
#74131=CARTESIAN_POINT('',(11.6618634261911,8.92066834454425,-41.3486599091996));
#74132=CARTESIAN_POINT('Origin',(26.9856656232739,0.,0.));
#74133=CARTESIAN_POINT('',(12.3548486633046,9.3050598464565,-41.2638565969525));
#74134=CARTESIAN_POINT('Origin',(20.8267261185512,0.,0.));
#74135=CARTESIAN_POINT('',(13.103292255208,9.54677599452212,-41.2086042970448));
#74136=CARTESIAN_POINT('Origin',(25.13830739299,0.,0.));
#74137=CARTESIAN_POINT('',(21.896707744792,9.54677599452211,-41.2086042970448));
#74138=CARTESIAN_POINT('',(17.5,9.54677599452211,-41.2086042970448));
#74139=CARTESIAN_POINT('',(22.6451513366954,9.3050598464565,-41.2638565969525));
#74140=CARTESIAN_POINT('Origin',(9.86169260701005,0.,0.));
#74141=CARTESIAN_POINT('',(23.3381365738089,8.92066834454425,-41.3486599091996));
#74142=CARTESIAN_POINT('Origin',(14.1732738814488,0.,0.));
#74143=CARTESIAN_POINT('',(24.1697957402248,8.67772749978828,-41.4003266344532));
#74144=CARTESIAN_POINT('Origin',(8.01433437672608,0.,0.));
#74145=CARTESIAN_POINT('',(29.9005519666592,9.02641690470009,-41.325703839893));
#74146=CARTESIAN_POINT('Origin',(97.7155570771054,0.,0.));
#74147=CARTESIAN_POINT('',(29.9040600247032,9.54677599452211,-41.2086042970448));
#74148=CARTESIAN_POINT('Origin',(35.8405517186909,0.,0.));
#74149=CARTESIAN_POINT('',(17.5,9.54677599452211,-41.2086042970448));
#74150=CARTESIAN_POINT('Origin',(33.1,8.22356354381348,-37.1361751213135));
#74151=CARTESIAN_POINT('',(30.5247014514712,8.16871696615112,-36.9673747121716));
#74152=CARTESIAN_POINT('Origin',(30.5,8.22356354381348,-37.1361751213135));
#74153=CARTESIAN_POINT('',(30.4955273645547,7.74082391359483,-37.253610541118));
#74154=CARTESIAN_POINT('Origin',(30.5,7.73115966730738,-37.2229992101469));
#74155=CARTESIAN_POINT('',(24.1012882089558,7.36197779558789,-37.3682767550424));
#74156=CARTESIAN_POINT('Origin',(24.1,7.33723656610249,-37.2924584812137));
#74157=CARTESIAN_POINT('',(23.1004586919557,7.63515978098255,-37.2482773116316));
#74158=CARTESIAN_POINT('Origin',(23.1,7.63267889200616,-37.2403640279136));
#74159=CARTESIAN_POINT('',(22.399682944576,8.02494855741035,-37.1656113221937));
#74160=CARTESIAN_POINT('Origin',(22.4,8.02660199321104,-37.1709047568469));
#74161=CARTESIAN_POINT('',(21.7998387845652,8.22135769906883,-37.1293862292573));
#74162=CARTESIAN_POINT('Origin',(21.8,8.22356354381348,-37.1361751213135));
#74163=CARTESIAN_POINT('',(13.2021921742626,8.19356892151486,-37.0438611660612));
#74164=CARTESIAN_POINT('Origin',(13.2,8.22356354381348,-37.1361751213135));
#74165=CARTESIAN_POINT('',(12.6002487187375,8.02530493145532,-37.1667522450638));
#74166=CARTESIAN_POINT('Origin',(12.6,8.02660199321104,-37.1709047568469));
#74167=CARTESIAN_POINT('',(11.8996457869536,7.63459469460788,-37.2464748574103));
#74168=CARTESIAN_POINT('Origin',(11.9,7.63267889200616,-37.2403640279136));
#74169=CARTESIAN_POINT('',(10.899790263986,7.34126473779835,-37.3048026141052));
#74170=CARTESIAN_POINT('Origin',(10.9,7.33723656610249,-37.2924584812137));
#74171=CARTESIAN_POINT('',(4.55736144060343,7.85510339046015,-37.6155887839604));
#74172=CARTESIAN_POINT('Origin',(4.5,7.73115966730738,-37.2229992101469));
#74173=CARTESIAN_POINT('',(4.49524972087093,8.21301612503226,-37.1037135041708));
#74174=CARTESIAN_POINT('Origin',(4.5,8.22356354381348,-37.1361751213135));
#74175=CARTESIAN_POINT('',(1.90350512467335,8.20273209378166,-37.0720625104951));
#74176=CARTESIAN_POINT('Origin',(1.9,8.22356354381348,-37.1361751213135));
#74177=CARTESIAN_POINT('Ctrl Pts',(0.138207714141623,8.41238483838183,-41.9261572390061));
#74178=CARTESIAN_POINT('Ctrl Pts',(0.370217470900092,8.52664381638163,-41.6665974739903));
#74179=CARTESIAN_POINT('Ctrl Pts',(0.600000000000007,8.63936369090331,-41.4083493394303));
#74180=CARTESIAN_POINT('Origin',(1.9,4.9736979588732,-37.7092141076143));
#74181=CARTESIAN_POINT('',(5.09593997529677,5.1231377935775,-41.9886110647639));
#74182=CARTESIAN_POINT('',(17.5,5.1231377935775,-41.9886110647639));
#74183=CARTESIAN_POINT('',(4.47529854852883,4.96750374304975,-37.5318349744051));
#74184=CARTESIAN_POINT('Origin',(4.5,4.9736979588732,-37.7092141076143));
#74185=CARTESIAN_POINT('',(5.09944803334083,5.65216579287044,-41.9206753505941));
#74186=CARTESIAN_POINT('Origin',(-0.840551718690874,0.,0.));
#74187=CARTESIAN_POINT('',(4.50447263544529,5.46749010626365,-37.6544606275072));
#74188=CARTESIAN_POINT('Origin',(4.5,5.4661018353793,-37.6223900187809));
#74189=CARTESIAN_POINT('',(10.8302042597752,6.00534915250317,-41.8715390397407));
#74190=CARTESIAN_POINT('Origin',(-62.7155570771055,0.,0.));
#74191=CARTESIAN_POINT('',(10.8987117910442,5.86270716268917,-37.6326386190063));
#74192=CARTESIAN_POINT('Origin',(10.9,5.86002493658418,-37.5529307477141));
#74193=CARTESIAN_POINT('',(11.6618634261911,5.75938837262205,-41.9060788618227));
#74194=CARTESIAN_POINT('Origin',(26.9856656232739,0.,0.));
#74195=CARTESIAN_POINT('',(11.8995413080444,5.5649578400478,-37.6133097693334));
#74196=CARTESIAN_POINT('Origin',(11.9,5.56458261068052,-37.6050252010142));
#74197=CARTESIAN_POINT('',(12.3548486633046,5.36917407377308,-41.9578594516632));
#74198=CARTESIAN_POINT('Origin',(20.8267261185512,0.,0.));
#74199=CARTESIAN_POINT('',(12.600317055424,5.17040276961774,-37.6689447622493));
#74200=CARTESIAN_POINT('Origin',(12.6,5.17065950947564,-37.674484472081));
#74201=CARTESIAN_POINT('',(13.103292255208,5.1231377935775,-41.9886110647639));
#74202=CARTESIAN_POINT('Origin',(25.13830739299,0.,0.));
#74203=CARTESIAN_POINT('',(13.2001612154348,4.97344883706827,-37.7020801925101));
#74204=CARTESIAN_POINT('Origin',(13.2,4.9736979588732,-37.7092141076143));
#74205=CARTESIAN_POINT('',(21.896707744792,5.1231377935775,-41.9886110647639));
#74206=CARTESIAN_POINT('',(17.5,5.1231377935775,-41.9886110647639));
#74207=CARTESIAN_POINT('',(21.7978078257374,4.97031045190413,-37.6122086000506));
#74208=CARTESIAN_POINT('Origin',(21.8,4.9736979588732,-37.7092141076143));
#74209=CARTESIAN_POINT('',(22.6451513366954,5.36917407377308,-41.9578594516632));
#74210=CARTESIAN_POINT('Origin',(9.86169260701005,0.,0.));
#74211=CARTESIAN_POINT('',(22.3997512812625,5.17045810616097,-37.6701387661531));
#74212=CARTESIAN_POINT('Origin',(22.4,5.17065950947564,-37.674484472081));
#74213=CARTESIAN_POINT('',(23.3381365738089,5.75938837262205,-41.9060788618227));
#74214=CARTESIAN_POINT('Origin',(14.1732738814488,0.,0.));
#74215=CARTESIAN_POINT('',(23.1003542130464,5.5648723718931,-37.6114227454796));
#74216=CARTESIAN_POINT('Origin',(23.1,5.56458261068052,-37.6050252010142));
#74217=CARTESIAN_POINT('',(24.1697957402248,6.00534915250317,-41.8715390397407));
#74218=CARTESIAN_POINT('Origin',(8.01433437672608,0.,0.));
#74219=CARTESIAN_POINT('',(24.100209736014,5.86046163546709,-37.565908154163));
#74220=CARTESIAN_POINT('Origin',(24.1,5.86002493658418,-37.5529307477141));
#74221=CARTESIAN_POINT('',(29.9005519666592,5.65216579287044,-41.9206753505941));
#74222=CARTESIAN_POINT('Origin',(97.7155570771054,0.,0.));
#74223=CARTESIAN_POINT('',(30.4426385593966,5.48390637564376,-38.0336947942479));
#74224=CARTESIAN_POINT('Origin',(30.5,5.4661018353793,-37.6223900187809));
#74225=CARTESIAN_POINT('',(29.9040600247032,5.1231377935775,-41.9886110647639));
#74226=CARTESIAN_POINT('Origin',(35.8405517186909,0.,0.));
#74227=CARTESIAN_POINT('',(30.5047502791291,4.97250676352253,-37.6751027358433));
#74228=CARTESIAN_POINT('Origin',(30.5,4.9736979588732,-37.7092141076143));
#74229=CARTESIAN_POINT('',(17.5,5.1231377935775,-41.9886110647639));
#74230=CARTESIAN_POINT('Origin',(17.5,7.42345959526125,-42.1005314412719));
#74231=CARTESIAN_POINT('Origin',(17.5,0.,0.));
#74232=CARTESIAN_POINT('',(0.600000000000001,1.31762794090603,-42.2794732300362));
#74233=CARTESIAN_POINT('Origin',(0.600000000000001,0.,0.));
#74234=CARTESIAN_POINT('',(1.67735469196904,2.24593997529676,-42.240333256585));
#74235=CARTESIAN_POINT('Origin',(8.14497546096349,0.,0.));
#74236=CARTESIAN_POINT('',(5.09593997529677,2.24593997529676,-42.240333256585));
#74237=CARTESIAN_POINT('',(17.5,2.24593997529676,-42.240333256585));
#74238=CARTESIAN_POINT('',(5.09944803334083,1.71315218706844,-42.2652943865761));
#74239=CARTESIAN_POINT('Origin',(-0.840551718690872,0.,0.));
#74240=CARTESIAN_POINT('',(10.8302042597752,1.35680204543027,-42.2782342134758));
#74241=CARTESIAN_POINT('Origin',(-62.7155570771055,0.,0.));
#74242=CARTESIAN_POINT('',(11.6618634261911,1.6050239055556,-42.269538656846));
#74243=CARTESIAN_POINT('Origin',(26.9856656232739,0.,0.));
#74244=CARTESIAN_POINT('',(12.3548486633046,1.99830157746261,-42.2527725812817));
#74245=CARTESIAN_POINT('Origin',(20.8267261185512,0.,0.));
#74246=CARTESIAN_POINT('',(13.103292255208,2.24593997529676,-42.240333256585));
#74247=CARTESIAN_POINT('Origin',(25.13830739299,0.,0.));
#74248=CARTESIAN_POINT('',(21.896707744792,2.24593997529676,-42.240333256585));
#74249=CARTESIAN_POINT('',(17.5,2.24593997529676,-42.240333256585));
#74250=CARTESIAN_POINT('',(22.6451513366954,1.99830157746261,-42.2527725812817));
#74251=CARTESIAN_POINT('Origin',(9.86169260701006,0.,0.));
#74252=CARTESIAN_POINT('',(23.3381365738089,1.6050239055556,-42.269538656846));
#74253=CARTESIAN_POINT('Origin',(14.1732738814488,0.,0.));
#74254=CARTESIAN_POINT('',(24.1697957402248,1.35680204543027,-42.2782342134758));
#74255=CARTESIAN_POINT('Origin',(8.01433437672608,0.,0.));
#74256=CARTESIAN_POINT('',(29.9005519666592,1.71315218706844,-42.2652943865761));
#74257=CARTESIAN_POINT('Origin',(97.7155570771054,0.,0.));
#74258=CARTESIAN_POINT('',(29.9040600247032,2.24593997529676,-42.240333256585));
#74259=CARTESIAN_POINT('Origin',(35.8405517186909,0.,0.));
#74260=CARTESIAN_POINT('',(17.5,2.24593997529676,-42.240333256585));
#74261=CARTESIAN_POINT('Origin',(33.1,1.64999999999999,-38.));
#74262=CARTESIAN_POINT('',(30.5247014514712,1.62529854852883,-37.8242400401031));
#74263=CARTESIAN_POINT('Origin',(30.5,1.64999999999999,-38.));
#74264=CARTESIAN_POINT('',(30.4955273645547,1.15420182283181,-38.0318244548267));
#74265=CARTESIAN_POINT('Origin',(30.5,1.14999999999999,-38.));
#74266=CARTESIAN_POINT('',(24.1012882089558,0.761199649532065,-38.0789626932999));
#74267=CARTESIAN_POINT('Origin',(24.1,0.749999999999993,-38.));
#74268=CARTESIAN_POINT('',(23.1004586919557,1.05106907140132,-38.0082238650069));
#74269=CARTESIAN_POINT('Origin',(23.1,1.04999999999999,-38.));
#74270=CARTESIAN_POINT('',(22.399682944576,1.44929087888548,-37.9944998683999));
#74271=CARTESIAN_POINT('Origin',(22.4,1.44999999999999,-38.));
#74272=CARTESIAN_POINT('',(21.7998387845652,1.64900654572745,-37.9929312055486));
#74273=CARTESIAN_POINT('Origin',(21.8,1.64999999999999,-38.));
#74274=CARTESIAN_POINT('',(13.2021921742626,1.63649121351442,-37.9038799896544));
#74275=CARTESIAN_POINT('Origin',(13.2,1.64999999999999,-38.));
#74276=CARTESIAN_POINT('',(12.6002487187375,1.4494437196307,-37.9956853417913));
#74277=CARTESIAN_POINT('Origin',(12.6,1.44999999999999,-38.));
#74278=CARTESIAN_POINT('',(11.8996457869536,1.05082556284928,-38.0063506678963));
#74279=CARTESIAN_POINT('Origin',(11.9,1.04999999999999,-38.));
#74280=CARTESIAN_POINT('',(10.899790263986,0.751823438535061,-38.01285608245));
#74281=CARTESIAN_POINT('Origin',(10.9,0.749999999999993,-38.));
#74282=CARTESIAN_POINT('',(4.55736144060343,1.20388827543429,-38.408147857702));
#74283=CARTESIAN_POINT('Origin',(4.5,1.14999999999999,-38.));
#74284=CARTESIAN_POINT('',(4.49524972087093,1.64524972087092,-37.9662000077121));
#74285=CARTESIAN_POINT('Origin',(4.5,1.64999999999999,-38.));
#74286=CARTESIAN_POINT('',(1.90350512467335,1.64061806453626,-37.933244060464));
#74287=CARTESIAN_POINT('Origin',(1.9,1.64999999999999,-38.));
#74288=CARTESIAN_POINT('Ctrl Pts',(0.138207714141622,1.0041810090302,-42.75));
#74289=CARTESIAN_POINT('Ctrl Pts',(0.370217470898645,1.16177621660533,-42.5142243943556));
#74290=CARTESIAN_POINT('Ctrl Pts',(0.600000000000007,1.31762794090604,-42.2794732300361));
#74291=CARTESIAN_POINT('Origin',(1.9,-1.65000000000001,-38.));
#74292=CARTESIAN_POINT('',(5.09593997529677,-2.24593997529678,-42.240333256585));
#74293=CARTESIAN_POINT('',(17.5,-2.24593997529678,-42.240333256585));
#74294=CARTESIAN_POINT('',(4.47529854852883,-1.62529854852884,-37.8242400401031));
#74295=CARTESIAN_POINT('Origin',(4.5,-1.65000000000001,-38.));
#74296=CARTESIAN_POINT('',(5.09944803334083,-1.71315218706845,-42.2652943865761));
#74297=CARTESIAN_POINT('Origin',(-0.840551718690874,0.,0.));
#74298=CARTESIAN_POINT('',(4.50447263544529,-1.15420182283182,-38.0318244548267));
#74299=CARTESIAN_POINT('Origin',(4.5,-1.15000000000001,-38.));
#74300=CARTESIAN_POINT('',(10.8302042597752,-1.35680204543028,-42.2782342134758));
#74301=CARTESIAN_POINT('Origin',(-62.7155570771055,0.,0.));
#74302=CARTESIAN_POINT('',(10.8987117910442,-0.761199649532079,-38.0789626932999));
#74303=CARTESIAN_POINT('Origin',(10.9,-0.750000000000007,-38.));
#74304=CARTESIAN_POINT('',(11.6618634261911,-1.60502390555562,-42.269538656846));
#74305=CARTESIAN_POINT('Origin',(26.9856656232739,0.,0.));
#74306=CARTESIAN_POINT('',(11.8995413080444,-1.05106907140134,-38.0082238650069));
#74307=CARTESIAN_POINT('Origin',(11.9,-1.05000000000001,-38.));
#74308=CARTESIAN_POINT('',(12.3548486633046,-1.99830157746262,-42.2527725812817));
#74309=CARTESIAN_POINT('Origin',(20.8267261185512,0.,0.));
#74310=CARTESIAN_POINT('',(12.600317055424,-1.4492908788855,-37.9944998683999));
#74311=CARTESIAN_POINT('Origin',(12.6,-1.45000000000001,-38.));
#74312=CARTESIAN_POINT('',(13.103292255208,-2.24593997529678,-42.240333256585));
#74313=CARTESIAN_POINT('Origin',(25.13830739299,0.,0.));
#74314=CARTESIAN_POINT('',(13.2001612154348,-1.64900654572746,-37.9929312055486));
#74315=CARTESIAN_POINT('Origin',(13.2,-1.65000000000001,-38.));
#74316=CARTESIAN_POINT('',(21.896707744792,-2.24593997529678,-42.240333256585));
#74317=CARTESIAN_POINT('',(17.5,-2.24593997529678,-42.240333256585));
#74318=CARTESIAN_POINT('',(21.7978078257374,-1.63649121351443,-37.9038799896544));
#74319=CARTESIAN_POINT('Origin',(21.8,-1.65000000000001,-38.));
#74320=CARTESIAN_POINT('',(22.6451513366954,-1.99830157746262,-42.2527725812817));
#74321=CARTESIAN_POINT('Origin',(9.86169260701005,0.,0.));
#74322=CARTESIAN_POINT('',(22.3997512812625,-1.44944371963072,-37.9956853417913));
#74323=CARTESIAN_POINT('Origin',(22.4,-1.45000000000001,-38.));
#74324=CARTESIAN_POINT('',(23.3381365738089,-1.60502390555562,-42.269538656846));
#74325=CARTESIAN_POINT('Origin',(14.1732738814488,0.,0.));
#74326=CARTESIAN_POINT('',(23.1003542130464,-1.05082556284929,-38.0063506678963));
#74327=CARTESIAN_POINT('Origin',(23.1,-1.05000000000001,-38.));
#74328=CARTESIAN_POINT('',(24.1697957402248,-1.35680204543028,-42.2782342134758));
#74329=CARTESIAN_POINT('Origin',(8.01433437672608,0.,0.));
#74330=CARTESIAN_POINT('',(24.100209736014,-0.751823438535075,-38.01285608245));
#74331=CARTESIAN_POINT('Origin',(24.1,-0.750000000000007,-38.));
#74332=CARTESIAN_POINT('',(29.9005519666592,-1.71315218706845,-42.2652943865761));
#74333=CARTESIAN_POINT('Origin',(97.7155570771054,0.,0.));
#74334=CARTESIAN_POINT('',(30.4426385593966,-1.20388827543431,-38.408147857702));
#74335=CARTESIAN_POINT('Origin',(30.5,-1.15000000000001,-38.));
#74336=CARTESIAN_POINT('',(29.9040600247032,-2.24593997529678,-42.240333256585));
#74337=CARTESIAN_POINT('Origin',(35.8405517186909,0.,0.));
#74338=CARTESIAN_POINT('',(30.5047502791291,-1.64524972087094,-37.9662000077121));
#74339=CARTESIAN_POINT('Origin',(30.5,-1.65000000000001,-38.));
#74340=CARTESIAN_POINT('',(17.5,-2.24593997529678,-42.240333256585));
#74341=CARTESIAN_POINT('Origin',(17.5,-7.8530475995324E-15,-42.75));
#74342=CARTESIAN_POINT('Origin',(17.5,0.,0.));
#74343=CARTESIAN_POINT('',(0.600000000000001,-6.04414326732376,-41.8659567209931));
#74344=CARTESIAN_POINT('Origin',(0.600000000000001,0.,0.));
#74345=CARTESIAN_POINT('',(1.67735469196905,-5.12313779357752,-41.9886110647639));
#74346=CARTESIAN_POINT('Origin',(8.14497546096349,0.,0.));
#74347=CARTESIAN_POINT('',(5.09593997529677,-5.12313779357752,-41.9886110647639));
#74348=CARTESIAN_POINT('',(17.5,-5.12313779357752,-41.9886110647639));
#74349=CARTESIAN_POINT('',(5.09944803334083,-5.65216579287046,-41.9206753505941));
#74350=CARTESIAN_POINT('Origin',(-0.840551718690872,0.,0.));
#74351=CARTESIAN_POINT('',(10.8302042597752,-6.00534915250318,-41.8715390397407));
#74352=CARTESIAN_POINT('Origin',(-62.7155570771055,0.,0.));
#74353=CARTESIAN_POINT('',(11.6618634261911,-5.75938837262207,-41.9060788618227));
#74354=CARTESIAN_POINT('Origin',(26.9856656232739,0.,0.));
#74355=CARTESIAN_POINT('',(12.3548486633046,-5.3691740737731,-41.9578594516632));
#74356=CARTESIAN_POINT('Origin',(20.8267261185512,0.,0.));
#74357=CARTESIAN_POINT('',(13.103292255208,-5.12313779357752,-41.9886110647639));
#74358=CARTESIAN_POINT('Origin',(25.13830739299,0.,0.));
#74359=CARTESIAN_POINT('',(21.896707744792,-5.12313779357752,-41.9886110647639));
#74360=CARTESIAN_POINT('',(17.5,-5.12313779357752,-41.9886110647639));
#74361=CARTESIAN_POINT('',(22.6451513366954,-5.3691740737731,-41.9578594516632));
#74362=CARTESIAN_POINT('Origin',(9.86169260701005,0.,0.));
#74363=CARTESIAN_POINT('',(23.3381365738089,-5.75938837262207,-41.9060788618227));
#74364=CARTESIAN_POINT('Origin',(14.1732738814488,0.,0.));
#74365=CARTESIAN_POINT('',(24.1697957402248,-6.00534915250318,-41.8715390397407));
#74366=CARTESIAN_POINT('Origin',(8.01433437672608,0.,0.));
#74367=CARTESIAN_POINT('',(29.9005519666592,-5.65216579287046,-41.9206753505941));
#74368=CARTESIAN_POINT('Origin',(97.7155570771054,0.,0.));
#74369=CARTESIAN_POINT('',(29.9040600247032,-5.12313779357752,-41.9886110647639));
#74370=CARTESIAN_POINT('Origin',(35.8405517186909,0.,0.));
#74371=CARTESIAN_POINT('',(17.5,-5.12313779357752,-41.9886110647639));
#74372=CARTESIAN_POINT('Origin',(33.1,-4.97369795887321,-37.7092141076143));
#74373=CARTESIAN_POINT('',(30.5247014514712,-4.96750374304976,-37.5318349744051));
#74374=CARTESIAN_POINT('Origin',(30.5,-4.97369795887321,-37.7092141076143));
#74375=CARTESIAN_POINT('',(30.4955273645547,-5.46749010626366,-37.6544606275072));
#74376=CARTESIAN_POINT('Origin',(30.5,-5.46610183537931,-37.6223900187809));
#74377=CARTESIAN_POINT('',(24.1012882089558,-5.86270716268919,-37.6326386190063));
#74378=CARTESIAN_POINT('Origin',(24.1,-5.8600249365842,-37.5529307477141));
#74379=CARTESIAN_POINT('',(23.1004586919557,-5.56495784004782,-37.6133097693334));
#74380=CARTESIAN_POINT('Origin',(23.1,-5.56458261068053,-37.6050252010142));
#74381=CARTESIAN_POINT('',(22.399682944576,-5.17040276961776,-37.6689447622493));
#74382=CARTESIAN_POINT('Origin',(22.4,-5.17065950947565,-37.674484472081));
#74383=CARTESIAN_POINT('',(21.7998387845652,-4.97344883706828,-37.7020801925101));
#74384=CARTESIAN_POINT('Origin',(21.8,-4.97369795887321,-37.7092141076143));
#74385=CARTESIAN_POINT('',(13.2021921742626,-4.97031045190415,-37.6122086000507));
#74386=CARTESIAN_POINT('Origin',(13.2,-4.97369795887321,-37.7092141076143));
#74387=CARTESIAN_POINT('',(12.6002487187375,-5.17045810616098,-37.6701387661531));
#74388=CARTESIAN_POINT('Origin',(12.6,-5.17065950947565,-37.674484472081));
#74389=CARTESIAN_POINT('',(11.8996457869536,-5.56487237189311,-37.6114227454796));
#74390=CARTESIAN_POINT('Origin',(11.9,-5.56458261068053,-37.6050252010142));
#74391=CARTESIAN_POINT('',(10.899790263986,-5.8604616354671,-37.565908154163));
#74392=CARTESIAN_POINT('Origin',(10.9,-5.8600249365842,-37.5529307477141));
#74393=CARTESIAN_POINT('',(4.55736144060343,-5.48390637564377,-38.0336947942479));
#74394=CARTESIAN_POINT('Origin',(4.5,-5.46610183537931,-37.6223900187809));
#74395=CARTESIAN_POINT('',(4.49524972087093,-4.97250676352255,-37.6751027358433));
#74396=CARTESIAN_POINT('Origin',(4.5,-4.97369795887321,-37.7092141076143));
#74397=CARTESIAN_POINT('',(1.90350512467335,-4.97134531440728,-37.6418431848034));
#74398=CARTESIAN_POINT('Origin',(1.9,-4.97369795887321,-37.7092141076143));
#74399=CARTESIAN_POINT('Ctrl Pts',(0.138207714141622,-6.4345343521407,-42.2749056435377));
#74400=CARTESIAN_POINT('Ctrl Pts',(0.370217470893856,-6.23839136562873,
-42.0700781197367));
#74401=CARTESIAN_POINT('Ctrl Pts',(0.600000000000006,-6.04414326732376,
-41.8659567209931));
#74402=CARTESIAN_POINT('Origin',(1.9,-8.2235635438135,-37.1361751213135));
#74403=CARTESIAN_POINT('',(5.09593997529677,-9.54677599452213,-41.2086042970448));
#74404=CARTESIAN_POINT('',(17.5,-9.54677599452213,-41.2086042970448));
#74405=CARTESIAN_POINT('',(4.47529854852883,-8.16871696615113,-36.9673747121716));
#74406=CARTESIAN_POINT('Origin',(4.5,-8.2235635438135,-37.1361751213135));
#74407=CARTESIAN_POINT('',(5.09944803334083,-9.02641690470011,-41.325703839893));
#74408=CARTESIAN_POINT('Origin',(-0.840551718690874,0.,0.));
#74409=CARTESIAN_POINT('',(4.50447263544529,-7.74082391359484,-37.253610541118));
#74410=CARTESIAN_POINT('Origin',(4.5,-7.73115966730739,-37.2229992101469));
#74411=CARTESIAN_POINT('',(10.8302042597752,-8.6777274997883,-41.4003266344532));
#74412=CARTESIAN_POINT('Origin',(-62.7155570771055,0.,0.));
#74413=CARTESIAN_POINT('',(10.8987117910442,-7.36197779558791,-37.3682767550424));
#74414=CARTESIAN_POINT('Origin',(10.9,-7.33723656610251,-37.2924584812137));
#74415=CARTESIAN_POINT('',(11.6618634261911,-8.92066834454427,-41.3486599091995));
#74416=CARTESIAN_POINT('Origin',(26.9856656232739,0.,0.));
#74417=CARTESIAN_POINT('',(11.8995413080444,-7.63515978098256,-37.2482773116316));
#74418=CARTESIAN_POINT('Origin',(11.9,-7.63267889200617,-37.2403640279136));
#74419=CARTESIAN_POINT('',(12.3548486633046,-9.30505984645652,-41.2638565969525));
#74420=CARTESIAN_POINT('Origin',(20.8267261185512,0.,0.));
#74421=CARTESIAN_POINT('',(12.600317055424,-8.02494855741037,-37.1656113221937));
#74422=CARTESIAN_POINT('Origin',(12.6,-8.02660199321105,-37.1709047568469));
#74423=CARTESIAN_POINT('',(13.103292255208,-9.54677599452213,-41.2086042970448));
#74424=CARTESIAN_POINT('Origin',(25.13830739299,0.,0.));
#74425=CARTESIAN_POINT('',(13.2001612154348,-8.22135769906884,-37.1293862292573));
#74426=CARTESIAN_POINT('Origin',(13.2,-8.2235635438135,-37.1361751213135));
#74427=CARTESIAN_POINT('',(21.896707744792,-9.54677599452213,-41.2086042970448));
#74428=CARTESIAN_POINT('',(17.5,-9.54677599452213,-41.2086042970448));
#74429=CARTESIAN_POINT('',(21.7978078257374,-8.19356892151487,-37.0438611660612));
#74430=CARTESIAN_POINT('Origin',(21.8,-8.2235635438135,-37.1361751213135));
#74431=CARTESIAN_POINT('',(22.6451513366954,-9.30505984645652,-41.2638565969525));
#74432=CARTESIAN_POINT('Origin',(9.86169260701004,0.,0.));
#74433=CARTESIAN_POINT('',(22.3997512812625,-8.02530493145534,-37.1667522450638));
#74434=CARTESIAN_POINT('Origin',(22.4,-8.02660199321105,-37.1709047568469));
#74435=CARTESIAN_POINT('',(23.3381365738089,-8.92066834454426,-41.3486599091995));
#74436=CARTESIAN_POINT('Origin',(14.1732738814488,0.,0.));
#74437=CARTESIAN_POINT('',(23.1003542130464,-7.6345946946079,-37.2464748574103));
#74438=CARTESIAN_POINT('Origin',(23.1,-7.63267889200617,-37.2403640279136));
#74439=CARTESIAN_POINT('',(24.1697957402248,-8.6777274997883,-41.4003266344532));
#74440=CARTESIAN_POINT('Origin',(8.01433437672608,0.,0.));
#74441=CARTESIAN_POINT('',(24.100209736014,-7.34126473779837,-37.3048026141052));
#74442=CARTESIAN_POINT('Origin',(24.1,-7.33723656610251,-37.2924584812137));
#74443=CARTESIAN_POINT('',(29.9005519666592,-9.02641690470011,-41.325703839893));
#74444=CARTESIAN_POINT('Origin',(97.7155570771055,0.,0.));
#74445=CARTESIAN_POINT('',(30.4426385593966,-7.85510339046017,-37.6155887839604));
#74446=CARTESIAN_POINT('Origin',(30.5,-7.73115966730739,-37.2229992101469));
#74447=CARTESIAN_POINT('',(29.9040600247032,-9.54677599452213,-41.2086042970448));
#74448=CARTESIAN_POINT('Origin',(35.8405517186909,0.,0.));
#74449=CARTESIAN_POINT('',(30.5047502791291,-8.21301612503227,-37.1037135041708));
#74450=CARTESIAN_POINT('Origin',(30.5,-8.2235635438135,-37.1361751213135));
#74451=CARTESIAN_POINT('',(17.5,-9.54677599452213,-41.2086042970448));
#74452=CARTESIAN_POINT('Origin',(17.5,-7.42345959526127,-42.1005314412719));
#74453=CARTESIAN_POINT('Origin',(17.5,0.,0.));
#74454=CARTESIAN_POINT('',(0.600000000000001,-13.22226624086,-40.1803643021789));
#74455=CARTESIAN_POINT('Origin',(0.600000000000001,0.,0.));
#74456=CARTESIAN_POINT('',(1.67735469196905,-12.3365516130268,-40.4610861730024));
#74457=CARTESIAN_POINT('Origin',(8.14497546096349,0.,0.));
#74458=CARTESIAN_POINT('',(5.09593997529677,-12.3365516130268,-40.4610861730024));
#74459=CARTESIAN_POINT('',(17.5,-12.3365516130268,-40.4610861730024));
#74460=CARTESIAN_POINT('',(5.09944803334083,-12.8457455753269,-40.3023178069695));
#74461=CARTESIAN_POINT('Origin',(-0.840551718690874,0.,0.));
#74462=CARTESIAN_POINT('',(10.8302042597752,-13.1850308552912,-40.1925983403041));
#74463=CARTESIAN_POINT('Origin',(-62.7155570771055,0.,0.));
#74464=CARTESIAN_POINT('',(11.6618634261911,-12.9488045494888,-40.2693240660821));
#74465=CARTESIAN_POINT('Origin',(26.9856656232739,0.,0.));
#74466=CARTESIAN_POINT('',(12.3548486633046,-12.5735100877104,-40.3880779943072));
#74467=CARTESIAN_POINT('Origin',(20.8267261185512,0.,0.));
#74468=CARTESIAN_POINT('',(13.103292255208,-12.3365516130268,-40.4610861730024));
#74469=CARTESIAN_POINT('Origin',(25.13830739299,0.,0.));
#74470=CARTESIAN_POINT('',(21.896707744792,-12.3365516130268,-40.4610861730024));
#74471=CARTESIAN_POINT('',(17.5,-12.3365516130268,-40.4610861730024));
#74472=CARTESIAN_POINT('',(22.6451513366954,-12.5735100877104,-40.3880779943072));
#74473=CARTESIAN_POINT('Origin',(9.86169260701005,0.,0.));
#74474=CARTESIAN_POINT('',(23.3381365738089,-12.9488045494888,-40.2693240660821));
#74475=CARTESIAN_POINT('Origin',(14.1732738814488,0.,0.));
#74476=CARTESIAN_POINT('',(24.1697957402248,-13.1850308552912,-40.1925983403042));
#74477=CARTESIAN_POINT('Origin',(8.01433437672608,0.,0.));
#74478=CARTESIAN_POINT('',(29.9005519666592,-12.8457455753269,-40.3023178069695));
#74479=CARTESIAN_POINT('Origin',(97.7155570771054,0.,0.));
#74480=CARTESIAN_POINT('',(29.9040600247032,-12.3365516130268,-40.4610861730024));
#74481=CARTESIAN_POINT('Origin',(35.8405517186909,0.,0.));
#74482=CARTESIAN_POINT('',(17.5,-12.3365516130268,-40.4610861730024));
#74483=CARTESIAN_POINT('Origin',(33.1,-11.4462726220787,-36.2726528263519));
#74484=CARTESIAN_POINT('',(30.5247014514712,-11.409370947074,-36.0990440950346));
#74485=CARTESIAN_POINT('Origin',(30.5,-11.4462726220787,-36.2726528263519));
#74486=CARTESIAN_POINT('',(30.4955273645547,-11.9230551151638,-36.1329850680974));
#74487=CARTESIAN_POINT('Origin',(30.5,-11.9161189324716,-36.101642754689));
#74488=CARTESIAN_POINT('',(24.1012882089558,-12.3084785844451,-36.0428658633082));
#74489=CARTESIAN_POINT('Origin',(24.1,-12.291995980786,-35.9648346973588));
#74490=CARTESIAN_POINT('',(23.1004586919557,-12.0118963235317,-36.0755342895717));
#74491=CARTESIAN_POINT('Origin',(23.1,-12.0100881945502,-36.0674407403565));
#74492=CARTESIAN_POINT('',(22.399682944576,-11.6329963463162,-36.1988378309035));
#74493=CARTESIAN_POINT('Origin',(22.4,-11.6342111462359,-36.2042487976867));
#74494=CARTESIAN_POINT('',(21.7998387845652,-11.4447884936363,-36.2656705509953));
#74495=CARTESIAN_POINT('Origin',(21.8,-11.4462726220787,-36.2726528263519));
#74496=CARTESIAN_POINT('',(13.2021921742626,-11.4260917493401,-36.1777092848303));
#74497=CARTESIAN_POINT('Origin',(13.2,-11.4462726220787,-36.2726528263519));
#74498=CARTESIAN_POINT('',(12.6002487187375,-11.633258178775,-36.2000040861152));
#74499=CARTESIAN_POINT('Origin',(12.6,-11.6342111462359,-36.2042487976867));
#74500=CARTESIAN_POINT('',(11.8996457869536,-12.0114844755769,-36.0736907752397));
#74501=CARTESIAN_POINT('Origin',(11.9,-12.0100881945502,-36.0674407403565));
#74502=CARTESIAN_POINT('',(10.899790263986,-12.2946795482123,-35.9775391158784));
#74503=CARTESIAN_POINT('Origin',(10.9,-12.291995980786,-35.9648346973588));
#74504=CARTESIAN_POINT('',(4.55736144060343,-12.0050753064885,-36.5036071604488));
#74505=CARTESIAN_POINT('Origin',(4.5,-11.9161189324716,-36.101642754689));
#74506=CARTESIAN_POINT('',(4.49524972087093,-11.4391761461162,-36.2392665318678));
#74507=CARTESIAN_POINT('Origin',(4.5,-11.4462726220787,-36.2726528263519));
#74508=CARTESIAN_POINT('',(1.90350512467335,-11.4322568815947,-36.2067139516643));
#74509=CARTESIAN_POINT('Origin',(1.9,-11.4462726220787,-36.2726528263519));
#74510=CARTESIAN_POINT('Ctrl Pts',(0.138207714141628,-13.6777396430533,
-40.515309671231));
#74511=CARTESIAN_POINT('Ctrl Pts',(0.370217470898111,-13.4490085829891,
-40.3476538099283));
#74512=CARTESIAN_POINT('Ctrl Pts',(0.600000000000007,-13.22226624086,-40.1803643021789));
#74513=CARTESIAN_POINT('Origin',(1.9,-14.5472582706722,-35.1439863533772));
#74514=CARTESIAN_POINT('',(5.09593997529677,-16.5575380560557,-38.9247727484987));
#74515=CARTESIAN_POINT('',(17.5,-16.5575380560557,-38.9247727484987));
#74516=CARTESIAN_POINT('',(4.47529854852883,-14.4639330523272,-34.987274410005));
#74517=CARTESIAN_POINT('Origin',(4.5,-14.5472582706722,-35.1439863533772));
#74518=CARTESIAN_POINT('',(5.09944803334084,-16.0654185122698,-39.1304526938498));
#74519=CARTESIAN_POINT('Origin',(-0.840551718690874,0.,0.));
#74520=CARTESIAN_POINT('',(4.50447263544529,-14.0922449867892,-35.343464522354));
#74521=CARTESIAN_POINT('Origin',(4.5,-14.0774119602792,-35.31499642504));
#74522=CARTESIAN_POINT('',(10.8302042597752,-15.7349845952073,-39.2644910802189));
#74523=CARTESIAN_POINT('Origin',(-62.7155570771055,0.,0.));
#74524=CARTESIAN_POINT('',(10.8987117910442,-13.7390659716653,-35.5221746368434));
#74525=CARTESIAN_POINT('Origin',(10.9,-13.7015349119649,-35.4518044823703));
#74526=CARTESIAN_POINT('',(11.6618634261911,-15.96526278996,-39.1714230536436));
#74527=CARTESIAN_POINT('Origin',(26.9856656232739,0.,0.));
#74528=CARTESIAN_POINT('',(11.8995413080444,-13.9872600241959,-35.35656070068));
#74529=CARTESIAN_POINT('Origin',(11.9,-13.9834426982006,-35.3491984393726));
#74530=CARTESIAN_POINT('',(12.3548486633046,-16.3290885806033,-39.0211592104439));
#74531=CARTESIAN_POINT('Origin',(20.8267261185512,0.,0.));
#74532=CARTESIAN_POINT('',(12.600317055424,-14.3567722348383,-35.2074644826695));
#74533=CARTESIAN_POINT('Origin',(12.6,-14.359319746515,-35.2123903820423));
#74534=CARTESIAN_POINT('',(13.103292255208,-16.5575380560557,-38.9247727484987));
#74535=CARTESIAN_POINT('Origin',(25.13830739299,0.,0.));
#74536=CARTESIAN_POINT('',(13.2001612154348,-14.5439070589318,-35.137683640766));
#74537=CARTESIAN_POINT('Origin',(13.2,-14.5472582706722,-35.1439863533772));
#74538=CARTESIAN_POINT('',(21.896707744792,-16.5575380560557,-38.9247727484987));
#74539=CARTESIAN_POINT('',(17.5,-16.5575380560557,-38.9247727484987));
#74540=CARTESIAN_POINT('',(21.7978078257374,-14.501689183981,-35.0582833660355));
#74541=CARTESIAN_POINT('Origin',(21.8,-14.5472582706722,-35.1439863533772));
#74542=CARTESIAN_POINT('',(22.6451513366954,-16.3290885806033,-39.0211592104439));
#74543=CARTESIAN_POINT('Origin',(9.86169260701004,0.,0.));
#74544=CARTESIAN_POINT('',(22.3997512812625,-14.357321313938,-35.208526188654));
#74545=CARTESIAN_POINT('Origin',(22.4,-14.359319746515,-35.2123903820423));
#74546=CARTESIAN_POINT('',(23.3381365738089,-15.96526278996,-39.1714230536436));
#74547=CARTESIAN_POINT('Origin',(14.1732738814488,0.,0.));
#74548=CARTESIAN_POINT('',(23.1003542130464,-13.9863905298622,-35.3548837560077));
#74549=CARTESIAN_POINT('Origin',(23.1,-13.9834426982006,-35.3491984393726));
#74550=CARTESIAN_POINT('',(24.1697957402248,-15.7349845952073,-39.2644910802189));
#74551=CARTESIAN_POINT('Origin',(8.01433437672606,0.,0.));
#74552=CARTESIAN_POINT('',(24.100209736014,-13.7076454228629,-35.4632615954717));
#74553=CARTESIAN_POINT('Origin',(24.1,-13.7015349119649,-35.4518044823703));
#74554=CARTESIAN_POINT('',(29.9005519666592,-16.0654185122698,-39.1304526938498));
#74555=CARTESIAN_POINT('Origin',(97.7155570771054,0.,0.));
#74556=CARTESIAN_POINT('',(30.4426385593966,-14.267645163841,-35.6800990794245));
#74557=CARTESIAN_POINT('Origin',(30.5,-14.0774119602792,-35.31499642504));
#74558=CARTESIAN_POINT('',(29.9040600247032,-16.5575380560557,-38.9247727484987));
#74559=CARTESIAN_POINT('Origin',(35.8405517186909,0.,0.));
#74560=CARTESIAN_POINT('',(30.5047502791291,-14.5312341902212,-35.1138494411902));
#74561=CARTESIAN_POINT('Origin',(30.5,-14.5472582706722,-35.1439863533772));
#74562=CARTESIAN_POINT('',(17.5,-16.5575380560557,-38.9247727484987));
#74563=CARTESIAN_POINT('Origin',(17.5,-14.6213611271724,-40.1718595385976));
#74564=CARTESIAN_POINT('Origin',(17.5,0.,0.));
#74565=CARTESIAN_POINT('',(0.600000000000001,-19.9986373454573,-37.2739118462884));
#74566=CARTESIAN_POINT('Origin',(0.600000000000001,0.,0.));
#74567=CARTESIAN_POINT('',(1.67735469196905,-19.1751255543105,-37.7041716521717));
#74568=CARTESIAN_POINT('Origin',(8.14497546096349,0.,0.));
#74569=CARTESIAN_POINT('',(5.09593997529677,-19.1751255543105,-37.7041716521717));
#74570=CARTESIAN_POINT('',(17.5,-19.1751255543105,-37.7041716521717));
#74571=CARTESIAN_POINT('',(5.09944803334083,-19.6490138787379,-37.459394730737));
#74572=CARTESIAN_POINT('Origin',(-0.840551718690872,0.,0.));
#74573=CARTESIAN_POINT('',(10.8302042597752,-19.9640920674886,-37.2924258787336));
#74574=CARTESIAN_POINT('Origin',(-62.7155570771055,0.,0.));
#74575=CARTESIAN_POINT('',(11.6618634261911,-19.7447778525305,-37.4090062358548));
#74576=CARTESIAN_POINT('Origin',(26.9856656232739,0.,0.));
#74577=CARTESIAN_POINT('',(12.3548486633046,-19.3958063601357,-37.5911252244478));
#74578=CARTESIAN_POINT('Origin',(20.8267261185512,0.,0.));
#74579=CARTESIAN_POINT('',(13.103292255208,-19.1751255543105,-37.7041716521717));
#74580=CARTESIAN_POINT('Origin',(25.13830739299,0.,0.));
#74581=CARTESIAN_POINT('',(21.896707744792,-19.1751255543105,-37.7041716521717));
#74582=CARTESIAN_POINT('',(17.5,-19.1751255543105,-37.7041716521717));
#74583=CARTESIAN_POINT('',(22.6451513366954,-19.3958063601357,-37.5911252244478));
#74584=CARTESIAN_POINT('Origin',(9.86169260701006,0.,0.));
#74585=CARTESIAN_POINT('',(23.3381365738089,-19.7447778525305,-37.4090062358548));
#74586=CARTESIAN_POINT('Origin',(14.1732738814488,0.,0.));
#74587=CARTESIAN_POINT('',(24.1697957402248,-19.9640920674886,-37.2924258787336));
#74588=CARTESIAN_POINT('Origin',(8.01433437672609,0.,0.));
#74589=CARTESIAN_POINT('',(29.9005519666592,-19.6490138787379,-37.459394730737));
#74590=CARTESIAN_POINT('Origin',(97.7155570771054,0.,0.));
#74591=CARTESIAN_POINT('',(29.9040600247032,-19.1751255543105,-37.7041716521717));
#74592=CARTESIAN_POINT('Origin',(35.8405517186909,0.,0.));
#74593=CARTESIAN_POINT('',(17.5,-19.1751255543105,-37.7041716521717));
#74594=CARTESIAN_POINT('Origin',(33.1,-17.5710580837557,-33.7339653438087));
#74595=CARTESIAN_POINT('',(30.5247014514712,-17.5045701882916,-33.5694020278342));
#74596=CARTESIAN_POINT('Origin',(30.5,-17.5710580837557,-33.7339653438087));
#74597=CARTESIAN_POINT('',(30.4955273645547,-18.0163441277467,-33.5136270415661));
#74598=CARTESIAN_POINT('Origin',(30.5,-18.0040707856479,-33.4839653438087));
#74599=CARTESIAN_POINT('',(24.1012882089558,-18.3802631128034,-33.3579488669236));
#74600=CARTESIAN_POINT('Origin',(24.1,-18.3504809471617,-33.2839653438087));
#74601=CARTESIAN_POINT('',(23.1004586919557,-18.0938594155378,-33.4416219555226));
#74602=CARTESIAN_POINT('Origin',(23.1,-18.0906733260264,-33.4339653438087));
#74603=CARTESIAN_POINT('',(22.399682944576,-17.742127215612,-33.6288475295615));
#74604=CARTESIAN_POINT('Origin',(22.4,-17.7442631645126,-33.6339653438087));
#74605=CARTESIAN_POINT('',(21.7998387845652,-17.5683840431675,-33.7273468611033));
#74606=CARTESIAN_POINT('Origin',(21.8,-17.5710580837557,-33.7339653438087));
#74607=CARTESIAN_POINT('',(13.2021921742626,-17.5346970308537,-33.6439685797945));
#74608=CARTESIAN_POINT('Origin',(13.2,-17.5710580837557,-33.7339653438087));
#74609=CARTESIAN_POINT('',(12.6002487187375,-17.7425875883397,-33.6299506000067));
#74610=CARTESIAN_POINT('Origin',(12.6,-17.7442631645126,-33.6339653438087));
#74611=CARTESIAN_POINT('',(11.8996457869536,-18.0931337015746,-33.4398779649625));
#74612=CARTESIAN_POINT('Origin',(11.9,-18.0906733260264,-33.4339653438087));
#74613=CARTESIAN_POINT('',(10.899790263986,-18.3553298442931,-33.2960107570711));
#74614=CARTESIAN_POINT('Origin',(10.9,-18.3504809471617,-33.2839653438087));
#74615=CARTESIAN_POINT('',(4.55736144060343,-18.1614760990067,-33.8643758947959));
#74616=CARTESIAN_POINT('Origin',(4.5,-18.0040707856479,-33.4839653438087));
#74617=CARTESIAN_POINT('',(4.49524972087093,-17.5582719500126,-33.7023185522751));
#74618=CARTESIAN_POINT('Origin',(4.5,-17.5710580837557,-33.7339653438087));
#74619=CARTESIAN_POINT('',(1.90350512467335,-17.5458051084359,-33.6714620365851));
#74620=CARTESIAN_POINT('Origin',(1.9,-17.5710580837557,-33.7339653438087));
#74621=CARTESIAN_POINT('Ctrl Pts',(0.138207714141623,-20.505353736182,-37.5246765162998));
#74622=CARTESIAN_POINT('Ctrl Pts',(0.370217470901057,-20.2509844800824,
-37.3992864560054));
#74623=CARTESIAN_POINT('Ctrl Pts',(0.600000000000006,-19.9986373454573,
-37.2739118462884));
#74624=CARTESIAN_POINT('Origin',(1.9,-20.4289419162443,-32.0839653438087));
#74625=CARTESIAN_POINT('',(5.09593997529677,-23.0652077022745,-35.4582316768749));
#74626=CARTESIAN_POINT('',(17.5,-23.0652077022745,-35.4582316768749));
#74627=CARTESIAN_POINT('',(4.47529854852883,-20.3196698518115,-31.9441034793054));
#74628=CARTESIAN_POINT('Origin',(4.5,-20.4289419162443,-32.0839653438087));
#74629=CARTESIAN_POINT('',(5.09944803334083,-22.6162805078382,-35.7462425436685));
#74630=CARTESIAN_POINT('Origin',(-0.840551718690874,0.,0.));
#74631=CARTESIAN_POINT('',(4.50447263544529,-20.01548032708,-32.3594252187343));
#74632=CARTESIAN_POINT('Origin',(4.5,-19.9959292143521,-32.3339653438087));
#74633=CARTESIAN_POINT('',(10.8302042597752,-22.3141421459872,-35.9356238333033));
#74634=CARTESIAN_POINT('Origin',(-62.7155570771054,0.,0.));
#74635=CARTESIAN_POINT('',(10.8987117910442,-19.6986995804965,-32.5967492173915));
#74636=CARTESIAN_POINT('Origin',(10.9,-19.6495190528383,-32.5339653438087));
#74637=CARTESIAN_POINT('',(11.6618634261911,-22.5247608043155,-35.8039823302991));
#74638=CARTESIAN_POINT('Origin',(26.9856656232739,0.,0.));
#74639=CARTESIAN_POINT('',(11.8995413080444,-19.9143644494692,-32.3905528841213));
#74640=CARTESIAN_POINT('Origin',(11.9,-19.9093266739737,-32.3839653438087));
#74641=CARTESIAN_POINT('',(12.3548486633046,-22.856966221146,-35.5928236469852));
#74642=CARTESIAN_POINT('Origin',(20.8267261185512,0.,0.));
#74643=CARTESIAN_POINT('',(12.600317055424,-20.2523726527879,-32.179556650676));
#74644=CARTESIAN_POINT('Origin',(12.6,-20.2557368354875,-32.1839653438087));
#74645=CARTESIAN_POINT('',(13.103292255208,-23.0652077022745,-35.4582316768749));
#74646=CARTESIAN_POINT('Origin',(25.13830739299,0.,0.));
#74647=CARTESIAN_POINT('',(13.2001612154348,-20.4245471623811,-32.0783403153759));
#74648=CARTESIAN_POINT('Origin',(13.2,-20.4289419162443,-32.0839653438087));
#74649=CARTESIAN_POINT('',(21.896707744792,-23.0652077022745,-35.4582316768749));
#74650=CARTESIAN_POINT('',(17.5,-23.0652077022745,-35.4582316768749));
#74651=CARTESIAN_POINT('',(21.7978078257374,-20.3691829588007,-32.0074773662801));
#74652=CARTESIAN_POINT('Origin',(21.8,-20.4289419162443,-32.0839653438087));
#74653=CARTESIAN_POINT('',(22.6451513366954,-22.856966221146,-35.5928236469852));
#74654=CARTESIAN_POINT('Origin',(9.86169260701005,0.,0.));
#74655=CARTESIAN_POINT('',(22.3997512812625,-20.2530977534517,-32.180506880376));
#74656=CARTESIAN_POINT('Origin',(22.4,-20.2557368354875,-32.1839653438087));
#74657=CARTESIAN_POINT('',(23.3381365738089,-22.5247608043155,-35.8039823302991));
#74658=CARTESIAN_POINT('Origin',(14.1732738814488,0.,0.));
#74659=CARTESIAN_POINT('',(23.1003542130464,-19.9132169663217,-32.3890524021132));
#74660=CARTESIAN_POINT('Origin',(23.1,-19.9093266739737,-32.3839653438087));
#74661=CARTESIAN_POINT('',(24.1697957402248,-22.3141421459872,-35.9356238333033));
#74662=CARTESIAN_POINT('Origin',(8.01433437672607,0.,0.));
#74663=CARTESIAN_POINT('',(24.100209736014,-19.657526238157,-32.544187318536));
#74664=CARTESIAN_POINT('Origin',(24.1,-19.6495190528383,-32.5339653438087));
#74665=CARTESIAN_POINT('',(29.9005519666592,-22.6162805078382,-35.7462425436685));
#74666=CARTESIAN_POINT('Origin',(97.7155570771054,0.,0.));
#74667=CARTESIAN_POINT('',(30.4426385593966,-20.2466717586954,-32.6604876193616));
#74668=CARTESIAN_POINT('Origin',(30.5,-19.9959292143521,-32.3339653438087));
#74669=CARTESIAN_POINT('',(29.9040600247032,-23.0652077022745,-35.4582316768749));
#74670=CARTESIAN_POINT('Origin',(35.8405517186909,0.,0.));
#74671=CARTESIAN_POINT('',(30.5047502791291,-20.4079280576996,-32.0570688314042));
#74672=CARTESIAN_POINT('Origin',(30.5,-20.4289419162443,-32.0839653438087));
#74673=CARTESIAN_POINT('',(17.5,-23.0652077022745,-35.4582316768749));
#74674=CARTESIAN_POINT('Origin',(17.5,-21.375,-37.0225860117847));
#74675=CARTESIAN_POINT('Origin',(17.5,0.,0.));
#74676=CARTESIAN_POINT('',(0.600000000000001,-26.1673599741116,-33.234910440458));
#74677=CARTESIAN_POINT('Origin',(0.600000000000001,0.,0.));
#74678=CARTESIAN_POINT('',(1.67735469196904,-25.4310730087083,-33.8016349549212));
#74679=CARTESIAN_POINT('Origin',(8.14497546096349,0.,0.));
#74680=CARTESIAN_POINT('',(5.09593997529677,-25.4310730087083,-33.8016349549212));
#74681=CARTESIAN_POINT('',(17.5,-25.4310730087083,-33.8016349549212));
#74682=CARTESIAN_POINT('',(5.09944803334083,-25.8552568383243,-33.4782869009794));
#74683=CARTESIAN_POINT('Origin',(-0.840551718690872,0.,0.));
#74684=CARTESIAN_POINT('',(10.8302042597752,-26.1365544445335,-33.2591419277157));
#74685=CARTESIAN_POINT('Origin',(-62.7155570771055,0.,0.));
#74686=CARTESIAN_POINT('',(11.6618634261911,-25.9408160718628,-33.4120346810215));
#74687=CARTESIAN_POINT('Origin',(26.9856656232739,0.,0.));
#74688=CARTESIAN_POINT('',(12.3548486633046,-25.6287708710599,-33.6519851366708));
#74689=CARTESIAN_POINT('Origin',(20.8267261185512,0.,0.));
#74690=CARTESIAN_POINT('',(13.103292255208,-25.4310730087083,-33.8016349549212));
#74691=CARTESIAN_POINT('Origin',(25.13830739299,0.,0.));
#74692=CARTESIAN_POINT('',(21.896707744792,-25.4310730087083,-33.8016349549212));
#74693=CARTESIAN_POINT('',(17.5,-25.4310730087083,-33.8016349549212));
#74694=CARTESIAN_POINT('',(22.6451513366954,-25.6287708710599,-33.6519851366708));
#74695=CARTESIAN_POINT('Origin',(9.86169260701005,0.,0.));
#74696=CARTESIAN_POINT('',(23.3381365738089,-25.9408160718628,-33.4120346810215));
#74697=CARTESIAN_POINT('Origin',(14.1732738814488,0.,0.));
#74698=CARTESIAN_POINT('',(24.1697957402248,-26.1365544445335,-33.2591419277157));
#74699=CARTESIAN_POINT('Origin',(8.01433437672609,0.,0.));
#74700=CARTESIAN_POINT('',(29.9005519666592,-25.8552568383243,-33.4782869009794));
#74701=CARTESIAN_POINT('Origin',(97.7155570771054,0.,0.));
#74702=CARTESIAN_POINT('',(29.9040600247032,-25.4310730087083,-33.8016349549212));
#74703=CARTESIAN_POINT('Origin',(35.8405517186909,0.,0.));
#74704=CARTESIAN_POINT('',(17.5,-25.4310730087083,-33.8016349549212));
#74705=CARTESIAN_POINT('Origin',(33.1,-23.1619558369422,-30.1702883945039));
#74706=CARTESIAN_POINT('',(30.5247014514712,-23.0679019220779,-30.0197706669552));
#74707=CARTESIAN_POINT('Origin',(30.5,-23.1619558369422,-30.1702883945039));
#74708=CARTESIAN_POINT('',(30.4955273645547,-23.562215640718,-29.8759744160904));
#74709=CARTESIAN_POINT('Origin',(30.5,-23.5449780585017,-29.8488945896607));
#74710=CARTESIAN_POINT('',(24.1012882089558,-23.893572647341,-29.6594674741542));
#74711=CARTESIAN_POINT('Origin',(24.1,-23.8513958357493,-29.5917795457861));
#74712=CARTESIAN_POINT('',(23.1004586919557,-23.6260497451375,-29.7916028606322));
#74713=CARTESIAN_POINT('Origin',(23.1,-23.6215825028136,-29.784615828692));
#74714=CARTESIAN_POINT('',(22.399682944576,-23.312172527411,-30.0370617130518));
#74715=CARTESIAN_POINT('Origin',(22.4,-23.315164725566,-30.0417308725666));
#74716=CARTESIAN_POINT('',(21.7998387845652,-23.1581731335784,-30.1642348036977));
#74717=CARTESIAN_POINT('Origin',(21.8,-23.1619558369422,-30.1702883945039));
#74718=CARTESIAN_POINT('',(13.2021921742626,-23.1105194160696,-30.0879729141313));
#74719=CARTESIAN_POINT('Origin',(13.2,-23.1619558369422,-30.1702883945039));
#74720=CARTESIAN_POINT('',(12.6002487187375,-23.3128174522151,-30.038068082493));
#74721=CARTESIAN_POINT('Origin',(12.6,-23.315164725566,-30.0417308725666));
#74722=CARTESIAN_POINT('',(11.8996457869536,-23.6250322156174,-29.7900113841146));
#74723=CARTESIAN_POINT('Origin',(11.9,-23.6215825028136,-29.784615828692));
#74724=CARTESIAN_POINT('',(10.899790263986,-23.8582627313001,-29.6027999600046));
#74725=CARTESIAN_POINT('Origin',(10.9,-23.8513958357493,-29.5917795457861));
#74726=CARTESIAN_POINT('',(4.55736144060343,-23.7660496304069,-30.1961927037808));
#74727=CARTESIAN_POINT('Origin',(4.5,-23.5449780585017,-29.8488945896607));
#74728=CARTESIAN_POINT('',(4.49524972087093,-23.1438685456221,-30.1413426776676));
#74729=CARTESIAN_POINT('Origin',(4.5,-23.1619558369422,-30.1702883945039));
#74730=CARTESIAN_POINT('',(1.90350512467335,-23.1262329256631,-30.1131197861062));
#74731=CARTESIAN_POINT('Origin',(1.9,-23.1619558369422,-30.1702883945039));
#74732=CARTESIAN_POINT('Ctrl Pts',(0.138207714141625,-26.7099230322463,
-33.3938750538235));
#74733=CARTESIAN_POINT('Ctrl Pts',(0.370217470898728,-26.4376444612466,
-33.3145607080718));
#74734=CARTESIAN_POINT('Ctrl Pts',(0.600000000000006,-26.1673599741116,
-33.234910440458));
#74735=CARTESIAN_POINT('Origin',(1.9,-25.6899024992348,-28.0490892825384));
#74736=CARTESIAN_POINT('',(5.09593997529677,-28.872052684018,-30.9143101784803));
#74737=CARTESIAN_POINT('',(17.5,-28.872052684018,-30.9143101784803));
#74738=CARTESIAN_POINT('',(4.47529854852883,-25.5580037650976,-27.9303271288835));
#74739=CARTESIAN_POINT('Origin',(4.5,-25.6899024992348,-28.0490892825384));
#74740=CARTESIAN_POINT('',(5.09944803334083,-28.4799582645661,-31.2759009022694));
#74741=CARTESIAN_POINT('Origin',(-0.840551718690874,0.,0.));
#74742=CARTESIAN_POINT('',(4.50447263544529,-25.3305554259542,-28.3921611545025));
#74743=CARTESIAN_POINT('Origin',(4.5,-25.3068802776753,-28.3704830873816));
#74744=CARTESIAN_POINT('',(10.8302042597752,-28.2152957791621,-31.5148708405159));
#74745=CARTESIAN_POINT('Origin',(-62.7155570771053,0.,0.));
#74746=CARTESIAN_POINT('',(10.8987117910442,-25.0597981705973,-28.6808880677203));
#74747=CARTESIAN_POINT('Origin',(10.9,-25.0004625004277,-28.6275981312563));
#74748=CARTESIAN_POINT('',(11.6618634261911,-28.3998553597108,-31.3486557215378));
#74749=CARTESIAN_POINT('Origin',(26.9856656232739,0.,0.));
#74750=CARTESIAN_POINT('',(11.8995413080444,-25.2363809880999,-28.4403745085892));
#74751=CARTESIAN_POINT('Origin',(11.9,-25.2302758333634,-28.4347618483503));
#74752=CARTESIAN_POINT('',(12.3548486633046,-28.6903465092421,-31.0830181478507));
#74753=CARTESIAN_POINT('Origin',(20.8267261185512,0.,0.));
#74754=CARTESIAN_POINT('',(12.600317055424,-25.5326149758775,-28.1738892734932));
#74755=CARTESIAN_POINT('Origin',(12.6,-25.536693610611,-28.1776468044757));
#74756=CARTESIAN_POINT('',(13.103292255208,-28.872052684018,-30.9143101784803));
#74757=CARTESIAN_POINT('Origin',(25.13830739299,0.,0.));
#74758=CARTESIAN_POINT('',(13.2001612154348,-25.684597735621,-28.0443128519265));
#74759=CARTESIAN_POINT('Origin',(13.2,-25.6899024992348,-28.0490892825384));
#74760=CARTESIAN_POINT('',(21.896707744792,-28.872052684018,-30.9143101784803));
#74761=CARTESIAN_POINT('',(17.5,-28.872052684018,-30.9143101784803));
#74762=CARTESIAN_POINT('',(21.7978078257374,-25.6177694167211,-27.9841403633154));
#74763=CARTESIAN_POINT('Origin',(21.8,-25.6899024992348,-28.0490892825384));
#74764=CARTESIAN_POINT('',(22.6451513366954,-28.6903465092421,-31.0830181478507));
#74765=CARTESIAN_POINT('Origin',(9.86169260701004,0.,0.));
#74766=CARTESIAN_POINT('',(22.3997512812625,-25.5334940662887,-28.1746991546599));
#74767=CARTESIAN_POINT('Origin',(22.4,-25.536693610611,-28.1776468044757));
#74768=CARTESIAN_POINT('',(23.3381365738089,-28.3998553597108,-31.3486557215378));
#74769=CARTESIAN_POINT('Origin',(14.1732738814488,0.,0.));
#74770=CARTESIAN_POINT('',(23.1003542130464,-25.2349903818335,-28.4390960806318));
#74771=CARTESIAN_POINT('Origin',(23.1,-25.2302758333634,-28.4347618483503));
#74772=CARTESIAN_POINT('',(24.1697957402248,-28.2152957791621,-31.5148708405159));
#74773=CARTESIAN_POINT('Origin',(8.01433437672607,0.,0.));
#74774=CARTESIAN_POINT('',(24.100209736014,-25.0101230658929,-28.63627437808));
#74775=CARTESIAN_POINT('Origin',(24.1,-25.0004625004277,-28.6275981312563));
#74776=CARTESIAN_POINT('',(29.9005519666592,-28.4799582645661,-31.2759009022694));
#74777=CARTESIAN_POINT('Origin',(97.7155570771054,0.,0.));
#74778=CARTESIAN_POINT('',(30.4426385593966,-25.610513477472,-28.6485037699886));
#74779=CARTESIAN_POINT('Origin',(30.5,-25.3068802776753,-28.3704830873816));
#74780=CARTESIAN_POINT('',(29.9040600247032,-28.872052684018,-30.9143101784803));
#74781=CARTESIAN_POINT('Origin',(35.8405517186909,0.,0.));
#74782=CARTESIAN_POINT('',(30.5047502791291,-25.6645373580546,-28.0262504068355));
#74783=CARTESIAN_POINT('Origin',(30.5,-25.6899024992348,-28.0490892825384));
#74784=CARTESIAN_POINT('',(17.5,-28.872052684018,-30.9143101784803));
#74785=CARTESIAN_POINT('Origin',(17.5,-27.4791703140996,-32.7483999433363));
#74786=CARTESIAN_POINT('Origin',(17.5,0.,0.));
#74787=CARTESIAN_POINT('',(0.600000000000001,-31.5410006112756,-28.1860830985703));
#74788=CARTESIAN_POINT('Origin',(0.600000000000001,0.,0.));
#74789=CARTESIAN_POINT('',(1.67735469196904,-30.9143101784803,-28.872052684018));
#74790=CARTESIAN_POINT('Origin',(8.14497546096349,0.,0.));
#74791=CARTESIAN_POINT('',(5.09593997529677,-30.9143101784803,-28.872052684018));
#74792=CARTESIAN_POINT('',(17.5,-30.9143101784803,-28.872052684018));
#74793=CARTESIAN_POINT('',(5.09944803334083,-31.2759009022694,-28.4799582645661));
#74794=CARTESIAN_POINT('Origin',(-0.840551718690872,0.,0.));
#74795=CARTESIAN_POINT('',(10.8302042597752,-31.5148708405159,-28.2152957791621));
#74796=CARTESIAN_POINT('Origin',(-62.7155570771055,0.,0.));
#74797=CARTESIAN_POINT('',(11.6618634261911,-31.3486557215378,-28.3998553597108));
#74798=CARTESIAN_POINT('Origin',(26.9856656232739,0.,0.));
#74799=CARTESIAN_POINT('',(12.3548486633046,-31.0830181478507,-28.6903465092421));
#74800=CARTESIAN_POINT('Origin',(20.8267261185512,0.,0.));
#74801=CARTESIAN_POINT('',(13.103292255208,-30.9143101784803,-28.872052684018));
#74802=CARTESIAN_POINT('Origin',(25.13830739299,0.,0.));
#74803=CARTESIAN_POINT('',(21.896707744792,-30.9143101784803,-28.872052684018));
#74804=CARTESIAN_POINT('',(17.5,-30.9143101784803,-28.872052684018));
#74805=CARTESIAN_POINT('',(22.6451513366954,-31.0830181478507,-28.6903465092421));
#74806=CARTESIAN_POINT('Origin',(9.86169260701006,0.,0.));
#74807=CARTESIAN_POINT('',(23.3381365738089,-31.3486557215378,-28.3998553597108));
#74808=CARTESIAN_POINT('Origin',(14.1732738814488,0.,0.));
#74809=CARTESIAN_POINT('',(24.1697957402248,-31.5148708405159,-28.2152957791621));
#74810=CARTESIAN_POINT('Origin',(8.01433437672608,0.,0.));
#74811=CARTESIAN_POINT('',(29.9005519666592,-31.2759009022694,-28.4799582645661));
#74812=CARTESIAN_POINT('Origin',(97.7155570771054,0.,0.));
#74813=CARTESIAN_POINT('',(29.9040600247032,-30.9143101784803,-28.872052684018));
#74814=CARTESIAN_POINT('Origin',(35.8405517186909,0.,0.));
#74815=CARTESIAN_POINT('',(17.5,-30.9143101784803,-28.872052684018));
#74816=CARTESIAN_POINT('Origin',(33.1,-28.0490892825384,-25.6899024992348));
#74817=CARTESIAN_POINT('',(30.5247014514712,-27.9303271288835,-25.5580037650976));
#74818=CARTESIAN_POINT('Origin',(30.5,-28.0490892825384,-25.6899024992348));
#74819=CARTESIAN_POINT('',(30.4955273645547,-28.3921611545025,-25.3305554259542));
#74820=CARTESIAN_POINT('Origin',(30.5,-28.3704830873816,-25.3068802776753));
#74821=CARTESIAN_POINT('',(24.1012882089558,-28.6808880677203,-25.0597981705973));
#74822=CARTESIAN_POINT('Origin',(24.1,-28.6275981312563,-25.0004625004277));
#74823=CARTESIAN_POINT('',(23.1004586919557,-28.4403745085892,-25.2363809880999));
#74824=CARTESIAN_POINT('Origin',(23.1,-28.4347618483503,-25.2302758333634));
#74825=CARTESIAN_POINT('',(22.399682944576,-28.1738892734932,-25.5326149758775));
#74826=CARTESIAN_POINT('Origin',(22.4,-28.1776468044757,-25.536693610611));
#74827=CARTESIAN_POINT('',(21.7998387845652,-28.0443128519265,-25.684597735621));
#74828=CARTESIAN_POINT('Origin',(21.8,-28.0490892825384,-25.6899024992348));
#74829=CARTESIAN_POINT('',(13.2021921742626,-27.9841403633154,-25.6177694167211));
#74830=CARTESIAN_POINT('Origin',(13.2,-28.0490892825384,-25.6899024992348));
#74831=CARTESIAN_POINT('',(12.6002487187375,-28.1746991546599,-25.5334940662887));
#74832=CARTESIAN_POINT('Origin',(12.6,-28.1776468044757,-25.536693610611));
#74833=CARTESIAN_POINT('',(11.8996457869536,-28.4390960806318,-25.2349903818335));
#74834=CARTESIAN_POINT('Origin',(11.9,-28.4347618483503,-25.2302758333634));
#74835=CARTESIAN_POINT('',(10.899790263986,-28.63627437808,-25.0101230658929));
#74836=CARTESIAN_POINT('Origin',(10.9,-28.6275981312563,-25.0004625004277));
#74837=CARTESIAN_POINT('',(4.55736144060343,-28.6485037699886,-25.610513477472));
#74838=CARTESIAN_POINT('Origin',(4.5,-28.3704830873816,-25.3068802776753));
#74839=CARTESIAN_POINT('',(4.49524972087093,-28.0262504068355,-25.6645373580546));
#74840=CARTESIAN_POINT('Origin',(4.5,-28.0490892825384,-25.6899024992348));
#74841=CARTESIAN_POINT('',(1.90350512467335,-28.0039818578826,-25.6398056289004));
#74842=CARTESIAN_POINT('Origin',(1.9,-28.0490892825384,-25.6899024992348));
#74843=CARTESIAN_POINT('Ctrl Pts',(0.138207714141624,-32.1029248328492,
-28.2484175959527));
#74844=CARTESIAN_POINT('Ctrl Pts',(0.370217470897375,-31.8210099935485,
-28.2175888910035));
#74845=CARTESIAN_POINT('Ctrl Pts',(0.600000000000006,-31.5410006112756,
-28.1860830985703));
#74846=CARTESIAN_POINT('Origin',(1.9,-30.170288394504,-23.1619558369422));
#74847=CARTESIAN_POINT('',(5.09593997529677,-33.8016349549212,-25.4310730087083));
#74848=CARTESIAN_POINT('',(17.5,-33.8016349549212,-25.4310730087083));
#74849=CARTESIAN_POINT('',(4.47529854852883,-30.0197706669552,-23.0679019220779));
#74850=CARTESIAN_POINT('Origin',(4.5,-30.170288394504,-23.1619558369422));
#74851=CARTESIAN_POINT('',(5.09944803334083,-33.4782869009794,-25.8552568383243));
#74852=CARTESIAN_POINT('Origin',(-0.840551718690874,0.,0.));
#74853=CARTESIAN_POINT('',(4.50447263544529,-29.8759744160904,-23.562215640718));
#74854=CARTESIAN_POINT('Origin',(4.5,-29.8488945896607,-23.5449780585017));
#74855=CARTESIAN_POINT('',(10.8302042597752,-33.2591419277157,-26.1365544445334));
#74856=CARTESIAN_POINT('Origin',(-62.7155570771055,0.,0.));
#74857=CARTESIAN_POINT('',(10.8987117910442,-29.6594674741542,-23.893572647341));
#74858=CARTESIAN_POINT('Origin',(10.9,-29.5917795457861,-23.8513958357493));
#74859=CARTESIAN_POINT('',(11.6618634261911,-33.4120346810215,-25.9408160718628));
#74860=CARTESIAN_POINT('Origin',(26.9856656232739,0.,0.));
#74861=CARTESIAN_POINT('',(11.8995413080444,-29.7916028606322,-23.6260497451375));
#74862=CARTESIAN_POINT('Origin',(11.9,-29.784615828692,-23.6215825028136));
#74863=CARTESIAN_POINT('',(12.3548486633046,-33.6519851366708,-25.6287708710599));
#74864=CARTESIAN_POINT('Origin',(20.8267261185512,0.,0.));
#74865=CARTESIAN_POINT('',(12.600317055424,-30.0370617130518,-23.312172527411));
#74866=CARTESIAN_POINT('Origin',(12.6,-30.0417308725667,-23.315164725566));
#74867=CARTESIAN_POINT('',(13.103292255208,-33.8016349549212,-25.4310730087083));
#74868=CARTESIAN_POINT('Origin',(25.13830739299,0.,0.));
#74869=CARTESIAN_POINT('',(13.2001612154348,-30.1642348036977,-23.1581731335784));
#74870=CARTESIAN_POINT('Origin',(13.2,-30.170288394504,-23.1619558369422));
#74871=CARTESIAN_POINT('',(21.896707744792,-33.8016349549212,-25.4310730087083));
#74872=CARTESIAN_POINT('',(17.5,-33.8016349549212,-25.4310730087083));
#74873=CARTESIAN_POINT('',(21.7978078257374,-30.0879729141313,-23.1105194160696));
#74874=CARTESIAN_POINT('Origin',(21.8,-30.170288394504,-23.1619558369422));
#74875=CARTESIAN_POINT('',(22.6451513366954,-33.6519851366708,-25.6287708710599));
#74876=CARTESIAN_POINT('Origin',(9.86169260701005,0.,0.));
#74877=CARTESIAN_POINT('',(22.3997512812625,-30.0380680824931,-23.3128174522151));
#74878=CARTESIAN_POINT('Origin',(22.4,-30.0417308725667,-23.315164725566));
#74879=CARTESIAN_POINT('',(23.3381365738089,-33.4120346810215,-25.9408160718628));
#74880=CARTESIAN_POINT('Origin',(14.1732738814488,0.,0.));
#74881=CARTESIAN_POINT('',(23.1003542130464,-29.7900113841146,-23.6250322156174));
#74882=CARTESIAN_POINT('Origin',(23.1,-29.784615828692,-23.6215825028136));
#74883=CARTESIAN_POINT('',(24.1697957402248,-33.2591419277157,-26.1365544445335));
#74884=CARTESIAN_POINT('Origin',(8.01433437672607,0.,0.));
#74885=CARTESIAN_POINT('',(24.100209736014,-29.6027999600046,-23.8582627313001));
#74886=CARTESIAN_POINT('Origin',(24.1,-29.5917795457861,-23.8513958357493));
#74887=CARTESIAN_POINT('',(29.9005519666592,-33.4782869009794,-25.8552568383243));
#74888=CARTESIAN_POINT('Origin',(97.7155570771054,0.,0.));
#74889=CARTESIAN_POINT('',(30.4426385593966,-30.1961927037808,-23.7660496304069));
#74890=CARTESIAN_POINT('Origin',(30.5,-29.8488945896607,-23.5449780585017));
#74891=CARTESIAN_POINT('',(29.9040600247032,-33.8016349549212,-25.4310730087083));
#74892=CARTESIAN_POINT('Origin',(35.8405517186909,0.,0.));
#74893=CARTESIAN_POINT('',(30.5047502791291,-30.1413426776677,-23.1438685456221));
#74894=CARTESIAN_POINT('Origin',(30.5,-30.170288394504,-23.1619558369422));
#74895=CARTESIAN_POINT('',(17.5,-33.8016349549212,-25.4310730087083));
#74896=CARTESIAN_POINT('Origin',(17.5,-32.7483999433363,-27.4791703140996));
#74897=CARTESIAN_POINT('Origin',(17.5,0.,0.));
#74898=CARTESIAN_POINT('',(0.600000000000001,-35.9562839053824,-22.2808358845789));
#74899=CARTESIAN_POINT('Origin',(0.600000000000001,0.,0.));
#74900=CARTESIAN_POINT('',(1.67735469196904,-35.4582316768749,-23.0652077022745));
#74901=CARTESIAN_POINT('Origin',(8.14497546096349,0.,0.));
#74902=CARTESIAN_POINT('',(5.09593997529677,-35.4582316768749,-23.0652077022745));
#74903=CARTESIAN_POINT('',(17.5,-35.4582316768749,-23.0652077022745));
#74904=CARTESIAN_POINT('',(5.09944803334083,-35.7462425436685,-22.6162805078382));
#74905=CARTESIAN_POINT('Origin',(-0.840551718690872,0.,0.));
#74906=CARTESIAN_POINT('',(10.8302042597752,-35.9356238333033,-22.3141421459872));
#74907=CARTESIAN_POINT('Origin',(-62.7155570771054,0.,0.));
#74908=CARTESIAN_POINT('',(11.6618634261911,-35.8039823302992,-22.5247608043154));
#74909=CARTESIAN_POINT('Origin',(26.9856656232739,0.,0.));
#74910=CARTESIAN_POINT('',(12.3548486633046,-35.5928236469852,-22.856966221146));
#74911=CARTESIAN_POINT('Origin',(20.8267261185512,0.,0.));
#74912=CARTESIAN_POINT('',(13.103292255208,-35.4582316768749,-23.0652077022745));
#74913=CARTESIAN_POINT('Origin',(25.13830739299,0.,0.));
#74914=CARTESIAN_POINT('',(21.896707744792,-35.4582316768749,-23.0652077022745));
#74915=CARTESIAN_POINT('',(17.5,-35.4582316768749,-23.0652077022745));
#74916=CARTESIAN_POINT('',(22.6451513366954,-35.5928236469852,-22.856966221146));
#74917=CARTESIAN_POINT('Origin',(9.86169260701006,0.,0.));
#74918=CARTESIAN_POINT('',(23.3381365738089,-35.8039823302992,-22.5247608043154));
#74919=CARTESIAN_POINT('Origin',(14.1732738814488,0.,0.));
#74920=CARTESIAN_POINT('',(24.1697957402248,-35.9356238333033,-22.3141421459872));
#74921=CARTESIAN_POINT('Origin',(8.0143343767261,0.,0.));
#74922=CARTESIAN_POINT('',(29.9005519666592,-35.7462425436685,-22.6162805078382));
#74923=CARTESIAN_POINT('Origin',(97.7155570771053,0.,0.));
#74924=CARTESIAN_POINT('',(29.9040600247032,-35.4582316768749,-23.0652077022745));
#74925=CARTESIAN_POINT('Origin',(35.8405517186909,0.,0.));
#74926=CARTESIAN_POINT('',(17.5,-35.4582316768749,-23.0652077022745));
#74927=CARTESIAN_POINT('Origin',(33.1,-32.0839653438087,-20.4289419162443));
#74928=CARTESIAN_POINT('',(30.5247014514712,-31.9441034793054,-20.3196698518115));
#74929=CARTESIAN_POINT('Origin',(30.5,-32.0839653438087,-20.4289419162443));
#74930=CARTESIAN_POINT('',(30.4955273645547,-32.3594252187343,-20.01548032708));
#74931=CARTESIAN_POINT('Origin',(30.5,-32.3339653438087,-19.9959292143521));
#74932=CARTESIAN_POINT('',(24.1012882089558,-32.5967492173916,-19.6986995804965));
#74933=CARTESIAN_POINT('Origin',(24.1,-32.5339653438087,-19.6495190528383));
#74934=CARTESIAN_POINT('',(23.1004586919557,-32.3905528841213,-19.9143644494691));
#74935=CARTESIAN_POINT('Origin',(23.1,-32.3839653438087,-19.9093266739736));
#74936=CARTESIAN_POINT('',(22.399682944576,-32.1795566506761,-20.2523726527878));
#74937=CARTESIAN_POINT('Origin',(22.4,-32.1839653438087,-20.2557368354874));
#74938=CARTESIAN_POINT('',(21.7998387845652,-32.0783403153759,-20.4245471623811));
#74939=CARTESIAN_POINT('Origin',(21.8,-32.0839653438087,-20.4289419162443));
#74940=CARTESIAN_POINT('',(13.2021921742626,-32.0074773662801,-20.3691829588007));
#74941=CARTESIAN_POINT('Origin',(13.2,-32.0839653438087,-20.4289419162443));
#74942=CARTESIAN_POINT('',(12.6002487187375,-32.180506880376,-20.2530977534517));
#74943=CARTESIAN_POINT('Origin',(12.6,-32.1839653438087,-20.2557368354874));
#74944=CARTESIAN_POINT('',(11.8996457869536,-32.3890524021132,-19.9132169663217));
#74945=CARTESIAN_POINT('Origin',(11.9,-32.3839653438087,-19.9093266739736));
#74946=CARTESIAN_POINT('',(10.899790263986,-32.544187318536,-19.6575262381569));
#74947=CARTESIAN_POINT('Origin',(10.9,-32.5339653438087,-19.6495190528383));
#74948=CARTESIAN_POINT('',(4.55736144060343,-32.6604876193617,-20.2466717586953));
#74949=CARTESIAN_POINT('Origin',(4.5,-32.3339653438087,-19.9959292143521));
#74950=CARTESIAN_POINT('',(4.49524972087093,-32.0570688314042,-20.4079280576995));
#74951=CARTESIAN_POINT('Origin',(4.5,-32.0839653438087,-20.4289419162443));
#74952=CARTESIAN_POINT('',(1.90350512467335,-32.0308439720488,-20.387438952028));
#74953=CARTESIAN_POINT('Origin',(1.9,-32.0839653438087,-20.4289419162443));
#74954=CARTESIAN_POINT('Ctrl Pts',(0.138207714141622,-36.5204955072697,
-22.244646263818));
#74955=CARTESIAN_POINT('Ctrl Pts',(0.37021747089714,-36.2375102394032,-22.2632399142705));
#74956=CARTESIAN_POINT('Ctrl Pts',(0.600000000000006,-35.9562839053824,
-22.2808358845789));
#74957=CARTESIAN_POINT('Origin',(1.9,-33.7339653438087,-17.5710580837557));
#74958=CARTESIAN_POINT('',(5.09593997529677,-37.7041716521717,-19.1751255543105));
#74959=CARTESIAN_POINT('',(17.5,-37.7041716521717,-19.1751255543105));
#74960=CARTESIAN_POINT('',(4.47529854852883,-33.5694020278343,-17.5045701882916));
#74961=CARTESIAN_POINT('Origin',(4.5,-33.7339653438087,-17.5710580837557));
#74962=CARTESIAN_POINT('',(5.09944803334084,-37.459394730737,-19.6490138787379));
#74963=CARTESIAN_POINT('Origin',(-0.840551718690874,0.,0.));
#74964=CARTESIAN_POINT('',(4.50447263544529,-33.5136270415661,-18.0163441277467));
#74965=CARTESIAN_POINT('Origin',(4.5,-33.4839653438087,-18.0040707856479));
#74966=CARTESIAN_POINT('',(10.8302042597752,-37.2924258787336,-19.9640920674886));
#74967=CARTESIAN_POINT('Origin',(-62.7155570771054,0.,0.));
#74968=CARTESIAN_POINT('',(10.8987117910442,-33.3579488669236,-18.3802631128033));
#74969=CARTESIAN_POINT('Origin',(10.9,-33.2839653438087,-18.3504809471617));
#74970=CARTESIAN_POINT('',(11.6618634261911,-37.4090062358548,-19.7447778525305));
#74971=CARTESIAN_POINT('Origin',(26.9856656232739,0.,0.));
#74972=CARTESIAN_POINT('',(11.8995413080444,-33.4416219555226,-18.0938594155378));
#74973=CARTESIAN_POINT('Origin',(11.9,-33.4339653438087,-18.0906733260263));
#74974=CARTESIAN_POINT('',(12.3548486633046,-37.5911252244479,-19.3958063601357));
#74975=CARTESIAN_POINT('Origin',(20.8267261185512,0.,0.));
#74976=CARTESIAN_POINT('',(12.600317055424,-33.6288475295616,-17.742127215612));
#74977=CARTESIAN_POINT('Origin',(12.6,-33.6339653438087,-17.7442631645126));
#74978=CARTESIAN_POINT('',(13.103292255208,-37.7041716521717,-19.1751255543105));
#74979=CARTESIAN_POINT('Origin',(25.13830739299,0.,0.));
#74980=CARTESIAN_POINT('',(13.2001612154348,-33.7273468611033,-17.5683840431675));
#74981=CARTESIAN_POINT('Origin',(13.2,-33.7339653438087,-17.5710580837557));
#74982=CARTESIAN_POINT('',(21.896707744792,-37.7041716521717,-19.1751255543105));
#74983=CARTESIAN_POINT('',(17.5,-37.7041716521717,-19.1751255543105));
#74984=CARTESIAN_POINT('',(21.7978078257374,-33.6439685797946,-17.5346970308537));
#74985=CARTESIAN_POINT('Origin',(21.8,-33.7339653438087,-17.5710580837557));
#74986=CARTESIAN_POINT('',(22.6451513366954,-37.5911252244479,-19.3958063601357));
#74987=CARTESIAN_POINT('Origin',(9.86169260701005,0.,0.));
#74988=CARTESIAN_POINT('',(22.3997512812625,-33.6299506000067,-17.7425875883397));
#74989=CARTESIAN_POINT('Origin',(22.4,-33.6339653438087,-17.7442631645126));
#74990=CARTESIAN_POINT('',(23.3381365738089,-37.4090062358548,-19.7447778525305));
#74991=CARTESIAN_POINT('Origin',(14.1732738814488,0.,0.));
#74992=CARTESIAN_POINT('',(23.1003542130464,-33.4398779649625,-18.0931337015746));
#74993=CARTESIAN_POINT('Origin',(23.1,-33.4339653438087,-18.0906733260263));
#74994=CARTESIAN_POINT('',(24.1697957402248,-37.2924258787336,-19.9640920674886));
#74995=CARTESIAN_POINT('Origin',(8.01433437672607,0.,0.));
#74996=CARTESIAN_POINT('',(24.100209736014,-33.2960107570711,-18.3553298442931));
#74997=CARTESIAN_POINT('Origin',(24.1,-33.2839653438087,-18.3504809471617));
#74998=CARTESIAN_POINT('',(29.9005519666592,-37.459394730737,-19.6490138787379));
#74999=CARTESIAN_POINT('Origin',(97.7155570771054,0.,0.));
#75000=CARTESIAN_POINT('',(30.4426385593966,-33.864375894796,-18.1614760990067));
#75001=CARTESIAN_POINT('Origin',(30.5,-33.4839653438087,-18.0040707856479));
#75002=CARTESIAN_POINT('',(29.9040600247032,-37.7041716521717,-19.1751255543105));
#75003=CARTESIAN_POINT('Origin',(35.8405517186909,0.,0.));
#75004=CARTESIAN_POINT('',(30.5047502791291,-33.7023185522751,-17.5582719500126));
#75005=CARTESIAN_POINT('Origin',(30.5,-33.7339653438087,-17.5710580837557));
#75006=CARTESIAN_POINT('',(17.5,-37.7041716521717,-19.1751255543105));
#75007=CARTESIAN_POINT('Origin',(17.5,-37.0225860117848,-21.375));
#75008=CARTESIAN_POINT('Origin',(17.5,0.,0.));
#75009=CARTESIAN_POINT('',(0.600000000000001,-39.2790537077817,-15.6985967468815));
#75010=CARTESIAN_POINT('Origin',(0.600000000000001,0.,0.));
#75011=CARTESIAN_POINT('',(1.67735469196904,-38.9247727484987,-16.5575380560557));
#75012=CARTESIAN_POINT('Origin',(8.14497546096349,0.,0.));
#75013=CARTESIAN_POINT('',(5.09593997529677,-38.9247727484987,-16.5575380560557));
#75014=CARTESIAN_POINT('',(17.5,-38.9247727484987,-16.5575380560557));
#75015=CARTESIAN_POINT('',(5.09944803334083,-39.1304526938498,-16.0654185122698));
#75016=CARTESIAN_POINT('Origin',(-0.840551718690872,0.,0.));
#75017=CARTESIAN_POINT('',(10.8302042597752,-39.2644910802189,-15.7349845952072));
#75018=CARTESIAN_POINT('Origin',(-62.7155570771054,0.,0.));
#75019=CARTESIAN_POINT('',(11.6618634261911,-39.1714230536436,-15.9652627899599));
#75020=CARTESIAN_POINT('Origin',(26.9856656232739,0.,0.));
#75021=CARTESIAN_POINT('',(12.3548486633046,-39.0211592104439,-16.3290885806033));
#75022=CARTESIAN_POINT('Origin',(20.8267261185512,0.,0.));
#75023=CARTESIAN_POINT('',(13.103292255208,-38.9247727484987,-16.5575380560557));
#75024=CARTESIAN_POINT('Origin',(25.13830739299,0.,0.));
#75025=CARTESIAN_POINT('',(21.896707744792,-38.9247727484987,-16.5575380560557));
#75026=CARTESIAN_POINT('',(17.5,-38.9247727484987,-16.5575380560557));
#75027=CARTESIAN_POINT('',(22.6451513366954,-39.0211592104439,-16.3290885806033));
#75028=CARTESIAN_POINT('Origin',(9.86169260701007,0.,0.));
#75029=CARTESIAN_POINT('',(23.3381365738089,-39.1714230536436,-15.9652627899599));
#75030=CARTESIAN_POINT('Origin',(14.1732738814488,0.,0.));
#75031=CARTESIAN_POINT('',(24.1697957402248,-39.2644910802189,-15.7349845952072));
#75032=CARTESIAN_POINT('Origin',(8.01433437672609,0.,0.));
#75033=CARTESIAN_POINT('',(29.9005519666592,-39.1304526938498,-16.0654185122698));
#75034=CARTESIAN_POINT('Origin',(97.7155570771054,0.,0.));
#75035=CARTESIAN_POINT('',(29.9040600247032,-38.9247727484987,-16.5575380560557));
#75036=CARTESIAN_POINT('Origin',(35.8405517186909,0.,0.));
#75037=CARTESIAN_POINT('',(17.5,-38.9247727484987,-16.5575380560557));
#75038=CARTESIAN_POINT('Origin',(33.1,-35.1439863533772,-14.5472582706722));
#75039=CARTESIAN_POINT('',(30.5247014514712,-34.987274410005,-14.4639330523272));
#75040=CARTESIAN_POINT('Origin',(30.5,-35.1439863533772,-14.5472582706722));
#75041=CARTESIAN_POINT('',(30.4955273645547,-35.343464522354,-14.0922449867892));
#75042=CARTESIAN_POINT('Origin',(30.5,-35.31499642504,-14.0774119602792));
#75043=CARTESIAN_POINT('',(24.1012882089558,-35.5221746368434,-13.7390659716653));
#75044=CARTESIAN_POINT('Origin',(24.1,-35.4518044823703,-13.7015349119648));
#75045=CARTESIAN_POINT('',(23.1004586919557,-35.35656070068,-13.9872600241959));
#75046=CARTESIAN_POINT('Origin',(23.1,-35.3491984393726,-13.9834426982006));
#75047=CARTESIAN_POINT('',(22.399682944576,-35.2074644826695,-14.3567722348382));
#75048=CARTESIAN_POINT('Origin',(22.4,-35.2123903820423,-14.359319746515));
#75049=CARTESIAN_POINT('',(21.7998387845652,-35.137683640766,-14.5439070589317));
#75050=CARTESIAN_POINT('Origin',(21.8,-35.1439863533772,-14.5472582706722));
#75051=CARTESIAN_POINT('',(13.2021921742626,-35.0582833660355,-14.501689183981));
#75052=CARTESIAN_POINT('Origin',(13.2,-35.1439863533772,-14.5472582706722));
#75053=CARTESIAN_POINT('',(12.6002487187375,-35.208526188654,-14.3573213139379));
#75054=CARTESIAN_POINT('Origin',(12.6,-35.2123903820423,-14.359319746515));
#75055=CARTESIAN_POINT('',(11.8996457869536,-35.3548837560077,-13.9863905298622));
#75056=CARTESIAN_POINT('Origin',(11.9,-35.3491984393726,-13.9834426982006));
#75057=CARTESIAN_POINT('',(10.899790263986,-35.4632615954717,-13.7076454228629));
#75058=CARTESIAN_POINT('Origin',(10.9,-35.4518044823703,-13.7015349119648));
#75059=CARTESIAN_POINT('',(4.55736144060343,-35.6800990794245,-14.267645163841));
#75060=CARTESIAN_POINT('Origin',(4.5,-35.31499642504,-14.0774119602792));
#75061=CARTESIAN_POINT('',(4.49524972087093,-35.1138494411902,-14.5312341902212));
#75062=CARTESIAN_POINT('Origin',(4.5,-35.1439863533772,-14.5472582706722));
#75063=CARTESIAN_POINT('',(1.90350512467335,-35.0844651005135,-14.5156102591402));
#75064=CARTESIAN_POINT('Origin',(1.9,-35.1439863533772,-14.5472582706722));
#75065=CARTESIAN_POINT('Ctrl Pts',(0.138207714141633,-39.8284094059642,
-15.5649826112914));
#75066=CARTESIAN_POINT('Ctrl Pts',(0.370217470894376,-39.5529520737016,
-15.6324336584845));
#75067=CARTESIAN_POINT('Ctrl Pts',(0.600000000000006,-39.2790537077817,
-15.6985967468815));
#75068=CARTESIAN_POINT('Origin',(1.9,-36.2726528263519,-11.4462726220787));
#75069=CARTESIAN_POINT('',(5.09593997529677,-40.4610861730024,-12.3365516130268));
#75070=CARTESIAN_POINT('',(17.5,-40.4610861730024,-12.3365516130268));
#75071=CARTESIAN_POINT('',(4.47529854852883,-36.0990440950346,-11.409370947074));
#75072=CARTESIAN_POINT('Origin',(4.5,-36.2726528263519,-11.4462726220787));
#75073=CARTESIAN_POINT('',(5.09944803334083,-40.3023178069695,-12.8457455753269));
#75074=CARTESIAN_POINT('Origin',(-0.840551718690874,0.,0.));
#75075=CARTESIAN_POINT('',(4.50447263544529,-36.1329850680974,-11.9230551151638));
#75076=CARTESIAN_POINT('Origin',(4.5,-36.101642754689,-11.9161189324716));
#75077=CARTESIAN_POINT('',(10.8302042597752,-40.1925983403042,-13.1850308552911));
#75078=CARTESIAN_POINT('Origin',(-62.7155570771055,0.,0.));
#75079=CARTESIAN_POINT('',(10.8987117910442,-36.0428658633082,-12.3084785844451));
#75080=CARTESIAN_POINT('Origin',(10.9,-35.9648346973588,-12.291995980786));
#75081=CARTESIAN_POINT('',(11.6618634261911,-40.2693240660821,-12.9488045494888));
#75082=CARTESIAN_POINT('Origin',(26.9856656232739,0.,0.));
#75083=CARTESIAN_POINT('',(11.8995413080444,-36.0755342895717,-12.0118963235316));
#75084=CARTESIAN_POINT('Origin',(11.9,-36.0674407403565,-12.0100881945502));
#75085=CARTESIAN_POINT('',(12.3548486633046,-40.3880779943072,-12.5735100877104));
#75086=CARTESIAN_POINT('Origin',(20.8267261185512,0.,0.));
#75087=CARTESIAN_POINT('',(12.600317055424,-36.1988378309035,-11.6329963463162));
#75088=CARTESIAN_POINT('Origin',(12.6,-36.2042487976867,-11.6342111462358));
#75089=CARTESIAN_POINT('',(13.103292255208,-40.4610861730024,-12.3365516130268));
#75090=CARTESIAN_POINT('Origin',(25.13830739299,0.,0.));
#75091=CARTESIAN_POINT('',(13.2001612154348,-36.2656705509953,-11.4447884936362));
#75092=CARTESIAN_POINT('Origin',(13.2,-36.2726528263519,-11.4462726220787));
#75093=CARTESIAN_POINT('',(21.896707744792,-40.4610861730024,-12.3365516130268));
#75094=CARTESIAN_POINT('',(17.5,-40.4610861730024,-12.3365516130268));
#75095=CARTESIAN_POINT('',(21.7978078257374,-36.1777092848303,-11.4260917493401));
#75096=CARTESIAN_POINT('Origin',(21.8,-36.2726528263519,-11.4462726220787));
#75097=CARTESIAN_POINT('',(22.6451513366954,-40.3880779943072,-12.5735100877104));
#75098=CARTESIAN_POINT('Origin',(9.86169260701005,0.,0.));
#75099=CARTESIAN_POINT('',(22.3997512812625,-36.2000040861152,-11.633258178775));
#75100=CARTESIAN_POINT('Origin',(22.4,-36.2042487976867,-11.6342111462358));
#75101=CARTESIAN_POINT('',(23.3381365738089,-40.2693240660821,-12.9488045494888));
#75102=CARTESIAN_POINT('Origin',(14.1732738814488,0.,0.));
#75103=CARTESIAN_POINT('',(23.1003542130464,-36.0736907752397,-12.0114844755768));
#75104=CARTESIAN_POINT('Origin',(23.1,-36.0674407403565,-12.0100881945502));
#75105=CARTESIAN_POINT('',(24.1697957402248,-40.1925983403042,-13.1850308552911));
#75106=CARTESIAN_POINT('Origin',(8.01433437672608,0.,0.));
#75107=CARTESIAN_POINT('',(24.100209736014,-35.9775391158784,-12.2946795482123));
#75108=CARTESIAN_POINT('Origin',(24.1,-35.9648346973588,-12.291995980786));
#75109=CARTESIAN_POINT('',(29.9005519666592,-40.3023178069695,-12.8457455753269));
#75110=CARTESIAN_POINT('Origin',(97.7155570771054,0.,0.));
#75111=CARTESIAN_POINT('',(30.4426385593966,-36.5036071604488,-12.0050753064884));
#75112=CARTESIAN_POINT('Origin',(30.5,-36.101642754689,-11.9161189324716));
#75113=CARTESIAN_POINT('',(29.9040600247032,-40.4610861730024,-12.3365516130268));
#75114=CARTESIAN_POINT('Origin',(35.8405517186909,0.,0.));
#75115=CARTESIAN_POINT('',(30.5047502791291,-36.2392665318678,-11.4391761461162));
#75116=CARTESIAN_POINT('Origin',(30.5,-36.2726528263519,-11.4462726220787));
#75117=CARTESIAN_POINT('',(17.5,-40.4610861730024,-12.3365516130268));
#75118=CARTESIAN_POINT('Origin',(17.5,-40.1718595385976,-14.6213611271723));
#75119=CARTESIAN_POINT('Origin',(17.5,0.,0.));
#75120=CARTESIAN_POINT('',(0.600000000000001,-41.4083493394303,-8.63936369090331));
#75121=CARTESIAN_POINT('Origin',(0.600000000000001,0.,0.));
#75122=CARTESIAN_POINT('',(1.67735469196904,-41.2086042970448,-9.54677599452212));
#75123=CARTESIAN_POINT('Origin',(8.14497546096349,0.,0.));
#75124=CARTESIAN_POINT('',(5.09593997529677,-41.2086042970448,-9.54677599452212));
#75125=CARTESIAN_POINT('',(17.5,-41.2086042970448,-9.54677599452212));
#75126=CARTESIAN_POINT('',(5.09944803334083,-41.325703839893,-9.02641690470009));
#75127=CARTESIAN_POINT('Origin',(-0.840551718690872,0.,0.));
#75128=CARTESIAN_POINT('',(10.8302042597752,-41.4003266344532,-8.67772749978829));
#75129=CARTESIAN_POINT('Origin',(-62.7155570771055,0.,0.));
#75130=CARTESIAN_POINT('',(11.6618634261911,-41.3486599091995,-8.92066834454425));
#75131=CARTESIAN_POINT('Origin',(26.9856656232739,0.,0.));
#75132=CARTESIAN_POINT('',(12.3548486633046,-41.2638565969525,-9.3050598464565));
#75133=CARTESIAN_POINT('Origin',(20.8267261185512,0.,0.));
#75134=CARTESIAN_POINT('',(13.103292255208,-41.2086042970448,-9.54677599452212));
#75135=CARTESIAN_POINT('Origin',(25.13830739299,0.,0.));
#75136=CARTESIAN_POINT('',(21.896707744792,-41.2086042970448,-9.54677599452212));
#75137=CARTESIAN_POINT('',(17.5,-41.2086042970448,-9.54677599452212));
#75138=CARTESIAN_POINT('',(22.6451513366954,-41.2638565969525,-9.3050598464565));
#75139=CARTESIAN_POINT('Origin',(9.86169260701005,0.,0.));
#75140=CARTESIAN_POINT('',(23.3381365738089,-41.3486599091995,-8.92066834454425));
#75141=CARTESIAN_POINT('Origin',(14.1732738814488,0.,0.));
#75142=CARTESIAN_POINT('',(24.1697957402248,-41.4003266344532,-8.67772749978828));
#75143=CARTESIAN_POINT('Origin',(8.01433437672607,0.,0.));
#75144=CARTESIAN_POINT('',(29.9005519666592,-41.325703839893,-9.02641690470009));
#75145=CARTESIAN_POINT('Origin',(97.7155570771054,0.,0.));
#75146=CARTESIAN_POINT('',(29.9040600247032,-41.2086042970448,-9.54677599452212));
#75147=CARTESIAN_POINT('Origin',(35.8405517186909,0.,0.));
#75148=CARTESIAN_POINT('',(17.5,-41.2086042970448,-9.54677599452212));
#75149=CARTESIAN_POINT('Origin',(33.1,-37.1361751213135,-8.22356354381348));
#75150=CARTESIAN_POINT('',(30.5247014514712,-36.9673747121716,-8.16871696615112));
#75151=CARTESIAN_POINT('Origin',(30.5,-37.1361751213135,-8.22356354381348));
#75152=CARTESIAN_POINT('',(30.4955273645547,-37.253610541118,-7.74082391359483));
#75153=CARTESIAN_POINT('Origin',(30.5,-37.2229992101469,-7.73115966730738));
#75154=CARTESIAN_POINT('',(24.1012882089558,-37.3682767550424,-7.3619777955879));
#75155=CARTESIAN_POINT('Origin',(24.1,-37.2924584812137,-7.3372365661025));
#75156=CARTESIAN_POINT('',(23.1004586919557,-37.2482773116316,-7.63515978098255));
#75157=CARTESIAN_POINT('Origin',(23.1,-37.2403640279136,-7.63267889200616));
#75158=CARTESIAN_POINT('',(22.399682944576,-37.1656113221937,-8.02494855741036));
#75159=CARTESIAN_POINT('Origin',(22.4,-37.1709047568469,-8.02660199321104));
#75160=CARTESIAN_POINT('',(21.7998387845652,-37.1293862292573,-8.22135769906883));
#75161=CARTESIAN_POINT('Origin',(21.8,-37.1361751213135,-8.22356354381348));
#75162=CARTESIAN_POINT('',(13.2021921742626,-37.0438611660612,-8.19356892151486));
#75163=CARTESIAN_POINT('Origin',(13.2,-37.1361751213135,-8.22356354381348));
#75164=CARTESIAN_POINT('',(12.6002487187375,-37.1667522450638,-8.02530493145533));
#75165=CARTESIAN_POINT('Origin',(12.6,-37.1709047568469,-8.02660199321104));
#75166=CARTESIAN_POINT('',(11.8996457869536,-37.2464748574103,-7.63459469460788));
#75167=CARTESIAN_POINT('Origin',(11.9,-37.2403640279136,-7.63267889200616));
#75168=CARTESIAN_POINT('',(10.899790263986,-37.3048026141052,-7.34126473779836));
#75169=CARTESIAN_POINT('Origin',(10.9,-37.2924584812137,-7.3372365661025));
#75170=CARTESIAN_POINT('',(4.55736144060343,-37.6155887839604,-7.85510339046015));
#75171=CARTESIAN_POINT('Origin',(4.5,-37.2229992101469,-7.73115966730738));
#75172=CARTESIAN_POINT('',(4.49524972087093,-37.1037135041708,-8.21301612503226));
#75173=CARTESIAN_POINT('Origin',(4.5,-37.1361751213135,-8.22356354381348));
#75174=CARTESIAN_POINT('',(1.90350512467335,-37.0720625104951,-8.20273209378166));
#75175=CARTESIAN_POINT('Origin',(1.9,-37.1361751213135,-8.22356354381348));
#75176=CARTESIAN_POINT('Ctrl Pts',(0.138207714141624,-41.9261572390061,
-8.41238483838183));
#75177=CARTESIAN_POINT('Ctrl Pts',(0.370217470898825,-41.6665974739917,
-8.52664381638101));
#75178=CARTESIAN_POINT('Ctrl Pts',(0.600000000000005,-41.4083493394303,
-8.63936369090331));
#75179=CARTESIAN_POINT('Origin',(1.9,-37.7092141076143,-4.9736979588732));
#75180=CARTESIAN_POINT('',(5.09593997529677,-41.9886110647639,-5.1231377935775));
#75181=CARTESIAN_POINT('',(17.5,-41.9886110647639,-5.1231377935775));
#75182=CARTESIAN_POINT('',(4.47529854852883,-37.5318349744051,-4.96750374304975));
#75183=CARTESIAN_POINT('Origin',(4.5,-37.7092141076143,-4.9736979588732));
#75184=CARTESIAN_POINT('',(5.09944803334083,-41.9206753505941,-5.65216579287045));
#75185=CARTESIAN_POINT('Origin',(-0.840551718690874,0.,0.));
#75186=CARTESIAN_POINT('',(4.50447263544529,-37.6544606275072,-5.46749010626365));
#75187=CARTESIAN_POINT('Origin',(4.5,-37.6223900187809,-5.4661018353793));
#75188=CARTESIAN_POINT('',(10.8302042597752,-41.8715390397407,-6.00534915250317));
#75189=CARTESIAN_POINT('Origin',(-62.7155570771055,0.,0.));
#75190=CARTESIAN_POINT('',(10.8987117910442,-37.6326386190063,-5.86270716268918));
#75191=CARTESIAN_POINT('Origin',(10.9,-37.5529307477141,-5.86002493658419));
#75192=CARTESIAN_POINT('',(11.6618634261911,-41.9060788618227,-5.75938837262205));
#75193=CARTESIAN_POINT('Origin',(26.9856656232739,0.,0.));
#75194=CARTESIAN_POINT('',(11.8995413080444,-37.6133097693334,-5.5649578400478));
#75195=CARTESIAN_POINT('Origin',(11.9,-37.6050252010142,-5.56458261068052));
#75196=CARTESIAN_POINT('',(12.3548486633046,-41.9578594516632,-5.36917407377309));
#75197=CARTESIAN_POINT('Origin',(20.8267261185512,0.,0.));
#75198=CARTESIAN_POINT('',(12.600317055424,-37.6689447622493,-5.17040276961774));
#75199=CARTESIAN_POINT('Origin',(12.6,-37.674484472081,-5.17065950947564));
#75200=CARTESIAN_POINT('',(13.103292255208,-41.9886110647639,-5.1231377935775));
#75201=CARTESIAN_POINT('Origin',(25.13830739299,0.,0.));
#75202=CARTESIAN_POINT('',(13.2001612154348,-37.7020801925101,-4.97344883706827));
#75203=CARTESIAN_POINT('Origin',(13.2,-37.7092141076143,-4.9736979588732));
#75204=CARTESIAN_POINT('',(21.896707744792,-41.9886110647639,-5.1231377935775));
#75205=CARTESIAN_POINT('',(17.5,-41.9886110647639,-5.1231377935775));
#75206=CARTESIAN_POINT('',(21.7978078257374,-37.6122086000506,-4.97031045190414));
#75207=CARTESIAN_POINT('Origin',(21.8,-37.7092141076143,-4.9736979588732));
#75208=CARTESIAN_POINT('',(22.6451513366954,-41.9578594516632,-5.36917407377309));
#75209=CARTESIAN_POINT('Origin',(9.86169260701005,0.,0.));
#75210=CARTESIAN_POINT('',(22.3997512812625,-37.6701387661531,-5.17045810616097));
#75211=CARTESIAN_POINT('Origin',(22.4,-37.674484472081,-5.17065950947564));
#75212=CARTESIAN_POINT('',(23.3381365738089,-41.9060788618227,-5.75938837262206));
#75213=CARTESIAN_POINT('Origin',(14.1732738814488,0.,0.));
#75214=CARTESIAN_POINT('',(23.1003542130464,-37.6114227454796,-5.5648723718931));
#75215=CARTESIAN_POINT('Origin',(23.1,-37.6050252010142,-5.56458261068052));
#75216=CARTESIAN_POINT('',(24.1697957402248,-41.8715390397407,-6.00534915250317));
#75217=CARTESIAN_POINT('Origin',(8.01433437672608,0.,0.));
#75218=CARTESIAN_POINT('',(24.100209736014,-37.565908154163,-5.86046163546709));
#75219=CARTESIAN_POINT('Origin',(24.1,-37.5529307477141,-5.86002493658419));
#75220=CARTESIAN_POINT('',(29.9005519666592,-41.9206753505941,-5.65216579287045));
#75221=CARTESIAN_POINT('Origin',(97.7155570771054,0.,0.));
#75222=CARTESIAN_POINT('',(30.4426385593966,-38.0336947942479,-5.48390637564376));
#75223=CARTESIAN_POINT('Origin',(30.5,-37.6223900187809,-5.4661018353793));
#75224=CARTESIAN_POINT('',(29.9040600247032,-41.9886110647639,-5.1231377935775));
#75225=CARTESIAN_POINT('Origin',(35.8405517186909,0.,0.));
#75226=CARTESIAN_POINT('',(30.5047502791291,-37.6751027358433,-4.97250676352253));
#75227=CARTESIAN_POINT('Origin',(30.5,-37.7092141076143,-4.9736979588732));
#75228=CARTESIAN_POINT('',(17.5,-41.9886110647639,-5.1231377935775));
#75229=CARTESIAN_POINT('Origin',(17.5,-42.1005314412719,-7.42345959526126));
#75230=CARTESIAN_POINT('Origin',(17.5,0.,0.));
#75231=CARTESIAN_POINT('',(0.600000000000001,-42.2794732300362,-1.31762794090604));
#75232=CARTESIAN_POINT('Origin',(0.600000000000001,0.,0.));
#75233=CARTESIAN_POINT('',(1.67735469196904,-42.240333256585,-2.24593997529677));
#75234=CARTESIAN_POINT('Origin',(8.14497546096349,0.,0.));
#75235=CARTESIAN_POINT('',(5.09593997529677,-42.240333256585,-2.24593997529676));
#75236=CARTESIAN_POINT('',(17.5,-42.240333256585,-2.24593997529677));
#75237=CARTESIAN_POINT('',(5.09944803334083,-42.2652943865761,-1.71315218706844));
#75238=CARTESIAN_POINT('Origin',(-0.840551718690872,0.,0.));
#75239=CARTESIAN_POINT('',(10.8302042597752,-42.2782342134758,-1.35680204543027));
#75240=CARTESIAN_POINT('Origin',(-62.7155570771055,0.,0.));
#75241=CARTESIAN_POINT('',(11.6618634261911,-42.269538656846,-1.60502390555561));
#75242=CARTESIAN_POINT('Origin',(26.9856656232739,0.,0.));
#75243=CARTESIAN_POINT('',(12.3548486633046,-42.2527725812817,-1.99830157746261));
#75244=CARTESIAN_POINT('Origin',(20.8267261185512,0.,0.));
#75245=CARTESIAN_POINT('',(13.103292255208,-42.240333256585,-2.24593997529677));
#75246=CARTESIAN_POINT('Origin',(25.13830739299,0.,0.));
#75247=CARTESIAN_POINT('',(21.896707744792,-42.240333256585,-2.24593997529677));
#75248=CARTESIAN_POINT('',(17.5,-42.240333256585,-2.24593997529677));
#75249=CARTESIAN_POINT('',(22.6451513366954,-42.2527725812817,-1.99830157746261));
#75250=CARTESIAN_POINT('Origin',(9.86169260701005,0.,0.));
#75251=CARTESIAN_POINT('',(23.3381365738089,-42.269538656846,-1.6050239055556));
#75252=CARTESIAN_POINT('Origin',(14.1732738814488,0.,0.));
#75253=CARTESIAN_POINT('',(24.1697957402248,-42.2782342134758,-1.35680204543027));
#75254=CARTESIAN_POINT('Origin',(8.01433437672608,0.,0.));
#75255=CARTESIAN_POINT('',(29.9005519666592,-42.2652943865761,-1.71315218706844));
#75256=CARTESIAN_POINT('Origin',(97.7155570771054,0.,0.));
#75257=CARTESIAN_POINT('',(29.9040600247032,-42.240333256585,-2.24593997529677));
#75258=CARTESIAN_POINT('Origin',(35.8405517186909,0.,0.));
#75259=CARTESIAN_POINT('',(17.5,-42.240333256585,-2.24593997529677));
#75260=CARTESIAN_POINT('Origin',(33.1,-38.,-1.65));
#75261=CARTESIAN_POINT('',(30.5247014514712,-37.8242400401031,-1.62529854852883));
#75262=CARTESIAN_POINT('Origin',(30.5,-38.,-1.65));
#75263=CARTESIAN_POINT('',(30.4955273645547,-38.0318244548267,-1.15420182283181));
#75264=CARTESIAN_POINT('Origin',(30.5,-38.,-1.15));
#75265=CARTESIAN_POINT('',(24.1012882089558,-38.0789626932999,-0.761199649532067));
#75266=CARTESIAN_POINT('Origin',(24.1,-38.,-0.749999999999995));
#75267=CARTESIAN_POINT('',(23.1004586919557,-38.0082238650069,-1.05106907140133));
#75268=CARTESIAN_POINT('Origin',(23.1,-38.,-1.05));
#75269=CARTESIAN_POINT('',(22.399682944576,-37.9944998683999,-1.44929087888548));
#75270=CARTESIAN_POINT('Origin',(22.4,-38.,-1.45));
#75271=CARTESIAN_POINT('',(21.7998387845652,-37.9929312055486,-1.64900654572745));
#75272=CARTESIAN_POINT('Origin',(21.8,-38.,-1.65));
#75273=CARTESIAN_POINT('',(13.2021921742626,-37.9038799896544,-1.63649121351442));
#75274=CARTESIAN_POINT('Origin',(13.2,-38.,-1.65));
#75275=CARTESIAN_POINT('',(12.6002487187375,-37.9956853417913,-1.44944371963071));
#75276=CARTESIAN_POINT('Origin',(12.6,-38.,-1.45));
#75277=CARTESIAN_POINT('',(11.8996457869536,-38.0063506678963,-1.05082556284928));
#75278=CARTESIAN_POINT('Origin',(11.9,-38.,-1.05));
#75279=CARTESIAN_POINT('',(10.899790263986,-38.01285608245,-0.751823438535063));
#75280=CARTESIAN_POINT('Origin',(10.9,-38.,-0.749999999999995));
#75281=CARTESIAN_POINT('',(4.55736144060343,-38.408147857702,-1.2038882754343));
#75282=CARTESIAN_POINT('Origin',(4.5,-38.,-1.15));
#75283=CARTESIAN_POINT('',(4.49524972087093,-37.9662000077121,-1.64524972087092));
#75284=CARTESIAN_POINT('Origin',(4.5,-38.,-1.65));
#75285=CARTESIAN_POINT('',(1.90350512467335,-37.933244060464,-1.64061806453626));
#75286=CARTESIAN_POINT('Origin',(1.9,-38.,-1.65));
#75287=CARTESIAN_POINT('Ctrl Pts',(0.138207714141623,-42.75,-1.00418100903021));
#75288=CARTESIAN_POINT('Ctrl Pts',(0.370217470896624,-42.5142243943577,
-1.16177621660397));
#75289=CARTESIAN_POINT('Ctrl Pts',(0.600000000000005,-42.2794732300361,
-1.31762794090604));
#75290=CARTESIAN_POINT('Origin',(1.9,-38.,1.65));
#75291=CARTESIAN_POINT('',(5.09593997529677,-42.240333256585,2.24593997529678));
#75292=CARTESIAN_POINT('',(17.5,-42.240333256585,2.24593997529678));
#75293=CARTESIAN_POINT('',(4.47529854852883,-37.8242400401031,1.62529854852884));
#75294=CARTESIAN_POINT('Origin',(4.5,-38.,1.65));
#75295=CARTESIAN_POINT('',(5.09944803334083,-42.2652943865761,1.71315218706845));
#75296=CARTESIAN_POINT('Origin',(-0.840551718690874,0.,0.));
#75297=CARTESIAN_POINT('',(4.50447263544529,-38.0318244548267,1.15420182283182));
#75298=CARTESIAN_POINT('Origin',(4.5,-38.,1.15));
#75299=CARTESIAN_POINT('',(10.8302042597752,-42.2782342134758,1.35680204543028));
#75300=CARTESIAN_POINT('Origin',(-62.7155570771055,0.,0.));
#75301=CARTESIAN_POINT('',(10.8987117910442,-38.0789626932999,0.761199649532077));
#75302=CARTESIAN_POINT('Origin',(10.9,-38.,0.750000000000005));
#75303=CARTESIAN_POINT('',(11.6618634261911,-42.269538656846,1.60502390555562));
#75304=CARTESIAN_POINT('Origin',(26.9856656232739,0.,0.));
#75305=CARTESIAN_POINT('',(11.8995413080444,-38.0082238650069,1.05106907140134));
#75306=CARTESIAN_POINT('Origin',(11.9,-38.,1.05));
#75307=CARTESIAN_POINT('',(12.3548486633046,-42.2527725812817,1.99830157746262));
#75308=CARTESIAN_POINT('Origin',(20.8267261185512,0.,0.));
#75309=CARTESIAN_POINT('',(12.600317055424,-37.9944998683999,1.44929087888549));
#75310=CARTESIAN_POINT('Origin',(12.6,-38.,1.45));
#75311=CARTESIAN_POINT('',(13.103292255208,-42.240333256585,2.24593997529678));
#75312=CARTESIAN_POINT('Origin',(25.13830739299,0.,0.));
#75313=CARTESIAN_POINT('',(13.2001612154348,-37.9929312055486,1.64900654572746));
#75314=CARTESIAN_POINT('Origin',(13.2,-38.,1.65));
#75315=CARTESIAN_POINT('',(21.896707744792,-42.240333256585,2.24593997529678));
#75316=CARTESIAN_POINT('',(17.5,-42.240333256585,2.24593997529678));
#75317=CARTESIAN_POINT('',(21.7978078257374,-37.9038799896544,1.63649121351443));
#75318=CARTESIAN_POINT('Origin',(21.8,-38.,1.65));
#75319=CARTESIAN_POINT('',(22.6451513366954,-42.2527725812817,1.99830157746262));
#75320=CARTESIAN_POINT('Origin',(9.86169260701005,0.,0.));
#75321=CARTESIAN_POINT('',(22.3997512812625,-37.9956853417913,1.44944371963072));
#75322=CARTESIAN_POINT('Origin',(22.4,-38.,1.45));
#75323=CARTESIAN_POINT('',(23.3381365738089,-42.269538656846,1.60502390555561));
#75324=CARTESIAN_POINT('Origin',(14.1732738814488,0.,0.));
#75325=CARTESIAN_POINT('',(23.1003542130464,-38.0063506678963,1.05082556284929));
#75326=CARTESIAN_POINT('Origin',(23.1,-38.,1.05));
#75327=CARTESIAN_POINT('',(24.1697957402248,-42.2782342134758,1.35680204543028));
#75328=CARTESIAN_POINT('Origin',(8.01433437672608,0.,0.));
#75329=CARTESIAN_POINT('',(24.100209736014,-38.01285608245,0.751823438535072));
#75330=CARTESIAN_POINT('Origin',(24.1,-38.,0.750000000000005));
#75331=CARTESIAN_POINT('',(29.9005519666592,-42.2652943865761,1.71315218706845));
#75332=CARTESIAN_POINT('Origin',(97.7155570771054,0.,0.));
#75333=CARTESIAN_POINT('',(30.4426385593966,-38.408147857702,1.20388827543431));
#75334=CARTESIAN_POINT('Origin',(30.5,-38.,1.15));
#75335=CARTESIAN_POINT('',(29.9040600247032,-42.240333256585,2.24593997529678));
#75336=CARTESIAN_POINT('Origin',(35.8405517186909,0.,0.));
#75337=CARTESIAN_POINT('',(30.5047502791291,-37.9662000077121,1.64524972087093));
#75338=CARTESIAN_POINT('Origin',(30.5,-38.,1.65));
#75339=CARTESIAN_POINT('',(17.5,-42.240333256585,2.24593997529678));
#75340=CARTESIAN_POINT('Origin',(17.5,-42.75,5.23536506635493E-15));
#75341=CARTESIAN_POINT('Origin',(17.5,0.,0.));
#75342=CARTESIAN_POINT('',(0.600000000000001,-41.8659567209931,6.04414326732378));
#75343=CARTESIAN_POINT('Origin',(0.600000000000001,0.,0.));
#75344=CARTESIAN_POINT('',(1.67735469196905,-41.9886110647639,5.12313779357753));
#75345=CARTESIAN_POINT('Origin',(8.14497546096349,0.,0.));
#75346=CARTESIAN_POINT('',(5.09593997529677,-41.9886110647639,5.12313779357753));
#75347=CARTESIAN_POINT('',(17.5,-41.9886110647639,5.12313779357753));
#75348=CARTESIAN_POINT('',(5.09944803334083,-41.9206753505941,5.65216579287047));
#75349=CARTESIAN_POINT('Origin',(-0.840551718690872,0.,0.));
#75350=CARTESIAN_POINT('',(10.8302042597752,-41.8715390397407,6.0053491525032));
#75351=CARTESIAN_POINT('Origin',(-62.7155570771055,0.,0.));
#75352=CARTESIAN_POINT('',(11.6618634261911,-41.9060788618227,5.75938837262208));
#75353=CARTESIAN_POINT('Origin',(26.9856656232739,0.,0.));
#75354=CARTESIAN_POINT('',(12.3548486633046,-41.9578594516632,5.36917407377311));
#75355=CARTESIAN_POINT('Origin',(20.8267261185512,0.,0.));
#75356=CARTESIAN_POINT('',(13.103292255208,-41.9886110647639,5.12313779357753));
#75357=CARTESIAN_POINT('Origin',(25.13830739299,0.,0.));
#75358=CARTESIAN_POINT('',(21.896707744792,-41.9886110647639,5.12313779357753));
#75359=CARTESIAN_POINT('',(17.5,-41.9886110647639,5.12313779357753));
#75360=CARTESIAN_POINT('',(22.6451513366954,-41.9578594516632,5.36917407377311));
#75361=CARTESIAN_POINT('Origin',(9.86169260701006,0.,0.));
#75362=CARTESIAN_POINT('',(23.3381365738089,-41.9060788618227,5.75938837262209));
#75363=CARTESIAN_POINT('Origin',(14.1732738814488,0.,0.));
#75364=CARTESIAN_POINT('',(24.1697957402248,-41.8715390397407,6.0053491525032));
#75365=CARTESIAN_POINT('Origin',(8.01433437672608,0.,0.));
#75366=CARTESIAN_POINT('',(29.9005519666592,-41.9206753505941,5.65216579287048));
#75367=CARTESIAN_POINT('Origin',(97.7155570771054,0.,0.));
#75368=CARTESIAN_POINT('',(29.9040600247032,-41.9886110647639,5.12313779357753));
#75369=CARTESIAN_POINT('Origin',(35.8405517186909,0.,0.));
#75370=CARTESIAN_POINT('',(17.5,-41.9886110647639,5.12313779357753));
#75371=CARTESIAN_POINT('Origin',(33.1,-37.7092141076143,4.97369795887322));
#75372=CARTESIAN_POINT('',(30.5247014514712,-37.5318349744051,4.96750374304978));
#75373=CARTESIAN_POINT('Origin',(30.5,-37.7092141076143,4.97369795887322));
#75374=CARTESIAN_POINT('',(30.4955273645547,-37.6544606275072,5.46749010626367));
#75375=CARTESIAN_POINT('Origin',(30.5,-37.6223900187809,5.46610183537933));
#75376=CARTESIAN_POINT('',(24.1012882089558,-37.6326386190063,5.8627071626892));
#75377=CARTESIAN_POINT('Origin',(24.1,-37.5529307477141,5.86002493658421));
#75378=CARTESIAN_POINT('',(23.1004586919557,-37.6133097693334,5.56495784004783));
#75379=CARTESIAN_POINT('Origin',(23.1,-37.6050252010142,5.56458261068055));
#75380=CARTESIAN_POINT('',(22.399682944576,-37.6689447622493,5.17040276961777));
#75381=CARTESIAN_POINT('Origin',(22.4,-37.674484472081,5.17065950947566));
#75382=CARTESIAN_POINT('',(21.7998387845652,-37.7020801925101,4.97344883706829));
#75383=CARTESIAN_POINT('Origin',(21.8,-37.7092141076143,4.97369795887322));
#75384=CARTESIAN_POINT('',(13.2021921742626,-37.6122086000506,4.97031045190416));
#75385=CARTESIAN_POINT('Origin',(13.2,-37.7092141076143,4.97369795887322));
#75386=CARTESIAN_POINT('',(12.6002487187375,-37.6701387661531,5.170458106161));
#75387=CARTESIAN_POINT('Origin',(12.6,-37.674484472081,5.17065950947566));
#75388=CARTESIAN_POINT('',(11.8996457869536,-37.6114227454796,5.56487237189313));
#75389=CARTESIAN_POINT('Origin',(11.9,-37.6050252010142,5.56458261068055));
#75390=CARTESIAN_POINT('',(10.899790263986,-37.565908154163,5.86046163546712));
#75391=CARTESIAN_POINT('Origin',(10.9,-37.5529307477141,5.86002493658421));
#75392=CARTESIAN_POINT('',(4.55736144060343,-38.0336947942479,5.48390637564379));
#75393=CARTESIAN_POINT('Origin',(4.5,-37.6223900187809,5.46610183537933));
#75394=CARTESIAN_POINT('',(4.49524972087093,-37.6751027358433,4.97250676352256));
#75395=CARTESIAN_POINT('Origin',(4.5,-37.7092141076143,4.97369795887322));
#75396=CARTESIAN_POINT('',(1.90350512467335,-37.6418431848034,4.9713453144073));
#75397=CARTESIAN_POINT('Origin',(1.9,-37.7092141076143,4.97369795887322));
#75398=CARTESIAN_POINT('Ctrl Pts',(0.138207714141624,-42.2749056435377,
6.43453435214071));
#75399=CARTESIAN_POINT('Ctrl Pts',(0.370217470893479,-42.070078119737,6.23839136562906));
#75400=CARTESIAN_POINT('Ctrl Pts',(0.600000000000005,-41.8659567209931,
6.04414326732377));
#75401=CARTESIAN_POINT('Origin',(1.9,-37.1361751213135,8.22356354381351));
#75402=CARTESIAN_POINT('',(5.09593997529677,-41.2086042970448,9.54677599452214));
#75403=CARTESIAN_POINT('',(17.5,-41.2086042970448,9.54677599452214));
#75404=CARTESIAN_POINT('',(4.47529854852883,-36.9673747121716,8.16871696615114));
#75405=CARTESIAN_POINT('Origin',(4.5,-37.1361751213135,8.22356354381351));
#75406=CARTESIAN_POINT('',(5.09944803334083,-41.325703839893,9.02641690470012));
#75407=CARTESIAN_POINT('Origin',(-0.840551718690874,0.,0.));
#75408=CARTESIAN_POINT('',(4.50447263544529,-37.253610541118,7.74082391359486));
#75409=CARTESIAN_POINT('Origin',(4.5,-37.2229992101469,7.73115966730741));
#75410=CARTESIAN_POINT('',(10.8302042597752,-41.4003266344532,8.67772749978831));
#75411=CARTESIAN_POINT('Origin',(-62.7155570771054,0.,0.));
#75412=CARTESIAN_POINT('',(10.8987117910442,-37.3682767550424,7.36197779558792));
#75413=CARTESIAN_POINT('Origin',(10.9,-37.2924584812137,7.33723656610252));
#75414=CARTESIAN_POINT('',(11.6618634261911,-41.3486599091995,8.92066834454429));
#75415=CARTESIAN_POINT('Origin',(26.9856656232739,0.,0.));
#75416=CARTESIAN_POINT('',(11.8995413080444,-37.2482773116316,7.63515978098258));
#75417=CARTESIAN_POINT('Origin',(11.9,-37.2403640279136,7.63267889200618));
#75418=CARTESIAN_POINT('',(12.3548486633046,-41.2638565969525,9.30505984645653));
#75419=CARTESIAN_POINT('Origin',(20.8267261185512,0.,0.));
#75420=CARTESIAN_POINT('',(12.600317055424,-37.1656113221937,8.02494855741038));
#75421=CARTESIAN_POINT('Origin',(12.6,-37.1709047568469,8.02660199321107));
#75422=CARTESIAN_POINT('',(13.103292255208,-41.2086042970448,9.54677599452214));
#75423=CARTESIAN_POINT('Origin',(25.13830739299,0.,0.));
#75424=CARTESIAN_POINT('',(13.2001612154348,-37.1293862292573,8.22135769906885));
#75425=CARTESIAN_POINT('Origin',(13.2,-37.1361751213135,8.22356354381351));
#75426=CARTESIAN_POINT('',(21.896707744792,-41.2086042970448,9.54677599452214));
#75427=CARTESIAN_POINT('',(17.5,-41.2086042970448,9.54677599452214));
#75428=CARTESIAN_POINT('',(21.7978078257374,-37.0438611660612,8.19356892151488));
#75429=CARTESIAN_POINT('Origin',(21.8,-37.1361751213135,8.22356354381351));
#75430=CARTESIAN_POINT('',(22.6451513366954,-41.2638565969525,9.30505984645653));
#75431=CARTESIAN_POINT('Origin',(9.86169260701005,0.,0.));
#75432=CARTESIAN_POINT('',(22.3997512812625,-37.1667522450638,8.02530493145535));
#75433=CARTESIAN_POINT('Origin',(22.4,-37.1709047568469,8.02660199321107));
#75434=CARTESIAN_POINT('',(23.3381365738089,-41.3486599091995,8.92066834454428));
#75435=CARTESIAN_POINT('Origin',(14.1732738814488,0.,0.));
#75436=CARTESIAN_POINT('',(23.1003542130464,-37.2464748574103,7.63459469460791));
#75437=CARTESIAN_POINT('Origin',(23.1,-37.2403640279136,7.63267889200618));
#75438=CARTESIAN_POINT('',(24.1697957402248,-41.4003266344532,8.67772749978831));
#75439=CARTESIAN_POINT('Origin',(8.01433437672608,0.,0.));
#75440=CARTESIAN_POINT('',(24.100209736014,-37.3048026141052,7.34126473779838));
#75441=CARTESIAN_POINT('Origin',(24.1,-37.2924584812137,7.33723656610252));
#75442=CARTESIAN_POINT('',(29.9005519666592,-41.325703839893,9.02641690470012));
#75443=CARTESIAN_POINT('Origin',(97.7155570771055,0.,0.));
#75444=CARTESIAN_POINT('',(30.4426385593966,-37.6155887839604,7.85510339046018));
#75445=CARTESIAN_POINT('Origin',(30.5,-37.2229992101469,7.73115966730741));
#75446=CARTESIAN_POINT('',(29.9040600247032,-41.2086042970448,9.54677599452215));
#75447=CARTESIAN_POINT('Origin',(35.8405517186909,0.,0.));
#75448=CARTESIAN_POINT('',(30.5047502791291,-37.1037135041708,8.21301612503228));
#75449=CARTESIAN_POINT('Origin',(30.5,-37.1361751213135,8.22356354381351));
#75450=CARTESIAN_POINT('',(17.5,-41.2086042970448,9.54677599452214));
#75451=CARTESIAN_POINT('Origin',(17.5,-42.1005314412719,7.42345959526129));
#75452=CARTESIAN_POINT('Origin',(17.5,0.,0.));
#75453=CARTESIAN_POINT('',(0.600000000000001,-40.1803643021789,13.22226624086));
#75454=CARTESIAN_POINT('Origin',(0.600000000000001,0.,0.));
#75455=CARTESIAN_POINT('',(1.67735469196905,-40.4610861730024,12.3365516130268));
#75456=CARTESIAN_POINT('Origin',(8.14497546096349,0.,0.));
#75457=CARTESIAN_POINT('',(5.09593997529677,-40.4610861730024,12.3365516130268));
#75458=CARTESIAN_POINT('',(17.5,-40.4610861730024,12.3365516130268));
#75459=CARTESIAN_POINT('',(5.09944803334083,-40.3023178069695,12.8457455753269));
#75460=CARTESIAN_POINT('Origin',(-0.840551718690872,0.,0.));
#75461=CARTESIAN_POINT('',(10.8302042597752,-40.1925983403042,13.1850308552911));
#75462=CARTESIAN_POINT('Origin',(-62.7155570771054,0.,0.));
#75463=CARTESIAN_POINT('',(11.6618634261911,-40.2693240660821,12.9488045494888));
#75464=CARTESIAN_POINT('Origin',(26.9856656232739,0.,0.));
#75465=CARTESIAN_POINT('',(12.3548486633046,-40.3880779943072,12.5735100877104));
#75466=CARTESIAN_POINT('Origin',(20.8267261185512,0.,0.));
#75467=CARTESIAN_POINT('',(13.103292255208,-40.4610861730024,12.3365516130268));
#75468=CARTESIAN_POINT('Origin',(25.13830739299,0.,0.));
#75469=CARTESIAN_POINT('',(21.896707744792,-40.4610861730024,12.3365516130268));
#75470=CARTESIAN_POINT('',(17.5,-40.4610861730024,12.3365516130268));
#75471=CARTESIAN_POINT('',(22.6451513366954,-40.3880779943072,12.5735100877104));
#75472=CARTESIAN_POINT('Origin',(9.86169260701006,0.,0.));
#75473=CARTESIAN_POINT('',(23.3381365738089,-40.2693240660821,12.9488045494888));
#75474=CARTESIAN_POINT('Origin',(14.1732738814488,0.,0.));
#75475=CARTESIAN_POINT('',(24.1697957402248,-40.1925983403042,13.1850308552911));
#75476=CARTESIAN_POINT('Origin',(8.01433437672608,0.,0.));
#75477=CARTESIAN_POINT('',(29.9005519666592,-40.3023178069695,12.8457455753269));
#75478=CARTESIAN_POINT('Origin',(97.7155570771054,0.,0.));
#75479=CARTESIAN_POINT('',(29.9040600247032,-40.4610861730024,12.3365516130268));
#75480=CARTESIAN_POINT('Origin',(35.8405517186909,0.,0.));
#75481=CARTESIAN_POINT('',(17.5,-40.4610861730024,12.3365516130268));
#75482=CARTESIAN_POINT('Origin',(33.1,-36.2726528263519,11.4462726220787));
#75483=CARTESIAN_POINT('',(30.5247014514712,-36.0990440950346,11.409370947074));
#75484=CARTESIAN_POINT('Origin',(30.5,-36.2726528263519,11.4462726220787));
#75485=CARTESIAN_POINT('',(30.4955273645547,-36.1329850680974,11.9230551151638));
#75486=CARTESIAN_POINT('Origin',(30.5,-36.101642754689,11.9161189324716));
#75487=CARTESIAN_POINT('',(24.1012882089558,-36.0428658633082,12.3084785844451));
#75488=CARTESIAN_POINT('Origin',(24.1,-35.9648346973588,12.291995980786));
#75489=CARTESIAN_POINT('',(23.1004586919557,-36.0755342895717,12.0118963235317));
#75490=CARTESIAN_POINT('Origin',(23.1,-36.0674407403565,12.0100881945502));
#75491=CARTESIAN_POINT('',(22.399682944576,-36.1988378309035,11.6329963463162));
#75492=CARTESIAN_POINT('Origin',(22.4,-36.2042487976867,11.6342111462359));
#75493=CARTESIAN_POINT('',(21.7998387845652,-36.2656705509953,11.4447884936363));
#75494=CARTESIAN_POINT('Origin',(21.8,-36.2726528263519,11.4462726220787));
#75495=CARTESIAN_POINT('',(13.2021921742626,-36.1777092848303,11.4260917493401));
#75496=CARTESIAN_POINT('Origin',(13.2,-36.2726528263519,11.4462726220787));
#75497=CARTESIAN_POINT('',(12.6002487187375,-36.2000040861152,11.633258178775));
#75498=CARTESIAN_POINT('Origin',(12.6,-36.2042487976867,11.6342111462359));
#75499=CARTESIAN_POINT('',(11.8996457869536,-36.0736907752397,12.0114844755768));
#75500=CARTESIAN_POINT('Origin',(11.9,-36.0674407403565,12.0100881945502));
#75501=CARTESIAN_POINT('',(10.899790263986,-35.9775391158784,12.2946795482123));
#75502=CARTESIAN_POINT('Origin',(10.9,-35.9648346973588,12.291995980786));
#75503=CARTESIAN_POINT('',(4.55736144060343,-36.5036071604488,12.0050753064884));
#75504=CARTESIAN_POINT('Origin',(4.5,-36.101642754689,11.9161189324716));
#75505=CARTESIAN_POINT('',(4.49524972087093,-36.2392665318678,11.4391761461162));
#75506=CARTESIAN_POINT('Origin',(4.5,-36.2726528263519,11.4462726220787));
#75507=CARTESIAN_POINT('',(1.90350512467335,-36.2067139516643,11.4322568815947));
#75508=CARTESIAN_POINT('Origin',(1.9,-36.2726528263519,11.4462726220787));
#75509=CARTESIAN_POINT('Ctrl Pts',(0.138207714141621,-40.515309671231,13.6777396430533));
#75510=CARTESIAN_POINT('Ctrl Pts',(0.370217470899141,-40.3476538099276,
13.4490085829881));
#75511=CARTESIAN_POINT('Ctrl Pts',(0.600000000000005,-40.1803643021789,
13.22226624086));
#75512=CARTESIAN_POINT('Origin',(1.9,-35.1439863533772,14.5472582706722));
#75513=CARTESIAN_POINT('',(5.09593997529677,-38.9247727484987,16.5575380560557));
#75514=CARTESIAN_POINT('',(17.5,-38.9247727484987,16.5575380560557));
#75515=CARTESIAN_POINT('',(4.47529854852883,-34.987274410005,14.4639330523272));
#75516=CARTESIAN_POINT('Origin',(4.5,-35.1439863533772,14.5472582706722));
#75517=CARTESIAN_POINT('',(5.09944803334083,-39.1304526938498,16.0654185122698));
#75518=CARTESIAN_POINT('Origin',(-0.840551718690874,0.,0.));
#75519=CARTESIAN_POINT('',(4.50447263544529,-35.343464522354,14.0922449867892));
#75520=CARTESIAN_POINT('Origin',(4.5,-35.31499642504,14.0774119602792));
#75521=CARTESIAN_POINT('',(10.8302042597752,-39.2644910802189,15.7349845952072));
#75522=CARTESIAN_POINT('Origin',(-62.7155570771055,0.,0.));
#75523=CARTESIAN_POINT('',(10.8987117910442,-35.5221746368434,13.7390659716653));
#75524=CARTESIAN_POINT('Origin',(10.9,-35.4518044823703,13.7015349119648));
#75525=CARTESIAN_POINT('',(11.6618634261911,-39.1714230536436,15.9652627899599));
#75526=CARTESIAN_POINT('Origin',(26.9856656232739,0.,0.));
#75527=CARTESIAN_POINT('',(11.8995413080444,-35.35656070068,13.9872600241959));
#75528=CARTESIAN_POINT('Origin',(11.9,-35.3491984393726,13.9834426982006));
#75529=CARTESIAN_POINT('',(12.3548486633046,-39.0211592104439,16.3290885806033));
#75530=CARTESIAN_POINT('Origin',(20.8267261185512,0.,0.));
#75531=CARTESIAN_POINT('',(12.600317055424,-35.2074644826695,14.3567722348383));
#75532=CARTESIAN_POINT('Origin',(12.6,-35.2123903820423,14.359319746515));
#75533=CARTESIAN_POINT('',(13.103292255208,-38.9247727484987,16.5575380560557));
#75534=CARTESIAN_POINT('Origin',(25.13830739299,0.,0.));
#75535=CARTESIAN_POINT('',(13.2001612154348,-35.137683640766,14.5439070589318));
#75536=CARTESIAN_POINT('Origin',(13.2,-35.1439863533772,14.5472582706722));
#75537=CARTESIAN_POINT('',(21.896707744792,-38.9247727484987,16.5575380560557));
#75538=CARTESIAN_POINT('',(17.5,-38.9247727484987,16.5575380560557));
#75539=CARTESIAN_POINT('',(21.7978078257374,-35.0582833660355,14.501689183981));
#75540=CARTESIAN_POINT('Origin',(21.8,-35.1439863533772,14.5472582706722));
#75541=CARTESIAN_POINT('',(22.6451513366954,-39.0211592104439,16.3290885806033));
#75542=CARTESIAN_POINT('Origin',(9.86169260701005,0.,0.));
#75543=CARTESIAN_POINT('',(22.3997512812625,-35.208526188654,14.3573213139379));
#75544=CARTESIAN_POINT('Origin',(22.4,-35.2123903820423,14.359319746515));
#75545=CARTESIAN_POINT('',(23.3381365738089,-39.1714230536436,15.9652627899599));
#75546=CARTESIAN_POINT('Origin',(14.1732738814488,0.,0.));
#75547=CARTESIAN_POINT('',(23.1003542130464,-35.3548837560077,13.9863905298622));
#75548=CARTESIAN_POINT('Origin',(23.1,-35.3491984393726,13.9834426982006));
#75549=CARTESIAN_POINT('',(24.1697957402248,-39.2644910802189,15.7349845952072));
#75550=CARTESIAN_POINT('Origin',(8.01433437672607,0.,0.));
#75551=CARTESIAN_POINT('',(24.100209736014,-35.4632615954717,13.7076454228629));
#75552=CARTESIAN_POINT('Origin',(24.1,-35.4518044823703,13.7015349119648));
#75553=CARTESIAN_POINT('',(29.9005519666592,-39.1304526938498,16.0654185122698));
#75554=CARTESIAN_POINT('Origin',(97.7155570771054,0.,0.));
#75555=CARTESIAN_POINT('',(30.4426385593966,-35.6800990794245,14.267645163841));
#75556=CARTESIAN_POINT('Origin',(30.5,-35.31499642504,14.0774119602792));
#75557=CARTESIAN_POINT('',(29.9040600247032,-38.9247727484987,16.5575380560557));
#75558=CARTESIAN_POINT('Origin',(35.8405517186909,0.,0.));
#75559=CARTESIAN_POINT('',(30.5047502791291,-35.1138494411902,14.5312341902212));
#75560=CARTESIAN_POINT('Origin',(30.5,-35.1439863533772,14.5472582706722));
#75561=CARTESIAN_POINT('',(17.5,-38.9247727484987,16.5575380560557));
#75562=CARTESIAN_POINT('Origin',(17.5,-40.1718595385976,14.6213611271723));
#75563=CARTESIAN_POINT('Origin',(17.5,0.,0.));
#75564=CARTESIAN_POINT('',(0.600000000000001,-37.2739118462884,19.9986373454573));
#75565=CARTESIAN_POINT('Origin',(0.600000000000001,0.,0.));
#75566=CARTESIAN_POINT('',(1.67735469196905,-37.7041716521717,19.1751255543105));
#75567=CARTESIAN_POINT('Origin',(8.14497546096349,0.,0.));
#75568=CARTESIAN_POINT('',(5.09593997529677,-37.7041716521717,19.1751255543105));
#75569=CARTESIAN_POINT('',(17.5,-37.7041716521717,19.1751255543105));
#75570=CARTESIAN_POINT('',(5.09944803334083,-37.459394730737,19.6490138787379));
#75571=CARTESIAN_POINT('Origin',(-0.840551718690874,0.,0.));
#75572=CARTESIAN_POINT('',(10.8302042597752,-37.2924258787336,19.9640920674886));
#75573=CARTESIAN_POINT('Origin',(-62.7155570771055,0.,0.));
#75574=CARTESIAN_POINT('',(11.6618634261911,-37.4090062358548,19.7447778525305));
#75575=CARTESIAN_POINT('Origin',(26.9856656232739,0.,0.));
#75576=CARTESIAN_POINT('',(12.3548486633046,-37.5911252244478,19.3958063601357));
#75577=CARTESIAN_POINT('Origin',(20.8267261185512,0.,0.));
#75578=CARTESIAN_POINT('',(13.103292255208,-37.7041716521717,19.1751255543105));
#75579=CARTESIAN_POINT('Origin',(25.13830739299,0.,0.));
#75580=CARTESIAN_POINT('',(21.896707744792,-37.7041716521717,19.1751255543105));
#75581=CARTESIAN_POINT('',(17.5,-37.7041716521717,19.1751255543105));
#75582=CARTESIAN_POINT('',(22.6451513366954,-37.5911252244478,19.3958063601357));
#75583=CARTESIAN_POINT('Origin',(9.86169260701006,0.,0.));
#75584=CARTESIAN_POINT('',(23.3381365738089,-37.4090062358548,19.7447778525305));
#75585=CARTESIAN_POINT('Origin',(14.1732738814488,0.,0.));
#75586=CARTESIAN_POINT('',(24.1697957402248,-37.2924258787336,19.9640920674886));
#75587=CARTESIAN_POINT('Origin',(8.01433437672608,0.,0.));
#75588=CARTESIAN_POINT('',(29.9005519666592,-37.459394730737,19.6490138787379));
#75589=CARTESIAN_POINT('Origin',(97.7155570771054,0.,0.));
#75590=CARTESIAN_POINT('',(29.9040600247032,-37.7041716521717,19.1751255543105));
#75591=CARTESIAN_POINT('Origin',(35.8405517186909,0.,0.));
#75592=CARTESIAN_POINT('',(17.5,-37.7041716521717,19.1751255543105));
#75593=CARTESIAN_POINT('Origin',(33.1,-33.7339653438087,17.5710580837557));
#75594=CARTESIAN_POINT('',(30.5247014514712,-33.5694020278343,17.5045701882916));
#75595=CARTESIAN_POINT('Origin',(30.5,-33.7339653438087,17.5710580837557));
#75596=CARTESIAN_POINT('',(30.4955273645547,-33.5136270415661,18.0163441277467));
#75597=CARTESIAN_POINT('Origin',(30.5,-33.4839653438087,18.0040707856479));
#75598=CARTESIAN_POINT('',(24.1012882089558,-33.3579488669236,18.3802631128033));
#75599=CARTESIAN_POINT('Origin',(24.1,-33.2839653438087,18.3504809471617));
#75600=CARTESIAN_POINT('',(23.1004586919557,-33.4416219555226,18.0938594155378));
#75601=CARTESIAN_POINT('Origin',(23.1,-33.4339653438087,18.0906733260263));
#75602=CARTESIAN_POINT('',(22.399682944576,-33.6288475295615,17.742127215612));
#75603=CARTESIAN_POINT('Origin',(22.4,-33.6339653438087,17.7442631645126));
#75604=CARTESIAN_POINT('',(21.7998387845652,-33.7273468611033,17.5683840431675));
#75605=CARTESIAN_POINT('Origin',(21.8,-33.7339653438087,17.5710580837557));
#75606=CARTESIAN_POINT('',(13.2021921742626,-33.6439685797946,17.5346970308537));
#75607=CARTESIAN_POINT('Origin',(13.2,-33.7339653438087,17.5710580837557));
#75608=CARTESIAN_POINT('',(12.6002487187375,-33.6299506000067,17.7425875883397));
#75609=CARTESIAN_POINT('Origin',(12.6,-33.6339653438087,17.7442631645126));
#75610=CARTESIAN_POINT('',(11.8996457869536,-33.4398779649625,18.0931337015746));
#75611=CARTESIAN_POINT('Origin',(11.9,-33.4339653438087,18.0906733260263));
#75612=CARTESIAN_POINT('',(10.899790263986,-33.2960107570711,18.3553298442931));
#75613=CARTESIAN_POINT('Origin',(10.9,-33.2839653438087,18.3504809471617));
#75614=CARTESIAN_POINT('',(4.55736144060343,-33.864375894796,18.1614760990067));
#75615=CARTESIAN_POINT('Origin',(4.5,-33.4839653438087,18.0040707856479));
#75616=CARTESIAN_POINT('',(4.49524972087093,-33.7023185522751,17.5582719500126));
#75617=CARTESIAN_POINT('Origin',(4.5,-33.7339653438087,17.5710580837557));
#75618=CARTESIAN_POINT('',(1.90350512467335,-33.6714620365851,17.5458051084359));
#75619=CARTESIAN_POINT('Origin',(1.9,-33.7339653438087,17.5710580837557));
#75620=CARTESIAN_POINT('Ctrl Pts',(0.138207714141623,-37.5246765162999,
20.5053537361819));
#75621=CARTESIAN_POINT('Ctrl Pts',(0.370217470897676,-37.3992864560072,
20.2509844800861));
#75622=CARTESIAN_POINT('Ctrl Pts',(0.600000000000005,-37.2739118462884,
19.9986373454573));
#75623=CARTESIAN_POINT('Origin',(1.9,-32.0839653438087,20.4289419162443));
#75624=CARTESIAN_POINT('',(5.09593997529677,-35.4582316768749,23.0652077022745));
#75625=CARTESIAN_POINT('',(17.5,-35.4582316768749,23.0652077022745));
#75626=CARTESIAN_POINT('',(4.47529854852883,-31.9441034793054,20.3196698518115));
#75627=CARTESIAN_POINT('Origin',(4.5,-32.0839653438087,20.4289419162443));
#75628=CARTESIAN_POINT('',(5.09944803334083,-35.7462425436685,22.6162805078382));
#75629=CARTESIAN_POINT('Origin',(-0.840551718690874,0.,0.));
#75630=CARTESIAN_POINT('',(4.50447263544529,-32.3594252187343,20.01548032708));
#75631=CARTESIAN_POINT('Origin',(4.5,-32.3339653438087,19.9959292143521));
#75632=CARTESIAN_POINT('',(10.8302042597752,-35.9356238333033,22.3141421459872));
#75633=CARTESIAN_POINT('Origin',(-62.7155570771055,0.,0.));
#75634=CARTESIAN_POINT('',(10.8987117910442,-32.5967492173916,19.6986995804965));
#75635=CARTESIAN_POINT('Origin',(10.9,-32.5339653438087,19.6495190528383));
#75636=CARTESIAN_POINT('',(11.6618634261911,-35.8039823302991,22.5247608043155));
#75637=CARTESIAN_POINT('Origin',(26.9856656232739,0.,0.));
#75638=CARTESIAN_POINT('',(11.8995413080444,-32.3905528841213,19.9143644494691));
#75639=CARTESIAN_POINT('Origin',(11.9,-32.3839653438087,19.9093266739737));
#75640=CARTESIAN_POINT('',(12.3548486633046,-35.5928236469852,22.856966221146));
#75641=CARTESIAN_POINT('Origin',(20.8267261185512,0.,0.));
#75642=CARTESIAN_POINT('',(12.600317055424,-32.1795566506761,20.2523726527878));
#75643=CARTESIAN_POINT('Origin',(12.6,-32.1839653438087,20.2557368354874));
#75644=CARTESIAN_POINT('',(13.103292255208,-35.4582316768749,23.0652077022745));
#75645=CARTESIAN_POINT('Origin',(25.13830739299,0.,0.));
#75646=CARTESIAN_POINT('',(13.2001612154348,-32.0783403153759,20.4245471623811));
#75647=CARTESIAN_POINT('Origin',(13.2,-32.0839653438087,20.4289419162443));
#75648=CARTESIAN_POINT('',(21.896707744792,-35.4582316768749,23.0652077022745));
#75649=CARTESIAN_POINT('',(17.5,-35.4582316768749,23.0652077022745));
#75650=CARTESIAN_POINT('',(21.7978078257374,-32.0074773662801,20.3691829588007));
#75651=CARTESIAN_POINT('Origin',(21.8,-32.0839653438087,20.4289419162443));
#75652=CARTESIAN_POINT('',(22.6451513366954,-35.5928236469852,22.856966221146));
#75653=CARTESIAN_POINT('Origin',(9.86169260701004,0.,0.));
#75654=CARTESIAN_POINT('',(22.3997512812625,-32.180506880376,20.2530977534517));
#75655=CARTESIAN_POINT('Origin',(22.4,-32.1839653438087,20.2557368354874));
#75656=CARTESIAN_POINT('',(23.3381365738089,-35.8039823302992,22.5247608043155));
#75657=CARTESIAN_POINT('Origin',(14.1732738814488,0.,0.));
#75658=CARTESIAN_POINT('',(23.1003542130464,-32.3890524021132,19.9132169663217));
#75659=CARTESIAN_POINT('Origin',(23.1,-32.3839653438087,19.9093266739737));
#75660=CARTESIAN_POINT('',(24.1697957402248,-35.9356238333033,22.3141421459872));
#75661=CARTESIAN_POINT('Origin',(8.01433437672607,0.,0.));
#75662=CARTESIAN_POINT('',(24.100209736014,-32.544187318536,19.6575262381569));
#75663=CARTESIAN_POINT('Origin',(24.1,-32.5339653438087,19.6495190528383));
#75664=CARTESIAN_POINT('',(29.9005519666592,-35.7462425436685,22.6162805078382));
#75665=CARTESIAN_POINT('Origin',(97.7155570771054,0.,0.));
#75666=CARTESIAN_POINT('',(30.4426385593966,-32.6604876193617,20.2466717586953));
#75667=CARTESIAN_POINT('Origin',(30.5,-32.3339653438087,19.9959292143521));
#75668=CARTESIAN_POINT('',(29.9040600247032,-35.4582316768749,23.0652077022745));
#75669=CARTESIAN_POINT('Origin',(35.8405517186909,0.,0.));
#75670=CARTESIAN_POINT('',(30.5047502791291,-32.0570688314042,20.4079280576996));
#75671=CARTESIAN_POINT('Origin',(30.5,-32.0839653438087,20.4289419162443));
#75672=CARTESIAN_POINT('',(17.5,-35.4582316768749,23.0652077022745));
#75673=CARTESIAN_POINT('Origin',(17.5,-37.0225860117848,21.375));
#75674=CARTESIAN_POINT('Origin',(17.5,0.,0.));
#75675=CARTESIAN_POINT('',(0.600000000000001,-33.234910440458,26.1673599741116));
#75676=CARTESIAN_POINT('Origin',(0.600000000000001,0.,0.));
#75677=CARTESIAN_POINT('',(1.67735469196904,-33.8016349549212,25.4310730087083));
#75678=CARTESIAN_POINT('Origin',(8.14497546096349,0.,0.));
#75679=CARTESIAN_POINT('',(5.09593997529677,-33.8016349549212,25.4310730087083));
#75680=CARTESIAN_POINT('',(17.5,-33.8016349549212,25.4310730087083));
#75681=CARTESIAN_POINT('',(5.09944803334083,-33.4782869009794,25.8552568383243));
#75682=CARTESIAN_POINT('Origin',(-0.840551718690872,0.,0.));
#75683=CARTESIAN_POINT('',(10.8302042597752,-33.2591419277157,26.1365544445335));
#75684=CARTESIAN_POINT('Origin',(-62.7155570771055,0.,0.));
#75685=CARTESIAN_POINT('',(11.6618634261911,-33.4120346810215,25.9408160718628));
#75686=CARTESIAN_POINT('Origin',(26.9856656232739,0.,0.));
#75687=CARTESIAN_POINT('',(12.3548486633046,-33.6519851366708,25.6287708710599));
#75688=CARTESIAN_POINT('Origin',(20.8267261185512,0.,0.));
#75689=CARTESIAN_POINT('',(13.103292255208,-33.8016349549212,25.4310730087083));
#75690=CARTESIAN_POINT('Origin',(25.13830739299,0.,0.));
#75691=CARTESIAN_POINT('',(21.896707744792,-33.8016349549212,25.4310730087083));
#75692=CARTESIAN_POINT('',(17.5,-33.8016349549212,25.4310730087083));
#75693=CARTESIAN_POINT('',(22.6451513366954,-33.6519851366708,25.6287708710599));
#75694=CARTESIAN_POINT('Origin',(9.86169260701005,0.,0.));
#75695=CARTESIAN_POINT('',(23.3381365738089,-33.4120346810215,25.9408160718628));
#75696=CARTESIAN_POINT('Origin',(14.1732738814488,0.,0.));
#75697=CARTESIAN_POINT('',(24.1697957402248,-33.2591419277157,26.1365544445335));
#75698=CARTESIAN_POINT('Origin',(8.01433437672609,0.,0.));
#75699=CARTESIAN_POINT('',(29.9005519666592,-33.4782869009794,25.8552568383243));
#75700=CARTESIAN_POINT('Origin',(97.7155570771054,0.,0.));
#75701=CARTESIAN_POINT('',(29.9040600247032,-33.8016349549212,25.4310730087083));
#75702=CARTESIAN_POINT('Origin',(35.8405517186909,0.,0.));
#75703=CARTESIAN_POINT('',(17.5,-33.8016349549212,25.4310730087083));
#75704=CARTESIAN_POINT('Origin',(33.1,-30.1702883945039,23.1619558369422));
#75705=CARTESIAN_POINT('',(30.5247014514712,-30.0197706669552,23.0679019220779));
#75706=CARTESIAN_POINT('Origin',(30.5,-30.1702883945039,23.1619558369422));
#75707=CARTESIAN_POINT('',(30.4955273645547,-29.8759744160904,23.562215640718));
#75708=CARTESIAN_POINT('Origin',(30.5,-29.8488945896607,23.5449780585017));
#75709=CARTESIAN_POINT('',(24.1012882089558,-29.6594674741542,23.893572647341));
#75710=CARTESIAN_POINT('Origin',(24.1,-29.5917795457861,23.8513958357493));
#75711=CARTESIAN_POINT('',(23.1004586919557,-29.7916028606322,23.6260497451375));
#75712=CARTESIAN_POINT('Origin',(23.1,-29.784615828692,23.6215825028136));
#75713=CARTESIAN_POINT('',(22.399682944576,-30.0370617130518,23.312172527411));
#75714=CARTESIAN_POINT('Origin',(22.4,-30.0417308725666,23.315164725566));
#75715=CARTESIAN_POINT('',(21.7998387845652,-30.1642348036977,23.1581731335784));
#75716=CARTESIAN_POINT('Origin',(21.8,-30.1702883945039,23.1619558369422));
#75717=CARTESIAN_POINT('',(13.2021921742626,-30.0879729141313,23.1105194160696));
#75718=CARTESIAN_POINT('Origin',(13.2,-30.1702883945039,23.1619558369422));
#75719=CARTESIAN_POINT('',(12.6002487187375,-30.038068082493,23.3128174522151));
#75720=CARTESIAN_POINT('Origin',(12.6,-30.0417308725666,23.315164725566));
#75721=CARTESIAN_POINT('',(11.8996457869536,-29.7900113841146,23.6250322156174));
#75722=CARTESIAN_POINT('Origin',(11.9,-29.784615828692,23.6215825028136));
#75723=CARTESIAN_POINT('',(10.899790263986,-29.6027999600046,23.8582627313001));
#75724=CARTESIAN_POINT('Origin',(10.9,-29.5917795457861,23.8513958357493));
#75725=CARTESIAN_POINT('',(4.55736144060343,-30.1961927037808,23.7660496304069));
#75726=CARTESIAN_POINT('Origin',(4.5,-29.8488945896607,23.5449780585017));
#75727=CARTESIAN_POINT('',(4.49524972087093,-30.1413426776676,23.1438685456221));
#75728=CARTESIAN_POINT('Origin',(4.5,-30.1702883945039,23.1619558369422));
#75729=CARTESIAN_POINT('',(1.90350512467335,-30.1131197861062,23.1262329256631));
#75730=CARTESIAN_POINT('Origin',(1.9,-30.1702883945039,23.1619558369422));
#75731=CARTESIAN_POINT('Ctrl Pts',(0.138207714141626,-33.3938750538235,
26.7099230322464));
#75732=CARTESIAN_POINT('Ctrl Pts',(0.370217470898796,-33.3145607080718,
26.4376444612465));
#75733=CARTESIAN_POINT('Ctrl Pts',(0.600000000000004,-33.234910440458,26.1673599741116));
#75734=CARTESIAN_POINT('Origin',(1.9,-28.0490892825384,25.6899024992348));
#75735=CARTESIAN_POINT('',(5.09593997529677,-30.9143101784803,28.872052684018));
#75736=CARTESIAN_POINT('',(17.5,-30.9143101784803,28.872052684018));
#75737=CARTESIAN_POINT('',(4.47529854852883,-27.9303271288835,25.5580037650976));
#75738=CARTESIAN_POINT('Origin',(4.5,-28.0490892825384,25.6899024992348));
#75739=CARTESIAN_POINT('',(5.09944803334083,-31.2759009022694,28.4799582645661));
#75740=CARTESIAN_POINT('Origin',(-0.840551718690874,0.,0.));
#75741=CARTESIAN_POINT('',(4.50447263544529,-28.3921611545025,25.3305554259542));
#75742=CARTESIAN_POINT('Origin',(4.5,-28.3704830873816,25.3068802776753));
#75743=CARTESIAN_POINT('',(10.8302042597752,-31.5148708405159,28.2152957791621));
#75744=CARTESIAN_POINT('Origin',(-62.7155570771054,0.,0.));
#75745=CARTESIAN_POINT('',(10.8987117910442,-28.6808880677203,25.0597981705973));
#75746=CARTESIAN_POINT('Origin',(10.9,-28.6275981312563,25.0004625004277));
#75747=CARTESIAN_POINT('',(11.6618634261911,-31.3486557215378,28.3998553597108));
#75748=CARTESIAN_POINT('Origin',(26.9856656232739,0.,0.));
#75749=CARTESIAN_POINT('',(11.8995413080444,-28.4403745085892,25.2363809880999));
#75750=CARTESIAN_POINT('Origin',(11.9,-28.4347618483503,25.2302758333634));
#75751=CARTESIAN_POINT('',(12.3548486633046,-31.0830181478507,28.6903465092421));
#75752=CARTESIAN_POINT('Origin',(20.8267261185512,0.,0.));
#75753=CARTESIAN_POINT('',(12.600317055424,-28.1738892734932,25.5326149758775));
#75754=CARTESIAN_POINT('Origin',(12.6,-28.1776468044757,25.536693610611));
#75755=CARTESIAN_POINT('',(13.103292255208,-30.9143101784803,28.872052684018));
#75756=CARTESIAN_POINT('Origin',(25.13830739299,0.,0.));
#75757=CARTESIAN_POINT('',(13.2001612154348,-28.0443128519265,25.684597735621));
#75758=CARTESIAN_POINT('Origin',(13.2,-28.0490892825384,25.6899024992348));
#75759=CARTESIAN_POINT('',(21.896707744792,-30.9143101784803,28.872052684018));
#75760=CARTESIAN_POINT('',(17.5,-30.9143101784803,28.872052684018));
#75761=CARTESIAN_POINT('',(21.7978078257374,-27.9841403633154,25.6177694167211));
#75762=CARTESIAN_POINT('Origin',(21.8,-28.0490892825384,25.6899024992348));
#75763=CARTESIAN_POINT('',(22.6451513366954,-31.0830181478507,28.6903465092421));
#75764=CARTESIAN_POINT('Origin',(9.86169260701004,0.,0.));
#75765=CARTESIAN_POINT('',(22.3997512812625,-28.1746991546599,25.5334940662887));
#75766=CARTESIAN_POINT('Origin',(22.4,-28.1776468044757,25.536693610611));
#75767=CARTESIAN_POINT('',(23.3381365738089,-31.3486557215378,28.3998553597108));
#75768=CARTESIAN_POINT('Origin',(14.1732738814488,0.,0.));
#75769=CARTESIAN_POINT('',(23.1003542130464,-28.4390960806318,25.2349903818335));
#75770=CARTESIAN_POINT('Origin',(23.1,-28.4347618483503,25.2302758333634));
#75771=CARTESIAN_POINT('',(24.1697957402248,-31.5148708405159,28.2152957791621));
#75772=CARTESIAN_POINT('Origin',(8.01433437672607,0.,0.));
#75773=CARTESIAN_POINT('',(24.100209736014,-28.63627437808,25.0101230658929));
#75774=CARTESIAN_POINT('Origin',(24.1,-28.6275981312563,25.0004625004277));
#75775=CARTESIAN_POINT('',(29.9005519666592,-31.2759009022694,28.4799582645661));
#75776=CARTESIAN_POINT('Origin',(97.7155570771055,0.,0.));
#75777=CARTESIAN_POINT('',(30.4426385593966,-28.6485037699886,25.610513477472));
#75778=CARTESIAN_POINT('Origin',(30.5,-28.3704830873816,25.3068802776753));
#75779=CARTESIAN_POINT('',(29.9040600247032,-30.9143101784803,28.872052684018));
#75780=CARTESIAN_POINT('Origin',(35.8405517186909,0.,0.));
#75781=CARTESIAN_POINT('',(30.5047502791291,-28.0262504068355,25.6645373580546));
#75782=CARTESIAN_POINT('Origin',(30.5,-28.0490892825384,25.6899024992348));
#75783=CARTESIAN_POINT('',(17.5,-30.9143101784803,28.872052684018));
#75784=CARTESIAN_POINT('Origin',(17.5,-32.7483999433363,27.4791703140996));
#75785=CARTESIAN_POINT('Origin',(17.5,0.,0.));
#75786=CARTESIAN_POINT('',(0.600000000000001,-28.1860830985703,31.5410006112756));
#75787=CARTESIAN_POINT('Origin',(0.600000000000001,0.,0.));
#75788=CARTESIAN_POINT('',(1.67735469196904,-28.872052684018,30.9143101784803));
#75789=CARTESIAN_POINT('Origin',(8.14497546096349,0.,0.));
#75790=CARTESIAN_POINT('',(5.09593997529677,-28.872052684018,30.9143101784803));
#75791=CARTESIAN_POINT('',(17.5,-28.872052684018,30.9143101784803));
#75792=CARTESIAN_POINT('',(5.09944803334083,-28.4799582645661,31.2759009022694));
#75793=CARTESIAN_POINT('Origin',(-0.840551718690872,0.,0.));
#75794=CARTESIAN_POINT('',(10.8302042597752,-28.2152957791621,31.5148708405159));
#75795=CARTESIAN_POINT('Origin',(-62.7155570771055,0.,0.));
#75796=CARTESIAN_POINT('',(11.6618634261911,-28.3998553597108,31.3486557215378));
#75797=CARTESIAN_POINT('Origin',(26.9856656232739,0.,0.));
#75798=CARTESIAN_POINT('',(12.3548486633046,-28.6903465092421,31.0830181478507));
#75799=CARTESIAN_POINT('Origin',(20.8267261185512,0.,0.));
#75800=CARTESIAN_POINT('',(13.103292255208,-28.872052684018,30.9143101784803));
#75801=CARTESIAN_POINT('Origin',(25.13830739299,0.,0.));
#75802=CARTESIAN_POINT('',(21.896707744792,-28.872052684018,30.9143101784803));
#75803=CARTESIAN_POINT('',(17.5,-28.872052684018,30.9143101784803));
#75804=CARTESIAN_POINT('',(22.6451513366954,-28.6903465092421,31.0830181478507));
#75805=CARTESIAN_POINT('Origin',(9.86169260701006,0.,0.));
#75806=CARTESIAN_POINT('',(23.3381365738089,-28.3998553597108,31.3486557215378));
#75807=CARTESIAN_POINT('Origin',(14.1732738814488,0.,0.));
#75808=CARTESIAN_POINT('',(24.1697957402248,-28.2152957791621,31.5148708405159));
#75809=CARTESIAN_POINT('Origin',(8.01433437672609,0.,0.));
#75810=CARTESIAN_POINT('',(29.9005519666592,-28.4799582645661,31.2759009022694));
#75811=CARTESIAN_POINT('Origin',(97.7155570771053,0.,0.));
#75812=CARTESIAN_POINT('',(29.9040600247032,-28.872052684018,30.9143101784803));
#75813=CARTESIAN_POINT('Origin',(35.8405517186909,0.,0.));
#75814=CARTESIAN_POINT('',(17.5,-28.872052684018,30.9143101784803));
#75815=CARTESIAN_POINT('Origin',(33.1,-25.6899024992348,28.0490892825384));
#75816=CARTESIAN_POINT('',(30.5247014514712,-25.5580037650976,27.9303271288835));
#75817=CARTESIAN_POINT('Origin',(30.5,-25.6899024992348,28.0490892825384));
#75818=CARTESIAN_POINT('',(30.4955273645547,-25.3305554259542,28.3921611545025));
#75819=CARTESIAN_POINT('Origin',(30.5,-25.3068802776753,28.3704830873816));
#75820=CARTESIAN_POINT('',(24.1012882089558,-25.0597981705973,28.6808880677203));
#75821=CARTESIAN_POINT('Origin',(24.1,-25.0004625004277,28.6275981312563));
#75822=CARTESIAN_POINT('',(23.1004586919557,-25.2363809880999,28.4403745085892));
#75823=CARTESIAN_POINT('Origin',(23.1,-25.2302758333634,28.4347618483503));
#75824=CARTESIAN_POINT('',(22.399682944576,-25.5326149758775,28.1738892734932));
#75825=CARTESIAN_POINT('Origin',(22.4,-25.536693610611,28.1776468044757));
#75826=CARTESIAN_POINT('',(21.7998387845652,-25.684597735621,28.0443128519265));
#75827=CARTESIAN_POINT('Origin',(21.8,-25.6899024992348,28.0490892825384));
#75828=CARTESIAN_POINT('',(13.2021921742626,-25.6177694167211,27.9841403633154));
#75829=CARTESIAN_POINT('Origin',(13.2,-25.6899024992348,28.0490892825384));
#75830=CARTESIAN_POINT('',(12.6002487187375,-25.5334940662887,28.1746991546599));
#75831=CARTESIAN_POINT('Origin',(12.6,-25.536693610611,28.1776468044757));
#75832=CARTESIAN_POINT('',(11.8996457869536,-25.2349903818335,28.4390960806318));
#75833=CARTESIAN_POINT('Origin',(11.9,-25.2302758333634,28.4347618483503));
#75834=CARTESIAN_POINT('',(10.899790263986,-25.0101230658929,28.63627437808));
#75835=CARTESIAN_POINT('Origin',(10.9,-25.0004625004277,28.6275981312563));
#75836=CARTESIAN_POINT('',(4.55736144060343,-25.610513477472,28.6485037699886));
#75837=CARTESIAN_POINT('Origin',(4.5,-25.3068802776753,28.3704830873816));
#75838=CARTESIAN_POINT('',(4.49524972087093,-25.6645373580546,28.0262504068355));
#75839=CARTESIAN_POINT('Origin',(4.5,-25.6899024992348,28.0490892825384));
#75840=CARTESIAN_POINT('',(1.90350512467335,-25.6398056289004,28.0039818578826));
#75841=CARTESIAN_POINT('Origin',(1.9,-25.6899024992348,28.0490892825384));
#75842=CARTESIAN_POINT('Ctrl Pts',(0.13820771414163,-28.2484175959528,32.1029248328492));
#75843=CARTESIAN_POINT('Ctrl Pts',(0.370217470902555,-28.2175888910028,
31.8210099935422));
#75844=CARTESIAN_POINT('Ctrl Pts',(0.600000000000005,-28.1860830985703,
31.5410006112756));
#75845=CARTESIAN_POINT('Origin',(1.9,-23.1619558369422,30.170288394504));
#75846=CARTESIAN_POINT('',(5.09593997529677,-25.4310730087083,33.8016349549212));
#75847=CARTESIAN_POINT('',(17.5,-25.4310730087083,33.8016349549212));
#75848=CARTESIAN_POINT('',(4.47529854852883,-23.0679019220779,30.0197706669552));
#75849=CARTESIAN_POINT('Origin',(4.5,-23.1619558369422,30.170288394504));
#75850=CARTESIAN_POINT('',(5.09944803334083,-25.8552568383243,33.4782869009794));
#75851=CARTESIAN_POINT('Origin',(-0.840551718690874,0.,0.));
#75852=CARTESIAN_POINT('',(4.50447263544529,-23.562215640718,29.8759744160904));
#75853=CARTESIAN_POINT('Origin',(4.5,-23.5449780585017,29.8488945896607));
#75854=CARTESIAN_POINT('',(10.8302042597752,-26.1365544445335,33.2591419277157));
#75855=CARTESIAN_POINT('Origin',(-62.7155570771055,0.,0.));
#75856=CARTESIAN_POINT('',(10.8987117910442,-23.893572647341,29.6594674741542));
#75857=CARTESIAN_POINT('Origin',(10.9,-23.8513958357493,29.5917795457861));
#75858=CARTESIAN_POINT('',(11.6618634261911,-25.9408160718628,33.4120346810215));
#75859=CARTESIAN_POINT('Origin',(26.9856656232739,0.,0.));
#75860=CARTESIAN_POINT('',(11.8995413080444,-23.6260497451375,29.7916028606322));
#75861=CARTESIAN_POINT('Origin',(11.9,-23.6215825028136,29.784615828692));
#75862=CARTESIAN_POINT('',(12.3548486633046,-25.6287708710599,33.6519851366708));
#75863=CARTESIAN_POINT('Origin',(20.8267261185512,0.,0.));
#75864=CARTESIAN_POINT('',(12.600317055424,-23.312172527411,30.0370617130518));
#75865=CARTESIAN_POINT('Origin',(12.6,-23.315164725566,30.0417308725666));
#75866=CARTESIAN_POINT('',(13.103292255208,-25.4310730087083,33.8016349549212));
#75867=CARTESIAN_POINT('Origin',(25.13830739299,0.,0.));
#75868=CARTESIAN_POINT('',(13.2001612154348,-23.1581731335784,30.1642348036977));
#75869=CARTESIAN_POINT('Origin',(13.2,-23.1619558369422,30.170288394504));
#75870=CARTESIAN_POINT('',(21.896707744792,-25.4310730087083,33.8016349549212));
#75871=CARTESIAN_POINT('',(17.5,-25.4310730087083,33.8016349549212));
#75872=CARTESIAN_POINT('',(21.7978078257374,-23.1105194160696,30.0879729141313));
#75873=CARTESIAN_POINT('Origin',(21.8,-23.1619558369422,30.170288394504));
#75874=CARTESIAN_POINT('',(22.6451513366954,-25.6287708710599,33.6519851366708));
#75875=CARTESIAN_POINT('Origin',(9.86169260701004,0.,0.));
#75876=CARTESIAN_POINT('',(22.3997512812625,-23.3128174522151,30.038068082493));
#75877=CARTESIAN_POINT('Origin',(22.4,-23.315164725566,30.0417308725666));
#75878=CARTESIAN_POINT('',(23.3381365738089,-25.9408160718628,33.4120346810215));
#75879=CARTESIAN_POINT('Origin',(14.1732738814488,0.,0.));
#75880=CARTESIAN_POINT('',(23.1003542130464,-23.6250322156174,29.7900113841146));
#75881=CARTESIAN_POINT('Origin',(23.1,-23.6215825028136,29.784615828692));
#75882=CARTESIAN_POINT('',(24.1697957402248,-26.1365544445335,33.2591419277157));
#75883=CARTESIAN_POINT('Origin',(8.01433437672608,0.,0.));
#75884=CARTESIAN_POINT('',(24.100209736014,-23.8582627313001,29.6027999600046));
#75885=CARTESIAN_POINT('Origin',(24.1,-23.8513958357493,29.5917795457861));
#75886=CARTESIAN_POINT('',(29.9005519666592,-25.8552568383243,33.4782869009794));
#75887=CARTESIAN_POINT('Origin',(97.7155570771056,0.,0.));
#75888=CARTESIAN_POINT('',(30.4426385593966,-23.7660496304069,30.1961927037808));
#75889=CARTESIAN_POINT('Origin',(30.5,-23.5449780585017,29.8488945896607));
#75890=CARTESIAN_POINT('',(29.9040600247032,-25.4310730087083,33.8016349549212));
#75891=CARTESIAN_POINT('Origin',(35.8405517186909,0.,0.));
#75892=CARTESIAN_POINT('',(30.5047502791291,-23.1438685456221,30.1413426776677));
#75893=CARTESIAN_POINT('Origin',(30.5,-23.1619558369422,30.170288394504));
#75894=CARTESIAN_POINT('',(17.5,-25.4310730087083,33.8016349549212));
#75895=CARTESIAN_POINT('Origin',(17.5,-27.4791703140996,32.7483999433363));
#75896=CARTESIAN_POINT('Origin',(17.5,0.,0.));
#75897=CARTESIAN_POINT('',(0.600000000000001,-22.2808358845789,35.9562839053824));
#75898=CARTESIAN_POINT('Origin',(0.600000000000001,0.,0.));
#75899=CARTESIAN_POINT('',(1.67735469196904,-23.0652077022745,35.4582316768749));
#75900=CARTESIAN_POINT('Origin',(8.14497546096349,0.,0.));
#75901=CARTESIAN_POINT('',(5.09593997529677,-23.0652077022745,35.4582316768749));
#75902=CARTESIAN_POINT('',(17.5,-23.0652077022745,35.4582316768749));
#75903=CARTESIAN_POINT('',(5.09944803334083,-22.6162805078382,35.7462425436685));
#75904=CARTESIAN_POINT('Origin',(-0.840551718690874,0.,0.));
#75905=CARTESIAN_POINT('',(10.8302042597752,-22.3141421459872,35.9356238333033));
#75906=CARTESIAN_POINT('Origin',(-62.7155570771055,0.,0.));
#75907=CARTESIAN_POINT('',(11.6618634261911,-22.5247608043154,35.8039823302992));
#75908=CARTESIAN_POINT('Origin',(26.9856656232739,0.,0.));
#75909=CARTESIAN_POINT('',(12.3548486633046,-22.856966221146,35.5928236469852));
#75910=CARTESIAN_POINT('Origin',(20.8267261185512,0.,0.));
#75911=CARTESIAN_POINT('',(13.103292255208,-23.0652077022745,35.4582316768749));
#75912=CARTESIAN_POINT('Origin',(25.13830739299,0.,0.));
#75913=CARTESIAN_POINT('',(21.896707744792,-23.0652077022745,35.4582316768749));
#75914=CARTESIAN_POINT('',(17.5,-23.0652077022745,35.4582316768749));
#75915=CARTESIAN_POINT('',(22.6451513366954,-22.856966221146,35.5928236469852));
#75916=CARTESIAN_POINT('Origin',(9.86169260701006,0.,0.));
#75917=CARTESIAN_POINT('',(23.3381365738089,-22.5247608043154,35.8039823302992));
#75918=CARTESIAN_POINT('Origin',(14.1732738814488,0.,0.));
#75919=CARTESIAN_POINT('',(24.1697957402248,-22.3141421459872,35.9356238333033));
#75920=CARTESIAN_POINT('Origin',(8.01433437672609,0.,0.));
#75921=CARTESIAN_POINT('',(29.9005519666592,-22.6162805078382,35.7462425436685));
#75922=CARTESIAN_POINT('Origin',(97.7155570771054,0.,0.));
#75923=CARTESIAN_POINT('',(29.9040600247032,-23.0652077022745,35.4582316768749));
#75924=CARTESIAN_POINT('Origin',(35.8405517186909,0.,0.));
#75925=CARTESIAN_POINT('',(17.5,-23.0652077022745,35.4582316768749));
#75926=CARTESIAN_POINT('Origin',(33.1,-20.4289419162443,32.0839653438087));
#75927=CARTESIAN_POINT('',(30.5247014514712,-20.3196698518115,31.9441034793054));
#75928=CARTESIAN_POINT('Origin',(30.5,-20.4289419162443,32.0839653438087));
#75929=CARTESIAN_POINT('',(30.4955273645547,-20.01548032708,32.3594252187343));
#75930=CARTESIAN_POINT('Origin',(30.5,-19.9959292143521,32.3339653438087));
#75931=CARTESIAN_POINT('',(24.1012882089558,-19.6986995804965,32.5967492173916));
#75932=CARTESIAN_POINT('Origin',(24.1,-19.6495190528383,32.5339653438087));
#75933=CARTESIAN_POINT('',(23.1004586919557,-19.9143644494691,32.3905528841213));
#75934=CARTESIAN_POINT('Origin',(23.1,-19.9093266739737,32.3839653438087));
#75935=CARTESIAN_POINT('',(22.399682944576,-20.2523726527878,32.1795566506761));
#75936=CARTESIAN_POINT('Origin',(22.4,-20.2557368354874,32.1839653438087));
#75937=CARTESIAN_POINT('',(21.7998387845652,-20.4245471623811,32.0783403153759));
#75938=CARTESIAN_POINT('Origin',(21.8,-20.4289419162443,32.0839653438087));
#75939=CARTESIAN_POINT('',(13.2021921742626,-20.3691829588007,32.0074773662801));
#75940=CARTESIAN_POINT('Origin',(13.2,-20.4289419162443,32.0839653438087));
#75941=CARTESIAN_POINT('',(12.6002487187375,-20.2530977534517,32.180506880376));
#75942=CARTESIAN_POINT('Origin',(12.6,-20.2557368354874,32.1839653438087));
#75943=CARTESIAN_POINT('',(11.8996457869536,-19.9132169663217,32.3890524021132));
#75944=CARTESIAN_POINT('Origin',(11.9,-19.9093266739737,32.3839653438087));
#75945=CARTESIAN_POINT('',(10.899790263986,-19.6575262381569,32.544187318536));
#75946=CARTESIAN_POINT('Origin',(10.9,-19.6495190528383,32.5339653438087));
#75947=CARTESIAN_POINT('',(4.55736144060343,-20.2466717586953,32.6604876193617));
#75948=CARTESIAN_POINT('Origin',(4.5,-19.9959292143521,32.3339653438087));
#75949=CARTESIAN_POINT('',(4.49524972087093,-20.4079280576995,32.0570688314042));
#75950=CARTESIAN_POINT('Origin',(4.5,-20.4289419162443,32.0839653438087));
#75951=CARTESIAN_POINT('',(1.90350512467335,-20.387438952028,32.0308439720488));
#75952=CARTESIAN_POINT('Origin',(1.9,-20.4289419162443,32.0839653438087));
#75953=CARTESIAN_POINT('Ctrl Pts',(0.138207714141625,-22.244646263818,36.5204955072697));
#75954=CARTESIAN_POINT('Ctrl Pts',(0.370217470898828,-22.2632399142706,
36.2375102394012));
#75955=CARTESIAN_POINT('Ctrl Pts',(0.600000000000003,-22.2808358845789,
35.9562839053824));
#75956=CARTESIAN_POINT('Origin',(1.9,-17.5710580837557,33.7339653438087));
#75957=CARTESIAN_POINT('',(5.09593997529677,-19.1751255543105,37.7041716521717));
#75958=CARTESIAN_POINT('',(17.5,-19.1751255543105,37.7041716521717));
#75959=CARTESIAN_POINT('',(4.47529854852883,-17.5045701882916,33.5694020278343));
#75960=CARTESIAN_POINT('Origin',(4.5,-17.5710580837557,33.7339653438087));
#75961=CARTESIAN_POINT('',(5.09944803334083,-19.6490138787379,37.459394730737));
#75962=CARTESIAN_POINT('Origin',(-0.840551718690876,0.,0.));
#75963=CARTESIAN_POINT('',(4.50447263544529,-18.0163441277467,33.5136270415661));
#75964=CARTESIAN_POINT('Origin',(4.5,-18.0040707856479,33.4839653438087));
#75965=CARTESIAN_POINT('',(10.8302042597752,-19.9640920674886,37.2924258787336));
#75966=CARTESIAN_POINT('Origin',(-62.7155570771054,0.,0.));
#75967=CARTESIAN_POINT('',(10.8987117910442,-18.3802631128033,33.3579488669236));
#75968=CARTESIAN_POINT('Origin',(10.9,-18.3504809471617,33.2839653438087));
#75969=CARTESIAN_POINT('',(11.6618634261911,-19.7447778525305,37.4090062358548));
#75970=CARTESIAN_POINT('Origin',(26.9856656232739,0.,0.));
#75971=CARTESIAN_POINT('',(11.8995413080444,-18.0938594155378,33.4416219555226));
#75972=CARTESIAN_POINT('Origin',(11.9,-18.0906733260263,33.4339653438087));
#75973=CARTESIAN_POINT('',(12.3548486633046,-19.3958063601357,37.5911252244478));
#75974=CARTESIAN_POINT('Origin',(20.8267261185512,0.,0.));
#75975=CARTESIAN_POINT('',(12.600317055424,-17.742127215612,33.6288475295616));
#75976=CARTESIAN_POINT('Origin',(12.6,-17.7442631645126,33.6339653438087));
#75977=CARTESIAN_POINT('',(13.103292255208,-19.1751255543105,37.7041716521717));
#75978=CARTESIAN_POINT('Origin',(25.13830739299,0.,0.));
#75979=CARTESIAN_POINT('',(13.2001612154348,-17.5683840431675,33.7273468611033));
#75980=CARTESIAN_POINT('Origin',(13.2,-17.5710580837557,33.7339653438087));
#75981=CARTESIAN_POINT('',(21.896707744792,-19.1751255543105,37.7041716521717));
#75982=CARTESIAN_POINT('',(17.5,-19.1751255543105,37.7041716521717));
#75983=CARTESIAN_POINT('',(21.7978078257374,-17.5346970308537,33.6439685797946));
#75984=CARTESIAN_POINT('Origin',(21.8,-17.5710580837557,33.7339653438087));
#75985=CARTESIAN_POINT('',(22.6451513366954,-19.3958063601357,37.5911252244479));
#75986=CARTESIAN_POINT('Origin',(9.86169260701005,0.,0.));
#75987=CARTESIAN_POINT('',(22.3997512812625,-17.7425875883397,33.6299506000067));
#75988=CARTESIAN_POINT('Origin',(22.4,-17.7442631645126,33.6339653438087));
#75989=CARTESIAN_POINT('',(23.3381365738089,-19.7447778525305,37.4090062358548));
#75990=CARTESIAN_POINT('Origin',(14.1732738814488,0.,0.));
#75991=CARTESIAN_POINT('',(23.1003542130464,-18.0931337015746,33.4398779649625));
#75992=CARTESIAN_POINT('Origin',(23.1,-18.0906733260263,33.4339653438087));
#75993=CARTESIAN_POINT('',(24.1697957402248,-19.9640920674886,37.2924258787336));
#75994=CARTESIAN_POINT('Origin',(8.01433437672606,0.,0.));
#75995=CARTESIAN_POINT('',(24.100209736014,-18.3553298442931,33.2960107570711));
#75996=CARTESIAN_POINT('Origin',(24.1,-18.3504809471617,33.2839653438087));
#75997=CARTESIAN_POINT('',(29.9005519666592,-19.6490138787379,37.459394730737));
#75998=CARTESIAN_POINT('Origin',(97.7155570771054,0.,0.));
#75999=CARTESIAN_POINT('',(30.4426385593966,-18.1614760990067,33.864375894796));
#76000=CARTESIAN_POINT('Origin',(30.5,-18.0040707856479,33.4839653438087));
#76001=CARTESIAN_POINT('',(29.9040600247032,-19.1751255543105,37.7041716521717));
#76002=CARTESIAN_POINT('Origin',(35.8405517186909,0.,0.));
#76003=CARTESIAN_POINT('',(30.5047502791291,-17.5582719500126,33.7023185522751));
#76004=CARTESIAN_POINT('Origin',(30.5,-17.5710580837557,33.7339653438087));
#76005=CARTESIAN_POINT('',(17.5,-19.1751255543105,37.7041716521717));
#76006=CARTESIAN_POINT('Origin',(17.5,-21.375,37.0225860117848));
#76007=CARTESIAN_POINT('Origin',(17.5,0.,0.));
#76008=CARTESIAN_POINT('',(0.600000000000001,-15.6985967468815,39.2790537077817));
#76009=CARTESIAN_POINT('Origin',(0.600000000000001,0.,0.));
#76010=CARTESIAN_POINT('',(1.67735469196904,-16.5575380560557,38.9247727484987));
#76011=CARTESIAN_POINT('Origin',(8.14497546096349,0.,0.));
#76012=CARTESIAN_POINT('',(5.09593997529677,-16.5575380560557,38.9247727484987));
#76013=CARTESIAN_POINT('',(17.5,-16.5575380560557,38.9247727484987));
#76014=CARTESIAN_POINT('',(5.09944803334083,-16.0654185122698,39.1304526938498));
#76015=CARTESIAN_POINT('Origin',(-0.840551718690872,0.,0.));
#76016=CARTESIAN_POINT('',(10.8302042597752,-15.7349845952072,39.2644910802189));
#76017=CARTESIAN_POINT('Origin',(-62.7155570771055,0.,0.));
#76018=CARTESIAN_POINT('',(11.6618634261911,-15.9652627899599,39.1714230536436));
#76019=CARTESIAN_POINT('Origin',(26.9856656232739,0.,0.));
#76020=CARTESIAN_POINT('',(12.3548486633046,-16.3290885806033,39.0211592104439));
#76021=CARTESIAN_POINT('Origin',(20.8267261185512,0.,0.));
#76022=CARTESIAN_POINT('',(13.103292255208,-16.5575380560557,38.9247727484987));
#76023=CARTESIAN_POINT('Origin',(25.13830739299,0.,0.));
#76024=CARTESIAN_POINT('',(21.896707744792,-16.5575380560557,38.9247727484987));
#76025=CARTESIAN_POINT('',(17.5,-16.5575380560557,38.9247727484987));
#76026=CARTESIAN_POINT('',(22.6451513366954,-16.3290885806033,39.0211592104439));
#76027=CARTESIAN_POINT('Origin',(9.86169260701006,0.,0.));
#76028=CARTESIAN_POINT('',(23.3381365738089,-15.9652627899599,39.1714230536436));
#76029=CARTESIAN_POINT('Origin',(14.1732738814488,0.,0.));
#76030=CARTESIAN_POINT('',(24.1697957402248,-15.7349845952072,39.2644910802189));
#76031=CARTESIAN_POINT('Origin',(8.01433437672609,0.,0.));
#76032=CARTESIAN_POINT('',(29.9005519666592,-16.0654185122698,39.1304526938498));
#76033=CARTESIAN_POINT('Origin',(97.7155570771054,0.,0.));
#76034=CARTESIAN_POINT('',(29.9040600247032,-16.5575380560557,38.9247727484987));
#76035=CARTESIAN_POINT('Origin',(35.8405517186909,0.,0.));
#76036=CARTESIAN_POINT('',(17.5,-16.5575380560557,38.9247727484987));
#76037=CARTESIAN_POINT('Origin',(33.1,-14.5472582706722,35.1439863533772));
#76038=CARTESIAN_POINT('',(30.5247014514712,-14.4639330523272,34.987274410005));
#76039=CARTESIAN_POINT('Origin',(30.5,-14.5472582706722,35.1439863533772));
#76040=CARTESIAN_POINT('',(30.4955273645547,-14.0922449867892,35.343464522354));
#76041=CARTESIAN_POINT('Origin',(30.5,-14.0774119602792,35.31499642504));
#76042=CARTESIAN_POINT('',(24.1012882089558,-13.7390659716653,35.5221746368434));
#76043=CARTESIAN_POINT('Origin',(24.1,-13.7015349119648,35.4518044823703));
#76044=CARTESIAN_POINT('',(23.1004586919557,-13.9872600241959,35.35656070068));
#76045=CARTESIAN_POINT('Origin',(23.1,-13.9834426982006,35.3491984393726));
#76046=CARTESIAN_POINT('',(22.399682944576,-14.3567722348382,35.2074644826695));
#76047=CARTESIAN_POINT('Origin',(22.4,-14.359319746515,35.2123903820423));
#76048=CARTESIAN_POINT('',(21.7998387845652,-14.5439070589317,35.137683640766));
#76049=CARTESIAN_POINT('Origin',(21.8,-14.5472582706722,35.1439863533772));
#76050=CARTESIAN_POINT('',(13.2021921742626,-14.501689183981,35.0582833660355));
#76051=CARTESIAN_POINT('Origin',(13.2,-14.5472582706722,35.1439863533772));
#76052=CARTESIAN_POINT('',(12.6002487187375,-14.3573213139379,35.208526188654));
#76053=CARTESIAN_POINT('Origin',(12.6,-14.359319746515,35.2123903820423));
#76054=CARTESIAN_POINT('',(11.8996457869536,-13.9863905298622,35.3548837560077));
#76055=CARTESIAN_POINT('Origin',(11.9,-13.9834426982006,35.3491984393726));
#76056=CARTESIAN_POINT('',(10.899790263986,-13.7076454228629,35.4632615954717));
#76057=CARTESIAN_POINT('Origin',(10.9,-13.7015349119648,35.4518044823703));
#76058=CARTESIAN_POINT('',(4.55736144060343,-14.267645163841,35.6800990794245));
#76059=CARTESIAN_POINT('Origin',(4.5,-14.0774119602792,35.31499642504));
#76060=CARTESIAN_POINT('',(4.49524972087093,-14.5312341902212,35.1138494411902));
#76061=CARTESIAN_POINT('Origin',(4.5,-14.5472582706722,35.1439863533772));
#76062=CARTESIAN_POINT('',(1.90350512467335,-14.5156102591402,35.0844651005135));
#76063=CARTESIAN_POINT('Origin',(1.9,-14.5472582706722,35.1439863533772));
#76064=CARTESIAN_POINT('Ctrl Pts',(0.138207714141622,-15.5649826112914,
39.8284094059642));
#76065=CARTESIAN_POINT('Ctrl Pts',(0.370217470894697,-15.6324336584846,
39.5529520737012));
#76066=CARTESIAN_POINT('Ctrl Pts',(0.600000000000004,-15.6985967468815,
39.2790537077817));
#76067=CARTESIAN_POINT('Origin',(1.9,-11.4462726220787,36.2726528263519));
#76068=CARTESIAN_POINT('',(5.09593997529677,-12.3365516130268,40.4610861730024));
#76069=CARTESIAN_POINT('',(17.5,-12.3365516130268,40.4610861730024));
#76070=CARTESIAN_POINT('',(4.47529854852883,-11.409370947074,36.0990440950346));
#76071=CARTESIAN_POINT('Origin',(4.5,-11.4462726220787,36.2726528263519));
#76072=CARTESIAN_POINT('',(5.09944803334083,-12.8457455753269,40.3023178069695));
#76073=CARTESIAN_POINT('Origin',(-0.840551718690874,0.,0.));
#76074=CARTESIAN_POINT('',(4.50447263544529,-11.9230551151638,36.1329850680974));
#76075=CARTESIAN_POINT('Origin',(4.5,-11.9161189324716,36.101642754689));
#76076=CARTESIAN_POINT('',(10.8302042597752,-13.1850308552911,40.1925983403042));
#76077=CARTESIAN_POINT('Origin',(-62.7155570771054,0.,0.));
#76078=CARTESIAN_POINT('',(10.8987117910442,-12.3084785844451,36.0428658633082));
#76079=CARTESIAN_POINT('Origin',(10.9,-12.291995980786,35.9648346973588));
#76080=CARTESIAN_POINT('',(11.6618634261911,-12.9488045494888,40.2693240660821));
#76081=CARTESIAN_POINT('Origin',(26.9856656232739,0.,0.));
#76082=CARTESIAN_POINT('',(11.8995413080444,-12.0118963235316,36.0755342895717));
#76083=CARTESIAN_POINT('Origin',(11.9,-12.0100881945502,36.0674407403565));
#76084=CARTESIAN_POINT('',(12.3548486633046,-12.5735100877104,40.3880779943072));
#76085=CARTESIAN_POINT('Origin',(20.8267261185512,0.,0.));
#76086=CARTESIAN_POINT('',(12.600317055424,-11.6329963463162,36.1988378309035));
#76087=CARTESIAN_POINT('Origin',(12.6,-11.6342111462358,36.2042487976867));
#76088=CARTESIAN_POINT('',(13.103292255208,-12.3365516130268,40.4610861730024));
#76089=CARTESIAN_POINT('Origin',(25.13830739299,0.,0.));
#76090=CARTESIAN_POINT('',(13.2001612154348,-11.4447884936362,36.2656705509953));
#76091=CARTESIAN_POINT('Origin',(13.2,-11.4462726220787,36.2726528263519));
#76092=CARTESIAN_POINT('',(21.896707744792,-12.3365516130268,40.4610861730024));
#76093=CARTESIAN_POINT('',(17.5,-12.3365516130268,40.4610861730024));
#76094=CARTESIAN_POINT('',(21.7978078257374,-11.4260917493401,36.1777092848303));
#76095=CARTESIAN_POINT('Origin',(21.8,-11.4462726220787,36.2726528263519));
#76096=CARTESIAN_POINT('',(22.6451513366954,-12.5735100877104,40.3880779943072));
#76097=CARTESIAN_POINT('Origin',(9.86169260701004,0.,0.));
#76098=CARTESIAN_POINT('',(22.3997512812625,-11.633258178775,36.2000040861152));
#76099=CARTESIAN_POINT('Origin',(22.4,-11.6342111462358,36.2042487976867));
#76100=CARTESIAN_POINT('',(23.3381365738089,-12.9488045494888,40.2693240660821));
#76101=CARTESIAN_POINT('Origin',(14.1732738814488,0.,0.));
#76102=CARTESIAN_POINT('',(23.1003542130464,-12.0114844755768,36.0736907752397));
#76103=CARTESIAN_POINT('Origin',(23.1,-12.0100881945502,36.0674407403565));
#76104=CARTESIAN_POINT('',(24.1697957402248,-13.1850308552911,40.1925983403042));
#76105=CARTESIAN_POINT('Origin',(8.01433437672608,0.,0.));
#76106=CARTESIAN_POINT('',(24.100209736014,-12.2946795482123,35.9775391158784));
#76107=CARTESIAN_POINT('Origin',(24.1,-12.291995980786,35.9648346973588));
#76108=CARTESIAN_POINT('',(29.9005519666592,-12.8457455753269,40.3023178069695));
#76109=CARTESIAN_POINT('Origin',(97.7155570771054,0.,0.));
#76110=CARTESIAN_POINT('',(30.4426385593966,-12.0050753064884,36.5036071604488));
#76111=CARTESIAN_POINT('Origin',(30.5,-11.9161189324716,36.101642754689));
#76112=CARTESIAN_POINT('',(29.9040600247032,-12.3365516130268,40.4610861730024));
#76113=CARTESIAN_POINT('Origin',(35.8405517186909,0.,0.));
#76114=CARTESIAN_POINT('',(30.5047502791291,-11.4391761461162,36.2392665318678));
#76115=CARTESIAN_POINT('Origin',(30.5,-11.4462726220787,36.2726528263519));
#76116=CARTESIAN_POINT('',(17.5,-12.3365516130268,40.4610861730024));
#76117=CARTESIAN_POINT('Origin',(17.5,-14.6213611271723,40.1718595385976));
#76118=CARTESIAN_POINT('Origin',(17.5,0.,0.));
#76119=CARTESIAN_POINT('',(0.600000000000001,-8.63936369090332,41.4083493394303));
#76120=CARTESIAN_POINT('Origin',(0.600000000000001,0.,0.));
#76121=CARTESIAN_POINT('',(1.67735469196904,-9.54677599452213,41.2086042970448));
#76122=CARTESIAN_POINT('Origin',(8.1449754609635,0.,0.));
#76123=CARTESIAN_POINT('',(5.09593997529677,-9.54677599452213,41.2086042970448));
#76124=CARTESIAN_POINT('',(17.5,-9.54677599452213,41.2086042970448));
#76125=CARTESIAN_POINT('',(5.09944803334083,-9.02641690470011,41.325703839893));
#76126=CARTESIAN_POINT('Origin',(-0.840551718690872,0.,0.));
#76127=CARTESIAN_POINT('',(10.8302042597752,-8.6777274997883,41.4003266344532));
#76128=CARTESIAN_POINT('Origin',(-62.7155570771055,0.,0.));
#76129=CARTESIAN_POINT('',(11.6618634261911,-8.92066834454427,41.3486599091996));
#76130=CARTESIAN_POINT('Origin',(26.9856656232739,0.,0.));
#76131=CARTESIAN_POINT('',(12.3548486633046,-9.30505984645652,41.2638565969525));
#76132=CARTESIAN_POINT('Origin',(20.8267261185512,0.,0.));
#76133=CARTESIAN_POINT('',(13.103292255208,-9.54677599452213,41.2086042970448));
#76134=CARTESIAN_POINT('Origin',(25.13830739299,0.,0.));
#76135=CARTESIAN_POINT('',(21.896707744792,-9.54677599452213,41.2086042970448));
#76136=CARTESIAN_POINT('',(17.5,-9.54677599452213,41.2086042970448));
#76137=CARTESIAN_POINT('',(22.6451513366954,-9.30505984645651,41.2638565969525));
#76138=CARTESIAN_POINT('Origin',(9.86169260701005,0.,0.));
#76139=CARTESIAN_POINT('',(23.3381365738089,-8.92066834454427,41.3486599091995));
#76140=CARTESIAN_POINT('Origin',(14.1732738814488,0.,0.));
#76141=CARTESIAN_POINT('',(24.1697957402248,-8.6777274997883,41.4003266344532));
#76142=CARTESIAN_POINT('Origin',(8.01433437672608,0.,0.));
#76143=CARTESIAN_POINT('',(29.9005519666592,-9.02641690470011,41.325703839893));
#76144=CARTESIAN_POINT('Origin',(97.7155570771054,0.,0.));
#76145=CARTESIAN_POINT('',(29.9040600247032,-9.54677599452213,41.2086042970448));
#76146=CARTESIAN_POINT('Origin',(35.8405517186909,0.,0.));
#76147=CARTESIAN_POINT('',(17.5,-9.54677599452213,41.2086042970448));
#76148=CARTESIAN_POINT('Origin',(33.1,-8.22356354381349,37.1361751213135));
#76149=CARTESIAN_POINT('',(30.5247014514712,-8.16871696615113,36.9673747121716));
#76150=CARTESIAN_POINT('Origin',(30.5,-8.22356354381349,37.1361751213135));
#76151=CARTESIAN_POINT('',(30.4955273645547,-7.74082391359484,37.253610541118));
#76152=CARTESIAN_POINT('Origin',(30.5,-7.73115966730739,37.2229992101469));
#76153=CARTESIAN_POINT('',(24.1012882089558,-7.36197779558791,37.3682767550424));
#76154=CARTESIAN_POINT('Origin',(24.1,-7.33723656610251,37.2924584812137));
#76155=CARTESIAN_POINT('',(23.1004586919557,-7.63515978098256,37.2482773116316));
#76156=CARTESIAN_POINT('Origin',(23.1,-7.63267889200617,37.2403640279136));
#76157=CARTESIAN_POINT('',(22.399682944576,-8.02494855741037,37.1656113221937));
#76158=CARTESIAN_POINT('Origin',(22.4,-8.02660199321105,37.1709047568469));
#76159=CARTESIAN_POINT('',(21.7998387845652,-8.22135769906884,37.1293862292573));
#76160=CARTESIAN_POINT('Origin',(21.8,-8.22356354381349,37.1361751213135));
#76161=CARTESIAN_POINT('',(13.2021921742626,-8.19356892151487,37.0438611660612));
#76162=CARTESIAN_POINT('Origin',(13.2,-8.22356354381349,37.1361751213135));
#76163=CARTESIAN_POINT('',(12.6002487187375,-8.02530493145534,37.1667522450638));
#76164=CARTESIAN_POINT('Origin',(12.6,-8.02660199321105,37.1709047568469));
#76165=CARTESIAN_POINT('',(11.8996457869536,-7.6345946946079,37.2464748574103));
#76166=CARTESIAN_POINT('Origin',(11.9,-7.63267889200617,37.2403640279136));
#76167=CARTESIAN_POINT('',(10.899790263986,-7.34126473779837,37.3048026141052));
#76168=CARTESIAN_POINT('Origin',(10.9,-7.33723656610251,37.2924584812137));
#76169=CARTESIAN_POINT('',(4.55736144060343,-7.85510339046016,37.6155887839604));
#76170=CARTESIAN_POINT('Origin',(4.5,-7.73115966730739,37.2229992101469));
#76171=CARTESIAN_POINT('',(4.49524972087093,-8.21301612503227,37.1037135041708));
#76172=CARTESIAN_POINT('Origin',(4.5,-8.22356354381349,37.1361751213135));
#76173=CARTESIAN_POINT('',(1.90350512467335,-8.20273209378168,37.0720625104951));
#76174=CARTESIAN_POINT('Origin',(1.9,-8.22356354381349,37.1361751213135));
#76175=CARTESIAN_POINT('Ctrl Pts',(0.138207714141624,-8.41238483838185,
41.9261572390061));
#76176=CARTESIAN_POINT('Ctrl Pts',(0.37021747089798,-8.52664381638061,41.6665974739926));
#76177=CARTESIAN_POINT('Ctrl Pts',(0.600000000000004,-8.63936369090332,
41.4083493394303));
#76178=CARTESIAN_POINT('Origin',(1.9,-4.97369795887321,37.7092141076143));
#76179=CARTESIAN_POINT('',(5.09593997529677,-5.12313779357752,41.9886110647639));
#76180=CARTESIAN_POINT('',(17.5,-5.12313779357752,41.9886110647639));
#76181=CARTESIAN_POINT('',(4.47529854852883,-4.96750374304976,37.5318349744051));
#76182=CARTESIAN_POINT('Origin',(4.5,-4.97369795887321,37.7092141076143));
#76183=CARTESIAN_POINT('',(5.09944803334083,-5.65216579287046,41.9206753505941));
#76184=CARTESIAN_POINT('Origin',(-0.840551718690874,0.,0.));
#76185=CARTESIAN_POINT('',(4.50447263544529,-5.46749010626366,37.6544606275072));
#76186=CARTESIAN_POINT('Origin',(4.5,-5.46610183537931,37.6223900187809));
#76187=CARTESIAN_POINT('',(10.8302042597752,-6.00534915250318,41.8715390397407));
#76188=CARTESIAN_POINT('Origin',(-62.7155570771055,0.,0.));
#76189=CARTESIAN_POINT('',(10.8987117910442,-5.86270716268919,37.6326386190063));
#76190=CARTESIAN_POINT('Origin',(10.9,-5.8600249365842,37.5529307477141));
#76191=CARTESIAN_POINT('',(11.6618634261911,-5.75938837262207,41.9060788618227));
#76192=CARTESIAN_POINT('Origin',(26.9856656232739,0.,0.));
#76193=CARTESIAN_POINT('',(11.8995413080444,-5.56495784004781,37.6133097693334));
#76194=CARTESIAN_POINT('Origin',(11.9,-5.56458261068053,37.6050252010142));
#76195=CARTESIAN_POINT('',(12.3548486633046,-5.3691740737731,41.9578594516632));
#76196=CARTESIAN_POINT('Origin',(20.8267261185512,0.,0.));
#76197=CARTESIAN_POINT('',(12.600317055424,-5.17040276961776,37.6689447622493));
#76198=CARTESIAN_POINT('Origin',(12.6,-5.17065950947565,37.674484472081));
#76199=CARTESIAN_POINT('',(13.103292255208,-5.12313779357752,41.9886110647639));
#76200=CARTESIAN_POINT('Origin',(25.13830739299,0.,0.));
#76201=CARTESIAN_POINT('',(13.2001612154348,-4.97344883706828,37.7020801925101));
#76202=CARTESIAN_POINT('Origin',(13.2,-4.97369795887321,37.7092141076143));
#76203=CARTESIAN_POINT('',(21.896707744792,-5.12313779357752,41.9886110647639));
#76204=CARTESIAN_POINT('',(17.5,-5.12313779357752,41.9886110647639));
#76205=CARTESIAN_POINT('',(21.7978078257374,-4.97031045190415,37.6122086000506));
#76206=CARTESIAN_POINT('Origin',(21.8,-4.97369795887321,37.7092141076143));
#76207=CARTESIAN_POINT('',(22.6451513366954,-5.3691740737731,41.9578594516632));
#76208=CARTESIAN_POINT('Origin',(9.86169260701005,0.,0.));
#76209=CARTESIAN_POINT('',(22.3997512812625,-5.17045810616098,37.6701387661531));
#76210=CARTESIAN_POINT('Origin',(22.4,-5.17065950947565,37.674484472081));
#76211=CARTESIAN_POINT('',(23.3381365738089,-5.75938837262207,41.9060788618227));
#76212=CARTESIAN_POINT('Origin',(14.1732738814488,0.,0.));
#76213=CARTESIAN_POINT('',(23.1003542130464,-5.56487237189312,37.6114227454796));
#76214=CARTESIAN_POINT('Origin',(23.1,-5.56458261068053,37.6050252010142));
#76215=CARTESIAN_POINT('',(24.1697957402248,-6.00534915250318,41.8715390397407));
#76216=CARTESIAN_POINT('Origin',(8.01433437672608,0.,0.));
#76217=CARTESIAN_POINT('',(24.100209736014,-5.8604616354671,37.565908154163));
#76218=CARTESIAN_POINT('Origin',(24.1,-5.8600249365842,37.5529307477141));
#76219=CARTESIAN_POINT('',(29.9005519666592,-5.65216579287046,41.9206753505941));
#76220=CARTESIAN_POINT('Origin',(97.7155570771054,0.,0.));
#76221=CARTESIAN_POINT('',(30.4426385593966,-5.48390637564377,38.0336947942479));
#76222=CARTESIAN_POINT('Origin',(30.5,-5.46610183537931,37.6223900187809));
#76223=CARTESIAN_POINT('',(29.9040600247032,-5.12313779357752,41.9886110647639));
#76224=CARTESIAN_POINT('Origin',(35.8405517186909,0.,0.));
#76225=CARTESIAN_POINT('',(30.5047502791291,-4.97250676352255,37.6751027358433));
#76226=CARTESIAN_POINT('Origin',(30.5,-4.97369795887321,37.7092141076143));
#76227=CARTESIAN_POINT('',(17.5,-5.12313779357752,41.9886110647639));
#76228=CARTESIAN_POINT('Origin',(17.5,-7.42345959526127,42.1005314412719));
#76229=CARTESIAN_POINT('Origin',(17.5,0.,0.));
#76230=CARTESIAN_POINT('',(0.600000000000001,-1.31762794090604,42.2794732300362));
#76231=CARTESIAN_POINT('Origin',(0.600000000000001,0.,0.));
#76232=CARTESIAN_POINT('',(1.67735469196904,-2.24593997529677,42.240333256585));
#76233=CARTESIAN_POINT('Origin',(8.14497546096349,0.,0.));
#76234=CARTESIAN_POINT('',(5.09593997529677,-2.24593997529677,42.240333256585));
#76235=CARTESIAN_POINT('',(17.5,-2.24593997529677,42.240333256585));
#76236=CARTESIAN_POINT('',(5.09944803334083,-1.71315218706844,42.2652943865761));
#76237=CARTESIAN_POINT('Origin',(-0.840551718690872,0.,0.));
#76238=CARTESIAN_POINT('',(10.8302042597752,-1.35680204543027,42.2782342134758));
#76239=CARTESIAN_POINT('Origin',(-62.7155570771055,0.,0.));
#76240=CARTESIAN_POINT('',(11.6618634261911,-1.60502390555561,42.269538656846));
#76241=CARTESIAN_POINT('Origin',(26.9856656232739,0.,0.));
#76242=CARTESIAN_POINT('',(12.3548486633046,-1.99830157746261,42.2527725812817));
#76243=CARTESIAN_POINT('Origin',(20.8267261185512,0.,0.));
#76244=CARTESIAN_POINT('',(13.103292255208,-2.24593997529677,42.240333256585));
#76245=CARTESIAN_POINT('Origin',(25.13830739299,0.,0.));
#76246=CARTESIAN_POINT('',(21.896707744792,-2.24593997529677,42.240333256585));
#76247=CARTESIAN_POINT('',(17.5,-2.24593997529677,42.240333256585));
#76248=CARTESIAN_POINT('',(22.6451513366954,-1.99830157746261,42.2527725812817));
#76249=CARTESIAN_POINT('Origin',(9.86169260701006,0.,0.));
#76250=CARTESIAN_POINT('',(23.3381365738089,-1.60502390555561,42.269538656846));
#76251=CARTESIAN_POINT('Origin',(14.1732738814488,0.,0.));
#76252=CARTESIAN_POINT('',(24.1697957402248,-1.35680204543027,42.2782342134758));
#76253=CARTESIAN_POINT('Origin',(8.01433437672608,0.,0.));
#76254=CARTESIAN_POINT('',(29.9005519666592,-1.71315218706844,42.2652943865761));
#76255=CARTESIAN_POINT('Origin',(97.7155570771054,0.,0.));
#76256=CARTESIAN_POINT('',(29.9040600247032,-2.24593997529677,42.240333256585));
#76257=CARTESIAN_POINT('Origin',(35.8405517186909,0.,0.));
#76258=CARTESIAN_POINT('',(17.5,-2.24593997529677,42.240333256585));
#76259=CARTESIAN_POINT('Origin',(33.1,-1.65,38.));
#76260=CARTESIAN_POINT('',(30.5247014514712,-1.62529854852883,37.8242400401031));
#76261=CARTESIAN_POINT('Origin',(30.5,-1.65,38.));
#76262=CARTESIAN_POINT('',(30.4955273645547,-1.15420182283181,38.0318244548267));
#76263=CARTESIAN_POINT('Origin',(30.5,-1.15,38.));
#76264=CARTESIAN_POINT('',(24.1012882089558,-0.761199649532069,38.0789626932999));
#76265=CARTESIAN_POINT('Origin',(24.1,-0.749999999999998,38.));
#76266=CARTESIAN_POINT('',(23.1004586919557,-1.05106907140133,38.0082238650069));
#76267=CARTESIAN_POINT('Origin',(23.1,-1.05,38.));
#76268=CARTESIAN_POINT('',(22.399682944576,-1.44929087888549,37.9944998683999));
#76269=CARTESIAN_POINT('Origin',(22.4,-1.45,38.));
#76270=CARTESIAN_POINT('',(21.7998387845652,-1.64900654572746,37.9929312055486));
#76271=CARTESIAN_POINT('Origin',(21.8,-1.65,38.));
#76272=CARTESIAN_POINT('',(13.2021921742626,-1.63649121351442,37.9038799896544));
#76273=CARTESIAN_POINT('Origin',(13.2,-1.65,38.));
#76274=CARTESIAN_POINT('',(12.6002487187375,-1.44944371963071,37.9956853417913));
#76275=CARTESIAN_POINT('Origin',(12.6,-1.45,38.));
#76276=CARTESIAN_POINT('',(11.8996457869536,-1.05082556284928,38.0063506678963));
#76277=CARTESIAN_POINT('Origin',(11.9,-1.05,38.));
#76278=CARTESIAN_POINT('',(10.899790263986,-0.751823438535066,38.01285608245));
#76279=CARTESIAN_POINT('Origin',(10.9,-0.749999999999998,38.));
#76280=CARTESIAN_POINT('',(4.55736144060343,-1.2038882754343,38.408147857702));
#76281=CARTESIAN_POINT('Origin',(4.5,-1.15,38.));
#76282=CARTESIAN_POINT('',(4.49524972087093,-1.64524972087093,37.9662000077121));
#76283=CARTESIAN_POINT('Origin',(4.5,-1.65,38.));
#76284=CARTESIAN_POINT('',(1.90350512467335,-1.64061806453626,37.933244060464));
#76285=CARTESIAN_POINT('Origin',(1.9,-1.65,38.));
#76286=CARTESIAN_POINT('Ctrl Pts',(0.13820771414162,-1.0041810090302,42.75));
#76287=CARTESIAN_POINT('Ctrl Pts',(0.370217470898037,-1.16177621660492,
42.5142243943562));
#76288=CARTESIAN_POINT('Ctrl Pts',(0.600000000000004,-1.31762794090604,
42.2794732300361));
#76289=CARTESIAN_POINT('Origin',(1.9,1.65,38.));
#76290=CARTESIAN_POINT('',(5.09593997529677,2.24593997529677,42.240333256585));
#76291=CARTESIAN_POINT('',(17.5,2.24593997529677,42.240333256585));
#76292=CARTESIAN_POINT('',(4.47529854852883,1.62529854852884,37.8242400401031));
#76293=CARTESIAN_POINT('Origin',(4.5,1.65,38.));
#76294=CARTESIAN_POINT('',(5.09944803334083,1.71315218706845,42.2652943865761));
#76295=CARTESIAN_POINT('Origin',(-0.840551718690874,0.,0.));
#76296=CARTESIAN_POINT('',(4.50447263544529,1.15420182283181,38.0318244548267));
#76297=CARTESIAN_POINT('Origin',(4.5,1.15,38.));
#76298=CARTESIAN_POINT('',(10.8302042597752,1.35680204543028,42.2782342134758));
#76299=CARTESIAN_POINT('Origin',(-62.7155570771055,0.,0.));
#76300=CARTESIAN_POINT('',(10.8987117910442,0.761199649532074,38.0789626932999));
#76301=CARTESIAN_POINT('Origin',(10.9,0.750000000000002,38.));
#76302=CARTESIAN_POINT('',(11.6618634261911,1.60502390555562,42.269538656846));
#76303=CARTESIAN_POINT('Origin',(26.9856656232739,0.,0.));
#76304=CARTESIAN_POINT('',(11.8995413080444,1.05106907140134,38.0082238650069));
#76305=CARTESIAN_POINT('Origin',(11.9,1.05,38.));
#76306=CARTESIAN_POINT('',(12.3548486633046,1.99830157746262,42.2527725812817));
#76307=CARTESIAN_POINT('Origin',(20.8267261185512,0.,0.));
#76308=CARTESIAN_POINT('',(12.600317055424,1.44929087888549,37.9944998683999));
#76309=CARTESIAN_POINT('Origin',(12.6,1.45,38.));
#76310=CARTESIAN_POINT('',(13.103292255208,2.24593997529677,42.240333256585));
#76311=CARTESIAN_POINT('Origin',(25.13830739299,0.,0.));
#76312=CARTESIAN_POINT('',(13.2001612154348,1.64900654572746,37.9929312055486));
#76313=CARTESIAN_POINT('Origin',(13.2,1.65,38.));
#76314=CARTESIAN_POINT('',(21.896707744792,2.24593997529677,42.240333256585));
#76315=CARTESIAN_POINT('',(17.5,2.24593997529677,42.240333256585));
#76316=CARTESIAN_POINT('',(21.7978078257374,1.63649121351443,37.9038799896544));
#76317=CARTESIAN_POINT('Origin',(21.8,1.65,38.));
#76318=CARTESIAN_POINT('',(22.6451513366954,1.99830157746262,42.2527725812817));
#76319=CARTESIAN_POINT('Origin',(9.86169260701005,0.,0.));
#76320=CARTESIAN_POINT('',(22.3997512812625,1.44944371963071,37.9956853417913));
#76321=CARTESIAN_POINT('Origin',(22.4,1.45,38.));
#76322=CARTESIAN_POINT('',(23.3381365738089,1.60502390555561,42.269538656846));
#76323=CARTESIAN_POINT('Origin',(14.1732738814488,0.,0.));
#76324=CARTESIAN_POINT('',(23.1003542130464,1.05082556284928,38.0063506678963));
#76325=CARTESIAN_POINT('Origin',(23.1,1.05,38.));
#76326=CARTESIAN_POINT('',(24.1697957402248,1.35680204543028,42.2782342134758));
#76327=CARTESIAN_POINT('Origin',(8.01433437672608,0.,0.));
#76328=CARTESIAN_POINT('',(24.100209736014,0.75182343853507,38.01285608245));
#76329=CARTESIAN_POINT('Origin',(24.1,0.750000000000002,38.));
#76330=CARTESIAN_POINT('',(29.9005519666592,1.71315218706845,42.2652943865761));
#76331=CARTESIAN_POINT('Origin',(97.7155570771054,0.,0.));
#76332=CARTESIAN_POINT('',(30.4426385593966,1.2038882754343,38.408147857702));
#76333=CARTESIAN_POINT('Origin',(30.5,1.15,38.));
#76334=CARTESIAN_POINT('',(29.9040600247032,2.24593997529677,42.240333256585));
#76335=CARTESIAN_POINT('Origin',(35.8405517186909,0.,0.));
#76336=CARTESIAN_POINT('',(30.5047502791291,1.64524972087093,37.9662000077121));
#76337=CARTESIAN_POINT('Origin',(30.5,1.65,38.));
#76338=CARTESIAN_POINT('',(17.5,2.24593997529677,42.240333256585));
#76339=CARTESIAN_POINT('Origin',(17.5,2.61768253317747E-15,42.75));
#76340=CARTESIAN_POINT('Origin',(17.5,0.,0.));
#76341=CARTESIAN_POINT('',(0.600000000000001,6.04414326732376,41.8659567209931));
#76342=CARTESIAN_POINT('Origin',(0.600000000000001,0.,0.));
#76343=CARTESIAN_POINT('',(1.67735469196905,5.12313779357752,41.9886110647639));
#76344=CARTESIAN_POINT('Origin',(8.14497546096349,0.,0.));
#76345=CARTESIAN_POINT('',(5.09593997529677,5.12313779357752,41.9886110647639));
#76346=CARTESIAN_POINT('',(17.5,5.12313779357752,41.9886110647639));
#76347=CARTESIAN_POINT('',(5.09944803334083,5.65216579287046,41.9206753505941));
#76348=CARTESIAN_POINT('Origin',(-0.840551718690872,0.,0.));
#76349=CARTESIAN_POINT('',(10.8302042597752,6.00534915250319,41.8715390397407));
#76350=CARTESIAN_POINT('Origin',(-62.7155570771055,0.,0.));
#76351=CARTESIAN_POINT('',(11.6618634261911,5.75938837262207,41.9060788618227));
#76352=CARTESIAN_POINT('Origin',(26.9856656232739,0.,0.));
#76353=CARTESIAN_POINT('',(12.3548486633046,5.3691740737731,41.9578594516632));
#76354=CARTESIAN_POINT('Origin',(20.8267261185512,0.,0.));
#76355=CARTESIAN_POINT('',(13.103292255208,5.12313779357752,41.9886110647639));
#76356=CARTESIAN_POINT('Origin',(25.13830739299,0.,0.));
#76357=CARTESIAN_POINT('',(21.896707744792,5.12313779357752,41.9886110647639));
#76358=CARTESIAN_POINT('',(17.5,5.12313779357752,41.9886110647639));
#76359=CARTESIAN_POINT('',(22.6451513366954,5.3691740737731,41.9578594516632));
#76360=CARTESIAN_POINT('Origin',(9.86169260701005,0.,0.));
#76361=CARTESIAN_POINT('',(23.3381365738089,5.75938837262207,41.9060788618227));
#76362=CARTESIAN_POINT('Origin',(14.1732738814488,0.,0.));
#76363=CARTESIAN_POINT('',(24.1697957402248,6.00534915250319,41.8715390397407));
#76364=CARTESIAN_POINT('Origin',(8.01433437672607,0.,0.));
#76365=CARTESIAN_POINT('',(29.9005519666592,5.65216579287046,41.9206753505941));
#76366=CARTESIAN_POINT('Origin',(97.7155570771054,0.,0.));
#76367=CARTESIAN_POINT('',(29.9040600247032,5.12313779357752,41.9886110647639));
#76368=CARTESIAN_POINT('Origin',(35.8405517186909,0.,0.));
#76369=CARTESIAN_POINT('',(17.5,5.12313779357752,41.9886110647639));
#76370=CARTESIAN_POINT('Origin',(33.1,4.97369795887321,37.7092141076143));
#76371=CARTESIAN_POINT('',(30.5247014514712,4.96750374304977,37.5318349744051));
#76372=CARTESIAN_POINT('Origin',(30.5,4.97369795887321,37.7092141076143));
#76373=CARTESIAN_POINT('',(30.4955273645547,5.46749010626367,37.6544606275072));
#76374=CARTESIAN_POINT('Origin',(30.5,5.46610183537932,37.6223900187809));
#76375=CARTESIAN_POINT('',(24.1012882089558,5.86270716268919,37.6326386190063));
#76376=CARTESIAN_POINT('Origin',(24.1,5.8600249365842,37.5529307477141));
#76377=CARTESIAN_POINT('',(23.1004586919557,5.56495784004782,37.6133097693334));
#76378=CARTESIAN_POINT('Origin',(23.1,5.56458261068054,37.6050252010142));
#76379=CARTESIAN_POINT('',(22.399682944576,5.17040276961776,37.6689447622493));
#76380=CARTESIAN_POINT('Origin',(22.4,5.17065950947566,37.674484472081));
#76381=CARTESIAN_POINT('',(21.7998387845652,4.97344883706828,37.7020801925101));
#76382=CARTESIAN_POINT('Origin',(21.8,4.97369795887321,37.7092141076143));
#76383=CARTESIAN_POINT('',(13.2021921742626,4.97031045190415,37.6122086000507));
#76384=CARTESIAN_POINT('Origin',(13.2,4.97369795887321,37.7092141076143));
#76385=CARTESIAN_POINT('',(12.6002487187375,5.17045810616099,37.6701387661531));
#76386=CARTESIAN_POINT('Origin',(12.6,5.17065950947566,37.674484472081));
#76387=CARTESIAN_POINT('',(11.8996457869536,5.56487237189312,37.6114227454796));
#76388=CARTESIAN_POINT('Origin',(11.9,5.56458261068054,37.6050252010142));
#76389=CARTESIAN_POINT('',(10.899790263986,5.86046163546711,37.565908154163));
#76390=CARTESIAN_POINT('Origin',(10.9,5.8600249365842,37.5529307477141));
#76391=CARTESIAN_POINT('',(4.55736144060343,5.48390637564378,38.0336947942479));
#76392=CARTESIAN_POINT('Origin',(4.5,5.46610183537932,37.6223900187809));
#76393=CARTESIAN_POINT('',(4.49524972087093,4.97250676352255,37.6751027358433));
#76394=CARTESIAN_POINT('Origin',(4.5,4.97369795887321,37.7092141076143));
#76395=CARTESIAN_POINT('',(1.90350512467335,4.97134531440729,37.6418431848034));
#76396=CARTESIAN_POINT('Origin',(1.9,4.97369795887321,37.7092141076143));
#76397=CARTESIAN_POINT('Ctrl Pts',(0.138207714141615,6.43453435214071,42.2749056435377));
#76398=CARTESIAN_POINT('Ctrl Pts',(0.370217470897385,6.23839136562575,42.0700781197336));
#76399=CARTESIAN_POINT('Ctrl Pts',(0.600000000000003,6.04414326732376,41.8659567209931));
#76400=CARTESIAN_POINT('Origin',(1.9,8.2235635438135,37.1361751213135));
#76401=CARTESIAN_POINT('',(5.09593997529677,9.54677599452213,41.2086042970448));
#76402=CARTESIAN_POINT('',(17.5,9.54677599452213,41.2086042970448));
#76403=CARTESIAN_POINT('',(4.47529854852883,8.16871696615114,36.9673747121716));
#76404=CARTESIAN_POINT('Origin',(4.5,8.2235635438135,37.1361751213135));
#76405=CARTESIAN_POINT('',(5.09944803334083,9.02641690470011,41.325703839893));
#76406=CARTESIAN_POINT('Origin',(-0.840551718690874,0.,0.));
#76407=CARTESIAN_POINT('',(4.50447263544529,7.74082391359485,37.253610541118));
#76408=CARTESIAN_POINT('Origin',(4.5,7.7311596673074,37.2229992101469));
#76409=CARTESIAN_POINT('',(10.8302042597752,8.6777274997883,41.4003266344532));
#76410=CARTESIAN_POINT('Origin',(-62.7155570771055,0.,0.));
#76411=CARTESIAN_POINT('',(10.8987117910442,7.36197779558791,37.3682767550424));
#76412=CARTESIAN_POINT('Origin',(10.9,7.33723656610251,37.2924584812137));
#76413=CARTESIAN_POINT('',(11.6618634261911,8.92066834454427,41.3486599091995));
#76414=CARTESIAN_POINT('Origin',(26.9856656232739,0.,0.));
#76415=CARTESIAN_POINT('',(11.8995413080444,7.63515978098257,37.2482773116316));
#76416=CARTESIAN_POINT('Origin',(11.9,7.63267889200617,37.2403640279136));
#76417=CARTESIAN_POINT('',(12.3548486633046,9.30505984645652,41.2638565969525));
#76418=CARTESIAN_POINT('Origin',(20.8267261185512,0.,0.));
#76419=CARTESIAN_POINT('',(12.600317055424,8.02494855741037,37.1656113221937));
#76420=CARTESIAN_POINT('Origin',(12.6,8.02660199321106,37.1709047568469));
#76421=CARTESIAN_POINT('',(13.103292255208,9.54677599452213,41.2086042970448));
#76422=CARTESIAN_POINT('Origin',(25.13830739299,0.,0.));
#76423=CARTESIAN_POINT('',(13.2001612154348,8.22135769906884,37.1293862292573));
#76424=CARTESIAN_POINT('Origin',(13.2,8.2235635438135,37.1361751213135));
#76425=CARTESIAN_POINT('',(21.896707744792,9.54677599452213,41.2086042970448));
#76426=CARTESIAN_POINT('',(17.5,9.54677599452213,41.2086042970448));
#76427=CARTESIAN_POINT('',(21.7978078257374,8.19356892151488,37.0438611660612));
#76428=CARTESIAN_POINT('Origin',(21.8,8.2235635438135,37.1361751213135));
#76429=CARTESIAN_POINT('',(22.6451513366954,9.30505984645652,41.2638565969525));
#76430=CARTESIAN_POINT('Origin',(9.86169260701005,0.,0.));
#76431=CARTESIAN_POINT('',(22.3997512812625,8.02530493145534,37.1667522450638));
#76432=CARTESIAN_POINT('Origin',(22.4,8.02660199321106,37.1709047568469));
#76433=CARTESIAN_POINT('',(23.3381365738089,8.92066834454427,41.3486599091995));
#76434=CARTESIAN_POINT('Origin',(14.1732738814488,0.,0.));
#76435=CARTESIAN_POINT('',(23.1003542130464,7.6345946946079,37.2464748574103));
#76436=CARTESIAN_POINT('Origin',(23.1,7.63267889200617,37.2403640279136));
#76437=CARTESIAN_POINT('',(24.1697957402248,8.6777274997883,41.4003266344532));
#76438=CARTESIAN_POINT('Origin',(8.01433437672608,0.,0.));
#76439=CARTESIAN_POINT('',(24.100209736014,7.34126473779837,37.3048026141052));
#76440=CARTESIAN_POINT('Origin',(24.1,7.33723656610251,37.2924584812137));
#76441=CARTESIAN_POINT('',(29.9005519666592,9.02641690470011,41.325703839893));
#76442=CARTESIAN_POINT('Origin',(97.7155570771055,0.,0.));
#76443=CARTESIAN_POINT('',(30.4426385593966,7.85510339046017,37.6155887839604));
#76444=CARTESIAN_POINT('Origin',(30.5,7.7311596673074,37.2229992101469));
#76445=CARTESIAN_POINT('',(29.9040600247032,9.54677599452213,41.2086042970448));
#76446=CARTESIAN_POINT('Origin',(35.8405517186909,0.,0.));
#76447=CARTESIAN_POINT('',(30.5047502791291,8.21301612503228,37.1037135041708));
#76448=CARTESIAN_POINT('Origin',(30.5,8.2235635438135,37.1361751213135));
#76449=CARTESIAN_POINT('',(17.5,9.54677599452213,41.2086042970448));
#76450=CARTESIAN_POINT('Origin',(17.5,7.42345959526128,42.1005314412719));
#76451=CARTESIAN_POINT('Origin',(17.5,0.,0.));
#76452=CARTESIAN_POINT('',(0.600000000000001,13.22226624086,40.1803643021789));
#76453=CARTESIAN_POINT('Origin',(0.600000000000001,0.,0.));
#76454=CARTESIAN_POINT('',(1.67735469196905,12.3365516130268,40.4610861730024));
#76455=CARTESIAN_POINT('Origin',(8.14497546096349,0.,0.));
#76456=CARTESIAN_POINT('',(5.09593997529677,12.3365516130268,40.4610861730024));
#76457=CARTESIAN_POINT('',(17.5,12.3365516130268,40.4610861730024));
#76458=CARTESIAN_POINT('',(5.09944803334083,12.8457455753269,40.3023178069695));
#76459=CARTESIAN_POINT('Origin',(-0.840551718690872,0.,0.));
#76460=CARTESIAN_POINT('',(10.8302042597752,13.1850308552911,40.1925983403042));
#76461=CARTESIAN_POINT('Origin',(-62.7155570771055,0.,0.));
#76462=CARTESIAN_POINT('',(11.6618634261911,12.9488045494888,40.2693240660821));
#76463=CARTESIAN_POINT('Origin',(26.9856656232739,0.,0.));
#76464=CARTESIAN_POINT('',(12.3548486633046,12.5735100877104,40.3880779943072));
#76465=CARTESIAN_POINT('Origin',(20.8267261185512,0.,0.));
#76466=CARTESIAN_POINT('',(13.103292255208,12.3365516130268,40.4610861730024));
#76467=CARTESIAN_POINT('Origin',(25.13830739299,0.,0.));
#76468=CARTESIAN_POINT('',(21.896707744792,12.3365516130268,40.4610861730024));
#76469=CARTESIAN_POINT('',(17.5,12.3365516130268,40.4610861730024));
#76470=CARTESIAN_POINT('',(22.6451513366954,12.5735100877104,40.3880779943072));
#76471=CARTESIAN_POINT('Origin',(9.86169260701005,0.,0.));
#76472=CARTESIAN_POINT('',(23.3381365738089,12.9488045494888,40.2693240660821));
#76473=CARTESIAN_POINT('Origin',(14.1732738814488,0.,0.));
#76474=CARTESIAN_POINT('',(24.1697957402248,13.1850308552911,40.1925983403042));
#76475=CARTESIAN_POINT('Origin',(8.01433437672608,0.,0.));
#76476=CARTESIAN_POINT('',(29.9005519666592,12.8457455753269,40.3023178069695));
#76477=CARTESIAN_POINT('Origin',(97.7155570771054,0.,0.));
#76478=CARTESIAN_POINT('',(29.9040600247032,12.3365516130268,40.4610861730024));
#76479=CARTESIAN_POINT('Origin',(35.8405517186909,0.,0.));
#76480=CARTESIAN_POINT('',(17.5,12.3365516130268,40.4610861730024));
#76481=CARTESIAN_POINT('Origin',(33.1,11.4462726220787,36.2726528263519));
#76482=CARTESIAN_POINT('',(30.5247014514712,11.409370947074,36.0990440950346));
#76483=CARTESIAN_POINT('Origin',(30.5,11.4462726220787,36.2726528263519));
#76484=CARTESIAN_POINT('',(30.4955273645547,11.9230551151638,36.1329850680974));
#76485=CARTESIAN_POINT('Origin',(30.5,11.9161189324716,36.101642754689));
#76486=CARTESIAN_POINT('',(24.1012882089558,12.3084785844451,36.0428658633082));
#76487=CARTESIAN_POINT('Origin',(24.1,12.291995980786,35.9648346973588));
#76488=CARTESIAN_POINT('',(23.1004586919557,12.0118963235317,36.0755342895717));
#76489=CARTESIAN_POINT('Origin',(23.1,12.0100881945502,36.0674407403565));
#76490=CARTESIAN_POINT('',(22.399682944576,11.6329963463162,36.1988378309035));
#76491=CARTESIAN_POINT('Origin',(22.4,11.6342111462359,36.2042487976867));
#76492=CARTESIAN_POINT('',(21.7998387845652,11.4447884936362,36.2656705509953));
#76493=CARTESIAN_POINT('Origin',(21.8,11.4462726220787,36.2726528263519));
#76494=CARTESIAN_POINT('',(13.2021921742626,11.4260917493401,36.1777092848303));
#76495=CARTESIAN_POINT('Origin',(13.2,11.4462726220787,36.2726528263519));
#76496=CARTESIAN_POINT('',(12.6002487187375,11.633258178775,36.2000040861152));
#76497=CARTESIAN_POINT('Origin',(12.6,11.6342111462359,36.2042487976867));
#76498=CARTESIAN_POINT('',(11.8996457869536,12.0114844755768,36.0736907752397));
#76499=CARTESIAN_POINT('Origin',(11.9,12.0100881945502,36.0674407403565));
#76500=CARTESIAN_POINT('',(10.899790263986,12.2946795482123,35.9775391158784));
#76501=CARTESIAN_POINT('Origin',(10.9,12.291995980786,35.9648346973588));
#76502=CARTESIAN_POINT('',(4.55736144060343,12.0050753064884,36.5036071604488));
#76503=CARTESIAN_POINT('Origin',(4.5,11.9161189324716,36.101642754689));
#76504=CARTESIAN_POINT('',(4.49524972087093,11.4391761461162,36.2392665318678));
#76505=CARTESIAN_POINT('Origin',(4.5,11.4462726220787,36.2726528263519));
#76506=CARTESIAN_POINT('',(1.90350512467335,11.4322568815947,36.2067139516643));
#76507=CARTESIAN_POINT('Origin',(1.9,11.4462726220787,36.2726528263519));
#76508=CARTESIAN_POINT('Ctrl Pts',(0.138207714141621,13.6777396430533,40.515309671231));
#76509=CARTESIAN_POINT('Ctrl Pts',(0.370217470897303,13.4490085829899,40.3476538099289));
#76510=CARTESIAN_POINT('Ctrl Pts',(0.600000000000004,13.22226624086,40.1803643021789));
#76511=CARTESIAN_POINT('Origin',(1.9,14.5472582706722,35.1439863533772));
#76512=CARTESIAN_POINT('',(5.09593997529677,16.5575380560557,38.9247727484987));
#76513=CARTESIAN_POINT('',(17.5,16.5575380560557,38.9247727484987));
#76514=CARTESIAN_POINT('',(4.47529854852883,14.4639330523272,34.987274410005));
#76515=CARTESIAN_POINT('Origin',(4.5,14.5472582706722,35.1439863533772));
#76516=CARTESIAN_POINT('',(5.09944803334083,16.0654185122698,39.1304526938498));
#76517=CARTESIAN_POINT('Origin',(-0.840551718690874,0.,0.));
#76518=CARTESIAN_POINT('',(4.50447263544529,14.0922449867892,35.343464522354));
#76519=CARTESIAN_POINT('Origin',(4.5,14.0774119602792,35.31499642504));
#76520=CARTESIAN_POINT('',(10.8302042597752,15.7349845952072,39.2644910802189));
#76521=CARTESIAN_POINT('Origin',(-62.7155570771055,0.,0.));
#76522=CARTESIAN_POINT('',(10.8987117910442,13.7390659716653,35.5221746368434));
#76523=CARTESIAN_POINT('Origin',(10.9,13.7015349119648,35.4518044823703));
#76524=CARTESIAN_POINT('',(11.6618634261911,15.9652627899599,39.1714230536436));
#76525=CARTESIAN_POINT('Origin',(26.9856656232739,0.,0.));
#76526=CARTESIAN_POINT('',(11.8995413080444,13.9872600241959,35.35656070068));
#76527=CARTESIAN_POINT('Origin',(11.9,13.9834426982006,35.3491984393726));
#76528=CARTESIAN_POINT('',(12.3548486633046,16.3290885806033,39.0211592104439));
#76529=CARTESIAN_POINT('Origin',(20.8267261185512,0.,0.));
#76530=CARTESIAN_POINT('',(12.600317055424,14.3567722348383,35.2074644826695));
#76531=CARTESIAN_POINT('Origin',(12.6,14.359319746515,35.2123903820423));
#76532=CARTESIAN_POINT('',(13.103292255208,16.5575380560557,38.9247727484987));
#76533=CARTESIAN_POINT('Origin',(25.13830739299,0.,0.));
#76534=CARTESIAN_POINT('',(13.2001612154348,14.5439070589318,35.137683640766));
#76535=CARTESIAN_POINT('Origin',(13.2,14.5472582706722,35.1439863533772));
#76536=CARTESIAN_POINT('',(21.896707744792,16.5575380560557,38.9247727484987));
#76537=CARTESIAN_POINT('',(17.5,16.5575380560557,38.9247727484987));
#76538=CARTESIAN_POINT('',(21.7978078257374,14.501689183981,35.0582833660355));
#76539=CARTESIAN_POINT('Origin',(21.8,14.5472582706722,35.1439863533772));
#76540=CARTESIAN_POINT('',(22.6451513366954,16.3290885806033,39.0211592104439));
#76541=CARTESIAN_POINT('Origin',(9.86169260701006,0.,0.));
#76542=CARTESIAN_POINT('',(22.3997512812625,14.3573213139379,35.208526188654));
#76543=CARTESIAN_POINT('Origin',(22.4,14.359319746515,35.2123903820423));
#76544=CARTESIAN_POINT('',(23.3381365738089,15.9652627899599,39.1714230536436));
#76545=CARTESIAN_POINT('Origin',(14.1732738814488,0.,0.));
#76546=CARTESIAN_POINT('',(23.1003542130464,13.9863905298622,35.3548837560077));
#76547=CARTESIAN_POINT('Origin',(23.1,13.9834426982006,35.3491984393726));
#76548=CARTESIAN_POINT('',(24.1697957402248,15.7349845952072,39.2644910802189));
#76549=CARTESIAN_POINT('Origin',(8.01433437672608,0.,0.));
#76550=CARTESIAN_POINT('',(24.100209736014,13.7076454228629,35.4632615954717));
#76551=CARTESIAN_POINT('Origin',(24.1,13.7015349119648,35.4518044823703));
#76552=CARTESIAN_POINT('',(29.9005519666592,16.0654185122698,39.1304526938498));
#76553=CARTESIAN_POINT('Origin',(97.7155570771054,0.,0.));
#76554=CARTESIAN_POINT('',(30.4426385593966,14.267645163841,35.6800990794245));
#76555=CARTESIAN_POINT('Origin',(30.5,14.0774119602792,35.31499642504));
#76556=CARTESIAN_POINT('',(29.9040600247032,16.5575380560557,38.9247727484987));
#76557=CARTESIAN_POINT('Origin',(35.8405517186909,0.,0.));
#76558=CARTESIAN_POINT('',(30.5047502791291,14.5312341902212,35.1138494411902));
#76559=CARTESIAN_POINT('Origin',(30.5,14.5472582706722,35.1439863533772));
#76560=CARTESIAN_POINT('',(17.5,16.5575380560557,38.9247727484987));
#76561=CARTESIAN_POINT('Origin',(17.5,14.6213611271723,40.1718595385976));
#76562=CARTESIAN_POINT('Origin',(17.5,0.,0.));
#76563=CARTESIAN_POINT('',(0.600000000000001,19.9986373454573,37.2739118462884));
#76564=CARTESIAN_POINT('Origin',(0.600000000000001,0.,0.));
#76565=CARTESIAN_POINT('',(1.67735469196905,19.1751255543105,37.7041716521717));
#76566=CARTESIAN_POINT('Origin',(8.14497546096349,0.,0.));
#76567=CARTESIAN_POINT('',(5.09593997529677,19.1751255543105,37.7041716521717));
#76568=CARTESIAN_POINT('',(17.5,19.1751255543105,37.7041716521717));
#76569=CARTESIAN_POINT('',(5.09944803334083,19.6490138787379,37.459394730737));
#76570=CARTESIAN_POINT('Origin',(-0.840551718690872,0.,0.));
#76571=CARTESIAN_POINT('',(10.8302042597752,19.9640920674886,37.2924258787336));
#76572=CARTESIAN_POINT('Origin',(-62.7155570771055,0.,0.));
#76573=CARTESIAN_POINT('',(11.6618634261911,19.7447778525305,37.4090062358548));
#76574=CARTESIAN_POINT('Origin',(26.9856656232739,0.,0.));
#76575=CARTESIAN_POINT('',(12.3548486633046,19.3958063601357,37.5911252244478));
#76576=CARTESIAN_POINT('Origin',(20.8267261185512,0.,0.));
#76577=CARTESIAN_POINT('',(13.103292255208,19.1751255543105,37.7041716521717));
#76578=CARTESIAN_POINT('Origin',(25.13830739299,0.,0.));
#76579=CARTESIAN_POINT('',(21.896707744792,19.1751255543105,37.7041716521717));
#76580=CARTESIAN_POINT('',(17.5,19.1751255543105,37.7041716521717));
#76581=CARTESIAN_POINT('',(22.6451513366954,19.3958063601357,37.5911252244478));
#76582=CARTESIAN_POINT('Origin',(9.86169260701005,0.,0.));
#76583=CARTESIAN_POINT('',(23.3381365738089,19.7447778525305,37.4090062358548));
#76584=CARTESIAN_POINT('Origin',(14.1732738814488,0.,0.));
#76585=CARTESIAN_POINT('',(24.1697957402248,19.9640920674886,37.2924258787336));
#76586=CARTESIAN_POINT('Origin',(8.01433437672609,0.,0.));
#76587=CARTESIAN_POINT('',(29.9005519666592,19.6490138787379,37.459394730737));
#76588=CARTESIAN_POINT('Origin',(97.7155570771053,0.,0.));
#76589=CARTESIAN_POINT('',(29.9040600247032,19.1751255543105,37.7041716521717));
#76590=CARTESIAN_POINT('Origin',(35.8405517186909,0.,0.));
#76591=CARTESIAN_POINT('',(17.5,19.1751255543105,37.7041716521717));
#76592=CARTESIAN_POINT('Origin',(33.1,17.5710580837557,33.7339653438087));
#76593=CARTESIAN_POINT('',(30.5247014514712,17.5045701882916,33.5694020278343));
#76594=CARTESIAN_POINT('Origin',(30.5,17.5710580837557,33.7339653438087));
#76595=CARTESIAN_POINT('',(30.4955273645547,18.0163441277467,33.5136270415661));
#76596=CARTESIAN_POINT('Origin',(30.5,18.0040707856479,33.4839653438087));
#76597=CARTESIAN_POINT('',(24.1012882089558,18.3802631128034,33.3579488669236));
#76598=CARTESIAN_POINT('Origin',(24.1,18.3504809471617,33.2839653438087));
#76599=CARTESIAN_POINT('',(23.1004586919557,18.0938594155378,33.4416219555226));
#76600=CARTESIAN_POINT('Origin',(23.1,18.0906733260263,33.4339653438087));
#76601=CARTESIAN_POINT('',(22.399682944576,17.742127215612,33.6288475295615));
#76602=CARTESIAN_POINT('Origin',(22.4,17.7442631645126,33.6339653438087));
#76603=CARTESIAN_POINT('',(21.7998387845652,17.5683840431675,33.7273468611033));
#76604=CARTESIAN_POINT('Origin',(21.8,17.5710580837557,33.7339653438087));
#76605=CARTESIAN_POINT('',(13.2021921742626,17.5346970308537,33.6439685797946));
#76606=CARTESIAN_POINT('Origin',(13.2,17.5710580837557,33.7339653438087));
#76607=CARTESIAN_POINT('',(12.6002487187375,17.7425875883397,33.6299506000067));
#76608=CARTESIAN_POINT('Origin',(12.6,17.7442631645126,33.6339653438087));
#76609=CARTESIAN_POINT('',(11.8996457869536,18.0931337015746,33.4398779649625));
#76610=CARTESIAN_POINT('Origin',(11.9,18.0906733260263,33.4339653438087));
#76611=CARTESIAN_POINT('',(10.899790263986,18.3553298442931,33.2960107570711));
#76612=CARTESIAN_POINT('Origin',(10.9,18.3504809471617,33.2839653438087));
#76613=CARTESIAN_POINT('',(4.55736144060343,18.1614760990067,33.864375894796));
#76614=CARTESIAN_POINT('Origin',(4.5,18.0040707856479,33.4839653438087));
#76615=CARTESIAN_POINT('',(4.49524972087093,17.5582719500126,33.7023185522751));
#76616=CARTESIAN_POINT('Origin',(4.5,17.5710580837557,33.7339653438087));
#76617=CARTESIAN_POINT('',(1.90350512467335,17.5458051084359,33.6714620365851));
#76618=CARTESIAN_POINT('Origin',(1.9,17.5710580837557,33.7339653438087));
#76619=CARTESIAN_POINT('Ctrl Pts',(0.138207714141623,20.505353736182,37.5246765162999));
#76620=CARTESIAN_POINT('Ctrl Pts',(0.370217470902976,20.2509844800803,37.3992864560044));
#76621=CARTESIAN_POINT('Ctrl Pts',(0.600000000000002,19.9986373454573,37.2739118462884));
#76622=CARTESIAN_POINT('Origin',(1.9,20.4289419162443,32.0839653438087));
#76623=CARTESIAN_POINT('',(5.09593997529677,23.0652077022745,35.4582316768749));
#76624=CARTESIAN_POINT('',(17.5,23.0652077022745,35.4582316768749));
#76625=CARTESIAN_POINT('',(4.47529854852883,20.3196698518115,31.9441034793054));
#76626=CARTESIAN_POINT('Origin',(4.5,20.4289419162443,32.0839653438087));
#76627=CARTESIAN_POINT('',(5.09944803334083,22.6162805078382,35.7462425436685));
#76628=CARTESIAN_POINT('Origin',(-0.840551718690874,0.,0.));
#76629=CARTESIAN_POINT('',(4.50447263544529,20.01548032708,32.3594252187343));
#76630=CARTESIAN_POINT('Origin',(4.5,19.9959292143521,32.3339653438087));
#76631=CARTESIAN_POINT('',(10.8302042597752,22.3141421459872,35.9356238333033));
#76632=CARTESIAN_POINT('Origin',(-62.7155570771054,0.,0.));
#76633=CARTESIAN_POINT('',(10.8987117910442,19.6986995804965,32.5967492173916));
#76634=CARTESIAN_POINT('Origin',(10.9,19.6495190528383,32.5339653438087));
#76635=CARTESIAN_POINT('',(11.6618634261911,22.5247608043155,35.8039823302991));
#76636=CARTESIAN_POINT('Origin',(26.9856656232739,0.,0.));
#76637=CARTESIAN_POINT('',(11.8995413080444,19.9143644494692,32.3905528841213));
#76638=CARTESIAN_POINT('Origin',(11.9,19.9093266739737,32.3839653438087));
#76639=CARTESIAN_POINT('',(12.3548486633046,22.856966221146,35.5928236469852));
#76640=CARTESIAN_POINT('Origin',(20.8267261185512,0.,0.));
#76641=CARTESIAN_POINT('',(12.600317055424,20.2523726527879,32.1795566506761));
#76642=CARTESIAN_POINT('Origin',(12.6,20.2557368354874,32.1839653438087));
#76643=CARTESIAN_POINT('',(13.103292255208,23.0652077022745,35.4582316768749));
#76644=CARTESIAN_POINT('Origin',(25.13830739299,0.,0.));
#76645=CARTESIAN_POINT('',(13.2001612154348,20.4245471623811,32.0783403153759));
#76646=CARTESIAN_POINT('Origin',(13.2,20.4289419162443,32.0839653438087));
#76647=CARTESIAN_POINT('',(21.896707744792,23.0652077022745,35.4582316768749));
#76648=CARTESIAN_POINT('',(17.5,23.0652077022745,35.4582316768749));
#76649=CARTESIAN_POINT('',(21.7978078257374,20.3691829588007,32.0074773662801));
#76650=CARTESIAN_POINT('Origin',(21.8,20.4289419162443,32.0839653438087));
#76651=CARTESIAN_POINT('',(22.6451513366954,22.856966221146,35.5928236469852));
#76652=CARTESIAN_POINT('Origin',(9.86169260701004,0.,0.));
#76653=CARTESIAN_POINT('',(22.3997512812625,20.2530977534517,32.180506880376));
#76654=CARTESIAN_POINT('Origin',(22.4,20.2557368354874,32.1839653438087));
#76655=CARTESIAN_POINT('',(23.3381365738089,22.5247608043155,35.8039823302992));
#76656=CARTESIAN_POINT('Origin',(14.1732738814488,0.,0.));
#76657=CARTESIAN_POINT('',(23.1003542130464,19.9132169663217,32.3890524021132));
#76658=CARTESIAN_POINT('Origin',(23.1,19.9093266739737,32.3839653438087));
#76659=CARTESIAN_POINT('',(24.1697957402248,22.3141421459872,35.9356238333033));
#76660=CARTESIAN_POINT('Origin',(8.01433437672608,0.,0.));
#76661=CARTESIAN_POINT('',(24.100209736014,19.657526238157,32.544187318536));
#76662=CARTESIAN_POINT('Origin',(24.1,19.6495190528383,32.5339653438087));
#76663=CARTESIAN_POINT('',(29.9005519666592,22.6162805078382,35.7462425436685));
#76664=CARTESIAN_POINT('Origin',(97.7155570771054,0.,0.));
#76665=CARTESIAN_POINT('',(30.4426385593966,20.2466717586954,32.6604876193617));
#76666=CARTESIAN_POINT('Origin',(30.5,19.9959292143521,32.3339653438087));
#76667=CARTESIAN_POINT('',(29.9040600247032,23.0652077022745,35.4582316768749));
#76668=CARTESIAN_POINT('Origin',(35.8405517186909,0.,0.));
#76669=CARTESIAN_POINT('',(30.5047502791291,20.4079280576996,32.0570688314042));
#76670=CARTESIAN_POINT('Origin',(30.5,20.4289419162443,32.0839653438087));
#76671=CARTESIAN_POINT('',(17.5,23.0652077022745,35.4582316768749));
#76672=CARTESIAN_POINT('Origin',(17.5,21.375,37.0225860117847));
#76673=CARTESIAN_POINT('Origin',(17.5,0.,0.));
#76674=CARTESIAN_POINT('',(0.600000000000001,26.1673599741116,33.234910440458));
#76675=CARTESIAN_POINT('Origin',(0.600000000000001,0.,0.));
#76676=CARTESIAN_POINT('',(1.67735469196904,25.4310730087083,33.8016349549212));
#76677=CARTESIAN_POINT('Origin',(8.14497546096349,0.,0.));
#76678=CARTESIAN_POINT('',(5.09593997529677,25.4310730087083,33.8016349549212));
#76679=CARTESIAN_POINT('',(17.5,25.4310730087083,33.8016349549212));
#76680=CARTESIAN_POINT('',(5.09944803334083,25.8552568383243,33.4782869009794));
#76681=CARTESIAN_POINT('Origin',(-0.840551718690872,0.,0.));
#76682=CARTESIAN_POINT('',(10.8302042597752,26.1365544445335,33.2591419277157));
#76683=CARTESIAN_POINT('Origin',(-62.7155570771055,0.,0.));
#76684=CARTESIAN_POINT('',(11.6618634261911,25.9408160718628,33.4120346810215));
#76685=CARTESIAN_POINT('Origin',(26.9856656232739,0.,0.));
#76686=CARTESIAN_POINT('',(12.3548486633046,25.6287708710599,33.6519851366708));
#76687=CARTESIAN_POINT('Origin',(20.8267261185512,0.,0.));
#76688=CARTESIAN_POINT('',(13.103292255208,25.4310730087083,33.8016349549212));
#76689=CARTESIAN_POINT('Origin',(25.13830739299,0.,0.));
#76690=CARTESIAN_POINT('',(21.896707744792,25.4310730087083,33.8016349549212));
#76691=CARTESIAN_POINT('',(17.5,25.4310730087083,33.8016349549212));
#76692=CARTESIAN_POINT('',(22.6451513366954,25.6287708710599,33.6519851366708));
#76693=CARTESIAN_POINT('Origin',(9.86169260701005,0.,0.));
#76694=CARTESIAN_POINT('',(23.3381365738089,25.9408160718628,33.4120346810215));
#76695=CARTESIAN_POINT('Origin',(14.1732738814488,0.,0.));
#76696=CARTESIAN_POINT('',(24.1697957402248,26.1365544445335,33.2591419277157));
#76697=CARTESIAN_POINT('Origin',(8.0143343767261,0.,0.));
#76698=CARTESIAN_POINT('',(29.9005519666592,25.8552568383243,33.4782869009794));
#76699=CARTESIAN_POINT('Origin',(97.7155570771055,0.,0.));
#76700=CARTESIAN_POINT('',(29.9040600247032,25.4310730087083,33.8016349549212));
#76701=CARTESIAN_POINT('Origin',(35.8405517186909,0.,0.));
#76702=CARTESIAN_POINT('',(17.5,25.4310730087083,33.8016349549212));
#76703=CARTESIAN_POINT('Origin',(33.1,23.1619558369422,30.170288394504));
#76704=CARTESIAN_POINT('',(30.5247014514712,23.0679019220779,30.0197706669552));
#76705=CARTESIAN_POINT('Origin',(30.5,23.1619558369422,30.170288394504));
#76706=CARTESIAN_POINT('',(30.4955273645547,23.562215640718,29.8759744160904));
#76707=CARTESIAN_POINT('Origin',(30.5,23.5449780585017,29.8488945896607));
#76708=CARTESIAN_POINT('',(24.1012882089558,23.893572647341,29.6594674741542));
#76709=CARTESIAN_POINT('Origin',(24.1,23.8513958357493,29.5917795457861));
#76710=CARTESIAN_POINT('',(23.1004586919557,23.6260497451375,29.7916028606322));
#76711=CARTESIAN_POINT('Origin',(23.1,23.6215825028136,29.784615828692));
#76712=CARTESIAN_POINT('',(22.399682944576,23.312172527411,30.0370617130518));
#76713=CARTESIAN_POINT('Origin',(22.4,23.315164725566,30.0417308725666));
#76714=CARTESIAN_POINT('',(21.7998387845652,23.1581731335784,30.1642348036977));
#76715=CARTESIAN_POINT('Origin',(21.8,23.1619558369422,30.170288394504));
#76716=CARTESIAN_POINT('',(13.2021921742626,23.1105194160696,30.0879729141313));
#76717=CARTESIAN_POINT('Origin',(13.2,23.1619558369422,30.170288394504));
#76718=CARTESIAN_POINT('',(12.6002487187375,23.3128174522151,30.038068082493));
#76719=CARTESIAN_POINT('Origin',(12.6,23.315164725566,30.0417308725666));
#76720=CARTESIAN_POINT('',(11.8996457869536,23.6250322156174,29.7900113841146));
#76721=CARTESIAN_POINT('Origin',(11.9,23.6215825028136,29.784615828692));
#76722=CARTESIAN_POINT('',(10.899790263986,23.8582627313001,29.6027999600046));
#76723=CARTESIAN_POINT('Origin',(10.9,23.8513958357493,29.5917795457861));
#76724=CARTESIAN_POINT('',(4.55736144060343,23.7660496304069,30.1961927037808));
#76725=CARTESIAN_POINT('Origin',(4.5,23.5449780585017,29.8488945896607));
#76726=CARTESIAN_POINT('',(4.49524972087093,23.1438685456221,30.1413426776677));
#76727=CARTESIAN_POINT('Origin',(4.5,23.1619558369422,30.170288394504));
#76728=CARTESIAN_POINT('',(1.90350512467335,23.1262329256631,30.1131197861062));
#76729=CARTESIAN_POINT('Origin',(1.9,23.1619558369422,30.170288394504));
#76730=CARTESIAN_POINT('Ctrl Pts',(0.138207714141625,26.7099230322463,33.3938750538235));
#76731=CARTESIAN_POINT('Ctrl Pts',(0.370217470894606,26.4376444612514,33.3145607080732));
#76732=CARTESIAN_POINT('Ctrl Pts',(0.600000000000002,26.1673599741116,33.234910440458));
#76733=CARTESIAN_POINT('Origin',(1.9,25.6899024992348,28.0490892825384));
#76734=CARTESIAN_POINT('',(5.09593997529677,28.872052684018,30.9143101784803));
#76735=CARTESIAN_POINT('',(17.5,28.872052684018,30.9143101784803));
#76736=CARTESIAN_POINT('',(4.47529854852883,25.5580037650976,27.9303271288835));
#76737=CARTESIAN_POINT('Origin',(4.5,25.6899024992348,28.0490892825384));
#76738=CARTESIAN_POINT('',(5.09944803334083,28.4799582645661,31.2759009022694));
#76739=CARTESIAN_POINT('Origin',(-0.840551718690874,0.,0.));
#76740=CARTESIAN_POINT('',(4.50447263544529,25.3305554259542,28.3921611545025));
#76741=CARTESIAN_POINT('Origin',(4.5,25.3068802776753,28.3704830873816));
#76742=CARTESIAN_POINT('',(10.8302042597752,28.2152957791621,31.5148708405159));
#76743=CARTESIAN_POINT('Origin',(-62.7155570771054,0.,0.));
#76744=CARTESIAN_POINT('',(10.8987117910442,25.0597981705973,28.6808880677203));
#76745=CARTESIAN_POINT('Origin',(10.9,25.0004625004277,28.6275981312563));
#76746=CARTESIAN_POINT('',(11.6618634261911,28.3998553597108,31.3486557215378));
#76747=CARTESIAN_POINT('Origin',(26.9856656232739,0.,0.));
#76748=CARTESIAN_POINT('',(11.8995413080444,25.2363809880999,28.4403745085892));
#76749=CARTESIAN_POINT('Origin',(11.9,25.2302758333634,28.4347618483503));
#76750=CARTESIAN_POINT('',(12.3548486633046,28.6903465092421,31.0830181478507));
#76751=CARTESIAN_POINT('Origin',(20.8267261185512,0.,0.));
#76752=CARTESIAN_POINT('',(12.600317055424,25.5326149758775,28.1738892734932));
#76753=CARTESIAN_POINT('Origin',(12.6,25.536693610611,28.1776468044757));
#76754=CARTESIAN_POINT('',(13.103292255208,28.872052684018,30.9143101784803));
#76755=CARTESIAN_POINT('Origin',(25.13830739299,0.,0.));
#76756=CARTESIAN_POINT('',(13.2001612154348,25.684597735621,28.0443128519265));
#76757=CARTESIAN_POINT('Origin',(13.2,25.6899024992348,28.0490892825384));
#76758=CARTESIAN_POINT('',(21.896707744792,28.872052684018,30.9143101784803));
#76759=CARTESIAN_POINT('',(17.5,28.872052684018,30.9143101784803));
#76760=CARTESIAN_POINT('',(21.7978078257374,25.6177694167211,27.9841403633154));
#76761=CARTESIAN_POINT('Origin',(21.8,25.6899024992348,28.0490892825384));
#76762=CARTESIAN_POINT('',(22.6451513366954,28.6903465092421,31.0830181478507));
#76763=CARTESIAN_POINT('Origin',(9.86169260701003,0.,0.));
#76764=CARTESIAN_POINT('',(22.3997512812625,25.5334940662887,28.1746991546599));
#76765=CARTESIAN_POINT('Origin',(22.4,25.536693610611,28.1776468044757));
#76766=CARTESIAN_POINT('',(23.3381365738089,28.3998553597108,31.3486557215378));
#76767=CARTESIAN_POINT('Origin',(14.1732738814488,0.,0.));
#76768=CARTESIAN_POINT('',(23.1003542130464,25.2349903818335,28.4390960806318));
#76769=CARTESIAN_POINT('Origin',(23.1,25.2302758333634,28.4347618483503));
#76770=CARTESIAN_POINT('',(24.1697957402248,28.2152957791621,31.5148708405159));
#76771=CARTESIAN_POINT('Origin',(8.01433437672607,0.,0.));
#76772=CARTESIAN_POINT('',(24.100209736014,25.0101230658929,28.63627437808));
#76773=CARTESIAN_POINT('Origin',(24.1,25.0004625004277,28.6275981312563));
#76774=CARTESIAN_POINT('',(29.9005519666592,28.4799582645661,31.2759009022694));
#76775=CARTESIAN_POINT('Origin',(97.7155570771054,0.,0.));
#76776=CARTESIAN_POINT('',(30.4426385593966,25.610513477472,28.6485037699886));
#76777=CARTESIAN_POINT('Origin',(30.5,25.3068802776753,28.3704830873816));
#76778=CARTESIAN_POINT('',(29.9040600247032,28.872052684018,30.9143101784803));
#76779=CARTESIAN_POINT('Origin',(35.8405517186909,0.,0.));
#76780=CARTESIAN_POINT('',(30.5047502791291,25.6645373580546,28.0262504068355));
#76781=CARTESIAN_POINT('Origin',(30.5,25.6899024992348,28.0490892825384));
#76782=CARTESIAN_POINT('',(17.5,28.872052684018,30.9143101784803));
#76783=CARTESIAN_POINT('Origin',(17.5,27.4791703140996,32.7483999433363));
#76784=CARTESIAN_POINT('Origin',(17.5,0.,0.));
#76785=CARTESIAN_POINT('',(0.600000000000001,31.5410006112756,28.1860830985703));
#76786=CARTESIAN_POINT('Origin',(0.600000000000001,0.,0.));
#76787=CARTESIAN_POINT('',(1.67735469196904,30.9143101784803,28.872052684018));
#76788=CARTESIAN_POINT('Origin',(8.14497546096349,0.,0.));
#76789=CARTESIAN_POINT('',(5.09593997529677,30.9143101784803,28.872052684018));
#76790=CARTESIAN_POINT('',(17.5,30.9143101784803,28.872052684018));
#76791=CARTESIAN_POINT('',(5.09944803334083,31.2759009022694,28.4799582645661));
#76792=CARTESIAN_POINT('Origin',(-0.840551718690872,0.,0.));
#76793=CARTESIAN_POINT('',(10.8302042597752,31.5148708405159,28.2152957791621));
#76794=CARTESIAN_POINT('Origin',(-62.7155570771055,0.,0.));
#76795=CARTESIAN_POINT('',(11.6618634261911,31.3486557215378,28.3998553597108));
#76796=CARTESIAN_POINT('Origin',(26.9856656232739,0.,0.));
#76797=CARTESIAN_POINT('',(12.3548486633046,31.0830181478507,28.6903465092421));
#76798=CARTESIAN_POINT('Origin',(20.8267261185512,0.,0.));
#76799=CARTESIAN_POINT('',(13.103292255208,30.9143101784803,28.872052684018));
#76800=CARTESIAN_POINT('Origin',(25.13830739299,0.,0.));
#76801=CARTESIAN_POINT('',(21.896707744792,30.9143101784803,28.872052684018));
#76802=CARTESIAN_POINT('',(17.5,30.9143101784803,28.872052684018));
#76803=CARTESIAN_POINT('',(22.6451513366954,31.0830181478507,28.6903465092421));
#76804=CARTESIAN_POINT('Origin',(9.86169260701006,0.,0.));
#76805=CARTESIAN_POINT('',(23.3381365738089,31.3486557215378,28.3998553597108));
#76806=CARTESIAN_POINT('Origin',(14.1732738814488,0.,0.));
#76807=CARTESIAN_POINT('',(24.1697957402248,31.5148708405159,28.2152957791621));
#76808=CARTESIAN_POINT('Origin',(8.01433437672608,0.,0.));
#76809=CARTESIAN_POINT('',(29.9005519666592,31.2759009022694,28.4799582645661));
#76810=CARTESIAN_POINT('Origin',(97.7155570771054,0.,0.));
#76811=CARTESIAN_POINT('',(29.9040600247032,30.9143101784803,28.872052684018));
#76812=CARTESIAN_POINT('Origin',(35.8405517186909,0.,0.));
#76813=CARTESIAN_POINT('',(17.5,30.9143101784803,28.872052684018));
#76814=CARTESIAN_POINT('Origin',(33.1,28.0490892825384,25.6899024992348));
#76815=CARTESIAN_POINT('',(30.5247014514712,27.9303271288835,25.5580037650976));
#76816=CARTESIAN_POINT('Origin',(30.5,28.0490892825384,25.6899024992348));
#76817=CARTESIAN_POINT('',(30.4955273645547,28.3921611545025,25.3305554259542));
#76818=CARTESIAN_POINT('Origin',(30.5,28.3704830873816,25.3068802776753));
#76819=CARTESIAN_POINT('',(24.1012882089558,28.6808880677203,25.0597981705973));
#76820=CARTESIAN_POINT('Origin',(24.1,28.6275981312563,25.0004625004277));
#76821=CARTESIAN_POINT('',(23.1004586919557,28.4403745085892,25.2363809880999));
#76822=CARTESIAN_POINT('Origin',(23.1,28.4347618483503,25.2302758333634));
#76823=CARTESIAN_POINT('',(22.399682944576,28.1738892734932,25.5326149758775));
#76824=CARTESIAN_POINT('Origin',(22.4,28.1776468044757,25.536693610611));
#76825=CARTESIAN_POINT('',(21.7998387845652,28.0443128519265,25.684597735621));
#76826=CARTESIAN_POINT('Origin',(21.8,28.0490892825384,25.6899024992348));
#76827=CARTESIAN_POINT('',(13.2021921742626,27.9841403633154,25.6177694167211));
#76828=CARTESIAN_POINT('Origin',(13.2,28.0490892825384,25.6899024992348));
#76829=CARTESIAN_POINT('',(12.6002487187375,28.1746991546599,25.5334940662887));
#76830=CARTESIAN_POINT('Origin',(12.6,28.1776468044757,25.536693610611));
#76831=CARTESIAN_POINT('',(11.8996457869536,28.4390960806318,25.2349903818335));
#76832=CARTESIAN_POINT('Origin',(11.9,28.4347618483503,25.2302758333634));
#76833=CARTESIAN_POINT('',(10.899790263986,28.63627437808,25.0101230658929));
#76834=CARTESIAN_POINT('Origin',(10.9,28.6275981312563,25.0004625004277));
#76835=CARTESIAN_POINT('',(4.55736144060343,28.6485037699886,25.610513477472));
#76836=CARTESIAN_POINT('Origin',(4.5,28.3704830873816,25.3068802776753));
#76837=CARTESIAN_POINT('',(4.49524972087093,28.0262504068355,25.6645373580546));
#76838=CARTESIAN_POINT('Origin',(4.5,28.0490892825384,25.6899024992348));
#76839=CARTESIAN_POINT('',(1.90350512467335,28.0039818578826,25.6398056289004));
#76840=CARTESIAN_POINT('Origin',(1.9,28.0490892825384,25.6899024992348));
#76841=CARTESIAN_POINT('Ctrl Pts',(0.138207714141624,32.1029248328492,28.2484175959527));
#76842=CARTESIAN_POINT('Ctrl Pts',(0.370217470898456,31.8210099935472,28.2175888910033));
#76843=CARTESIAN_POINT('Ctrl Pts',(0.600000000000002,31.5410006112756,28.1860830985703));
#76844=CARTESIAN_POINT('Origin',(1.9,30.170288394504,23.1619558369422));
#76845=CARTESIAN_POINT('',(5.09593997529677,33.8016349549212,25.4310730087083));
#76846=CARTESIAN_POINT('',(17.5,33.8016349549212,25.4310730087083));
#76847=CARTESIAN_POINT('',(4.47529854852883,30.0197706669552,23.0679019220779));
#76848=CARTESIAN_POINT('Origin',(4.5,30.170288394504,23.1619558369422));
#76849=CARTESIAN_POINT('',(5.09944803334083,33.4782869009794,25.8552568383243));
#76850=CARTESIAN_POINT('Origin',(-0.840551718690874,0.,0.));
#76851=CARTESIAN_POINT('',(4.50447263544529,29.8759744160904,23.562215640718));
#76852=CARTESIAN_POINT('Origin',(4.5,29.8488945896607,23.5449780585017));
#76853=CARTESIAN_POINT('',(10.8302042597752,33.2591419277157,26.1365544445334));
#76854=CARTESIAN_POINT('Origin',(-62.7155570771055,0.,0.));
#76855=CARTESIAN_POINT('',(10.8987117910442,29.6594674741542,23.893572647341));
#76856=CARTESIAN_POINT('Origin',(10.9,29.5917795457861,23.8513958357493));
#76857=CARTESIAN_POINT('',(11.6618634261911,33.4120346810215,25.9408160718628));
#76858=CARTESIAN_POINT('Origin',(26.9856656232739,0.,0.));
#76859=CARTESIAN_POINT('',(11.8995413080444,29.7916028606322,23.6260497451375));
#76860=CARTESIAN_POINT('Origin',(11.9,29.784615828692,23.6215825028136));
#76861=CARTESIAN_POINT('',(12.3548486633046,33.6519851366708,25.6287708710599));
#76862=CARTESIAN_POINT('Origin',(20.8267261185512,0.,0.));
#76863=CARTESIAN_POINT('',(12.600317055424,30.0370617130518,23.312172527411));
#76864=CARTESIAN_POINT('Origin',(12.6,30.0417308725667,23.315164725566));
#76865=CARTESIAN_POINT('',(13.103292255208,33.8016349549212,25.4310730087083));
#76866=CARTESIAN_POINT('Origin',(25.13830739299,0.,0.));
#76867=CARTESIAN_POINT('',(13.2001612154348,30.1642348036977,23.1581731335784));
#76868=CARTESIAN_POINT('Origin',(13.2,30.170288394504,23.1619558369422));
#76869=CARTESIAN_POINT('',(21.896707744792,33.8016349549212,25.4310730087083));
#76870=CARTESIAN_POINT('',(17.5,33.8016349549212,25.4310730087083));
#76871=CARTESIAN_POINT('',(21.7978078257374,30.0879729141313,23.1105194160696));
#76872=CARTESIAN_POINT('Origin',(21.8,30.170288394504,23.1619558369422));
#76873=CARTESIAN_POINT('',(22.6451513366954,33.6519851366708,25.6287708710599));
#76874=CARTESIAN_POINT('Origin',(9.86169260701005,0.,0.));
#76875=CARTESIAN_POINT('',(22.3997512812625,30.0380680824931,23.3128174522151));
#76876=CARTESIAN_POINT('Origin',(22.4,30.0417308725667,23.315164725566));
#76877=CARTESIAN_POINT('',(23.3381365738089,33.4120346810215,25.9408160718628));
#76878=CARTESIAN_POINT('Origin',(14.1732738814488,0.,0.));
#76879=CARTESIAN_POINT('',(23.1003542130464,29.7900113841146,23.6250322156174));
#76880=CARTESIAN_POINT('Origin',(23.1,29.784615828692,23.6215825028136));
#76881=CARTESIAN_POINT('',(24.1697957402248,33.2591419277157,26.1365544445335));
#76882=CARTESIAN_POINT('Origin',(8.01433437672607,0.,0.));
#76883=CARTESIAN_POINT('',(24.100209736014,29.6027999600046,23.8582627313001));
#76884=CARTESIAN_POINT('Origin',(24.1,29.5917795457861,23.8513958357493));
#76885=CARTESIAN_POINT('',(29.9005519666592,33.4782869009794,25.8552568383243));
#76886=CARTESIAN_POINT('Origin',(97.7155570771054,0.,0.));
#76887=CARTESIAN_POINT('',(30.4426385593966,30.1961927037808,23.7660496304069));
#76888=CARTESIAN_POINT('Origin',(30.5,29.8488945896607,23.5449780585017));
#76889=CARTESIAN_POINT('',(29.9040600247032,33.8016349549212,25.4310730087083));
#76890=CARTESIAN_POINT('Origin',(35.8405517186909,0.,0.));
#76891=CARTESIAN_POINT('',(30.5047502791291,30.1413426776677,23.1438685456221));
#76892=CARTESIAN_POINT('Origin',(30.5,30.170288394504,23.1619558369422));
#76893=CARTESIAN_POINT('',(17.5,33.8016349549212,25.4310730087083));
#76894=CARTESIAN_POINT('Origin',(17.5,32.7483999433363,27.4791703140996));
#76895=CARTESIAN_POINT('Origin',(17.5,0.,0.));
#76896=CARTESIAN_POINT('',(0.600000000000001,35.9562839053824,22.2808358845789));
#76897=CARTESIAN_POINT('Origin',(0.600000000000001,0.,0.));
#76898=CARTESIAN_POINT('',(1.67735469196904,35.4582316768749,23.0652077022745));
#76899=CARTESIAN_POINT('Origin',(8.14497546096349,0.,0.));
#76900=CARTESIAN_POINT('',(5.09593997529677,35.4582316768749,23.0652077022745));
#76901=CARTESIAN_POINT('',(17.5,35.4582316768749,23.0652077022745));
#76902=CARTESIAN_POINT('',(5.09944803334083,35.7462425436685,22.6162805078382));
#76903=CARTESIAN_POINT('Origin',(-0.840551718690872,0.,0.));
#76904=CARTESIAN_POINT('',(10.8302042597752,35.9356238333033,22.3141421459872));
#76905=CARTESIAN_POINT('Origin',(-62.7155570771055,0.,0.));
#76906=CARTESIAN_POINT('',(11.6618634261911,35.8039823302991,22.5247608043155));
#76907=CARTESIAN_POINT('Origin',(26.9856656232739,0.,0.));
#76908=CARTESIAN_POINT('',(12.3548486633046,35.5928236469852,22.856966221146));
#76909=CARTESIAN_POINT('Origin',(20.8267261185512,0.,0.));
#76910=CARTESIAN_POINT('',(13.103292255208,35.4582316768749,23.0652077022745));
#76911=CARTESIAN_POINT('Origin',(25.13830739299,0.,0.));
#76912=CARTESIAN_POINT('',(21.896707744792,35.4582316768749,23.0652077022745));
#76913=CARTESIAN_POINT('',(17.5,35.4582316768749,23.0652077022745));
#76914=CARTESIAN_POINT('',(22.6451513366954,35.5928236469852,22.856966221146));
#76915=CARTESIAN_POINT('Origin',(9.86169260701005,0.,0.));
#76916=CARTESIAN_POINT('',(23.3381365738089,35.8039823302992,22.5247608043155));
#76917=CARTESIAN_POINT('Origin',(14.1732738814488,0.,0.));
#76918=CARTESIAN_POINT('',(24.1697957402248,35.9356238333033,22.3141421459872));
#76919=CARTESIAN_POINT('Origin',(8.01433437672608,0.,0.));
#76920=CARTESIAN_POINT('',(29.9005519666592,35.7462425436685,22.6162805078382));
#76921=CARTESIAN_POINT('Origin',(97.7155570771054,0.,0.));
#76922=CARTESIAN_POINT('',(29.9040600247032,35.4582316768749,23.0652077022745));
#76923=CARTESIAN_POINT('Origin',(35.8405517186909,0.,0.));
#76924=CARTESIAN_POINT('',(17.5,35.4582316768749,23.0652077022745));
#76925=CARTESIAN_POINT('Origin',(33.1,32.0839653438087,20.4289419162443));
#76926=CARTESIAN_POINT('',(30.5247014514712,31.9441034793054,20.3196698518115));
#76927=CARTESIAN_POINT('Origin',(30.5,32.0839653438087,20.4289419162443));
#76928=CARTESIAN_POINT('',(30.4955273645547,32.3594252187343,20.01548032708));
#76929=CARTESIAN_POINT('Origin',(30.5,32.3339653438087,19.9959292143521));
#76930=CARTESIAN_POINT('',(24.1012882089558,32.5967492173916,19.6986995804965));
#76931=CARTESIAN_POINT('Origin',(24.1,32.5339653438087,19.6495190528383));
#76932=CARTESIAN_POINT('',(23.1004586919557,32.3905528841213,19.9143644494691));
#76933=CARTESIAN_POINT('Origin',(23.1,32.3839653438087,19.9093266739737));
#76934=CARTESIAN_POINT('',(22.399682944576,32.1795566506761,20.2523726527878));
#76935=CARTESIAN_POINT('Origin',(22.4,32.1839653438087,20.2557368354874));
#76936=CARTESIAN_POINT('',(21.7998387845652,32.0783403153759,20.4245471623811));
#76937=CARTESIAN_POINT('Origin',(21.8,32.0839653438087,20.4289419162443));
#76938=CARTESIAN_POINT('',(13.2021921742626,32.0074773662801,20.3691829588007));
#76939=CARTESIAN_POINT('Origin',(13.2,32.0839653438087,20.4289419162443));
#76940=CARTESIAN_POINT('',(12.6002487187375,32.180506880376,20.2530977534517));
#76941=CARTESIAN_POINT('Origin',(12.6,32.1839653438087,20.2557368354874));
#76942=CARTESIAN_POINT('',(11.8996457869536,32.3890524021132,19.9132169663217));
#76943=CARTESIAN_POINT('Origin',(11.9,32.3839653438087,19.9093266739737));
#76944=CARTESIAN_POINT('',(10.899790263986,32.544187318536,19.6575262381569));
#76945=CARTESIAN_POINT('Origin',(10.9,32.5339653438087,19.6495190528383));
#76946=CARTESIAN_POINT('',(4.55736144060343,32.6604876193617,20.2466717586953));
#76947=CARTESIAN_POINT('Origin',(4.5,32.3339653438087,19.9959292143521));
#76948=CARTESIAN_POINT('',(4.49524972087093,32.0570688314042,20.4079280576996));
#76949=CARTESIAN_POINT('Origin',(4.5,32.0839653438087,20.4289419162443));
#76950=CARTESIAN_POINT('',(1.90350512467335,32.0308439720488,20.387438952028));
#76951=CARTESIAN_POINT('Origin',(1.9,32.0839653438087,20.4289419162443));
#76952=CARTESIAN_POINT('Ctrl Pts',(0.138207714141628,36.5204955072696,22.2446462638181));
#76953=CARTESIAN_POINT('Ctrl Pts',(0.370217470898585,36.2375102394015,22.2632399142706));
#76954=CARTESIAN_POINT('Ctrl Pts',(0.600000000000001,35.9562839053824,22.2808358845789));
#76955=CARTESIAN_POINT('Origin',(1.9,33.7339653438087,17.5710580837557));
#76956=CARTESIAN_POINT('',(5.09593997529677,37.7041716521717,19.1751255543105));
#76957=CARTESIAN_POINT('',(17.5,37.7041716521717,19.1751255543105));
#76958=CARTESIAN_POINT('',(4.47529854852883,33.5694020278343,17.5045701882916));
#76959=CARTESIAN_POINT('Origin',(4.5,33.7339653438087,17.5710580837557));
#76960=CARTESIAN_POINT('',(5.09944803334083,37.459394730737,19.6490138787379));
#76961=CARTESIAN_POINT('Origin',(-0.840551718690874,0.,0.));
#76962=CARTESIAN_POINT('',(4.50447263544529,33.5136270415661,18.0163441277467));
#76963=CARTESIAN_POINT('Origin',(4.5,33.4839653438087,18.0040707856479));
#76964=CARTESIAN_POINT('',(10.8302042597752,37.2924258787336,19.9640920674886));
#76965=CARTESIAN_POINT('Origin',(-62.7155570771054,0.,0.));
#76966=CARTESIAN_POINT('',(10.8987117910442,33.3579488669236,18.3802631128033));
#76967=CARTESIAN_POINT('Origin',(10.9,33.2839653438087,18.3504809471617));
#76968=CARTESIAN_POINT('',(11.6618634261911,37.4090062358548,19.7447778525305));
#76969=CARTESIAN_POINT('Origin',(26.9856656232739,0.,0.));
#76970=CARTESIAN_POINT('',(11.8995413080444,33.4416219555226,18.0938594155378));
#76971=CARTESIAN_POINT('Origin',(11.9,33.4339653438087,18.0906733260263));
#76972=CARTESIAN_POINT('',(12.3548486633046,37.5911252244478,19.3958063601357));
#76973=CARTESIAN_POINT('Origin',(20.8267261185512,0.,0.));
#76974=CARTESIAN_POINT('',(12.600317055424,33.6288475295615,17.742127215612));
#76975=CARTESIAN_POINT('Origin',(12.6,33.6339653438087,17.7442631645126));
#76976=CARTESIAN_POINT('',(13.103292255208,37.7041716521717,19.1751255543105));
#76977=CARTESIAN_POINT('Origin',(25.13830739299,0.,0.));
#76978=CARTESIAN_POINT('',(13.2001612154348,33.7273468611033,17.5683840431675));
#76979=CARTESIAN_POINT('Origin',(13.2,33.7339653438087,17.5710580837557));
#76980=CARTESIAN_POINT('',(21.896707744792,37.7041716521717,19.1751255543105));
#76981=CARTESIAN_POINT('',(17.5,37.7041716521717,19.1751255543105));
#76982=CARTESIAN_POINT('',(21.7978078257374,33.6439685797946,17.5346970308537));
#76983=CARTESIAN_POINT('Origin',(21.8,33.7339653438087,17.5710580837557));
#76984=CARTESIAN_POINT('',(22.6451513366954,37.5911252244478,19.3958063601357));
#76985=CARTESIAN_POINT('Origin',(9.86169260701005,0.,0.));
#76986=CARTESIAN_POINT('',(22.3997512812625,33.6299506000067,17.7425875883397));
#76987=CARTESIAN_POINT('Origin',(22.4,33.6339653438087,17.7442631645126));
#76988=CARTESIAN_POINT('',(23.3381365738089,37.4090062358548,19.7447778525305));
#76989=CARTESIAN_POINT('Origin',(14.1732738814488,0.,0.));
#76990=CARTESIAN_POINT('',(23.1003542130464,33.4398779649625,18.0931337015746));
#76991=CARTESIAN_POINT('Origin',(23.1,33.4339653438087,18.0906733260263));
#76992=CARTESIAN_POINT('',(24.1697957402248,37.2924258787336,19.9640920674886));
#76993=CARTESIAN_POINT('Origin',(8.01433437672608,0.,0.));
#76994=CARTESIAN_POINT('',(24.100209736014,33.2960107570711,18.3553298442931));
#76995=CARTESIAN_POINT('Origin',(24.1,33.2839653438087,18.3504809471617));
#76996=CARTESIAN_POINT('',(29.9005519666592,37.459394730737,19.6490138787379));
#76997=CARTESIAN_POINT('Origin',(97.7155570771054,0.,0.));
#76998=CARTESIAN_POINT('',(30.4426385593966,33.864375894796,18.1614760990067));
#76999=CARTESIAN_POINT('Origin',(30.5,33.4839653438087,18.0040707856479));
#77000=CARTESIAN_POINT('',(29.9040600247032,37.7041716521717,19.1751255543105));
#77001=CARTESIAN_POINT('Origin',(35.8405517186909,0.,0.));
#77002=CARTESIAN_POINT('',(30.5047502791291,33.7023185522751,17.5582719500126));
#77003=CARTESIAN_POINT('Origin',(30.5,33.7339653438087,17.5710580837557));
#77004=CARTESIAN_POINT('',(17.5,37.7041716521717,19.1751255543105));
#77005=CARTESIAN_POINT('Origin',(17.5,37.0225860117848,21.375));
#77006=CARTESIAN_POINT('Origin',(17.5,0.,0.));
#77007=CARTESIAN_POINT('',(0.600000000000001,39.2790537077817,15.6985967468815));
#77008=CARTESIAN_POINT('Origin',(0.600000000000001,0.,0.));
#77009=CARTESIAN_POINT('',(1.67735469196904,38.9247727484987,16.5575380560557));
#77010=CARTESIAN_POINT('Origin',(8.14497546096349,0.,0.));
#77011=CARTESIAN_POINT('',(5.09593997529677,38.9247727484987,16.5575380560557));
#77012=CARTESIAN_POINT('',(17.5,38.9247727484987,16.5575380560557));
#77013=CARTESIAN_POINT('',(5.09944803334083,39.1304526938498,16.0654185122698));
#77014=CARTESIAN_POINT('Origin',(-0.840551718690872,0.,0.));
#77015=CARTESIAN_POINT('',(10.8302042597752,39.2644910802189,15.7349845952072));
#77016=CARTESIAN_POINT('Origin',(-62.7155570771055,0.,0.));
#77017=CARTESIAN_POINT('',(11.6618634261911,39.1714230536436,15.9652627899599));
#77018=CARTESIAN_POINT('Origin',(26.9856656232739,0.,0.));
#77019=CARTESIAN_POINT('',(12.3548486633046,39.0211592104439,16.3290885806033));
#77020=CARTESIAN_POINT('Origin',(20.8267261185512,0.,0.));
#77021=CARTESIAN_POINT('',(13.103292255208,38.9247727484987,16.5575380560557));
#77022=CARTESIAN_POINT('Origin',(25.13830739299,0.,0.));
#77023=CARTESIAN_POINT('',(21.896707744792,38.9247727484987,16.5575380560557));
#77024=CARTESIAN_POINT('',(17.5,38.9247727484987,16.5575380560557));
#77025=CARTESIAN_POINT('',(22.6451513366954,39.0211592104439,16.3290885806033));
#77026=CARTESIAN_POINT('Origin',(9.86169260701006,0.,0.));
#77027=CARTESIAN_POINT('',(23.3381365738089,39.1714230536436,15.9652627899599));
#77028=CARTESIAN_POINT('Origin',(14.1732738814488,0.,0.));
#77029=CARTESIAN_POINT('',(24.1697957402248,39.2644910802189,15.7349845952072));
#77030=CARTESIAN_POINT('Origin',(8.01433437672609,0.,0.));
#77031=CARTESIAN_POINT('',(29.9005519666592,39.1304526938498,16.0654185122698));
#77032=CARTESIAN_POINT('Origin',(97.7155570771054,0.,0.));
#77033=CARTESIAN_POINT('',(29.9040600247032,38.9247727484987,16.5575380560557));
#77034=CARTESIAN_POINT('Origin',(35.8405517186909,0.,0.));
#77035=CARTESIAN_POINT('',(17.5,38.9247727484987,16.5575380560557));
#77036=CARTESIAN_POINT('Origin',(33.1,35.1439863533772,14.5472582706722));
#77037=CARTESIAN_POINT('',(30.5247014514712,34.987274410005,14.4639330523272));
#77038=CARTESIAN_POINT('Origin',(30.5,35.1439863533772,14.5472582706722));
#77039=CARTESIAN_POINT('',(30.4955273645547,35.343464522354,14.0922449867892));
#77040=CARTESIAN_POINT('Origin',(30.5,35.31499642504,14.0774119602792));
#77041=CARTESIAN_POINT('',(24.1012882089558,35.5221746368434,13.7390659716653));
#77042=CARTESIAN_POINT('Origin',(24.1,35.4518044823703,13.7015349119648));
#77043=CARTESIAN_POINT('',(23.1004586919557,35.35656070068,13.9872600241959));
#77044=CARTESIAN_POINT('Origin',(23.1,35.3491984393726,13.9834426982006));
#77045=CARTESIAN_POINT('',(22.399682944576,35.2074644826695,14.3567722348382));
#77046=CARTESIAN_POINT('Origin',(22.4,35.2123903820423,14.359319746515));
#77047=CARTESIAN_POINT('',(21.7998387845652,35.137683640766,14.5439070589317));
#77048=CARTESIAN_POINT('Origin',(21.8,35.1439863533772,14.5472582706722));
#77049=CARTESIAN_POINT('',(13.2021921742626,35.0582833660355,14.501689183981));
#77050=CARTESIAN_POINT('Origin',(13.2,35.1439863533772,14.5472582706722));
#77051=CARTESIAN_POINT('',(12.6002487187375,35.208526188654,14.3573213139379));
#77052=CARTESIAN_POINT('Origin',(12.6,35.2123903820423,14.359319746515));
#77053=CARTESIAN_POINT('',(11.8996457869536,35.3548837560077,13.9863905298622));
#77054=CARTESIAN_POINT('Origin',(11.9,35.3491984393726,13.9834426982006));
#77055=CARTESIAN_POINT('',(10.899790263986,35.4632615954717,13.7076454228629));
#77056=CARTESIAN_POINT('Origin',(10.9,35.4518044823703,13.7015349119648));
#77057=CARTESIAN_POINT('',(4.55736144060343,35.6800990794245,14.267645163841));
#77058=CARTESIAN_POINT('Origin',(4.5,35.31499642504,14.0774119602792));
#77059=CARTESIAN_POINT('',(4.49524972087093,35.1138494411902,14.5312341902212));
#77060=CARTESIAN_POINT('Origin',(4.5,35.1439863533772,14.5472582706722));
#77061=CARTESIAN_POINT('',(1.90350512467335,35.0844651005135,14.5156102591402));
#77062=CARTESIAN_POINT('Origin',(1.9,35.1439863533772,14.5472582706722));
#77063=CARTESIAN_POINT('Ctrl Pts',(0.138207714141622,39.8284094059642,15.5649826112914));
#77064=CARTESIAN_POINT('Ctrl Pts',(0.37021747089279,39.5529520737035,15.6324336584841));
#77065=CARTESIAN_POINT('Ctrl Pts',(0.600000000000001,39.2790537077817,15.6985967468815));
#77066=CARTESIAN_POINT('Origin',(1.9,36.2726528263519,11.4462726220787));
#77067=CARTESIAN_POINT('',(5.09593997529677,40.4610861730024,12.3365516130268));
#77068=CARTESIAN_POINT('',(17.5,40.4610861730024,12.3365516130268));
#77069=CARTESIAN_POINT('',(4.47529854852883,36.0990440950346,11.409370947074));
#77070=CARTESIAN_POINT('Origin',(4.5,36.2726528263519,11.4462726220787));
#77071=CARTESIAN_POINT('',(5.09944803334083,40.3023178069695,12.8457455753269));
#77072=CARTESIAN_POINT('Origin',(-0.840551718690874,0.,0.));
#77073=CARTESIAN_POINT('',(4.50447263544529,36.1329850680974,11.9230551151638));
#77074=CARTESIAN_POINT('Origin',(4.5,36.101642754689,11.9161189324716));
#77075=CARTESIAN_POINT('',(10.8302042597752,40.1925983403042,13.1850308552911));
#77076=CARTESIAN_POINT('Origin',(-62.7155570771055,0.,0.));
#77077=CARTESIAN_POINT('',(10.8987117910442,36.0428658633082,12.3084785844451));
#77078=CARTESIAN_POINT('Origin',(10.9,35.9648346973588,12.291995980786));
#77079=CARTESIAN_POINT('',(11.6618634261911,40.2693240660821,12.9488045494888));
#77080=CARTESIAN_POINT('Origin',(26.9856656232739,0.,0.));
#77081=CARTESIAN_POINT('',(11.8995413080444,36.0755342895717,12.0118963235316));
#77082=CARTESIAN_POINT('Origin',(11.9,36.0674407403565,12.0100881945502));
#77083=CARTESIAN_POINT('',(12.3548486633046,40.3880779943072,12.5735100877104));
#77084=CARTESIAN_POINT('Origin',(20.8267261185512,0.,0.));
#77085=CARTESIAN_POINT('',(12.600317055424,36.1988378309035,11.6329963463162));
#77086=CARTESIAN_POINT('Origin',(12.6,36.2042487976867,11.6342111462358));
#77087=CARTESIAN_POINT('',(13.103292255208,40.4610861730024,12.3365516130268));
#77088=CARTESIAN_POINT('Origin',(25.13830739299,0.,0.));
#77089=CARTESIAN_POINT('',(13.2001612154348,36.2656705509953,11.4447884936362));
#77090=CARTESIAN_POINT('Origin',(13.2,36.2726528263519,11.4462726220787));
#77091=CARTESIAN_POINT('',(21.896707744792,40.4610861730024,12.3365516130268));
#77092=CARTESIAN_POINT('',(17.5,40.4610861730024,12.3365516130268));
#77093=CARTESIAN_POINT('',(21.7978078257374,36.1777092848303,11.4260917493401));
#77094=CARTESIAN_POINT('Origin',(21.8,36.2726528263519,11.4462726220787));
#77095=CARTESIAN_POINT('',(22.6451513366954,40.3880779943072,12.5735100877104));
#77096=CARTESIAN_POINT('Origin',(9.86169260701004,0.,0.));
#77097=CARTESIAN_POINT('',(22.3997512812625,36.2000040861152,11.633258178775));
#77098=CARTESIAN_POINT('Origin',(22.4,36.2042487976867,11.6342111462358));
#77099=CARTESIAN_POINT('',(23.3381365738089,40.2693240660821,12.9488045494888));
#77100=CARTESIAN_POINT('Origin',(14.1732738814488,0.,0.));
#77101=CARTESIAN_POINT('',(23.1003542130464,36.0736907752397,12.0114844755768));
#77102=CARTESIAN_POINT('Origin',(23.1,36.0674407403565,12.0100881945502));
#77103=CARTESIAN_POINT('',(24.1697957402248,40.1925983403042,13.1850308552911));
#77104=CARTESIAN_POINT('Origin',(8.01433437672608,0.,0.));
#77105=CARTESIAN_POINT('',(24.100209736014,35.9775391158784,12.2946795482123));
#77106=CARTESIAN_POINT('Origin',(24.1,35.9648346973588,12.291995980786));
#77107=CARTESIAN_POINT('',(29.9005519666592,40.3023178069695,12.8457455753269));
#77108=CARTESIAN_POINT('Origin',(97.7155570771054,0.,0.));
#77109=CARTESIAN_POINT('',(30.4426385593966,36.5036071604488,12.0050753064884));
#77110=CARTESIAN_POINT('Origin',(30.5,36.101642754689,11.9161189324716));
#77111=CARTESIAN_POINT('',(29.9040600247032,40.4610861730024,12.3365516130268));
#77112=CARTESIAN_POINT('Origin',(35.8405517186909,0.,0.));
#77113=CARTESIAN_POINT('',(30.5047502791291,36.2392665318678,11.4391761461162));
#77114=CARTESIAN_POINT('Origin',(30.5,36.2726528263519,11.4462726220787));
#77115=CARTESIAN_POINT('',(17.5,40.4610861730024,12.3365516130268));
#77116=CARTESIAN_POINT('Origin',(17.5,40.1718595385976,14.6213611271723));
#77117=CARTESIAN_POINT('Origin',(17.5,0.,0.));
#77118=CARTESIAN_POINT('',(0.600000000000001,41.4083493394303,8.63936369090332));
#77119=CARTESIAN_POINT('Origin',(0.600000000000001,0.,0.));
#77120=CARTESIAN_POINT('',(1.67735469196904,41.2086042970448,9.54677599452213));
#77121=CARTESIAN_POINT('Origin',(8.14497546096349,0.,0.));
#77122=CARTESIAN_POINT('',(5.09593997529677,41.2086042970448,9.54677599452213));
#77123=CARTESIAN_POINT('',(17.5,41.2086042970448,9.54677599452213));
#77124=CARTESIAN_POINT('',(5.09944803334083,41.325703839893,9.02641690470011));
#77125=CARTESIAN_POINT('Origin',(-0.840551718690872,0.,0.));
#77126=CARTESIAN_POINT('',(10.8302042597752,41.4003266344532,8.6777274997883));
#77127=CARTESIAN_POINT('Origin',(-62.7155570771055,0.,0.));
#77128=CARTESIAN_POINT('',(11.6618634261911,41.3486599091995,8.92066834454426));
#77129=CARTESIAN_POINT('Origin',(26.9856656232739,0.,0.));
#77130=CARTESIAN_POINT('',(12.3548486633046,41.2638565969525,9.30505984645652));
#77131=CARTESIAN_POINT('Origin',(20.8267261185512,0.,0.));
#77132=CARTESIAN_POINT('',(13.103292255208,41.2086042970448,9.54677599452213));
#77133=CARTESIAN_POINT('Origin',(25.13830739299,0.,0.));
#77134=CARTESIAN_POINT('',(21.896707744792,41.2086042970448,9.54677599452213));
#77135=CARTESIAN_POINT('',(17.5,41.2086042970448,9.54677599452213));
#77136=CARTESIAN_POINT('',(22.6451513366954,41.2638565969525,9.30505984645652));
#77137=CARTESIAN_POINT('Origin',(9.86169260701005,0.,0.));
#77138=CARTESIAN_POINT('',(23.3381365738089,41.3486599091995,8.92066834454427));
#77139=CARTESIAN_POINT('Origin',(14.1732738814488,0.,0.));
#77140=CARTESIAN_POINT('',(24.1697957402248,41.4003266344532,8.6777274997883));
#77141=CARTESIAN_POINT('Origin',(8.01433437672608,0.,0.));
#77142=CARTESIAN_POINT('',(29.9005519666592,41.325703839893,9.02641690470011));
#77143=CARTESIAN_POINT('Origin',(97.7155570771054,0.,0.));
#77144=CARTESIAN_POINT('',(29.9040600247032,41.2086042970448,9.54677599452213));
#77145=CARTESIAN_POINT('Origin',(35.8405517186909,0.,0.));
#77146=CARTESIAN_POINT('',(17.5,41.2086042970448,9.54677599452213));
#77147=CARTESIAN_POINT('Origin',(33.1,37.1361751213135,8.2235635438135));
#77148=CARTESIAN_POINT('',(30.5247014514712,36.9673747121716,8.16871696615113));
#77149=CARTESIAN_POINT('Origin',(30.5,37.1361751213135,8.2235635438135));
#77150=CARTESIAN_POINT('',(30.4955273645547,37.253610541118,7.74082391359484));
#77151=CARTESIAN_POINT('Origin',(30.5,37.2229992101469,7.73115966730739));
#77152=CARTESIAN_POINT('',(24.1012882089558,37.3682767550424,7.36197779558791));
#77153=CARTESIAN_POINT('Origin',(24.1,37.2924584812137,7.33723656610251));
#77154=CARTESIAN_POINT('',(23.1004586919557,37.2482773116316,7.63515978098256));
#77155=CARTESIAN_POINT('Origin',(23.1,37.2403640279136,7.63267889200617));
#77156=CARTESIAN_POINT('',(22.399682944576,37.1656113221937,8.02494855741037));
#77157=CARTESIAN_POINT('Origin',(22.4,37.1709047568469,8.02660199321105));
#77158=CARTESIAN_POINT('',(21.7998387845652,37.1293862292573,8.22135769906884));
#77159=CARTESIAN_POINT('Origin',(21.8,37.1361751213135,8.2235635438135));
#77160=CARTESIAN_POINT('',(13.2021921742626,37.0438611660612,8.19356892151487));
#77161=CARTESIAN_POINT('Origin',(13.2,37.1361751213135,8.2235635438135));
#77162=CARTESIAN_POINT('',(12.6002487187375,37.1667522450638,8.02530493145534));
#77163=CARTESIAN_POINT('Origin',(12.6,37.1709047568469,8.02660199321105));
#77164=CARTESIAN_POINT('',(11.8996457869536,37.2464748574103,7.6345946946079));
#77165=CARTESIAN_POINT('Origin',(11.9,37.2403640279136,7.63267889200617));
#77166=CARTESIAN_POINT('',(10.899790263986,37.3048026141052,7.34126473779837));
#77167=CARTESIAN_POINT('Origin',(10.9,37.2924584812137,7.33723656610251));
#77168=CARTESIAN_POINT('',(4.55736144060343,37.6155887839604,7.85510339046017));
#77169=CARTESIAN_POINT('Origin',(4.5,37.2229992101469,7.73115966730739));
#77170=CARTESIAN_POINT('',(4.49524972087093,37.1037135041708,8.21301612503227));
#77171=CARTESIAN_POINT('Origin',(4.5,37.1361751213135,8.2235635438135));
#77172=CARTESIAN_POINT('',(1.90350512467335,37.0720625104951,8.20273209378168));
#77173=CARTESIAN_POINT('Origin',(1.9,37.1361751213135,8.2235635438135));
#77174=CARTESIAN_POINT('Ctrl Pts',(0.138207714141622,41.9261572390061,8.41238483838184));
#77175=CARTESIAN_POINT('Ctrl Pts',(0.37021747089976,41.6665974739906,8.52664381638148));
#77176=CARTESIAN_POINT('Ctrl Pts',(0.600000000000001,41.4083493394303,8.63936369090332));
#77177=CARTESIAN_POINT('Origin',(1.9,37.7092141076143,4.97369795887321));
#77178=CARTESIAN_POINT('',(5.09593997529677,41.9886110647639,5.12313779357752));
#77179=CARTESIAN_POINT('',(17.5,41.9886110647639,5.12313779357752));
#77180=CARTESIAN_POINT('',(4.47529854852883,37.5318349744051,4.96750374304976));
#77181=CARTESIAN_POINT('Origin',(4.5,37.7092141076143,4.97369795887321));
#77182=CARTESIAN_POINT('',(5.09944803334083,41.9206753505941,5.65216579287046));
#77183=CARTESIAN_POINT('Origin',(-0.840551718690874,0.,0.));
#77184=CARTESIAN_POINT('',(4.50447263544529,37.6544606275072,5.46749010626366));
#77185=CARTESIAN_POINT('Origin',(4.5,37.6223900187809,5.46610183537931));
#77186=CARTESIAN_POINT('',(10.8302042597752,41.8715390397407,6.00534915250318));
#77187=CARTESIAN_POINT('Origin',(-62.7155570771055,0.,0.));
#77188=CARTESIAN_POINT('',(10.8987117910442,37.6326386190063,5.86270716268919));
#77189=CARTESIAN_POINT('Origin',(10.9,37.5529307477141,5.8600249365842));
#77190=CARTESIAN_POINT('',(11.6618634261911,41.9060788618227,5.75938837262207));
#77191=CARTESIAN_POINT('Origin',(26.9856656232739,0.,0.));
#77192=CARTESIAN_POINT('',(11.8995413080444,37.6133097693334,5.56495784004781));
#77193=CARTESIAN_POINT('Origin',(11.9,37.6050252010142,5.56458261068053));
#77194=CARTESIAN_POINT('',(12.3548486633046,41.9578594516632,5.3691740737731));
#77195=CARTESIAN_POINT('Origin',(20.8267261185512,0.,0.));
#77196=CARTESIAN_POINT('',(12.600317055424,37.6689447622493,5.17040276961776));
#77197=CARTESIAN_POINT('Origin',(12.6,37.674484472081,5.17065950947565));
#77198=CARTESIAN_POINT('',(13.103292255208,41.9886110647639,5.12313779357752));
#77199=CARTESIAN_POINT('Origin',(25.13830739299,0.,0.));
#77200=CARTESIAN_POINT('',(13.2001612154348,37.7020801925101,4.97344883706828));
#77201=CARTESIAN_POINT('Origin',(13.2,37.7092141076143,4.97369795887321));
#77202=CARTESIAN_POINT('',(21.896707744792,41.9886110647639,5.12313779357752));
#77203=CARTESIAN_POINT('',(17.5,41.9886110647639,5.12313779357752));
#77204=CARTESIAN_POINT('',(21.7978078257374,37.6122086000506,4.97031045190415));
#77205=CARTESIAN_POINT('Origin',(21.8,37.7092141076143,4.97369795887321));
#77206=CARTESIAN_POINT('',(22.6451513366954,41.9578594516632,5.3691740737731));
#77207=CARTESIAN_POINT('Origin',(9.86169260701005,0.,0.));
#77208=CARTESIAN_POINT('',(22.3997512812625,37.6701387661531,5.17045810616099));
#77209=CARTESIAN_POINT('Origin',(22.4,37.674484472081,5.17065950947565));
#77210=CARTESIAN_POINT('',(23.3381365738089,41.9060788618227,5.75938837262207));
#77211=CARTESIAN_POINT('Origin',(14.1732738814488,0.,0.));
#77212=CARTESIAN_POINT('',(23.1003542130464,37.6114227454796,5.56487237189312));
#77213=CARTESIAN_POINT('Origin',(23.1,37.6050252010142,5.56458261068053));
#77214=CARTESIAN_POINT('',(24.1697957402248,41.8715390397407,6.00534915250318));
#77215=CARTESIAN_POINT('Origin',(8.01433437672607,0.,0.));
#77216=CARTESIAN_POINT('',(24.100209736014,37.565908154163,5.8604616354671));
#77217=CARTESIAN_POINT('Origin',(24.1,37.5529307477141,5.8600249365842));
#77218=CARTESIAN_POINT('',(29.9005519666592,41.9206753505941,5.65216579287046));
#77219=CARTESIAN_POINT('Origin',(97.7155570771054,0.,0.));
#77220=CARTESIAN_POINT('',(30.4426385593966,38.0336947942479,5.48390637564377));
#77221=CARTESIAN_POINT('Origin',(30.5,37.6223900187809,5.46610183537931));
#77222=CARTESIAN_POINT('',(29.9040600247032,41.9886110647639,5.12313779357752));
#77223=CARTESIAN_POINT('Origin',(35.8405517186909,0.,0.));
#77224=CARTESIAN_POINT('',(30.5047502791291,37.6751027358433,4.97250676352255));
#77225=CARTESIAN_POINT('Origin',(30.5,37.7092141076143,4.97369795887321));
#77226=CARTESIAN_POINT('',(17.5,41.9886110647639,5.12313779357752));
#77227=CARTESIAN_POINT('Origin',(17.5,42.1005314412719,7.42345959526127));
#77228=CARTESIAN_POINT('Origin',(17.5,0.,0.));
#77229=CARTESIAN_POINT('',(0.600000000000001,42.2794732300362,1.31762794090604));
#77230=CARTESIAN_POINT('Origin',(0.600000000000001,0.,0.));
#77231=CARTESIAN_POINT('',(1.67735469196904,42.240333256585,2.24593997529677));
#77232=CARTESIAN_POINT('Origin',(8.14497546096349,0.,0.));
#77233=CARTESIAN_POINT('',(5.09593997529677,42.240333256585,2.24593997529677));
#77234=CARTESIAN_POINT('',(17.5,42.240333256585,2.24593997529677));
#77235=CARTESIAN_POINT('',(5.09944803334083,42.2652943865761,1.71315218706844));
#77236=CARTESIAN_POINT('Origin',(-0.840551718690872,0.,0.));
#77237=CARTESIAN_POINT('',(10.8302042597752,42.2782342134758,1.35680204543027));
#77238=CARTESIAN_POINT('Origin',(-62.7155570771055,0.,0.));
#77239=CARTESIAN_POINT('',(11.6618634261911,42.269538656846,1.60502390555561));
#77240=CARTESIAN_POINT('Origin',(26.9856656232739,0.,0.));
#77241=CARTESIAN_POINT('',(12.3548486633046,42.2527725812817,1.99830157746262));
#77242=CARTESIAN_POINT('Origin',(20.8267261185512,0.,0.));
#77243=CARTESIAN_POINT('',(13.103292255208,42.240333256585,2.24593997529677));
#77244=CARTESIAN_POINT('Origin',(25.13830739299,0.,0.));
#77245=CARTESIAN_POINT('',(21.896707744792,42.240333256585,2.24593997529677));
#77246=CARTESIAN_POINT('',(17.5,42.240333256585,2.24593997529677));
#77247=CARTESIAN_POINT('',(22.6451513366954,42.2527725812817,1.99830157746261));
#77248=CARTESIAN_POINT('Origin',(9.86169260701005,0.,0.));
#77249=CARTESIAN_POINT('',(23.3381365738089,42.269538656846,1.60502390555561));
#77250=CARTESIAN_POINT('Origin',(14.1732738814488,0.,0.));
#77251=CARTESIAN_POINT('',(24.1697957402248,42.2782342134758,1.35680204543027));
#77252=CARTESIAN_POINT('Origin',(8.01433437672608,0.,0.));
#77253=CARTESIAN_POINT('',(29.9005519666592,42.2652943865761,1.71315218706844));
#77254=CARTESIAN_POINT('Origin',(97.7155570771054,0.,0.));
#77255=CARTESIAN_POINT('',(29.9040600247032,42.240333256585,2.24593997529677));
#77256=CARTESIAN_POINT('Origin',(35.8405517186909,0.,0.));
#77257=CARTESIAN_POINT('',(17.5,42.240333256585,2.24593997529677));
#77258=CARTESIAN_POINT('Origin',(1.9,38.,-1.65));
#77259=CARTESIAN_POINT('',(5.09593997529677,42.240333256585,-2.24593997529677));
#77260=CARTESIAN_POINT('',(17.5,42.240333256585,-2.24593997529677));
#77261=CARTESIAN_POINT('',(4.47529854852883,37.8242400401031,-1.62529854852883));
#77262=CARTESIAN_POINT('Origin',(4.5,38.,-1.65));
#77263=CARTESIAN_POINT('',(5.09944803334083,42.2652943865761,-1.71315218706844));
#77264=CARTESIAN_POINT('Origin',(-0.840551718690874,0.,0.));
#77265=CARTESIAN_POINT('',(4.50447263544529,38.0318244548267,-1.15420182283181));
#77266=CARTESIAN_POINT('Origin',(4.5,38.,-1.15));
#77267=CARTESIAN_POINT('',(10.8302042597752,42.2782342134758,-1.35680204543028));
#77268=CARTESIAN_POINT('Origin',(-62.7155570771055,0.,0.));
#77269=CARTESIAN_POINT('',(10.8987117910442,38.0789626932999,-0.761199649532072));
#77270=CARTESIAN_POINT('Origin',(10.9,38.,-0.75));
#77271=CARTESIAN_POINT('',(11.6618634261911,42.269538656846,-1.60502390555561));
#77272=CARTESIAN_POINT('Origin',(26.9856656232739,0.,0.));
#77273=CARTESIAN_POINT('',(11.8995413080444,38.0082238650069,-1.05106907140133));
#77274=CARTESIAN_POINT('Origin',(11.9,38.,-1.05));
#77275=CARTESIAN_POINT('',(12.3548486633046,42.2527725812817,-1.99830157746261));
#77276=CARTESIAN_POINT('Origin',(20.8267261185512,0.,0.));
#77277=CARTESIAN_POINT('',(12.600317055424,37.9944998683999,-1.44929087888549));
#77278=CARTESIAN_POINT('Origin',(12.6,38.,-1.45));
#77279=CARTESIAN_POINT('',(13.103292255208,42.240333256585,-2.24593997529677));
#77280=CARTESIAN_POINT('Origin',(25.13830739299,0.,0.));
#77281=CARTESIAN_POINT('',(13.2001612154348,37.9929312055486,-1.64900654572746));
#77282=CARTESIAN_POINT('Origin',(13.2,38.,-1.65));
#77283=CARTESIAN_POINT('',(21.896707744792,42.240333256585,-2.24593997529677));
#77284=CARTESIAN_POINT('',(17.5,42.240333256585,-2.24593997529677));
#77285=CARTESIAN_POINT('',(21.7978078257374,37.9038799896544,-1.63649121351442));
#77286=CARTESIAN_POINT('Origin',(21.8,38.,-1.65));
#77287=CARTESIAN_POINT('',(22.6451513366954,42.2527725812817,-1.99830157746261));
#77288=CARTESIAN_POINT('Origin',(9.86169260701005,0.,0.));
#77289=CARTESIAN_POINT('',(22.3997512812625,37.9956853417913,-1.44944371963071));
#77290=CARTESIAN_POINT('Origin',(22.4,38.,-1.45));
#77291=CARTESIAN_POINT('',(23.3381365738089,42.269538656846,-1.60502390555561));
#77292=CARTESIAN_POINT('Origin',(14.1732738814488,0.,0.));
#77293=CARTESIAN_POINT('',(23.1003542130464,38.0063506678963,-1.05082556284928));
#77294=CARTESIAN_POINT('Origin',(23.1,38.,-1.05));
#77295=CARTESIAN_POINT('',(24.1697957402248,42.2782342134758,-1.35680204543027));
#77296=CARTESIAN_POINT('Origin',(8.01433437672608,0.,0.));
#77297=CARTESIAN_POINT('',(24.100209736014,38.01285608245,-0.751823438535068));
#77298=CARTESIAN_POINT('Origin',(24.1,38.,-0.75));
#77299=CARTESIAN_POINT('',(29.9005519666592,42.2652943865761,-1.71315218706844));
#77300=CARTESIAN_POINT('Origin',(97.7155570771054,0.,0.));
#77301=CARTESIAN_POINT('',(30.4426385593966,38.408147857702,-1.2038882754343));
#77302=CARTESIAN_POINT('Origin',(30.5,38.,-1.15));
#77303=CARTESIAN_POINT('',(29.9040600247032,42.240333256585,-2.24593997529677));
#77304=CARTESIAN_POINT('Origin',(35.8405517186909,0.,0.));
#77305=CARTESIAN_POINT('',(30.5047502791291,37.9662000077121,-1.64524972087093));
#77306=CARTESIAN_POINT('Origin',(30.5,38.,-1.65));
#77307=CARTESIAN_POINT('',(33.3226453080309,42.240333256585,-2.24593997529677));
#77308=CARTESIAN_POINT('',(17.5,42.240333256585,-2.24593997529677));
#77309=CARTESIAN_POINT('',(33.0964948753266,37.933244060464,-1.64061806453627));
#77310=CARTESIAN_POINT('Origin',(33.1,38.,-1.65));
#77311=CARTESIAN_POINT('Origin',(26.8550245390365,0.,0.));
#77312=CARTESIAN_POINT('Origin',(33.1,38.,1.65));
#77313=CARTESIAN_POINT('',(30.5247014514712,37.8242400401031,1.62529854852883));
#77314=CARTESIAN_POINT('Origin',(30.5,38.,1.65));
#77315=CARTESIAN_POINT('',(30.4955273645547,38.0318244548267,1.15420182283181));
#77316=CARTESIAN_POINT('Origin',(30.5,38.,1.15));
#77317=CARTESIAN_POINT('',(24.1012882089558,38.0789626932999,0.761199649532072));
#77318=CARTESIAN_POINT('Origin',(24.1,38.,0.75));
#77319=CARTESIAN_POINT('',(23.1004586919557,38.0082238650069,1.05106907140133));
#77320=CARTESIAN_POINT('Origin',(23.1,38.,1.05));
#77321=CARTESIAN_POINT('',(22.399682944576,37.9944998683999,1.44929087888549));
#77322=CARTESIAN_POINT('Origin',(22.4,38.,1.45));
#77323=CARTESIAN_POINT('',(21.7998387845652,37.9929312055486,1.64900654572746));
#77324=CARTESIAN_POINT('Origin',(21.8,38.,1.65));
#77325=CARTESIAN_POINT('',(13.2021921742626,37.9038799896544,1.63649121351442));
#77326=CARTESIAN_POINT('Origin',(13.2,38.,1.65));
#77327=CARTESIAN_POINT('',(12.6002487187375,37.9956853417913,1.44944371963071));
#77328=CARTESIAN_POINT('Origin',(12.6,38.,1.45));
#77329=CARTESIAN_POINT('',(11.8996457869536,38.0063506678963,1.05082556284928));
#77330=CARTESIAN_POINT('Origin',(11.9,38.,1.05));
#77331=CARTESIAN_POINT('',(10.899790263986,38.01285608245,0.751823438535068));
#77332=CARTESIAN_POINT('Origin',(10.9,38.,0.75));
#77333=CARTESIAN_POINT('',(4.55736144060343,38.408147857702,1.2038882754343));
#77334=CARTESIAN_POINT('Origin',(4.5,38.,1.15));
#77335=CARTESIAN_POINT('',(4.49524972087093,37.9662000077121,1.64524972087093));
#77336=CARTESIAN_POINT('Origin',(4.5,38.,1.65));
#77337=CARTESIAN_POINT('',(1.90350512467335,37.933244060464,1.64061806453627));
#77338=CARTESIAN_POINT('Origin',(1.9,38.,1.65));
#77339=CARTESIAN_POINT('Ctrl Pts',(0.138207714141622,42.75,1.00418100903021));
#77340=CARTESIAN_POINT('Ctrl Pts',(0.37021747090124,42.514224394353,1.1617762166071));
#77341=CARTESIAN_POINT('Ctrl Pts',(0.6,42.2794732300361,1.31762794090604));
#77342=CARTESIAN_POINT('Origin',(0.299999999999998,0.,0.));
#77343=CARTESIAN_POINT('Origin',(0.600000000000001,0.,0.));
#77344=CARTESIAN_POINT('',(-2.8796409701215E-15,-42.9,-5.25373476834215E-15));
#77345=CARTESIAN_POINT('',(0.299999999999998,-42.6,-5.21699536436772E-15));
#77346=CARTESIAN_POINT('Origin',(0.,0.,0.));
#77347=CARTESIAN_POINT('Origin',(34.8112283287268,0.,-1.45831369988988E-15));
#77348=CARTESIAN_POINT('',(35.,47.1,-5.76808642398403E-15));
#77349=CARTESIAN_POINT('Origin',(35.,0.,0.));
#77350=CARTESIAN_POINT('',(34.6224566574536,47.6321401698912,5.83325479955954E-15));
#77351=CARTESIAN_POINT('',(34.8112283287268,47.3660700849456,5.80067061177179E-15));
#77352=CARTESIAN_POINT('',(34.6224566574536,-47.6321401698912,-5.83325479955954E-15));
#77353=CARTESIAN_POINT('Origin',(34.6224566574536,0.,-2.91662739977977E-15));
#77354=CARTESIAN_POINT('Origin',(34.6224566574536,0.,-2.91662739977977E-15));
#77355=CARTESIAN_POINT('Origin',(30.,0.,0.));
#77356=CARTESIAN_POINT('',(25.9624281765825,-50.6631501381961,-6.20444646514636E-15));
#77357=CARTESIAN_POINT('',(30.,-49.25,-6.03138548580071E-15));
#77358=CARTESIAN_POINT('',(25.9624281765825,-6.20444646514636E-15,50.6631501381961));
#77359=CARTESIAN_POINT('Origin',(25.9624281765825,0.,-7.75555808143296E-15));
#77360=CARTESIAN_POINT('Origin',(25.9624281765825,0.,-7.75555808143296E-15));
#77361=CARTESIAN_POINT('Origin',(35.,42.9,0.));
#77362=CARTESIAN_POINT('Origin',(23.9803256282139,0.,0.));
#77363=CARTESIAN_POINT('',(23.9803256282139,-6.2456986756515E-15,51.));
#77364=CARTESIAN_POINT('Origin',(23.9803256282139,-5.51091059616309E-15,
45.));
#77365=CARTESIAN_POINT('',(23.9803256282139,-51.,-6.2456986756515E-15));
#77366=CARTESIAN_POINT('Origin',(23.9803256282139,0.,0.));
#77367=CARTESIAN_POINT('Origin',(23.9803256282139,0.,0.));
#77368=CARTESIAN_POINT('Origin',(19.9,0.,0.));
#77369=CARTESIAN_POINT('',(14.8,-51.,-6.2456986756515E-15));
#77370=CARTESIAN_POINT('',(19.9,-51.,-6.2456986756515E-15));
#77371=CARTESIAN_POINT('Origin',(14.8,0.,0.));
#77372=CARTESIAN_POINT('Origin',(12.6,0.,0.));
#77373=CARTESIAN_POINT('',(12.6,-46.5,-5.69460761603519E-15));
#77374=CARTESIAN_POINT('',(12.6,-5.69460761603519E-15,46.5));
#77375=CARTESIAN_POINT('Origin',(12.6,0.,0.));
#77376=CARTESIAN_POINT('',(13.,-5.74359348800109E-15,46.9));
#77377=CARTESIAN_POINT('Origin',(12.6,-5.74359348800109E-15,46.9));
#77378=CARTESIAN_POINT('Origin',(13.,0.,0.));
#77379=CARTESIAN_POINT('Origin',(12.6,0.,0.));
#77380=CARTESIAN_POINT('Origin',(9.25,0.,0.));
#77381=CARTESIAN_POINT('',(5.9,-46.5,-5.69460761603519E-15));
#77382=CARTESIAN_POINT('',(9.25,-46.5,-5.69460761603519E-15));
#77383=CARTESIAN_POINT('',(5.9,-5.69460761603519E-15,46.5));
#77384=CARTESIAN_POINT('Origin',(5.9,0.,0.));
#77385=CARTESIAN_POINT('Origin',(5.9,0.,0.));
#77386=CARTESIAN_POINT('Origin',(13.,50.4,0.));
#77387=CARTESIAN_POINT('',(13.,-50.4,-6.17221986770266E-15));
#77388=CARTESIAN_POINT('Origin',(13.,0.,0.));
#77389=CARTESIAN_POINT('Origin',(5.9,0.,0.));
#77390=CARTESIAN_POINT('',(5.5,-5.74359348800109E-15,46.9));
#77391=CARTESIAN_POINT('Origin',(5.5,0.,0.));
#77392=CARTESIAN_POINT('Origin',(5.9,-5.74359348800109E-15,46.9));
#77393=CARTESIAN_POINT('Origin',(5.5,46.5,0.));
#77394=CARTESIAN_POINT('',(5.5,-50.,-6.12323399573677E-15));
#77395=CARTESIAN_POINT('Origin',(5.5,0.,0.));
#77396=CARTESIAN_POINT('Origin',(17.5,0.,0.));
#77397=CARTESIAN_POINT('Origin',(0.,49.7,0.));
#77398=CARTESIAN_POINT('',(1.31838984174237E-15,-49.7,-6.08649459176235E-15));
#77399=CARTESIAN_POINT('Origin',(0.,0.,0.));
#77400=CARTESIAN_POINT('Origin',(0.4,0.,0.));
#77401=CARTESIAN_POINT('',(0.800000000000004,-50.5,-6.18446633569413E-15));
#77402=CARTESIAN_POINT('Origin',(0.800000000000001,0.,0.));
#77403=CARTESIAN_POINT('',(0.4,-50.1,-6.13548046372824E-15));
#77404=CARTESIAN_POINT('Origin',(2.9,0.,0.));
#77405=CARTESIAN_POINT('',(5.,-50.5,-6.18446633569413E-15));
#77406=CARTESIAN_POINT('Origin',(5.,0.,0.));
#77407=CARTESIAN_POINT('',(2.9,-50.5,-6.18446633569413E-15));
#77408=CARTESIAN_POINT('Origin',(5.25,0.,0.));
#77409=CARTESIAN_POINT('',(5.25,-50.25,-6.15385016571545E-15));
#77410=CARTESIAN_POINT('Origin',(13.75,0.,0.));
#77411=CARTESIAN_POINT('',(14.5,-50.4,-6.17221986770266E-15));
#77412=CARTESIAN_POINT('Origin',(14.5,0.,0.));
#77413=CARTESIAN_POINT('',(13.75,-50.4,-6.17221986770266E-15));
#77414=CARTESIAN_POINT('Origin',(14.65,0.,0.));
#77415=CARTESIAN_POINT('',(14.65,-50.7,-6.20895927167708E-15));
#77416=CARTESIAN_POINT('',(0.,0.,0.));
#77417=CARTESIAN_POINT('Origin',(0.,-14.743395421685,-41.6736702420106));
#77418=CARTESIAN_POINT('',(22.,-11.8091924752874,-35.3812517172812));
#77419=CARTESIAN_POINT('',(21.5,-12.0218682747234,-35.8373364409968));
#77420=CARTESIAN_POINT('Ctrl Pts',(22.,-11.8091924752874,-35.3812517172812));
#77421=CARTESIAN_POINT('Ctrl Pts',(21.7516860396895,-11.9148224027831,-35.6077758278089));
#77422=CARTESIAN_POINT('Ctrl Pts',(21.5,-12.0218682747234,-35.8373364409968));
#77423=CARTESIAN_POINT('',(22.,-10.7707837613225,-33.154377043866));
#77424=CARTESIAN_POINT('',(22.,-2.40948834572521,-15.223521160693));
#77425=CARTESIAN_POINT('',(0.,-10.7707837613225,-33.154377043866));
#77426=CARTESIAN_POINT('',(0.,-10.7707837613225,-33.154377043866));
#77427=CARTESIAN_POINT('',(3.46944695195361E-17,-11.8091924752874,-35.3812517172812));
#77428=CARTESIAN_POINT('',(0.,-2.11478812371661,-14.5915344951198));
#77429=CARTESIAN_POINT('',(0.499999999999998,-12.0218682747234,-35.8373364409968));
#77430=CARTESIAN_POINT('Ctrl Pts',(0.500000000000005,-12.0218682747234,
-35.8373364409968));
#77431=CARTESIAN_POINT('Ctrl Pts',(0.248313955079475,-11.9148224005581,
-35.6077758230372));
#77432=CARTESIAN_POINT('Ctrl Pts',(2.08166817117217E-16,-11.8091924752874,
-35.3812517172812));
#77433=CARTESIAN_POINT('',(11.,-12.0218682747234,-35.8373364409968));
#77434=CARTESIAN_POINT('Origin',(0.,-18.474399951134,-29.5621218190701));
#77435=CARTESIAN_POINT('',(21.5,-19.725484464535,-32.2450812162009));
#77436=CARTESIAN_POINT('',(22.,-19.5128086650989,-31.7889964924853));
#77437=CARTESIAN_POINT('Ctrl Pts',(21.5,-19.725484464535,-32.2450812162009));
#77438=CARTESIAN_POINT('Ctrl Pts',(21.7516860442549,-19.6184385906528,-32.0155205988484));
#77439=CARTESIAN_POINT('Ctrl Pts',(22.,-19.5128086650989,-31.7889964924853));
#77440=CARTESIAN_POINT('',(0.499999999999998,-19.725484464535,-32.2450812162009));
#77441=CARTESIAN_POINT('',(11.,-19.725484464535,-32.2450812162009));
#77442=CARTESIAN_POINT('',(6.93889390390723E-17,-19.5128086650989,-31.7889964924853));
#77443=CARTESIAN_POINT('Ctrl Pts',(-2.08166817117217E-16,-19.5128086650989,
-31.7889964924853));
#77444=CARTESIAN_POINT('Ctrl Pts',(0.248313955054683,-19.6184385903591,
-32.0155205982187));
#77445=CARTESIAN_POINT('Ctrl Pts',(0.500000000000004,-19.725484464535,-32.2450812162009));
#77446=CARTESIAN_POINT('',(0.,-18.474399951134,-29.5621218190701));
#77447=CARTESIAN_POINT('',(0.,-7.83209848334684,-6.73963267125159));
#77448=CARTESIAN_POINT('',(22.,-18.474399951134,-29.5621218190701));
#77449=CARTESIAN_POINT('',(0.,-18.474399951134,-29.5621218190701));
#77450=CARTESIAN_POINT('',(22.,-8.12679870535545,-7.37161933682474));
#77451=CARTESIAN_POINT('Origin',(0.,-10.7707837613225,-33.154377043866));
#77452=CARTESIAN_POINT('',(0.,2.62230665155162,-39.3996776697515));
#77453=CARTESIAN_POINT('',(22.,1.26700687356023,-38.7676910041784));
#77454=CARTESIAN_POINT('Origin',(11.,0.,0.));
#77455=CARTESIAN_POINT('',(0.499999999999998,-11.3395294590896,-36.0590497884572));
#77456=CARTESIAN_POINT('Origin',(0.499999999999998,0.,0.));
#77457=CARTESIAN_POINT('',(21.5,-11.3395294590896,-36.0590497884572));
#77458=CARTESIAN_POINT('',(11.,-11.3395294590896,-36.0590497884572));
#77459=CARTESIAN_POINT('Origin',(21.5,0.,0.));
#77460=CARTESIAN_POINT('Origin',(21.75,0.,0.));
#77461=CARTESIAN_POINT('',(22.,-24.7364665672137,27.9176865404195));
#77462=CARTESIAN_POINT('Origin',(22.,0.,0.));
#77463=CARTESIAN_POINT('',(21.5,-25.0251096245113,28.3299115473591));
#77464=CARTESIAN_POINT('Ctrl Pts',(22.,-24.7364665672137,27.9176865404195));
#77465=CARTESIAN_POINT('Ctrl Pts',(21.7516860460885,-24.8798272340583,28.1224267910188));
#77466=CARTESIAN_POINT('Ctrl Pts',(21.5,-25.0251096245113,28.3299115473591));
#77467=CARTESIAN_POINT('',(21.5,-25.5582884235871,27.8498454727622));
#77468=CARTESIAN_POINT('Origin',(21.5,0.,0.));
#77469=CARTESIAN_POINT('',(21.8,-25.3343218406523,27.6481850557002));
#77470=CARTESIAN_POINT('Ctrl Pts',(21.5,-25.5582884235871,27.8498454727622));
#77471=CARTESIAN_POINT('Ctrl Pts',(21.650603110123,-25.4458589814141,27.7486135483316));
#77472=CARTESIAN_POINT('Ctrl Pts',(21.8,-25.3343218406523,27.6481850557002));
#77473=CARTESIAN_POINT('',(21.8,-27.6481850557002,25.3343218406523));
#77474=CARTESIAN_POINT('Ctrl Pts',(21.8,-25.3343218406523,27.6481850557002));
#77475=CARTESIAN_POINT('Ctrl Pts',(21.8713861730393,-26.4912534481763,26.4912534481763));
#77476=CARTESIAN_POINT('Ctrl Pts',(21.8,-27.6481850557002,25.3343218406523));
#77477=CARTESIAN_POINT('',(21.5,-27.8498454727622,25.5582884235871));
#77478=CARTESIAN_POINT('Ctrl Pts',(21.8,-27.6481850557002,25.3343218406523));
#77479=CARTESIAN_POINT('Ctrl Pts',(21.6506031060906,-27.7486135510424,25.4458589844248));
#77480=CARTESIAN_POINT('Ctrl Pts',(21.5,-27.8498454727622,25.5582884235871));
#77481=CARTESIAN_POINT('',(21.5,-30.0060755079215,22.9885935327265));
#77482=CARTESIAN_POINT('Origin',(21.5,0.,0.));
#77483=CARTESIAN_POINT('',(21.8,-29.7504935167013,22.8288881795131));
#77484=CARTESIAN_POINT('Ctrl Pts',(21.5,-30.0060755079215,22.9885935327265));
#77485=CARTESIAN_POINT('Ctrl Pts',(21.6506031103503,-29.87777538221,22.9084227163233));
#77486=CARTESIAN_POINT('Ctrl Pts',(21.8,-29.7504935167013,22.8288881795131));
#77487=CARTESIAN_POINT('',(21.8,-31.6274058196267,20.1483796152605));
#77488=CARTESIAN_POINT('Ctrl Pts',(21.8,-29.7504935167013,22.8288881795131));
#77489=CARTESIAN_POINT('Ctrl Pts',(21.8713861730394,-30.688949668164,21.4886338973868));
#77490=CARTESIAN_POINT('Ctrl Pts',(21.8,-31.6274058196267,20.1483796152605));
#77491=CARTESIAN_POINT('',(21.5,-31.8648939508099,20.3339256786199));
#77492=CARTESIAN_POINT('Ctrl Pts',(21.8,-31.6274058196267,20.1483796152605));
#77493=CARTESIAN_POINT('Ctrl Pts',(21.6506031078004,-31.7456768008676,20.2407830329369));
#77494=CARTESIAN_POINT('Ctrl Pts',(21.5,-31.8648939508099,20.3339256786199));
#77495=CARTESIAN_POINT('',(21.5,-33.5421431717545,17.4288448109885));
#77496=CARTESIAN_POINT('Origin',(21.5,0.,0.));
#77497=CARTESIAN_POINT('',(21.8,-33.2627115017215,17.3159470879662));
#77498=CARTESIAN_POINT('Ctrl Pts',(21.5,-33.5421431717545,17.4288448109885));
#77499=CARTESIAN_POINT('Ctrl Pts',(21.6506031076066,-33.4018706996267,17.3721710534861));
#77500=CARTESIAN_POINT('Ctrl Pts',(21.8,-33.2627115017215,17.3159470879662));
#77501=CARTESIAN_POINT('',(21.8,-34.6456438619633,14.3502390708311));
#77502=CARTESIAN_POINT('Ctrl Pts',(21.8,-33.2627115017215,17.3159470879662));
#77503=CARTESIAN_POINT('Ctrl Pts',(21.8713861730393,-33.9541776818424,15.8330930793986));
#77504=CARTESIAN_POINT('Ctrl Pts',(21.8,-34.6456438619633,14.3502390708311));
#77505=CARTESIAN_POINT('',(21.5,-34.9117437505765,14.4917268913708));
#77506=CARTESIAN_POINT('Ctrl Pts',(21.8,-34.6456438619633,14.3502390708311));
#77507=CARTESIAN_POINT('Ctrl Pts',(21.6506031051379,-34.7781637286973,14.420701133856));
#77508=CARTESIAN_POINT('Ctrl Pts',(21.5,-34.9117437505765,14.4917268913708));
#77509=CARTESIAN_POINT('',(21.5,-36.0590497884572,11.3395294590896));
#77510=CARTESIAN_POINT('Origin',(21.5,0.,0.));
#77511=CARTESIAN_POINT('',(21.8,-35.764258829506,11.2768697064435));
#77512=CARTESIAN_POINT('Ctrl Pts',(21.5,-36.0590497884572,11.3395294590896));
#77513=CARTESIAN_POINT('Ctrl Pts',(21.6506031114238,-35.9110670719085,11.3080747616734));
#77514=CARTESIAN_POINT('Ctrl Pts',(21.8,-35.764258829506,11.2768697064435));
#77515=CARTESIAN_POINT('',(21.8,-36.6111915470959,8.11607377380575));
#77516=CARTESIAN_POINT('Ctrl Pts',(21.8,-35.764258829506,11.2768697064435));
#77517=CARTESIAN_POINT('Ctrl Pts',(21.8713861730393,-36.1877251883009,9.69647174012463));
#77518=CARTESIAN_POINT('Ctrl Pts',(21.8,-36.6111915470959,8.11607377380575));
#77519=CARTESIAN_POINT('',(21.5,-36.8978178826767,8.20920431569502));
#77520=CARTESIAN_POINT('Ctrl Pts',(21.8,-36.6111915470959,8.11607377380575));
#77521=CARTESIAN_POINT('Ctrl Pts',(21.6506031086383,-36.7539337447779,8.16245352531621));
#77522=CARTESIAN_POINT('Ctrl Pts',(21.5,-36.8978178826767,8.20920431569502));
#77523=CARTESIAN_POINT('',(21.5,-37.4803204240973,4.90566824265508));
#77524=CARTESIAN_POINT('Origin',(21.5,0.,0.));
#77525=CARTESIAN_POINT('',(21.8,-37.1791272503441,4.89515034526196));
#77526=CARTESIAN_POINT('Ctrl Pts',(21.5,-37.4803204240973,4.90566824265508));
#77527=CARTESIAN_POINT('Ctrl Pts',(21.6506031095962,-37.3291238484779,4.90038834188993));
#77528=CARTESIAN_POINT('Ctrl Pts',(21.8,-37.1791272503441,4.89515034526196));
#77529=CARTESIAN_POINT('',(21.8,-37.4643267032267,1.63530568209484));
#77530=CARTESIAN_POINT('Ctrl Pts',(21.8,-37.1791272503441,4.89515034526196));
#77531=CARTESIAN_POINT('Ctrl Pts',(21.8713861730394,-37.3217269767854,3.26522801367839));
#77532=CARTESIAN_POINT('Ctrl Pts',(21.8,-37.4643267032267,1.63530568209484));
#77533=CARTESIAN_POINT('',(21.5,-37.7627704896084,1.67724922094466));
#77534=CARTESIAN_POINT('Ctrl Pts',(21.8,-37.4643267032268,1.63530568209484));
#77535=CARTESIAN_POINT('Ctrl Pts',(21.6506031090722,-37.6129540850848,1.65619389840079));
#77536=CARTESIAN_POINT('Ctrl Pts',(21.5,-37.7627704896084,1.67724922094466));
#77537=CARTESIAN_POINT('',(21.5,-37.7627704896084,-1.67724922094464));
#77538=CARTESIAN_POINT('Origin',(21.5,0.,0.));
#77539=CARTESIAN_POINT('',(21.8,-37.4643267032267,-1.63530568209482));
#77540=CARTESIAN_POINT('Ctrl Pts',(21.5,-37.7627704896084,-1.67724922094464));
#77541=CARTESIAN_POINT('Ctrl Pts',(21.6506031054658,-37.6129540886727,-1.65619389890503));
#77542=CARTESIAN_POINT('Ctrl Pts',(21.8,-37.4643267032267,-1.63530568209482));
#77543=CARTESIAN_POINT('',(21.8,-37.1791272503441,-4.89515034526194));
#77544=CARTESIAN_POINT('Ctrl Pts',(21.8,-37.4643267032267,-1.63530568209482));
#77545=CARTESIAN_POINT('Ctrl Pts',(21.8713861730393,-37.3217269767854,-3.26522801367838));
#77546=CARTESIAN_POINT('Ctrl Pts',(21.8,-37.1791272503441,-4.89515034526194));
#77547=CARTESIAN_POINT('',(21.5,-37.4803204240973,-4.90566824265506));
#77548=CARTESIAN_POINT('Ctrl Pts',(21.8,-37.1791272503441,-4.89515034526194));
#77549=CARTESIAN_POINT('Ctrl Pts',(21.6506031056359,-37.3291238524543,-4.90038834202877));
#77550=CARTESIAN_POINT('Ctrl Pts',(21.5,-37.4803204240973,-4.90566824265506));
#77551=CARTESIAN_POINT('',(21.5,-36.8978178826767,-8.209204315695));
#77552=CARTESIAN_POINT('Origin',(21.5,0.,0.));
#77553=CARTESIAN_POINT('',(21.8,-36.6111915470959,-8.11607377380573));
#77554=CARTESIAN_POINT('Ctrl Pts',(21.5,-36.8978178826767,-8.209204315695));
#77555=CARTESIAN_POINT('Ctrl Pts',(21.6506031086279,-36.7539337447878,-8.16245352531941));
#77556=CARTESIAN_POINT('Ctrl Pts',(21.8,-36.6111915470959,-8.11607377380573));
#77557=CARTESIAN_POINT('',(21.8,-35.764258829506,-11.2768697064435));
#77558=CARTESIAN_POINT('Ctrl Pts',(21.8,-36.6111915470959,-8.11607377380573));
#77559=CARTESIAN_POINT('Ctrl Pts',(21.8713861730394,-36.1877251883009,-9.69647174012462));
#77560=CARTESIAN_POINT('Ctrl Pts',(21.8,-35.764258829506,-11.2768697064435));
#77561=CARTESIAN_POINT('',(21.5,-36.0590497884573,-11.3395294590896));
#77562=CARTESIAN_POINT('Ctrl Pts',(21.8,-35.764258829506,-11.2768697064435));
#77563=CARTESIAN_POINT('Ctrl Pts',(21.6506031113732,-35.9110670719583,-11.308074761684));
#77564=CARTESIAN_POINT('Ctrl Pts',(21.5,-36.0590497884573,-11.3395294590896));
#77565=CARTESIAN_POINT('',(21.5,-34.9117437505765,-14.4917268913708));
#77566=CARTESIAN_POINT('Origin',(21.5,0.,0.));
#77567=CARTESIAN_POINT('',(21.8,-34.6456438619633,-14.3502390708311));
#77568=CARTESIAN_POINT('Ctrl Pts',(21.5,-34.9117437505765,-14.4917268913708));
#77569=CARTESIAN_POINT('Ctrl Pts',(21.6506031088497,-34.7781637254046,-14.4207011321053));
#77570=CARTESIAN_POINT('Ctrl Pts',(21.8,-34.6456438619633,-14.3502390708311));
#77571=CARTESIAN_POINT('',(21.8,-33.2627115017215,-17.3159470879662));
#77572=CARTESIAN_POINT('Ctrl Pts',(21.8,-34.6456438619633,-14.3502390708311));
#77573=CARTESIAN_POINT('Ctrl Pts',(21.8713861730394,-33.9541776818424,-15.8330930793986));
#77574=CARTESIAN_POINT('Ctrl Pts',(21.8,-33.2627115017215,-17.3159470879662));
#77575=CARTESIAN_POINT('',(21.5,-33.5421431717545,-17.4288448109885));
#77576=CARTESIAN_POINT('Ctrl Pts',(21.8,-33.2627115017215,-17.3159470879662));
#77577=CARTESIAN_POINT('Ctrl Pts',(21.6506031080477,-33.4018706992158,-17.3721710533201));
#77578=CARTESIAN_POINT('Ctrl Pts',(21.5,-33.5421431717545,-17.4288448109885));
#77579=CARTESIAN_POINT('',(21.5,-31.8648939508099,-20.3339256786199));
#77580=CARTESIAN_POINT('Origin',(21.5,0.,0.));
#77581=CARTESIAN_POINT('',(21.8,-31.6274058196267,-20.1483796152605));
#77582=CARTESIAN_POINT('Ctrl Pts',(21.5,-31.8648939508099,-20.3339256786199));
#77583=CARTESIAN_POINT('Ctrl Pts',(21.6506031077088,-31.7456768009401,-20.2407830329936));
#77584=CARTESIAN_POINT('Ctrl Pts',(21.8,-31.6274058196267,-20.1483796152605));
#77585=CARTESIAN_POINT('',(21.8,-29.7504935167013,-22.8288881795131));
#77586=CARTESIAN_POINT('Ctrl Pts',(21.8,-31.6274058196267,-20.1483796152605));
#77587=CARTESIAN_POINT('Ctrl Pts',(21.8713861730394,-30.688949668164,-21.4886338973868));
#77588=CARTESIAN_POINT('Ctrl Pts',(21.8,-29.7504935167013,-22.8288881795131));
#77589=CARTESIAN_POINT('',(21.5,-30.0060755079215,-22.9885935327265));
#77590=CARTESIAN_POINT('Ctrl Pts',(21.8,-29.7504935167013,-22.8288881795131));
#77591=CARTESIAN_POINT('Ctrl Pts',(21.6506031102095,-29.87777538233,-22.9084227163982));
#77592=CARTESIAN_POINT('Ctrl Pts',(21.5,-30.0060755079215,-22.9885935327265));
#77593=CARTESIAN_POINT('',(21.5,-27.8498454727622,-25.5582884235871));
#77594=CARTESIAN_POINT('Origin',(21.5,0.,0.));
#77595=CARTESIAN_POINT('',(21.8,-27.6481850557002,-25.3343218406523));
#77596=CARTESIAN_POINT('Ctrl Pts',(21.5,-27.8498454727622,-25.5582884235871));
#77597=CARTESIAN_POINT('Ctrl Pts',(21.6506031063136,-27.7486135508925,-25.4458589842583));
#77598=CARTESIAN_POINT('Ctrl Pts',(21.8,-27.6481850557002,-25.3343218406523));
#77599=CARTESIAN_POINT('',(21.8,-25.3343218406523,-27.6481850557002));
#77600=CARTESIAN_POINT('Ctrl Pts',(21.8,-27.6481850557002,-25.3343218406523));
#77601=CARTESIAN_POINT('Ctrl Pts',(21.8713861730393,-26.4912534481763,-26.4912534481763));
#77602=CARTESIAN_POINT('Ctrl Pts',(21.8,-25.3343218406523,-27.6481850557002));
#77603=CARTESIAN_POINT('',(21.5,-25.5582884235871,-27.8498454727622));
#77604=CARTESIAN_POINT('Ctrl Pts',(21.8,-25.3343218406523,-27.6481850557002));
#77605=CARTESIAN_POINT('Ctrl Pts',(21.6506031088795,-25.4458589823425,-27.7486135491675));
#77606=CARTESIAN_POINT('Ctrl Pts',(21.5,-25.5582884235871,-27.8498454727622));
#77607=CARTESIAN_POINT('',(21.5,-22.9885935327265,-30.0060755079215));
#77608=CARTESIAN_POINT('Origin',(21.5,0.,0.));
#77609=CARTESIAN_POINT('',(21.8,-22.8288881795131,-29.7504935167013));
#77610=CARTESIAN_POINT('Ctrl Pts',(21.5,-22.9885935327265,-30.0060755079215));
#77611=CARTESIAN_POINT('Ctrl Pts',(21.6506031103464,-22.9084227163254,-29.8777753822133));
#77612=CARTESIAN_POINT('Ctrl Pts',(21.8,-22.8288881795131,-29.7504935167013));
#77613=CARTESIAN_POINT('',(21.8,-20.1483796152605,-31.6274058196267));
#77614=CARTESIAN_POINT('Ctrl Pts',(21.8,-22.8288881795131,-29.7504935167013));
#77615=CARTESIAN_POINT('Ctrl Pts',(21.8713861730393,-21.4886338973868,-30.688949668164));
#77616=CARTESIAN_POINT('Ctrl Pts',(21.8,-20.1483796152605,-31.6274058196267));
#77617=CARTESIAN_POINT('',(21.5,-20.3339256786199,-31.8648939508099));
#77618=CARTESIAN_POINT('Ctrl Pts',(21.8,-20.1483796152605,-31.6274058196267));
#77619=CARTESIAN_POINT('Ctrl Pts',(21.6506031036307,-20.240783035516,-31.7456768041687));
#77620=CARTESIAN_POINT('Ctrl Pts',(21.5,-20.3339256786199,-31.8648939508099));
#77621=CARTESIAN_POINT('Origin',(21.5,0.,0.));
#77622=CARTESIAN_POINT('Origin',(0.,37.3,0.));
#77623=CARTESIAN_POINT('',(0.,-24.7364665672137,27.9176865404195));
#77624=CARTESIAN_POINT('Origin',(0.,0.,0.));
#77625=CARTESIAN_POINT('',(0.,-23.3271408859744,25.9049608779072));
#77626=CARTESIAN_POINT('',(0.,-9.96441562446309,6.82101143103729));
#77627=CARTESIAN_POINT('',(0.,-16.364348509518,30.7803605868911));
#77628=CARTESIAN_POINT('',(0.,-9.07210495534843,35.8864444939818));
#77629=CARTESIAN_POINT('',(0.,-17.7736741907572,32.7930862494034));
#77630=CARTESIAN_POINT('',(0.,-0.305813997156748,7.84639653186291));
#77631=CARTESIAN_POINT('',(6.93889390390723E-17,36.545659042501,7.46356517686174));
#77632=CARTESIAN_POINT('Origin',(0.,0.,0.));
#77633=CARTESIAN_POINT('',(0.,34.0979246472968,7.24941616595889));
#77634=CARTESIAN_POINT('',(0.,40.0542037481797,7.77052306408252));
#77635=CARTESIAN_POINT('',(0.,34.8387484606519,-1.21823876782095));
#77636=CARTESIAN_POINT('',(0.,34.4247983037968,3.51323317576981));
#77637=CARTESIAN_POINT('',(3.46944695195361E-17,37.2864828558561,-1.0040897569181));
#77638=CARTESIAN_POINT('',(0.,36.1129124805036,-1.10676386061131));
#77639=CARTESIAN_POINT('Origin',(0.,0.,0.));
#77640=CARTESIAN_POINT('',(0.,-34.,-4.163799117101E-15));
#77641=CARTESIAN_POINT('Origin',(0.,0.,0.));
#77642=CARTESIAN_POINT('Origin',(0.249999999999999,0.,0.));
#77643=CARTESIAN_POINT('',(0.499999999999998,-20.3339256786199,-31.8648939508099));
#77644=CARTESIAN_POINT('Origin',(0.499999999999998,0.,0.));
#77645=CARTESIAN_POINT('',(0.200000000000003,-20.1483796152605,-31.6274058196267));
#77646=CARTESIAN_POINT('Ctrl Pts',(0.500000000000002,-20.3339256786199,
-31.8648939508099));
#77647=CARTESIAN_POINT('Ctrl Pts',(0.349396891053132,-20.2407830322278,
-31.74567679996));
#77648=CARTESIAN_POINT('Ctrl Pts',(0.200000000000003,-20.1483796152605,
-31.6274058196267));
#77649=CARTESIAN_POINT('',(0.200000000000009,-22.8288881795131,-29.7504935167013));
#77650=CARTESIAN_POINT('Ctrl Pts',(0.200000000000003,-20.1483796152605,
-31.6274058196267));
#77651=CARTESIAN_POINT('Ctrl Pts',(0.12861382696065,-21.4886338973868,-30.688949668164));
#77652=CARTESIAN_POINT('Ctrl Pts',(0.200000000000009,-22.8288881795131,
-29.7504935167013));
#77653=CARTESIAN_POINT('',(0.499999999999998,-22.9885935327265,-30.0060755079215));
#77654=CARTESIAN_POINT('Ctrl Pts',(0.200000000000009,-22.8288881795131,
-29.7504935167013));
#77655=CARTESIAN_POINT('Ctrl Pts',(0.349396889603209,-22.9084227162985,
-29.8777753821704));
#77656=CARTESIAN_POINT('Ctrl Pts',(0.500000000000002,-22.9885935327265,
-30.0060755079215));
#77657=CARTESIAN_POINT('',(0.499999999999998,-25.5582884235871,-27.8498454727622));
#77658=CARTESIAN_POINT('Origin',(0.499999999999998,0.,0.));
#77659=CARTESIAN_POINT('',(0.200000000000009,-25.3343218406523,-27.6481850557002));
#77660=CARTESIAN_POINT('Ctrl Pts',(0.500000000000002,-25.5582884235871,
-27.8498454727622));
#77661=CARTESIAN_POINT('Ctrl Pts',(0.349396891196147,-25.445858982399,-27.7486135492184));
#77662=CARTESIAN_POINT('Ctrl Pts',(0.200000000000009,-25.3343218406523,
-27.6481850557002));
#77663=CARTESIAN_POINT('',(0.200000000000006,-27.6481850557002,-25.3343218406523));
#77664=CARTESIAN_POINT('Ctrl Pts',(0.200000000000009,-25.3343218406523,
-27.6481850557002));
#77665=CARTESIAN_POINT('Ctrl Pts',(0.128613826960649,-26.4912534481763,
-26.4912534481763));
#77666=CARTESIAN_POINT('Ctrl Pts',(0.200000000000006,-27.6481850557002,
-25.3343218406523));
#77667=CARTESIAN_POINT('',(0.499999999999998,-27.8498454727622,-25.5582884235871));
#77668=CARTESIAN_POINT('Ctrl Pts',(0.200000000000006,-27.6481850557002,
-25.3343218406523));
#77669=CARTESIAN_POINT('Ctrl Pts',(0.349396897552966,-27.7486135534918,
-25.4458589871452));
#77670=CARTESIAN_POINT('Ctrl Pts',(0.500000000000002,-27.8498454727622,
-25.5582884235871));
#77671=CARTESIAN_POINT('',(0.499999999999998,-30.0060755079215,-22.9885935327265));
#77672=CARTESIAN_POINT('Origin',(0.499999999999998,0.,0.));
#77673=CARTESIAN_POINT('',(0.200000000000003,-29.7504935167013,-22.8288881795131));
#77674=CARTESIAN_POINT('Ctrl Pts',(0.500000000000002,-30.0060755079215,
-22.9885935327265));
#77675=CARTESIAN_POINT('Ctrl Pts',(0.349396888618098,-29.8777753813311,
-22.9084227157741));
#77676=CARTESIAN_POINT('Ctrl Pts',(0.200000000000003,-29.7504935167013,
-22.8288881795131));
#77677=CARTESIAN_POINT('',(0.200000000000007,-31.6274058196267,-20.1483796152605));
#77678=CARTESIAN_POINT('Ctrl Pts',(0.200000000000003,-29.7504935167013,
-22.8288881795131));
#77679=CARTESIAN_POINT('Ctrl Pts',(0.128613826960649,-30.688949668164,-21.4886338973868));
#77680=CARTESIAN_POINT('Ctrl Pts',(0.200000000000007,-31.6274058196267,
-20.1483796152605));
#77681=CARTESIAN_POINT('',(0.499999999999998,-31.8648939508099,-20.3339256786199));
#77682=CARTESIAN_POINT('Ctrl Pts',(0.200000000000007,-31.6274058196267,
-20.1483796152605));
#77683=CARTESIAN_POINT('Ctrl Pts',(0.349396887455971,-31.7456767971121,
-20.2407830300028));
#77684=CARTESIAN_POINT('Ctrl Pts',(0.500000000000002,-31.8648939508099,
-20.3339256786199));
#77685=CARTESIAN_POINT('',(0.499999999999998,-33.5421431717545,-17.4288448109885));
#77686=CARTESIAN_POINT('Origin',(0.499999999999998,0.,0.));
#77687=CARTESIAN_POINT('',(0.200000000000004,-33.2627115017215,-17.3159470879662));
#77688=CARTESIAN_POINT('Ctrl Pts',(0.500000000000002,-33.5421431717545,
-17.4288448109885));
#77689=CARTESIAN_POINT('Ctrl Pts',(0.349396892668332,-33.4018706998828,
-17.3721710535896));
#77690=CARTESIAN_POINT('Ctrl Pts',(0.200000000000004,-33.2627115017215,
-17.3159470879662));
#77691=CARTESIAN_POINT('',(0.200000000000004,-34.6456438619633,-14.3502390708311));
#77692=CARTESIAN_POINT('Ctrl Pts',(0.200000000000004,-33.2627115017215,
-17.3159470879662));
#77693=CARTESIAN_POINT('Ctrl Pts',(0.128613826960645,-33.9541776818424,
-15.8330930793986));
#77694=CARTESIAN_POINT('Ctrl Pts',(0.200000000000004,-34.6456438619633,
-14.3502390708311));
#77695=CARTESIAN_POINT('',(0.499999999999998,-34.9117437505765,-14.4917268913708));
#77696=CARTESIAN_POINT('Ctrl Pts',(0.200000000000004,-34.6456438619633,
-14.3502390708311));
#77697=CARTESIAN_POINT('Ctrl Pts',(0.34939689516993,-34.7781637289703,-14.4207011340012));
#77698=CARTESIAN_POINT('Ctrl Pts',(0.500000000000002,-34.9117437505765,
-14.4917268913708));
#77699=CARTESIAN_POINT('',(0.499999999999998,-36.0590497884573,-11.3395294590896));
#77700=CARTESIAN_POINT('Origin',(0.499999999999998,0.,0.));
#77701=CARTESIAN_POINT('',(0.200000000000006,-35.764258829506,-11.2768697064435));
#77702=CARTESIAN_POINT('Ctrl Pts',(0.500000000000002,-36.0590497884573,
-11.3395294590896));
#77703=CARTESIAN_POINT('Ctrl Pts',(0.349396896306784,-35.9110670795055,
-11.3080747632882));
#77704=CARTESIAN_POINT('Ctrl Pts',(0.200000000000006,-35.764258829506,-11.2768697064435));
#77705=CARTESIAN_POINT('',(0.200000000000009,-36.6111915470959,-8.11607377380573));
#77706=CARTESIAN_POINT('Ctrl Pts',(0.200000000000006,-35.764258829506,-11.2768697064435));
#77707=CARTESIAN_POINT('Ctrl Pts',(0.128613826960652,-36.1877251883009,
-9.69647174012461));
#77708=CARTESIAN_POINT('Ctrl Pts',(0.200000000000009,-36.6111915470959,
-8.11607377380573));
#77709=CARTESIAN_POINT('',(0.499999999999998,-36.8978178826767,-8.209204315695));
#77710=CARTESIAN_POINT('Ctrl Pts',(0.200000000000009,-36.6111915470959,
-8.11607377380573));
#77711=CARTESIAN_POINT('Ctrl Pts',(0.349396891239299,-36.753933744661,-8.1624535252782));
#77712=CARTESIAN_POINT('Ctrl Pts',(0.500000000000002,-36.8978178826767,
-8.209204315695));
#77713=CARTESIAN_POINT('',(0.499999999999998,-37.4803204240973,-4.90566824265506));
#77714=CARTESIAN_POINT('Origin',(0.499999999999998,0.,0.));
#77715=CARTESIAN_POINT('',(0.200000000000002,-37.1791272503441,-4.89515034526194));
#77716=CARTESIAN_POINT('Ctrl Pts',(0.500000000000002,-37.4803204240973,
-4.90566824265506));
#77717=CARTESIAN_POINT('Ctrl Pts',(0.349396898001153,-37.3291238561062,
-4.9003883421563));
#77718=CARTESIAN_POINT('Ctrl Pts',(0.200000000000002,-37.1791272503441,
-4.89515034526194));
#77719=CARTESIAN_POINT('',(0.200000000000005,-37.4643267032267,-1.63530568209482));
#77720=CARTESIAN_POINT('Ctrl Pts',(0.200000000000002,-37.1791272503441,
-4.89515034526194));
#77721=CARTESIAN_POINT('Ctrl Pts',(0.128613826960647,-37.3217269767854,
-3.26522801367837));
#77722=CARTESIAN_POINT('Ctrl Pts',(0.200000000000005,-37.4643267032267,
-1.63530568209482));
#77723=CARTESIAN_POINT('',(0.499999999999998,-37.7627704896084,-1.67724922094464));
#77724=CARTESIAN_POINT('Ctrl Pts',(0.200000000000005,-37.4643267032267,
-1.63530568209482));
#77725=CARTESIAN_POINT('Ctrl Pts',(0.34939689448424,-37.6129540886231,-1.65619389889805));
#77726=CARTESIAN_POINT('Ctrl Pts',(0.500000000000002,-37.7627704896084,
-1.67724922094464));
#77727=CARTESIAN_POINT('',(0.499999999999998,-37.7627704896084,1.67724922094466));
#77728=CARTESIAN_POINT('Origin',(0.499999999999998,0.,0.));
#77729=CARTESIAN_POINT('',(0.200000000000009,-37.4643267032267,1.63530568209484));
#77730=CARTESIAN_POINT('Ctrl Pts',(0.500000000000002,-37.7627704896084,
1.67724922094466));
#77731=CARTESIAN_POINT('Ctrl Pts',(0.349396890810879,-37.6129540849685,
1.65619389838445));
#77732=CARTESIAN_POINT('Ctrl Pts',(0.200000000000009,-37.4643267032267,
1.63530568209484));
#77733=CARTESIAN_POINT('',(0.200000000000002,-37.1791272503441,4.89515034526196));
#77734=CARTESIAN_POINT('Ctrl Pts',(0.200000000000009,-37.4643267032267,
1.63530568209484));
#77735=CARTESIAN_POINT('Ctrl Pts',(0.128613826960646,-37.3217269767854,
3.2652280136784));
#77736=CARTESIAN_POINT('Ctrl Pts',(0.200000000000002,-37.1791272503441,
4.89515034526196));
#77737=CARTESIAN_POINT('',(0.499999999999998,-37.4803204240973,4.90566824265508));
#77738=CARTESIAN_POINT('Ctrl Pts',(0.200000000000002,-37.1791272503441,
4.89515034526196));
#77739=CARTESIAN_POINT('Ctrl Pts',(0.349396890635592,-37.3291238487107,
4.90038834189806));
#77740=CARTESIAN_POINT('Ctrl Pts',(0.500000000000002,-37.4803204240973,
4.90566824265508));
#77741=CARTESIAN_POINT('',(0.499999999999998,-36.8978178826767,8.20920431569502));
#77742=CARTESIAN_POINT('Origin',(0.499999999999998,0.,0.));
#77743=CARTESIAN_POINT('',(0.200000000000009,-36.6111915470959,8.11607377380575));
#77744=CARTESIAN_POINT('Ctrl Pts',(0.500000000000001,-36.8978178826767,
8.20920431569502));
#77745=CARTESIAN_POINT('Ctrl Pts',(0.349396891227683,-36.7539337446499,
8.16245352527461));
#77746=CARTESIAN_POINT('Ctrl Pts',(0.200000000000009,-36.6111915470959,
8.11607377380575));
#77747=CARTESIAN_POINT('',(0.20000000000001,-35.764258829506,11.2768697064435));
#77748=CARTESIAN_POINT('Ctrl Pts',(0.200000000000009,-36.6111915470959,
8.11607377380575));
#77749=CARTESIAN_POINT('Ctrl Pts',(0.12861382696065,-36.1877251883009,9.69647174012464));
#77750=CARTESIAN_POINT('Ctrl Pts',(0.20000000000001,-35.764258829506,11.2768697064435));
#77751=CARTESIAN_POINT('',(0.499999999999998,-36.0590497884572,11.3395294590896));
#77752=CARTESIAN_POINT('Ctrl Pts',(0.20000000000001,-35.764258829506,11.2768697064435));
#77753=CARTESIAN_POINT('Ctrl Pts',(0.349396892541906,-35.9110670758057,
11.3080747625018));
#77754=CARTESIAN_POINT('Ctrl Pts',(0.500000000000002,-36.0590497884573,
11.3395294590896));
#77755=CARTESIAN_POINT('',(0.499999999999998,-34.9117437505765,14.4917268913708));
#77756=CARTESIAN_POINT('Origin',(0.499999999999998,0.,0.));
#77757=CARTESIAN_POINT('',(0.200000000000008,-34.6456438619633,14.3502390708311));
#77758=CARTESIAN_POINT('Ctrl Pts',(0.500000000000001,-34.9117437505765,
14.4917268913708));
#77759=CARTESIAN_POINT('Ctrl Pts',(0.349396895264272,-34.778163729054,14.4207011340457));
#77760=CARTESIAN_POINT('Ctrl Pts',(0.200000000000008,-34.6456438619633,
14.3502390708311));
#77761=CARTESIAN_POINT('',(0.200000000000004,-33.2627115017215,17.3159470879662));
#77762=CARTESIAN_POINT('Ctrl Pts',(0.200000000000008,-34.6456438619633,
14.3502390708311));
#77763=CARTESIAN_POINT('Ctrl Pts',(0.128613826960644,-33.9541776818424,
15.8330930793986));
#77764=CARTESIAN_POINT('Ctrl Pts',(0.200000000000004,-33.2627115017215,
17.3159470879662));
#77765=CARTESIAN_POINT('',(0.499999999999998,-33.5421431717545,17.4288448109885));
#77766=CARTESIAN_POINT('Ctrl Pts',(0.200000000000004,-33.2627115017215,
17.3159470879662));
#77767=CARTESIAN_POINT('Ctrl Pts',(0.349396887767451,-33.4018706953176,
17.3721710517451));
#77768=CARTESIAN_POINT('Ctrl Pts',(0.500000000000001,-33.5421431717545,
17.4288448109885));
#77769=CARTESIAN_POINT('',(0.499999999999998,-31.8648939508099,20.3339256786199));
#77770=CARTESIAN_POINT('Origin',(0.499999999999998,0.,0.));
#77771=CARTESIAN_POINT('',(0.200000000000003,-31.6274058196267,20.1483796152605));
#77772=CARTESIAN_POINT('Ctrl Pts',(0.500000000000001,-31.8648939508099,
20.3339256786199));
#77773=CARTESIAN_POINT('Ctrl Pts',(0.349396891074454,-31.7456767999768,
20.240783032241));
#77774=CARTESIAN_POINT('Ctrl Pts',(0.200000000000003,-31.6274058196267,
20.1483796152605));
#77775=CARTESIAN_POINT('',(0.200000000000009,-29.7504935167013,22.8288881795131));
#77776=CARTESIAN_POINT('Ctrl Pts',(0.200000000000003,-31.6274058196267,
20.1483796152605));
#77777=CARTESIAN_POINT('Ctrl Pts',(0.128613826960651,-30.688949668164,21.4886338973868));
#77778=CARTESIAN_POINT('Ctrl Pts',(0.200000000000009,-29.7504935167013,
22.8288881795131));
#77779=CARTESIAN_POINT('',(0.499999999999998,-30.0060755079215,22.9885935327265));
#77780=CARTESIAN_POINT('Ctrl Pts',(0.200000000000009,-29.7504935167013,
22.8288881795131));
#77781=CARTESIAN_POINT('Ctrl Pts',(0.349396889570691,-29.8777753821427,
22.9084227162812));
#77782=CARTESIAN_POINT('Ctrl Pts',(0.500000000000001,-30.0060755079215,
22.9885935327265));
#77783=CARTESIAN_POINT('',(0.499999999999998,-27.8498454727622,25.5582884235871));
#77784=CARTESIAN_POINT('Origin',(0.499999999999998,0.,0.));
#77785=CARTESIAN_POINT('',(0.200000000000006,-27.6481850557002,25.3343218406523));
#77786=CARTESIAN_POINT('Ctrl Pts',(0.500000000000001,-27.8498454727622,
25.5582884235871));
#77787=CARTESIAN_POINT('Ctrl Pts',(0.349396893632768,-27.7486135508564,
25.4458589842183));
#77788=CARTESIAN_POINT('Ctrl Pts',(0.200000000000006,-27.6481850557002,
25.3343218406523));
#77789=CARTESIAN_POINT('',(0.200000000000006,-25.3343218406523,27.6481850557002));
#77790=CARTESIAN_POINT('Ctrl Pts',(0.200000000000006,-27.6481850557002,
25.3343218406523));
#77791=CARTESIAN_POINT('Ctrl Pts',(0.128613826960647,-26.4912534481763,
26.4912534481763));
#77792=CARTESIAN_POINT('Ctrl Pts',(0.200000000000006,-25.3343218406523,
27.6481850557002));
#77793=CARTESIAN_POINT('',(0.499999999999998,-25.5582884235871,27.8498454727622));
#77794=CARTESIAN_POINT('Ctrl Pts',(0.200000000000006,-25.3343218406523,
27.6481850557002));
#77795=CARTESIAN_POINT('Ctrl Pts',(0.349396893895724,-25.4458589844146,
27.7486135510332));
#77796=CARTESIAN_POINT('Ctrl Pts',(0.500000000000001,-25.5582884235871,
27.8498454727622));
#77797=CARTESIAN_POINT('',(0.499999999999998,-25.0251096245113,28.3299115473591));
#77798=CARTESIAN_POINT('Origin',(0.499999999999998,0.,0.));
#77799=CARTESIAN_POINT('Ctrl Pts',(0.500000000000004,-25.0251096245113,
28.3299115473591));
#77800=CARTESIAN_POINT('Ctrl Pts',(0.248313951856147,-24.8798272328718,
28.1224267893243));
#77801=CARTESIAN_POINT('Ctrl Pts',(-2.08166817117217E-16,-24.7364665672137,
27.9176865404195));
#77802=CARTESIAN_POINT('Origin',(0.249999999999999,0.,0.));
#77803=CARTESIAN_POINT('',(0.499999999999998,37.7878017125899,-0.960230040142118));
#77804=CARTESIAN_POINT('Ctrl Pts',(1.04083408558608E-16,37.2864828558561,
-1.0040897569181));
#77805=CARTESIAN_POINT('Ctrl Pts',(0.248313954120435,37.5354734476842,-0.982305902808531));
#77806=CARTESIAN_POINT('Ctrl Pts',(0.500000000000005,37.7878017125899,-0.960230040142117));
#77807=CARTESIAN_POINT('',(0.499999999999998,37.7627704896084,-1.67724922094465));
#77808=CARTESIAN_POINT('Origin',(0.499999999999998,0.,0.));
#77809=CARTESIAN_POINT('',(0.200000000000005,37.4643267032267,-1.63530568209483));
#77810=CARTESIAN_POINT('Ctrl Pts',(0.500000000000005,37.7627704896084,-1.67724922094465));
#77811=CARTESIAN_POINT('Ctrl Pts',(0.349396890677128,37.6129540848354,-1.65619389836574));
#77812=CARTESIAN_POINT('Ctrl Pts',(0.200000000000005,37.4643267032267,-1.63530568209483));
#77813=CARTESIAN_POINT('',(0.200000000000002,37.1791272503441,-4.89515034526195));
#77814=CARTESIAN_POINT('Ctrl Pts',(0.200000000000005,37.4643267032267,-1.63530568209483));
#77815=CARTESIAN_POINT('Ctrl Pts',(0.128613826960643,37.3217269767854,-3.26522801367839));
#77816=CARTESIAN_POINT('Ctrl Pts',(0.200000000000002,37.1791272503441,-4.89515034526195));
#77817=CARTESIAN_POINT('',(0.499999999999998,37.4803204240973,-4.90566824265507));
#77818=CARTESIAN_POINT('Ctrl Pts',(0.200000000000002,37.1791272503441,-4.89515034526194));
#77819=CARTESIAN_POINT('Ctrl Pts',(0.349396890484736,37.3291238485592,-4.90038834189276));
#77820=CARTESIAN_POINT('Ctrl Pts',(0.500000000000004,37.4803204240973,-4.90566824265507));
#77821=CARTESIAN_POINT('',(0.499999999999998,36.8978178826767,-8.20920431569504));
#77822=CARTESIAN_POINT('Origin',(0.499999999999998,0.,0.));
#77823=CARTESIAN_POINT('',(0.200000000000008,36.6111915470958,-8.11607377380577));
#77824=CARTESIAN_POINT('Ctrl Pts',(0.500000000000004,36.8978178826767,-8.20920431569504));
#77825=CARTESIAN_POINT('Ctrl Pts',(0.349396891393874,36.7539337448086,-8.16245352532623));
#77826=CARTESIAN_POINT('Ctrl Pts',(0.200000000000008,36.6111915470958,-8.11607377380577));
#77827=CARTESIAN_POINT('',(0.200000000000001,35.764258829506,-11.2768697064435));
#77828=CARTESIAN_POINT('Ctrl Pts',(0.200000000000008,36.6111915470958,-8.11607377380577));
#77829=CARTESIAN_POINT('Ctrl Pts',(0.128613826960642,36.1877251883009,-9.69647174012466));
#77830=CARTESIAN_POINT('Ctrl Pts',(0.200000000000001,35.764258829506,-11.2768697064435));
#77831=CARTESIAN_POINT('',(0.499999999999998,36.0590497884572,-11.3395294590896));
#77832=CARTESIAN_POINT('Ctrl Pts',(0.200000000000001,35.764258829506,-11.2768697064435));
#77833=CARTESIAN_POINT('Ctrl Pts',(0.349396888726257,35.911067072056,-11.3080747617048));
#77834=CARTESIAN_POINT('Ctrl Pts',(0.500000000000004,36.0590497884572,-11.3395294590896));
#77835=CARTESIAN_POINT('',(0.499999999999998,34.9117437505765,-14.4917268913708));
#77836=CARTESIAN_POINT('Origin',(0.499999999999998,0.,0.));
#77837=CARTESIAN_POINT('',(0.200000000000003,34.6456438619633,-14.3502390708311));
#77838=CARTESIAN_POINT('Ctrl Pts',(0.500000000000004,34.9117437505765,-14.4917268913708));
#77839=CARTESIAN_POINT('Ctrl Pts',(0.349396890191469,34.7781637245541,-14.4207011316531));
#77840=CARTESIAN_POINT('Ctrl Pts',(0.200000000000003,34.6456438619633,-14.3502390708311));
#77841=CARTESIAN_POINT('',(0.200000000000004,33.2627115017215,-17.3159470879662));
#77842=CARTESIAN_POINT('Ctrl Pts',(0.200000000000003,34.6456438619633,-14.3502390708311));
#77843=CARTESIAN_POINT('Ctrl Pts',(0.128613826960647,33.9541776818424,-15.8330930793987));
#77844=CARTESIAN_POINT('Ctrl Pts',(0.200000000000004,33.2627115017215,-17.3159470879662));
#77845=CARTESIAN_POINT('',(0.499999999999998,33.5421431717545,-17.4288448109885));
#77846=CARTESIAN_POINT('Ctrl Pts',(0.200000000000004,33.2627115017215,-17.3159470879662));
#77847=CARTESIAN_POINT('Ctrl Pts',(0.349396888098001,33.4018706956255,-17.3721710518695));
#77848=CARTESIAN_POINT('Ctrl Pts',(0.500000000000004,33.5421431717545,-17.4288448109885));
#77849=CARTESIAN_POINT('',(0.499999999999998,31.8648939508099,-20.3339256786199));
#77850=CARTESIAN_POINT('Origin',(0.499999999999998,0.,0.));
#77851=CARTESIAN_POINT('',(0.199999999999999,31.6274058196267,-20.1483796152605));
#77852=CARTESIAN_POINT('Ctrl Pts',(0.500000000000004,31.8648939508099,-20.3339256786199));
#77853=CARTESIAN_POINT('Ctrl Pts',(0.349396893153553,31.7456768016228,-20.240783033527));
#77854=CARTESIAN_POINT('Ctrl Pts',(0.199999999999999,31.6274058196267,-20.1483796152605));
#77855=CARTESIAN_POINT('',(0.200000000000003,29.7504935167013,-22.8288881795131));
#77856=CARTESIAN_POINT('Ctrl Pts',(0.199999999999999,31.6274058196267,-20.1483796152605));
#77857=CARTESIAN_POINT('Ctrl Pts',(0.128613826960646,30.688949668164,-21.4886338973868));
#77858=CARTESIAN_POINT('Ctrl Pts',(0.200000000000003,29.7504935167013,-22.8288881795131));
#77859=CARTESIAN_POINT('',(0.499999999999998,30.0060755079215,-22.9885935327265));
#77860=CARTESIAN_POINT('Ctrl Pts',(0.200000000000003,29.7504935167013,-22.8288881795131));
#77861=CARTESIAN_POINT('Ctrl Pts',(0.34939689381316,29.8777753857573,-22.9084227185399));
#77862=CARTESIAN_POINT('Ctrl Pts',(0.500000000000003,30.0060755079215,-22.9885935327265));
#77863=CARTESIAN_POINT('',(0.499999999999998,27.8498454727622,-25.5582884235871));
#77864=CARTESIAN_POINT('Origin',(0.499999999999998,0.,0.));
#77865=CARTESIAN_POINT('',(0.2,27.6481850557002,-25.3343218406523));
#77866=CARTESIAN_POINT('Ctrl Pts',(0.500000000000003,27.8498454727622,-25.5582884235871));
#77867=CARTESIAN_POINT('Ctrl Pts',(0.34939689386556,27.7486135510129,-25.4458589843921));
#77868=CARTESIAN_POINT('Ctrl Pts',(0.2,27.6481850557002,-25.3343218406523));
#77869=CARTESIAN_POINT('',(0.200000000000006,25.3343218406523,-27.6481850557003));
#77870=CARTESIAN_POINT('Ctrl Pts',(0.2,27.6481850557002,-25.3343218406523));
#77871=CARTESIAN_POINT('Ctrl Pts',(0.128613826960646,26.4912534481763,-26.4912534481763));
#77872=CARTESIAN_POINT('Ctrl Pts',(0.200000000000006,25.3343218406523,-27.6481850557003));
#77873=CARTESIAN_POINT('',(0.499999999999998,25.5582884235871,-27.8498454727622));
#77874=CARTESIAN_POINT('Ctrl Pts',(0.200000000000006,25.3343218406523,-27.6481850557003));
#77875=CARTESIAN_POINT('Ctrl Pts',(0.34939689385293,25.4458589843826,-27.7486135510044));
#77876=CARTESIAN_POINT('Ctrl Pts',(0.500000000000003,25.5582884235871,-27.8498454727622));
#77877=CARTESIAN_POINT('',(0.499999999999998,22.9885935327265,-30.0060755079215));
#77878=CARTESIAN_POINT('Origin',(0.499999999999998,0.,0.));
#77879=CARTESIAN_POINT('',(0.200000000000003,22.8288881795131,-29.7504935167013));
#77880=CARTESIAN_POINT('Ctrl Pts',(0.500000000000003,22.9885935327265,-30.0060755079215));
#77881=CARTESIAN_POINT('Ctrl Pts',(0.349396892499578,22.9084227178406,-29.8777753846381));
#77882=CARTESIAN_POINT('Ctrl Pts',(0.200000000000003,22.8288881795131,-29.7504935167013));
#77883=CARTESIAN_POINT('',(0.200000000000009,20.1483796152605,-31.6274058196267));
#77884=CARTESIAN_POINT('Ctrl Pts',(0.200000000000003,22.8288881795131,-29.7504935167013));
#77885=CARTESIAN_POINT('Ctrl Pts',(0.128613826960651,21.4886338973868,-30.688949668164));
#77886=CARTESIAN_POINT('Ctrl Pts',(0.200000000000009,20.1483796152605,-31.6274058196267));
#77887=CARTESIAN_POINT('',(0.499999999999998,20.3339256786199,-31.8648939508099));
#77888=CARTESIAN_POINT('Ctrl Pts',(0.200000000000009,20.1483796152605,-31.6274058196267));
#77889=CARTESIAN_POINT('Ctrl Pts',(0.349396892229315,20.2407830329553,-31.7456768008911));
#77890=CARTESIAN_POINT('Ctrl Pts',(0.500000000000003,20.3339256786199,-31.8648939508099));
#77891=CARTESIAN_POINT('',(0.499999999999998,17.4288448109885,-33.5421431717545));
#77892=CARTESIAN_POINT('Origin',(0.499999999999998,0.,0.));
#77893=CARTESIAN_POINT('',(0.200000000000008,17.3159470879662,-33.2627115017215));
#77894=CARTESIAN_POINT('Ctrl Pts',(0.500000000000003,17.4288448109885,-33.5421431717546));
#77895=CARTESIAN_POINT('Ctrl Pts',(0.349396892187316,17.3721710534085,-33.4018706994348));
#77896=CARTESIAN_POINT('Ctrl Pts',(0.200000000000008,17.3159470879662,-33.2627115017215));
#77897=CARTESIAN_POINT('',(0.200000000000009,14.350239070831,-34.6456438619633));
#77898=CARTESIAN_POINT('Ctrl Pts',(0.200000000000008,17.3159470879662,-33.2627115017215));
#77899=CARTESIAN_POINT('Ctrl Pts',(0.128613826960651,15.8330930793986,-33.9541776818424));
#77900=CARTESIAN_POINT('Ctrl Pts',(0.200000000000009,14.350239070831,-34.6456438619633));
#77901=CARTESIAN_POINT('',(0.499999999999998,14.4917268913708,-34.9117437505765));
#77902=CARTESIAN_POINT('Ctrl Pts',(0.200000000000009,14.350239070831,-34.6456438619633));
#77903=CARTESIAN_POINT('Ctrl Pts',(0.349396890607192,14.4207011318491,-34.7781637249228));
#77904=CARTESIAN_POINT('Ctrl Pts',(0.500000000000003,14.4917268913708,-34.9117437505765));
#77905=CARTESIAN_POINT('',(0.499999999999998,11.3395294590896,-36.0590497884573));
#77906=CARTESIAN_POINT('Origin',(0.499999999999998,0.,0.));
#77907=CARTESIAN_POINT('',(0.200000000000006,11.2768697064435,-35.764258829506));
#77908=CARTESIAN_POINT('Ctrl Pts',(0.500000000000003,11.3395294590896,-36.0590497884573));
#77909=CARTESIAN_POINT('Ctrl Pts',(0.349396892569828,11.3080747625076,-35.9110670758332));
#77910=CARTESIAN_POINT('Ctrl Pts',(0.200000000000006,11.2768697064435,-35.764258829506));
#77911=CARTESIAN_POINT('',(0.200000000000008,8.11607377380573,-36.6111915470959));
#77912=CARTESIAN_POINT('Ctrl Pts',(0.200000000000006,11.2768697064435,-35.764258829506));
#77913=CARTESIAN_POINT('Ctrl Pts',(0.128613826960652,9.69647174012461,-36.1877251883009));
#77914=CARTESIAN_POINT('Ctrl Pts',(0.200000000000009,8.11607377380573,-36.6111915470959));
#77915=CARTESIAN_POINT('',(0.499999999999998,8.209204315695,-36.8978178826767));
#77916=CARTESIAN_POINT('Ctrl Pts',(0.200000000000008,8.11607377380573,-36.6111915470959));
#77917=CARTESIAN_POINT('Ctrl Pts',(0.349396891147052,8.16245352524956,-36.7539337445728));
#77918=CARTESIAN_POINT('Ctrl Pts',(0.500000000000003,8.209204315695,-36.8978178826767));
#77919=CARTESIAN_POINT('',(0.499999999999998,4.90566824265506,-37.4803204240973));
#77920=CARTESIAN_POINT('Origin',(0.499999999999998,0.,0.));
#77921=CARTESIAN_POINT('',(0.200000000000002,4.89515034526193,-37.1791272503441));
#77922=CARTESIAN_POINT('Ctrl Pts',(0.500000000000003,4.90566824265506,-37.4803204240973));
#77923=CARTESIAN_POINT('Ctrl Pts',(0.349396890683097,4.90038834189971,-37.3291238487584));
#77924=CARTESIAN_POINT('Ctrl Pts',(0.200000000000002,4.89515034526193,-37.1791272503441));
#77925=CARTESIAN_POINT('',(0.200000000000005,1.63530568209482,-37.4643267032267));
#77926=CARTESIAN_POINT('Ctrl Pts',(0.200000000000002,4.89515034526193,-37.1791272503441));
#77927=CARTESIAN_POINT('Ctrl Pts',(0.128613826960647,3.26522801367837,-37.3217269767854));
#77928=CARTESIAN_POINT('Ctrl Pts',(0.200000000000005,1.63530568209482,-37.4643267032267));
#77929=CARTESIAN_POINT('',(0.499999999999998,1.67724922094464,-37.7627704896084));
#77930=CARTESIAN_POINT('Ctrl Pts',(0.200000000000005,1.63530568209482,-37.4643267032267));
#77931=CARTESIAN_POINT('Ctrl Pts',(0.34939689445096,1.6561938988934,-37.61295408859));
#77932=CARTESIAN_POINT('Ctrl Pts',(0.500000000000003,1.67724922094464,-37.7627704896084));
#77933=CARTESIAN_POINT('',(0.499999999999998,-1.67724922094465,-37.7627704896084));
#77934=CARTESIAN_POINT('Origin',(0.499999999999998,0.,0.));
#77935=CARTESIAN_POINT('',(0.200000000000005,-1.63530568209482,-37.4643267032267));
#77936=CARTESIAN_POINT('Ctrl Pts',(0.500000000000003,-1.67724922094465,
-37.7627704896084));
#77937=CARTESIAN_POINT('Ctrl Pts',(0.349396890783986,-1.65619389838068,
-37.6129540849417));
#77938=CARTESIAN_POINT('Ctrl Pts',(0.200000000000005,-1.63530568209482,
-37.4643267032267));
#77939=CARTESIAN_POINT('',(0.200000000000002,-4.89515034526194,-37.1791272503441));
#77940=CARTESIAN_POINT('Ctrl Pts',(0.200000000000005,-1.63530568209482,
-37.4643267032267));
#77941=CARTESIAN_POINT('Ctrl Pts',(0.128613826960644,-3.26522801367839,
-37.3217269767854));
#77942=CARTESIAN_POINT('Ctrl Pts',(0.200000000000002,-4.89515034526194,
-37.1791272503441));
#77943=CARTESIAN_POINT('',(0.499999999999998,-4.90566824265507,-37.4803204240973));
#77944=CARTESIAN_POINT('Ctrl Pts',(0.200000000000002,-4.89515034526194,
-37.1791272503441));
#77945=CARTESIAN_POINT('Ctrl Pts',(0.349396894243145,-4.90038834202454,
-37.3291238523329));
#77946=CARTESIAN_POINT('Ctrl Pts',(0.500000000000003,-4.90566824265507,
-37.4803204240973));
#77947=CARTESIAN_POINT('',(0.499999999999998,-8.20920431569503,-36.8978178826767));
#77948=CARTESIAN_POINT('Origin',(0.499999999999998,0.,0.));
#77949=CARTESIAN_POINT('',(0.200000000000013,-8.11607377380577,-36.6111915470959));
#77950=CARTESIAN_POINT('Ctrl Pts',(0.500000000000003,-8.20920431569504,
-36.8978178826767));
#77951=CARTESIAN_POINT('Ctrl Pts',(0.349396891427038,-8.16245352533653,
-36.7539337448403));
#77952=CARTESIAN_POINT('Ctrl Pts',(0.200000000000013,-8.11607377380577,
-36.6111915470959));
#77953=CARTESIAN_POINT('',(0.200000000000006,-11.2768697064435,-35.764258829506));
#77954=CARTESIAN_POINT('Ctrl Pts',(0.200000000000013,-8.11607377380577,
-36.6111915470959));
#77955=CARTESIAN_POINT('Ctrl Pts',(0.12861382696065,-9.69647174012466,-36.1877251883009));
#77956=CARTESIAN_POINT('Ctrl Pts',(0.200000000000006,-11.2768697064435,
-35.764258829506));
#77957=CARTESIAN_POINT('Ctrl Pts',(0.200000000000006,-11.2768697064435,
-35.764258829506));
#77958=CARTESIAN_POINT('Ctrl Pts',(0.349396892466969,-11.3080747624862,
-35.9110670757321));
#77959=CARTESIAN_POINT('Ctrl Pts',(0.500000000000002,-11.3395294590896,
-36.0590497884572));
#77960=CARTESIAN_POINT('Origin',(0.,-28.7187593876742,33.6049900942237));
#77961=CARTESIAN_POINT('',(22.,-23.3271408859744,25.9049608779072));
#77962=CARTESIAN_POINT('',(22.,-10.5072490062194,7.59625784318566));
#77963=CARTESIAN_POINT('',(0.,-23.3271408859744,25.9049608779072));
#77964=CARTESIAN_POINT('',(11.,-25.0251096245113,28.3299115473591));
#77965=CARTESIAN_POINT('Origin',(0.,-16.364348509518,30.7803605868911));
#77966=CARTESIAN_POINT('',(21.5,-18.0623172480549,33.205311256343));
#77967=CARTESIAN_POINT('',(22.,-17.7736741907572,32.7930862494034));
#77968=CARTESIAN_POINT('Ctrl Pts',(21.5,-18.0623172480549,33.205311256343));
#77969=CARTESIAN_POINT('Ctrl Pts',(21.7516860460885,-17.9170348576018,32.9978265000027));
#77970=CARTESIAN_POINT('Ctrl Pts',(22.,-17.7736741907572,32.7930862494034));
#77971=CARTESIAN_POINT('',(0.499999999999998,-18.0623172480549,33.205311256343));
#77972=CARTESIAN_POINT('',(11.,-18.0623172480549,33.205311256343));
#77973=CARTESIAN_POINT('Ctrl Pts',(3.12250225675825E-16,-17.7736741907572,
32.7930862494034));
#77974=CARTESIAN_POINT('Ctrl Pts',(0.248313958347431,-17.9170348601627,
32.99782650366));
#77975=CARTESIAN_POINT('Ctrl Pts',(0.500000000000005,-18.0623172480549,
33.205311256343));
#77976=CARTESIAN_POINT('',(22.,-16.364348509518,30.7803605868911));
#77977=CARTESIAN_POINT('',(0.,-16.364348509518,30.7803605868911));
#77978=CARTESIAN_POINT('',(22.,-0.848647378913067,8.62164294401129));
#77979=CARTESIAN_POINT('Origin',(0.,-23.3271408859744,25.9049608779072));
#77980=CARTESIAN_POINT('',(22.,-10.1792715735921,35.1111980818334));
#77981=CARTESIAN_POINT('Origin',(21.75,0.,0.));
#77982=CARTESIAN_POINT('',(22.,36.545659042501,7.46356517686174));
#77983=CARTESIAN_POINT('Origin',(22.,0.,0.));
#77984=CARTESIAN_POINT('',(21.5,37.0469778992348,7.50742489363772));
#77985=CARTESIAN_POINT('Ctrl Pts',(22.,36.545659042501,7.46356517686174));
#77986=CARTESIAN_POINT('Ctrl Pts',(21.7516860406108,36.7946496396117,7.48534903143347));
#77987=CARTESIAN_POINT('Ctrl Pts',(21.5,37.0469778992348,7.50742489363772));
#77988=CARTESIAN_POINT('',(21.5,36.8978178826767,8.20920431569501));
#77989=CARTESIAN_POINT('Origin',(21.5,0.,0.));
#77990=CARTESIAN_POINT('',(21.8,36.6111915470959,8.11607377380574));
#77991=CARTESIAN_POINT('Ctrl Pts',(21.5,36.8978178826767,8.20920431569501));
#77992=CARTESIAN_POINT('Ctrl Pts',(21.6506031085866,36.7539337448273,8.16245352533225));
#77993=CARTESIAN_POINT('Ctrl Pts',(21.8,36.6111915470959,8.11607377380574));
#77994=CARTESIAN_POINT('',(21.8,35.764258829506,11.2768697064435));
#77995=CARTESIAN_POINT('Ctrl Pts',(21.8,36.6111915470959,8.11607377380574));
#77996=CARTESIAN_POINT('Ctrl Pts',(21.8713861730393,36.1877251883009,9.69647174012463));
#77997=CARTESIAN_POINT('Ctrl Pts',(21.8,35.764258829506,11.2768697064435));
#77998=CARTESIAN_POINT('',(21.5,36.0590497884573,11.3395294590896));
#77999=CARTESIAN_POINT('Ctrl Pts',(21.8,35.764258829506,11.2768697064435));
#78000=CARTESIAN_POINT('Ctrl Pts',(21.6506031072715,35.9110670759891,11.3080747625408));
#78001=CARTESIAN_POINT('Ctrl Pts',(21.5,36.0590497884573,11.3395294590896));
#78002=CARTESIAN_POINT('',(21.5,34.9117437505765,14.4917268913708));
#78003=CARTESIAN_POINT('Origin',(21.5,0.,0.));
#78004=CARTESIAN_POINT('',(21.8,34.6456438619633,14.3502390708311));
#78005=CARTESIAN_POINT('Ctrl Pts',(21.5,34.9117437505765,14.4917268913708));
#78006=CARTESIAN_POINT('Ctrl Pts',(21.6506031059505,34.7781637279764,14.4207011334727));
#78007=CARTESIAN_POINT('Ctrl Pts',(21.8,34.6456438619633,14.3502390708311));
#78008=CARTESIAN_POINT('',(21.8,33.2627115017215,17.3159470879662));
#78009=CARTESIAN_POINT('Ctrl Pts',(21.8,34.6456438619633,14.3502390708311));
#78010=CARTESIAN_POINT('Ctrl Pts',(21.8713861730394,33.9541776818424,15.8330930793986));
#78011=CARTESIAN_POINT('Ctrl Pts',(21.8,33.2627115017215,17.3159470879662));
#78012=CARTESIAN_POINT('',(21.5,33.5421431717545,17.4288448109885));
#78013=CARTESIAN_POINT('Ctrl Pts',(21.8,33.2627115017215,17.3159470879662));
#78014=CARTESIAN_POINT('Ctrl Pts',(21.650603107741,33.4018706995015,17.3721710534355));
#78015=CARTESIAN_POINT('Ctrl Pts',(21.5,33.5421431717545,17.4288448109885));
#78016=CARTESIAN_POINT('',(21.5,31.8648939508099,20.3339256786199));
#78017=CARTESIAN_POINT('Origin',(21.5,0.,0.));
#78018=CARTESIAN_POINT('',(21.8,31.6274058196267,20.1483796152605));
#78019=CARTESIAN_POINT('Ctrl Pts',(21.5,31.8648939508099,20.3339256786199));
#78020=CARTESIAN_POINT('Ctrl Pts',(21.6506031088134,31.7456768000656,20.2407830323103));
#78021=CARTESIAN_POINT('Ctrl Pts',(21.8,31.6274058196267,20.1483796152605));
#78022=CARTESIAN_POINT('',(21.8,29.7504935167013,22.8288881795131));
#78023=CARTESIAN_POINT('Ctrl Pts',(21.8,31.6274058196267,20.1483796152605));
#78024=CARTESIAN_POINT('Ctrl Pts',(21.8713861730394,30.688949668164,21.4886338973868));
#78025=CARTESIAN_POINT('Ctrl Pts',(21.8,29.7504935167013,22.8288881795131));
#78026=CARTESIAN_POINT('',(21.5,30.0060755079215,22.9885935327265));
#78027=CARTESIAN_POINT('Ctrl Pts',(21.8,29.7504935167013,22.8288881795131));
#78028=CARTESIAN_POINT('Ctrl Pts',(21.6506031101081,29.8777753824163,22.9084227164522));
#78029=CARTESIAN_POINT('Ctrl Pts',(21.5,30.0060755079215,22.9885935327265));
#78030=CARTESIAN_POINT('',(21.5,27.8498454727622,25.5582884235871));
#78031=CARTESIAN_POINT('Origin',(21.5,0.,0.));
#78032=CARTESIAN_POINT('',(21.8,27.6481850557002,25.3343218406523));
#78033=CARTESIAN_POINT('Ctrl Pts',(21.5,27.8498454727622,25.5582884235871));
#78034=CARTESIAN_POINT('Ctrl Pts',(21.6506031063136,27.7486135508925,25.4458589842583));
#78035=CARTESIAN_POINT('Ctrl Pts',(21.8,27.6481850557002,25.3343218406523));
#78036=CARTESIAN_POINT('',(21.8,25.3343218406523,27.6481850557002));
#78037=CARTESIAN_POINT('Ctrl Pts',(21.8,27.6481850557002,25.3343218406523));
#78038=CARTESIAN_POINT('Ctrl Pts',(21.8713861730393,26.4912534481763,26.4912534481763));
#78039=CARTESIAN_POINT('Ctrl Pts',(21.8,25.3343218406523,27.6481850557002));
#78040=CARTESIAN_POINT('',(21.5,25.5582884235871,27.8498454727622));
#78041=CARTESIAN_POINT('Ctrl Pts',(21.8,25.3343218406523,27.6481850557002));
#78042=CARTESIAN_POINT('Ctrl Pts',(21.6506031088795,25.4458589823425,27.7486135491675));
#78043=CARTESIAN_POINT('Ctrl Pts',(21.5,25.5582884235871,27.8498454727622));
#78044=CARTESIAN_POINT('',(21.5,22.9885935327265,30.0060755079215));
#78045=CARTESIAN_POINT('Origin',(21.5,0.,0.));
#78046=CARTESIAN_POINT('',(21.8,22.8288881795131,29.7504935167013));
#78047=CARTESIAN_POINT('Ctrl Pts',(21.5,22.9885935327265,30.0060755079215));
#78048=CARTESIAN_POINT('Ctrl Pts',(21.6506031143833,22.9084227141762,29.8777753787739));
#78049=CARTESIAN_POINT('Ctrl Pts',(21.8,22.8288881795131,29.7504935167013));
#78050=CARTESIAN_POINT('',(21.8,20.1483796152605,31.6274058196267));
#78051=CARTESIAN_POINT('Ctrl Pts',(21.8,22.8288881795131,29.7504935167013));
#78052=CARTESIAN_POINT('Ctrl Pts',(21.8713861730394,21.4886338973868,30.688949668164));
#78053=CARTESIAN_POINT('Ctrl Pts',(21.8,20.1483796152605,31.6274058196267));
#78054=CARTESIAN_POINT('',(21.5,20.3339256786199,31.8648939508099));
#78055=CARTESIAN_POINT('Ctrl Pts',(21.8,20.1483796152605,31.6274058196267));
#78056=CARTESIAN_POINT('Ctrl Pts',(21.6506031061559,20.2407830339541,31.7456768021696));
#78057=CARTESIAN_POINT('Ctrl Pts',(21.5,20.3339256786199,31.8648939508099));
#78058=CARTESIAN_POINT('',(21.5,17.4288448109885,33.5421431717545));
#78059=CARTESIAN_POINT('Origin',(21.5,0.,0.));
#78060=CARTESIAN_POINT('',(21.8,17.3159470879662,33.2627115017215));
#78061=CARTESIAN_POINT('Ctrl Pts',(21.5,17.4288448109885,33.5421431717545));
#78062=CARTESIAN_POINT('Ctrl Pts',(21.6506031121263,17.3721710517851,33.4018706954166));
#78063=CARTESIAN_POINT('Ctrl Pts',(21.8,17.3159470879662,33.2627115017215));
#78064=CARTESIAN_POINT('',(21.8,14.3502390708311,34.6456438619633));
#78065=CARTESIAN_POINT('Ctrl Pts',(21.8,17.3159470879662,33.2627115017215));
#78066=CARTESIAN_POINT('Ctrl Pts',(21.8713861730394,15.8330930793986,33.9541776818424));
#78067=CARTESIAN_POINT('Ctrl Pts',(21.8,14.3502390708311,34.6456438619633));
#78068=CARTESIAN_POINT('',(21.5,14.4917268913708,34.9117437505765));
#78069=CARTESIAN_POINT('Ctrl Pts',(21.8,14.3502390708311,34.6456438619633));
#78070=CARTESIAN_POINT('Ctrl Pts',(21.6506031093095,14.4207011318884,34.7781637249967));
#78071=CARTESIAN_POINT('Ctrl Pts',(21.5,14.4917268913708,34.9117437505765));
#78072=CARTESIAN_POINT('',(21.5,11.3395294590896,36.0590497884572));
#78073=CARTESIAN_POINT('Origin',(21.5,0.,0.));
#78074=CARTESIAN_POINT('',(21.8,11.2768697064435,35.764258829506));
#78075=CARTESIAN_POINT('Ctrl Pts',(21.5,11.3395294590896,36.0590497884573));
#78076=CARTESIAN_POINT('Ctrl Pts',(21.6506031035411,11.30807476332,35.911067079655));
#78077=CARTESIAN_POINT('Ctrl Pts',(21.8,11.2768697064435,35.764258829506));
#78078=CARTESIAN_POINT('',(21.8,8.11607377380575,36.6111915470959));
#78079=CARTESIAN_POINT('Ctrl Pts',(21.8,11.2768697064435,35.764258829506));
#78080=CARTESIAN_POINT('Ctrl Pts',(21.8713861730393,9.69647174012463,36.1877251883009));
#78081=CARTESIAN_POINT('Ctrl Pts',(21.8,8.11607377380575,36.6111915470959));
#78082=CARTESIAN_POINT('',(21.5,8.20920431569501,36.8978178826767));
#78083=CARTESIAN_POINT('Ctrl Pts',(21.8,8.11607377380575,36.6111915470959));
#78084=CARTESIAN_POINT('Ctrl Pts',(21.6506031086535,8.1624535253115,36.7539337447634));
#78085=CARTESIAN_POINT('Ctrl Pts',(21.5,8.20920431569501,36.8978178826767));
#78086=CARTESIAN_POINT('',(21.5,4.90566824265507,37.4803204240973));
#78087=CARTESIAN_POINT('Origin',(21.5,0.,0.));
#78088=CARTESIAN_POINT('',(21.8,4.89515034526195,37.1791272503441));
#78089=CARTESIAN_POINT('Ctrl Pts',(21.5,4.90566824265507,37.4803204240973));
#78090=CARTESIAN_POINT('Ctrl Pts',(21.6506031094157,4.90038834189625,37.3291238486592));
#78091=CARTESIAN_POINT('Ctrl Pts',(21.8,4.89515034526195,37.1791272503441));
#78092=CARTESIAN_POINT('',(21.8,1.63530568209483,37.4643267032268));
#78093=CARTESIAN_POINT('Ctrl Pts',(21.8,4.89515034526195,37.1791272503441));
#78094=CARTESIAN_POINT('Ctrl Pts',(21.8713861730393,3.26522801367839,37.3217269767854));
#78095=CARTESIAN_POINT('Ctrl Pts',(21.8,1.63530568209483,37.4643267032268));
#78096=CARTESIAN_POINT('',(21.5,1.67724922094465,37.7627704896084));
#78097=CARTESIAN_POINT('Ctrl Pts',(21.8,1.63530568209483,37.4643267032268));
#78098=CARTESIAN_POINT('Ctrl Pts',(21.6506031053325,1.65619389892368,37.6129540888054));
#78099=CARTESIAN_POINT('Ctrl Pts',(21.5,1.67724922094465,37.7627704896084));
#78100=CARTESIAN_POINT('',(21.5,-1.67724922094464,37.7627704896084));
#78101=CARTESIAN_POINT('Origin',(21.5,0.,0.));
#78102=CARTESIAN_POINT('',(21.8,-1.63530568209482,37.4643267032267));
#78103=CARTESIAN_POINT('Ctrl Pts',(21.5,-1.67724922094464,37.7627704896084));
#78104=CARTESIAN_POINT('Ctrl Pts',(21.6506031054257,-1.65619389891064,37.6129540887127));
#78105=CARTESIAN_POINT('Ctrl Pts',(21.8,-1.63530568209482,37.4643267032267));
#78106=CARTESIAN_POINT('',(21.8,-4.89515034526194,37.1791272503441));
#78107=CARTESIAN_POINT('Ctrl Pts',(21.8,-1.63530568209482,37.4643267032267));
#78108=CARTESIAN_POINT('Ctrl Pts',(21.8713861730394,-3.26522801367839,37.3217269767854));
#78109=CARTESIAN_POINT('Ctrl Pts',(21.8,-4.89515034526194,37.1791272503441));
#78110=CARTESIAN_POINT('',(21.5,-4.90566824265506,37.4803204240973));
#78111=CARTESIAN_POINT('Ctrl Pts',(21.8,-4.89515034526194,37.1791272503441));
#78112=CARTESIAN_POINT('Ctrl Pts',(21.6506031056954,-4.90038834202669,37.3291238523946));
#78113=CARTESIAN_POINT('Ctrl Pts',(21.5,-4.90566824265506,37.4803204240973));
#78114=CARTESIAN_POINT('',(21.5,-8.20920431569501,36.8978178826767));
#78115=CARTESIAN_POINT('Origin',(21.5,0.,0.));
#78116=CARTESIAN_POINT('',(21.8,-8.11607377380574,36.6111915470959));
#78117=CARTESIAN_POINT('Ctrl Pts',(21.5,-8.20920431569501,36.8978178826767));
#78118=CARTESIAN_POINT('Ctrl Pts',(21.6506031085607,-8.16245352534031,36.7539337448521));
#78119=CARTESIAN_POINT('Ctrl Pts',(21.8,-8.11607377380574,36.6111915470959));
#78120=CARTESIAN_POINT('',(21.8,-11.2768697064435,35.764258829506));
#78121=CARTESIAN_POINT('Ctrl Pts',(21.8,-8.11607377380574,36.6111915470959));
#78122=CARTESIAN_POINT('Ctrl Pts',(21.8713861730394,-9.69647174012463,36.1877251883009));
#78123=CARTESIAN_POINT('Ctrl Pts',(21.8,-11.2768697064435,35.764258829506));
#78124=CARTESIAN_POINT('',(21.5,-11.3395294590896,36.0590497884573));
#78125=CARTESIAN_POINT('Ctrl Pts',(21.8,-11.2768697064435,35.764258829506));
#78126=CARTESIAN_POINT('Ctrl Pts',(21.6506031074235,-11.308074762509,35.9110670758397));
#78127=CARTESIAN_POINT('Ctrl Pts',(21.5,-11.3395294590896,36.0590497884573));
#78128=CARTESIAN_POINT('',(21.5,-14.4917268913708,34.9117437505765));
#78129=CARTESIAN_POINT('Origin',(21.5,0.,0.));
#78130=CARTESIAN_POINT('',(21.8,-14.3502390708311,34.6456438619633));
#78131=CARTESIAN_POINT('Ctrl Pts',(21.5,-14.4917268913708,34.9117437505765));
#78132=CARTESIAN_POINT('Ctrl Pts',(21.6506031093456,-14.4207011318714,34.7781637249647));
#78133=CARTESIAN_POINT('Ctrl Pts',(21.8,-14.3502390708311,34.6456438619633));
#78134=CARTESIAN_POINT('',(21.8,-17.3159470879662,33.2627115017215));
#78135=CARTESIAN_POINT('Ctrl Pts',(21.8,-14.3502390708311,34.6456438619633));
#78136=CARTESIAN_POINT('Ctrl Pts',(21.8713861730394,-15.8330930793986,33.9541776818424));
#78137=CARTESIAN_POINT('Ctrl Pts',(21.8,-17.3159470879662,33.2627115017215));
#78138=CARTESIAN_POINT('',(21.5,-17.4288448109885,33.5421431717545));
#78139=CARTESIAN_POINT('Ctrl Pts',(21.8,-17.3159470879662,33.2627115017215));
#78140=CARTESIAN_POINT('Ctrl Pts',(21.6506031114957,-17.3721710520224,33.401870696004));
#78141=CARTESIAN_POINT('Ctrl Pts',(21.5,-17.4288448109885,33.5421431717545));
#78142=CARTESIAN_POINT('Origin',(21.5,0.,0.));
#78143=CARTESIAN_POINT('Origin',(21.75,0.,0.));
#78144=CARTESIAN_POINT('',(21.8,-11.2768697064435,-35.764258829506));
#78145=CARTESIAN_POINT('Ctrl Pts',(21.5,-11.3395294590896,-36.0590497884572));
#78146=CARTESIAN_POINT('Ctrl Pts',(21.6506031111505,-11.3080747617305,-35.9110670721771));
#78147=CARTESIAN_POINT('Ctrl Pts',(21.8,-11.2768697064435,-35.764258829506));
#78148=CARTESIAN_POINT('',(21.8,-8.11607377380577,-36.6111915470959));
#78149=CARTESIAN_POINT('Ctrl Pts',(21.8,-11.2768697064435,-35.764258829506));
#78150=CARTESIAN_POINT('Ctrl Pts',(21.8713861730393,-9.69647174012465,-36.1877251883009));
#78151=CARTESIAN_POINT('Ctrl Pts',(21.8,-8.11607377380577,-36.6111915470959));
#78152=CARTESIAN_POINT('',(21.5,-8.20920431569503,-36.8978178826767));
#78153=CARTESIAN_POINT('Ctrl Pts',(21.8,-8.11607377380577,-36.6111915470959));
#78154=CARTESIAN_POINT('Ctrl Pts',(21.6506031047876,-8.16245352651173,-36.7539337484572));
#78155=CARTESIAN_POINT('Ctrl Pts',(21.5,-8.20920431569504,-36.8978178826767));
#78156=CARTESIAN_POINT('',(21.5,-4.90566824265507,-37.4803204240973));
#78157=CARTESIAN_POINT('Origin',(21.5,0.,0.));
#78158=CARTESIAN_POINT('',(21.8,-4.89515034526194,-37.1791272503441));
#78159=CARTESIAN_POINT('Ctrl Pts',(21.5,-4.90566824265507,-37.4803204240973));
#78160=CARTESIAN_POINT('Ctrl Pts',(21.6506031094336,-4.90038834189562,-37.3291238486412));
#78161=CARTESIAN_POINT('Ctrl Pts',(21.8,-4.89515034526194,-37.1791272503441));
#78162=CARTESIAN_POINT('',(21.8,-1.63530568209482,-37.4643267032267));
#78163=CARTESIAN_POINT('Ctrl Pts',(21.8,-4.89515034526194,-37.1791272503441));
#78164=CARTESIAN_POINT('Ctrl Pts',(21.8713861730394,-3.26522801367838,-37.3217269767854));
#78165=CARTESIAN_POINT('Ctrl Pts',(21.8,-1.63530568209482,-37.4643267032267));
#78166=CARTESIAN_POINT('',(21.5,-1.67724922094465,-37.7627704896084));
#78167=CARTESIAN_POINT('Ctrl Pts',(21.8,-1.63530568209482,-37.4643267032267));
#78168=CARTESIAN_POINT('Ctrl Pts',(21.6506031054194,-1.65619389891153,-37.612954088719));
#78169=CARTESIAN_POINT('Ctrl Pts',(21.5,-1.67724922094465,-37.7627704896084));
#78170=CARTESIAN_POINT('',(21.5,1.67724922094464,-37.7627704896084));
#78171=CARTESIAN_POINT('Origin',(21.5,0.,0.));
#78172=CARTESIAN_POINT('',(21.8,1.63530568209482,-37.4643267032267));
#78173=CARTESIAN_POINT('Ctrl Pts',(21.5,1.67724922094464,-37.7627704896084));
#78174=CARTESIAN_POINT('Ctrl Pts',(21.6506031054903,1.6561938989016,-37.6129540886484));
#78175=CARTESIAN_POINT('Ctrl Pts',(21.8,1.63530568209482,-37.4643267032267));
#78176=CARTESIAN_POINT('',(21.8,4.89515034526193,-37.1791272503441));
#78177=CARTESIAN_POINT('Ctrl Pts',(21.8,1.63530568209482,-37.4643267032267));
#78178=CARTESIAN_POINT('Ctrl Pts',(21.8713861730394,3.26522801367838,-37.3217269767854));
#78179=CARTESIAN_POINT('Ctrl Pts',(21.8,4.89515034526193,-37.1791272503441));
#78180=CARTESIAN_POINT('',(21.5,4.90566824265506,-37.4803204240973));
#78181=CARTESIAN_POINT('Ctrl Pts',(21.8,4.89515034526193,-37.1791272503441));
#78182=CARTESIAN_POINT('Ctrl Pts',(21.6506031093552,4.90038834189836,-37.3291238487199));
#78183=CARTESIAN_POINT('Ctrl Pts',(21.5,4.90566824265506,-37.4803204240973));
#78184=CARTESIAN_POINT('',(21.5,8.209204315695,-36.8978178826767));
#78185=CARTESIAN_POINT('Origin',(21.5,0.,0.));
#78186=CARTESIAN_POINT('',(21.8,8.11607377380573,-36.6111915470959));
#78187=CARTESIAN_POINT('Ctrl Pts',(21.5,8.209204315695,-36.8978178826767));
#78188=CARTESIAN_POINT('Ctrl Pts',(21.6506031085797,8.1624535253344,-36.7539337448339));
#78189=CARTESIAN_POINT('Ctrl Pts',(21.8,8.11607377380573,-36.6111915470958));
#78190=CARTESIAN_POINT('',(21.8,11.2768697064435,-35.764258829506));
#78191=CARTESIAN_POINT('Ctrl Pts',(21.8,8.11607377380573,-36.6111915470959));
#78192=CARTESIAN_POINT('Ctrl Pts',(21.8713861730394,9.69647174012462,-36.1877251883009));
#78193=CARTESIAN_POINT('Ctrl Pts',(21.8,11.2768697064435,-35.764258829506));
#78194=CARTESIAN_POINT('',(21.5,11.3395294590896,-36.0590497884573));
#78195=CARTESIAN_POINT('Ctrl Pts',(21.8,11.2768697064435,-35.764258829506));
#78196=CARTESIAN_POINT('Ctrl Pts',(21.6506031037827,11.3080747632695,-35.9110670794176));
#78197=CARTESIAN_POINT('Ctrl Pts',(21.5,11.3395294590896,-36.0590497884573));
#78198=CARTESIAN_POINT('',(21.5,14.4917268913708,-34.9117437505765));
#78199=CARTESIAN_POINT('Origin',(21.5,0.,0.));
#78200=CARTESIAN_POINT('',(21.8,14.350239070831,-34.6456438619633));
#78201=CARTESIAN_POINT('Ctrl Pts',(21.5,14.4917268913708,-34.9117437505766));
#78202=CARTESIAN_POINT('Ctrl Pts',(21.6506031096943,14.4207011317069,-34.7781637246554));
#78203=CARTESIAN_POINT('Ctrl Pts',(21.8,14.350239070831,-34.6456438619633));
#78204=CARTESIAN_POINT('',(21.8,17.3159470879662,-33.2627115017215));
#78205=CARTESIAN_POINT('Ctrl Pts',(21.8,14.350239070831,-34.6456438619633));
#78206=CARTESIAN_POINT('Ctrl Pts',(21.8713861730393,15.8330930793986,-33.9541776818424));
#78207=CARTESIAN_POINT('Ctrl Pts',(21.8,17.3159470879662,-33.2627115017215));
#78208=CARTESIAN_POINT('',(21.5,17.4288448109885,-33.5421431717545));
#78209=CARTESIAN_POINT('Ctrl Pts',(21.8,17.3159470879662,-33.2627115017215));
#78210=CARTESIAN_POINT('Ctrl Pts',(21.6506031077603,17.3721710534283,-33.4018706994836));
#78211=CARTESIAN_POINT('Ctrl Pts',(21.5,17.4288448109885,-33.5421431717546));
#78212=CARTESIAN_POINT('',(21.5,20.3339256786199,-31.8648939508099));
#78213=CARTESIAN_POINT('Origin',(21.5,0.,0.));
#78214=CARTESIAN_POINT('',(21.8,20.1483796152605,-31.6274058196267));
#78215=CARTESIAN_POINT('Ctrl Pts',(21.5,20.3339256786199,-31.8648939508099));
#78216=CARTESIAN_POINT('Ctrl Pts',(21.6506031087829,20.2407830323292,-31.7456768000897));
#78217=CARTESIAN_POINT('Ctrl Pts',(21.8,20.1483796152605,-31.6274058196267));
#78218=CARTESIAN_POINT('',(21.8,22.8288881795131,-29.7504935167013));
#78219=CARTESIAN_POINT('Ctrl Pts',(21.8,20.1483796152605,-31.6274058196267));
#78220=CARTESIAN_POINT('Ctrl Pts',(21.8713861730394,21.4886338973868,-30.688949668164));
#78221=CARTESIAN_POINT('Ctrl Pts',(21.8,22.8288881795131,-29.7504935167013));
#78222=CARTESIAN_POINT('',(21.5,22.9885935327265,-30.0060755079215));
#78223=CARTESIAN_POINT('Ctrl Pts',(21.8,22.8288881795131,-29.7504935167013));
#78224=CARTESIAN_POINT('Ctrl Pts',(21.6506031065164,22.9084227183644,-29.8777753854765));
#78225=CARTESIAN_POINT('Ctrl Pts',(21.5,22.9885935327265,-30.0060755079215));
#78226=CARTESIAN_POINT('',(21.5,25.5582884235871,-27.8498454727622));
#78227=CARTESIAN_POINT('Origin',(21.5,0.,0.));
#78228=CARTESIAN_POINT('',(21.8,25.3343218406523,-27.6481850557002));
#78229=CARTESIAN_POINT('Ctrl Pts',(21.5,25.5582884235871,-27.8498454727622));
#78230=CARTESIAN_POINT('Ctrl Pts',(21.6506031049548,25.4458589852728,-27.748613551806));
#78231=CARTESIAN_POINT('Ctrl Pts',(21.8,25.3343218406523,-27.6481850557002));
#78232=CARTESIAN_POINT('',(21.8,27.6481850557002,-25.3343218406523));
#78233=CARTESIAN_POINT('Ctrl Pts',(21.8,25.3343218406523,-27.6481850557002));
#78234=CARTESIAN_POINT('Ctrl Pts',(21.8713861730394,26.4912534481763,-26.4912534481763));
#78235=CARTESIAN_POINT('Ctrl Pts',(21.8,27.6481850557002,-25.3343218406523));
#78236=CARTESIAN_POINT('',(21.5,27.8498454727622,-25.5582884235871));
#78237=CARTESIAN_POINT('Ctrl Pts',(21.8,27.6481850557002,-25.3343218406523));
#78238=CARTESIAN_POINT('Ctrl Pts',(21.650603106132,27.7486135510146,-25.4458589843939));
#78239=CARTESIAN_POINT('Ctrl Pts',(21.5,27.8498454727622,-25.5582884235871));
#78240=CARTESIAN_POINT('',(21.5,30.0060755079215,-22.9885935327265));
#78241=CARTESIAN_POINT('Origin',(21.5,0.,0.));
#78242=CARTESIAN_POINT('',(21.8,29.7504935167013,-22.8288881795131));
#78243=CARTESIAN_POINT('Ctrl Pts',(21.5,30.0060755079215,-22.9885935327265));
#78244=CARTESIAN_POINT('Ctrl Pts',(21.6506031103219,29.8777753822342,-22.9084227163384));
#78245=CARTESIAN_POINT('Ctrl Pts',(21.8,29.7504935167013,-22.8288881795131));
#78246=CARTESIAN_POINT('',(21.8,31.6274058196267,-20.1483796152605));
#78247=CARTESIAN_POINT('Ctrl Pts',(21.8,29.7504935167013,-22.8288881795131));
#78248=CARTESIAN_POINT('Ctrl Pts',(21.8713861730394,30.688949668164,-21.4886338973868));
#78249=CARTESIAN_POINT('Ctrl Pts',(21.8,31.6274058196267,-20.1483796152605));
#78250=CARTESIAN_POINT('',(21.5,31.8648939508099,-20.3339256786199));
#78251=CARTESIAN_POINT('Ctrl Pts',(21.8,31.6274058196267,-20.1483796152605));
#78252=CARTESIAN_POINT('Ctrl Pts',(21.6506031038392,31.7456768040036,-20.2407830353871));
#78253=CARTESIAN_POINT('Ctrl Pts',(21.5,31.8648939508099,-20.3339256786199));
#78254=CARTESIAN_POINT('',(21.5,33.5421431717545,-17.4288448109885));
#78255=CARTESIAN_POINT('Origin',(21.5,0.,0.));
#78256=CARTESIAN_POINT('',(21.8,33.2627115017215,-17.3159470879662));
#78257=CARTESIAN_POINT('Ctrl Pts',(21.5,33.5421431717545,-17.4288448109885));
#78258=CARTESIAN_POINT('Ctrl Pts',(21.6506031041173,33.4018707028771,-17.3721710547994));
#78259=CARTESIAN_POINT('Ctrl Pts',(21.8,33.2627115017215,-17.3159470879662));
#78260=CARTESIAN_POINT('',(21.8,34.6456438619633,-14.3502390708311));
#78261=CARTESIAN_POINT('Ctrl Pts',(21.8,33.2627115017215,-17.3159470879662));
#78262=CARTESIAN_POINT('Ctrl Pts',(21.8713861730393,33.9541776818424,-15.8330930793987));
#78263=CARTESIAN_POINT('Ctrl Pts',(21.8,34.6456438619633,-14.3502390708311));
#78264=CARTESIAN_POINT('',(21.5,34.9117437505765,-14.4917268913708));
#78265=CARTESIAN_POINT('Ctrl Pts',(21.8,34.6456438619633,-14.3502390708311));
#78266=CARTESIAN_POINT('Ctrl Pts',(21.6506031056005,34.7781637282868,-14.4207011336378));
#78267=CARTESIAN_POINT('Ctrl Pts',(21.5,34.9117437505765,-14.4917268913708));
#78268=CARTESIAN_POINT('',(21.5,36.0590497884572,-11.3395294590896));
#78269=CARTESIAN_POINT('Origin',(21.5,0.,0.));
#78270=CARTESIAN_POINT('',(21.8,35.764258829506,-11.2768697064435));
#78271=CARTESIAN_POINT('Ctrl Pts',(21.5,36.0590497884572,-11.3395294590896));
#78272=CARTESIAN_POINT('Ctrl Pts',(21.6506031073768,35.9110670758856,-11.3080747625188));
#78273=CARTESIAN_POINT('Ctrl Pts',(21.8,35.764258829506,-11.2768697064435));
#78274=CARTESIAN_POINT('',(21.8,36.6111915470958,-8.11607377380577));
#78275=CARTESIAN_POINT('Ctrl Pts',(21.8,35.764258829506,-11.2768697064435));
#78276=CARTESIAN_POINT('Ctrl Pts',(21.8713861730393,36.1877251883009,-9.69647174012465));
#78277=CARTESIAN_POINT('Ctrl Pts',(21.8,36.6111915470958,-8.11607377380577));
#78278=CARTESIAN_POINT('',(21.5,36.8978178826767,-8.20920431569504));
#78279=CARTESIAN_POINT('Ctrl Pts',(21.8,36.6111915470958,-8.11607377380577));
#78280=CARTESIAN_POINT('Ctrl Pts',(21.6506031087027,36.7539337447164,-8.16245352529625));
#78281=CARTESIAN_POINT('Ctrl Pts',(21.5,36.8978178826767,-8.20920431569504));
#78282=CARTESIAN_POINT('',(21.5,37.4803204240973,-4.90566824265507));
#78283=CARTESIAN_POINT('Origin',(21.5,0.,0.));
#78284=CARTESIAN_POINT('',(21.8,37.1791272503441,-4.89515034526195));
#78285=CARTESIAN_POINT('Ctrl Pts',(21.5,37.4803204240973,-4.90566824265507));
#78286=CARTESIAN_POINT('Ctrl Pts',(21.6506031020327,37.3291238560722,-4.90038834215512));
#78287=CARTESIAN_POINT('Ctrl Pts',(21.8,37.1791272503441,-4.89515034526195));
#78288=CARTESIAN_POINT('',(21.8,37.4643267032267,-1.63530568209483));
#78289=CARTESIAN_POINT('Ctrl Pts',(21.8,37.1791272503441,-4.89515034526195));
#78290=CARTESIAN_POINT('Ctrl Pts',(21.8713861730394,37.3217269767854,-3.26522801367838));
#78291=CARTESIAN_POINT('Ctrl Pts',(21.8,37.4643267032267,-1.63530568209483));
#78292=CARTESIAN_POINT('',(21.5,37.7627704896084,-1.67724922094465));
#78293=CARTESIAN_POINT('Ctrl Pts',(21.8,37.4643267032267,-1.63530568209483));
#78294=CARTESIAN_POINT('Ctrl Pts',(21.6506031055069,37.6129540886319,-1.6561938988993));
#78295=CARTESIAN_POINT('Ctrl Pts',(21.5,37.7627704896084,-1.67724922094465));
#78296=CARTESIAN_POINT('',(21.5,37.7878017125899,-0.960230040142118));
#78297=CARTESIAN_POINT('Origin',(21.5,0.,0.));
#78298=CARTESIAN_POINT('',(22.,37.2864828558561,-1.0040897569181));
#78299=CARTESIAN_POINT('Ctrl Pts',(21.5,37.7878017125899,-0.960230040142117));
#78300=CARTESIAN_POINT('Ctrl Pts',(21.7516860406602,37.5354734529172,-0.982305902350696));
#78301=CARTESIAN_POINT('Ctrl Pts',(22.,37.2864828558561,-1.0040897569181));
#78302=CARTESIAN_POINT('Origin',(22.,0.,0.));
#78303=CARTESIAN_POINT('Origin',(11.,0.,0.));
#78304=CARTESIAN_POINT('',(11.,-25.5582884235871,27.8498454727622));
#78305=CARTESIAN_POINT('Origin',(0.249999999999999,0.,0.));
#78306=CARTESIAN_POINT('',(0.499999999999998,-17.4288448109885,33.5421431717545));
#78307=CARTESIAN_POINT('Origin',(0.499999999999998,0.,0.));
#78308=CARTESIAN_POINT('',(0.200000000000004,-17.3159470879662,33.2627115017215));
#78309=CARTESIAN_POINT('Ctrl Pts',(0.500000000000001,-17.4288448109885,
33.5421431717545));
#78310=CARTESIAN_POINT('Ctrl Pts',(0.349396891634736,-17.3721710532006,
33.40187069892));
#78311=CARTESIAN_POINT('Ctrl Pts',(0.200000000000004,-17.3159470879662,
33.2627115017215));
#78312=CARTESIAN_POINT('',(0.200000000000008,-14.3502390708311,34.6456438619633));
#78313=CARTESIAN_POINT('Ctrl Pts',(0.200000000000004,-17.3159470879662,
33.2627115017215));
#78314=CARTESIAN_POINT('Ctrl Pts',(0.128613826960649,-15.8330930793986,
33.9541776818424));
#78315=CARTESIAN_POINT('Ctrl Pts',(0.200000000000008,-14.3502390708311,
34.6456438619633));
#78316=CARTESIAN_POINT('',(0.499999999999998,-14.4917268913708,34.9117437505765));
#78317=CARTESIAN_POINT('Ctrl Pts',(0.200000000000008,-14.3502390708311,
34.6456438619633));
#78318=CARTESIAN_POINT('Ctrl Pts',(0.349396894490965,-14.420701133681,34.778163728368));
#78319=CARTESIAN_POINT('Ctrl Pts',(0.500000000000001,-14.4917268913708,
34.9117437505765));
#78320=CARTESIAN_POINT('',(0.499999999999998,-11.3395294590896,36.0590497884573));
#78321=CARTESIAN_POINT('Origin',(0.499999999999998,0.,0.));
#78322=CARTESIAN_POINT('',(0.200000000000006,-11.2768697064435,35.764258829506));
#78323=CARTESIAN_POINT('Ctrl Pts',(0.500000000000001,-11.3395294590896,
36.0590497884573));
#78324=CARTESIAN_POINT('Ctrl Pts',(0.349396892532884,-11.3080747624999,
35.9110670757969));
#78325=CARTESIAN_POINT('Ctrl Pts',(0.200000000000006,-11.2768697064435,
35.764258829506));
#78326=CARTESIAN_POINT('',(0.200000000000009,-8.11607377380574,36.6111915470959));
#78327=CARTESIAN_POINT('Ctrl Pts',(0.200000000000006,-11.2768697064435,
35.764258829506));
#78328=CARTESIAN_POINT('Ctrl Pts',(0.128613826960651,-9.69647174012462,
36.1877251883009));
#78329=CARTESIAN_POINT('Ctrl Pts',(0.200000000000009,-8.11607377380574,
36.6111915470959));
#78330=CARTESIAN_POINT('',(0.499999999999998,-8.20920431569501,36.8978178826767));
#78331=CARTESIAN_POINT('Ctrl Pts',(0.200000000000009,-8.11607377380574,
36.6111915470959));
#78332=CARTESIAN_POINT('Ctrl Pts',(0.349396891056085,-8.16245352522133,
36.7539337444859));
#78333=CARTESIAN_POINT('Ctrl Pts',(0.500000000000001,-8.20920431569501,
36.8978178826767));
#78334=CARTESIAN_POINT('',(0.499999999999998,-4.90566824265506,37.4803204240973));
#78335=CARTESIAN_POINT('Origin',(0.499999999999998,0.,0.));
#78336=CARTESIAN_POINT('',(0.200000000000002,-4.89515034526194,37.1791272503441));
#78337=CARTESIAN_POINT('Ctrl Pts',(0.500000000000001,-4.90566824265506,
37.4803204240973));
#78338=CARTESIAN_POINT('Ctrl Pts',(0.349396894143512,-4.90038834202104,
37.3291238522329));
#78339=CARTESIAN_POINT('Ctrl Pts',(0.200000000000002,-4.89515034526194,
37.1791272503441));
#78340=CARTESIAN_POINT('',(0.200000000000005,-1.63530568209482,37.4643267032267));
#78341=CARTESIAN_POINT('Ctrl Pts',(0.200000000000002,-4.89515034526194,
37.1791272503441));
#78342=CARTESIAN_POINT('Ctrl Pts',(0.128613826960647,-3.26522801367838,
37.3217269767854));
#78343=CARTESIAN_POINT('Ctrl Pts',(0.200000000000005,-1.63530568209482,
37.4643267032267));
#78344=CARTESIAN_POINT('',(0.499999999999998,-1.67724922094464,37.7627704896084));
#78345=CARTESIAN_POINT('Ctrl Pts',(0.200000000000005,-1.63530568209482,
37.4643267032267));
#78346=CARTESIAN_POINT('Ctrl Pts',(0.349396890838704,-1.65619389838832,
37.6129540849961));
#78347=CARTESIAN_POINT('Ctrl Pts',(0.500000000000001,-1.67724922094464,
37.7627704896084));
#78348=CARTESIAN_POINT('',(0.499999999999998,1.67724922094465,37.7627704896084));
#78349=CARTESIAN_POINT('Origin',(0.499999999999998,0.,0.));
#78350=CARTESIAN_POINT('',(0.200000000000009,1.63530568209483,37.4643267032268));
#78351=CARTESIAN_POINT('Ctrl Pts',(0.500000000000001,1.67724922094465,37.7627704896084));
#78352=CARTESIAN_POINT('Ctrl Pts',(0.349396890774378,1.65619389837934,37.6129540849322));
#78353=CARTESIAN_POINT('Ctrl Pts',(0.200000000000009,1.63530568209483,37.4643267032268));
#78354=CARTESIAN_POINT('',(0.200000000000002,4.89515034526195,37.1791272503441));
#78355=CARTESIAN_POINT('Ctrl Pts',(0.200000000000009,1.63530568209483,37.4643267032268));
#78356=CARTESIAN_POINT('Ctrl Pts',(0.128613826960647,3.26522801367839,37.3217269767854));
#78357=CARTESIAN_POINT('Ctrl Pts',(0.200000000000002,4.89515034526195,37.1791272503441));
#78358=CARTESIAN_POINT('',(0.499999999999998,4.90566824265507,37.4803204240973));
#78359=CARTESIAN_POINT('Ctrl Pts',(0.200000000000002,4.89515034526195,37.1791272503441));
#78360=CARTESIAN_POINT('Ctrl Pts',(0.34939689050702,4.90038834189354,37.3291238485816));
#78361=CARTESIAN_POINT('Ctrl Pts',(0.500000000000001,4.90566824265507,37.4803204240973));
#78362=CARTESIAN_POINT('',(0.499999999999998,8.20920431569501,36.8978178826767));
#78363=CARTESIAN_POINT('Origin',(0.499999999999998,0.,0.));
#78364=CARTESIAN_POINT('',(0.200000000000009,8.11607377380574,36.6111915470959));
#78365=CARTESIAN_POINT('Ctrl Pts',(0.500000000000001,8.20920431569502,36.8978178826767));
#78366=CARTESIAN_POINT('Ctrl Pts',(0.349396891227305,8.16245352527449,36.7539337446495));
#78367=CARTESIAN_POINT('Ctrl Pts',(0.200000000000009,8.11607377380575,36.6111915470959));
#78368=CARTESIAN_POINT('',(0.20000000000001,11.2768697064435,35.764258829506));
#78369=CARTESIAN_POINT('Ctrl Pts',(0.200000000000009,8.11607377380574,36.6111915470959));
#78370=CARTESIAN_POINT('Ctrl Pts',(0.128613826960651,9.69647174012464,36.1877251883009));
#78371=CARTESIAN_POINT('Ctrl Pts',(0.20000000000001,11.2768697064435,35.764258829506));
#78372=CARTESIAN_POINT('',(0.499999999999998,11.3395294590896,36.0590497884572));
#78373=CARTESIAN_POINT('Ctrl Pts',(0.20000000000001,11.2768697064435,35.764258829506));
#78374=CARTESIAN_POINT('Ctrl Pts',(0.349396892476858,11.3080747624882,35.9110670757418));
#78375=CARTESIAN_POINT('Ctrl Pts',(0.500000000000001,11.3395294590896,36.0590497884572));
#78376=CARTESIAN_POINT('',(0.499999999999998,14.4917268913708,34.9117437505765));
#78377=CARTESIAN_POINT('Origin',(0.499999999999998,0.,0.));
#78378=CARTESIAN_POINT('',(0.200000000000003,14.3502390708311,34.6456438619633));
#78379=CARTESIAN_POINT('Ctrl Pts',(0.500000000000001,14.4917268913708,34.9117437505765));
#78380=CARTESIAN_POINT('Ctrl Pts',(0.349396894532555,14.4207011337006,34.7781637284049));
#78381=CARTESIAN_POINT('Ctrl Pts',(0.200000000000003,14.3502390708311,34.6456438619633));
#78382=CARTESIAN_POINT('',(0.200000000000003,17.3159470879662,33.2627115017215));
#78383=CARTESIAN_POINT('Ctrl Pts',(0.200000000000003,14.3502390708311,34.6456438619633));
#78384=CARTESIAN_POINT('Ctrl Pts',(0.128613826960644,15.8330930793986,33.9541776818424));
#78385=CARTESIAN_POINT('Ctrl Pts',(0.200000000000003,17.3159470879662,33.2627115017215));
#78386=CARTESIAN_POINT('',(0.499999999999998,17.4288448109885,33.5421431717545));
#78387=CARTESIAN_POINT('Ctrl Pts',(0.200000000000003,17.3159470879662,33.2627115017215));
#78388=CARTESIAN_POINT('Ctrl Pts',(0.349396895954869,17.3721710548265,33.4018707029443));
#78389=CARTESIAN_POINT('Ctrl Pts',(0.500000000000001,17.4288448109885,33.5421431717545));
#78390=CARTESIAN_POINT('',(0.499999999999998,20.3339256786199,31.8648939508099));
#78391=CARTESIAN_POINT('Origin',(0.499999999999998,0.,0.));
#78392=CARTESIAN_POINT('',(0.200000000000003,20.1483796152605,31.6274058196267));
#78393=CARTESIAN_POINT('Ctrl Pts',(0.500000000000001,20.3339256786199,31.8648939508099));
#78394=CARTESIAN_POINT('Ctrl Pts',(0.349396892392812,20.2407830330564,31.7456768010206));
#78395=CARTESIAN_POINT('Ctrl Pts',(0.200000000000003,20.1483796152605,31.6274058196267));
#78396=CARTESIAN_POINT('',(0.200000000000003,22.8288881795131,29.7504935167013));
#78397=CARTESIAN_POINT('Ctrl Pts',(0.200000000000003,20.1483796152605,31.6274058196267));
#78398=CARTESIAN_POINT('Ctrl Pts',(0.128613826960645,21.4886338973868,30.688949668164));
#78399=CARTESIAN_POINT('Ctrl Pts',(0.200000000000003,22.8288881795131,29.7504935167013));
#78400=CARTESIAN_POINT('',(0.499999999999998,22.9885935327265,30.0060755079215));
#78401=CARTESIAN_POINT('Ctrl Pts',(0.200000000000003,22.8288881795131,29.7504935167013));
#78402=CARTESIAN_POINT('Ctrl Pts',(0.349396892464199,22.9084227178217,29.877775384608));
#78403=CARTESIAN_POINT('Ctrl Pts',(0.500000000000001,22.9885935327265,30.0060755079215));
#78404=CARTESIAN_POINT('',(0.499999999999998,25.5582884235871,27.8498454727622));
#78405=CARTESIAN_POINT('Origin',(0.499999999999998,0.,0.));
#78406=CARTESIAN_POINT('',(0.200000000000009,25.3343218406523,27.6481850557002));
#78407=CARTESIAN_POINT('Ctrl Pts',(0.500000000000001,25.5582884235871,27.8498454727622));
#78408=CARTESIAN_POINT('Ctrl Pts',(0.3493968910558,25.4458589822943,27.7486135491241));
#78409=CARTESIAN_POINT('Ctrl Pts',(0.200000000000009,25.3343218406523,27.6481850557002));
#78410=CARTESIAN_POINT('',(0.200000000000006,27.6481850557002,25.3343218406523));
#78411=CARTESIAN_POINT('Ctrl Pts',(0.200000000000009,25.3343218406523,27.6481850557002));
#78412=CARTESIAN_POINT('Ctrl Pts',(0.128613826960648,26.4912534481763,26.4912534481763));
#78413=CARTESIAN_POINT('Ctrl Pts',(0.200000000000006,27.6481850557002,25.3343218406523));
#78414=CARTESIAN_POINT('',(0.499999999999998,27.8498454727622,25.5582884235871));
#78415=CARTESIAN_POINT('Ctrl Pts',(0.200000000000006,27.6481850557002,25.3343218406523));
#78416=CARTESIAN_POINT('Ctrl Pts',(0.349396897556482,27.7486135534942,25.4458589871478));
#78417=CARTESIAN_POINT('Ctrl Pts',(0.5,27.8498454727622,25.5582884235871));
#78418=CARTESIAN_POINT('',(0.499999999999998,30.0060755079215,22.9885935327265));
#78419=CARTESIAN_POINT('Origin',(0.499999999999998,0.,0.));
#78420=CARTESIAN_POINT('',(0.199999999999999,29.7504935167013,22.8288881795131));
#78421=CARTESIAN_POINT('Ctrl Pts',(0.5,30.0060755079215,22.9885935327265));
#78422=CARTESIAN_POINT('Ctrl Pts',(0.349396889752811,29.8777753822979,22.9084227163782));
#78423=CARTESIAN_POINT('Ctrl Pts',(0.199999999999999,29.7504935167013,22.8288881795131));
#78424=CARTESIAN_POINT('',(0.200000000000006,31.6274058196267,20.1483796152605));
#78425=CARTESIAN_POINT('Ctrl Pts',(0.199999999999999,29.7504935167013,22.8288881795131));
#78426=CARTESIAN_POINT('Ctrl Pts',(0.128613826960648,30.688949668164,21.4886338973868));
#78427=CARTESIAN_POINT('Ctrl Pts',(0.200000000000006,31.6274058196267,20.1483796152605));
#78428=CARTESIAN_POINT('',(0.499999999999998,31.8648939508099,20.3339256786199));
#78429=CARTESIAN_POINT('Ctrl Pts',(0.200000000000006,31.6274058196267,20.1483796152605));
#78430=CARTESIAN_POINT('Ctrl Pts',(0.349396891131353,31.7456768000219,20.2407830322762));
#78431=CARTESIAN_POINT('Ctrl Pts',(0.5,31.8648939508099,20.3339256786199));
#78432=CARTESIAN_POINT('',(0.499999999999998,33.5421431717545,17.4288448109885));
#78433=CARTESIAN_POINT('Origin',(0.499999999999998,0.,0.));
#78434=CARTESIAN_POINT('',(0.200000000000004,33.2627115017215,17.3159470879662));
#78435=CARTESIAN_POINT('Ctrl Pts',(0.5,33.5421431717545,17.4288448109885));
#78436=CARTESIAN_POINT('Ctrl Pts',(0.349396892387157,33.4018706996209,17.3721710534838));
#78437=CARTESIAN_POINT('Ctrl Pts',(0.200000000000004,33.2627115017215,17.3159470879662));
#78438=CARTESIAN_POINT('',(0.200000000000008,34.6456438619633,14.3502390708311));
#78439=CARTESIAN_POINT('Ctrl Pts',(0.200000000000004,33.2627115017215,17.3159470879662));
#78440=CARTESIAN_POINT('Ctrl Pts',(0.128613826960652,33.9541776818424,15.8330930793986));
#78441=CARTESIAN_POINT('Ctrl Pts',(0.200000000000008,34.6456438619633,14.3502390708311));
#78442=CARTESIAN_POINT('',(0.499999999999998,34.9117437505765,14.4917268913708));
#78443=CARTESIAN_POINT('Ctrl Pts',(0.200000000000008,34.6456438619633,14.3502390708311));
#78444=CARTESIAN_POINT('Ctrl Pts',(0.349396894409378,34.7781637282956,14.4207011336425));
#78445=CARTESIAN_POINT('Ctrl Pts',(0.5,34.9117437505765,14.4917268913708));
#78446=CARTESIAN_POINT('',(0.499999999999998,36.0590497884573,11.3395294590896));
#78447=CARTESIAN_POINT('Origin',(0.499999999999998,0.,0.));
#78448=CARTESIAN_POINT('',(0.20000000000001,35.764258829506,11.2768697064435));
#78449=CARTESIAN_POINT('Ctrl Pts',(0.5,36.0590497884572,11.3395294590896));
#78450=CARTESIAN_POINT('Ctrl Pts',(0.349396896292396,35.9110670794914,11.3080747632852));
#78451=CARTESIAN_POINT('Ctrl Pts',(0.20000000000001,35.764258829506,11.2768697064435));
#78452=CARTESIAN_POINT('',(0.200000000000009,36.6111915470959,8.11607377380574));
#78453=CARTESIAN_POINT('Ctrl Pts',(0.20000000000001,35.764258829506,11.2768697064435));
#78454=CARTESIAN_POINT('Ctrl Pts',(0.12861382696065,36.1877251883009,9.69647174012463));
#78455=CARTESIAN_POINT('Ctrl Pts',(0.200000000000009,36.6111915470958,8.11607377380574));
#78456=CARTESIAN_POINT('',(0.499999999999998,36.8978178826767,8.20920431569501));
#78457=CARTESIAN_POINT('Ctrl Pts',(0.200000000000009,36.6111915470959,8.11607377380574));
#78458=CARTESIAN_POINT('Ctrl Pts',(0.349396891698014,36.7539337450992,8.16245352542062));
#78459=CARTESIAN_POINT('Ctrl Pts',(0.5,36.8978178826767,8.20920431569501));
#78460=CARTESIAN_POINT('',(0.499999999999998,37.0469778992348,7.50742489363772));
#78461=CARTESIAN_POINT('Origin',(0.499999999999998,0.,0.));
#78462=CARTESIAN_POINT('Ctrl Pts',(0.500000000000004,37.0469778992348,7.50742489363772));
#78463=CARTESIAN_POINT('Ctrl Pts',(0.248313959403557,36.7946496396261,7.48534903143474));
#78464=CARTESIAN_POINT('Ctrl Pts',(-1.04083408558608E-16,36.545659042501,
7.46356517686174));
#78465=CARTESIAN_POINT('Origin',(0.,43.4621548093593,8.06868014778688));
#78466=CARTESIAN_POINT('',(22.,34.0979246472968,7.24941616595889));
#78467=CARTESIAN_POINT('',(22.,38.4167373519446,7.62726331750731));
#78468=CARTESIAN_POINT('',(0.,34.0979246472968,7.24941616595889));
#78469=CARTESIAN_POINT('',(11.,37.0469778992348,7.50742489363772));
#78470=CARTESIAN_POINT('Origin',(0.,34.8387484606519,-1.21823876782095));
#78471=CARTESIAN_POINT('',(11.,37.7878017125899,-0.960230040142118));
#78472=CARTESIAN_POINT('',(22.,34.8387484606519,-1.21823876782095));
#78473=CARTESIAN_POINT('',(0.,34.8387484606519,-1.21823876782095));
#78474=CARTESIAN_POINT('',(22.,34.4754460842685,-1.25002360718652));
#78475=CARTESIAN_POINT('Origin',(0.,34.0979246472968,7.24941616595889));
#78476=CARTESIAN_POINT('',(22.,34.4122647000319,3.65649292234502));
#78477=CARTESIAN_POINT('Origin',(11.,0.,0.));
#78478=CARTESIAN_POINT('',(11.,36.8978178826767,8.20920431569501));
#78479=CARTESIAN_POINT('Origin',(21.55,0.,0.));
#78480=CARTESIAN_POINT('',(21.3357142857143,40.9563385449745,9.52789761644379));
#78481=CARTESIAN_POINT('',(22.,40.3644845257006,9.33559258828708));
#78482=CARTESIAN_POINT('Ctrl Pts',(21.3357142857143,40.9563385449745,9.52789761644379));
#78483=CARTESIAN_POINT('Ctrl Pts',(21.6703423800909,40.6582137039501,9.43103098365865));
#78484=CARTESIAN_POINT('Ctrl Pts',(22.,40.3644845257006,9.33559258828708));
#78485=CARTESIAN_POINT('',(21.3357142857143,40.2331784341656,12.2267678919897));
#78486=CARTESIAN_POINT('Ctrl Pts',(21.3357142857143,40.2331784341656,12.2267678919897));
#78487=CARTESIAN_POINT('Ctrl Pts',(21.385443740297,40.5947584895701,10.8773327542167));
#78488=CARTESIAN_POINT('Ctrl Pts',(21.3357142857143,40.9563385449745,9.52789761644379));
#78489=CARTESIAN_POINT('',(22.,39.6244653040641,12.0973819220119));
#78490=CARTESIAN_POINT('Ctrl Pts',(22.,39.6244653040641,12.0973819220119));
#78491=CARTESIAN_POINT('Ctrl Pts',(21.670342377286,39.9265614345165,12.1615944367947));
#78492=CARTESIAN_POINT('Ctrl Pts',(21.3357142857143,40.2331784341656,12.2267678919897));
#78493=CARTESIAN_POINT('Origin',(22.,0.,0.));
#78494=CARTESIAN_POINT('Origin',(21.55,0.,0.));
#78495=CARTESIAN_POINT('',(21.3357142857143,38.6796176759911,16.4951409948251));
#78496=CARTESIAN_POINT('',(22.,38.1301486668543,16.2029831402613));
#78497=CARTESIAN_POINT('Ctrl Pts',(21.3357142857143,38.6796176759911,16.4951409948251));
#78498=CARTESIAN_POINT('Ctrl Pts',(21.6703423781672,38.4028427370355,16.3479771493348));
#78499=CARTESIAN_POINT('Ctrl Pts',(22.,38.1301486668543,16.2029831402613));
#78500=CARTESIAN_POINT('',(21.3357142857143,37.4987900870893,19.0274339311535));
#78501=CARTESIAN_POINT('Ctrl Pts',(21.3357142857143,37.4987900870893,19.0274339311535));
#78502=CARTESIAN_POINT('Ctrl Pts',(21.385443740297,38.0892038815402,17.7612874629893));
#78503=CARTESIAN_POINT('Ctrl Pts',(21.3357142857143,38.6796176759911,16.4951409948251));
#78504=CARTESIAN_POINT('',(22.,36.9217923151073,18.7943116990243));
#78505=CARTESIAN_POINT('Ctrl Pts',(22.,36.9217923151073,18.7943116990243));
#78506=CARTESIAN_POINT('Ctrl Pts',(21.6703423774372,37.2081485402251,18.9100071239031));
#78507=CARTESIAN_POINT('Ctrl Pts',(21.3357142857143,37.4987900870893,19.0274339311535));
#78508=CARTESIAN_POINT('Origin',(22.,0.,0.));
#78509=CARTESIAN_POINT('Origin',(21.55,0.,0.));
#78510=CARTESIAN_POINT('',(21.3357142857143,35.2276361967536,22.9611878610227));
#78511=CARTESIAN_POINT('',(22.,34.7372475355518,22.5780542486238));
#78512=CARTESIAN_POINT('Ctrl Pts',(21.3357142857143,35.2276361967536,22.9611878610227));
#78513=CARTESIAN_POINT('Ctrl Pts',(21.670342378474,34.9806208243921,22.7681983010704));
#78514=CARTESIAN_POINT('Ctrl Pts',(22.,34.7372475355518,22.5780542486238));
#78515=CARTESIAN_POINT('',(21.3357142857143,33.6250199785202,25.2499610186653));
#78516=CARTESIAN_POINT('Ctrl Pts',(21.3357142857143,33.6250199785202,25.2499610186653));
#78517=CARTESIAN_POINT('Ctrl Pts',(21.385443740297,34.4263280876369,24.105574439844));
#78518=CARTESIAN_POINT('Ctrl Pts',(21.3357142857143,35.2276361967536,22.9611878610227));
#78519=CARTESIAN_POINT('',(22.,33.0972693499844,24.9201858254425));
#78520=CARTESIAN_POINT('Ctrl Pts',(22.,33.0972693499844,24.9201858254425));
#78521=CARTESIAN_POINT('Ctrl Pts',(21.6703423824005,33.3591848769665,25.0838488110428));
#78522=CARTESIAN_POINT('Ctrl Pts',(21.3357142857143,33.6250199785202,25.2499610186653));
#78523=CARTESIAN_POINT('Origin',(22.,0.,0.));
#78524=CARTESIAN_POINT('Origin',(21.55,0.,0.));
#78525=CARTESIAN_POINT('',(21.3357142857143,30.7052808177218,28.7295706529848));
#78526=CARTESIAN_POINT('',(22.,30.288872715777,28.2671026036886));
#78527=CARTESIAN_POINT('Ctrl Pts',(21.3357142857143,30.7052808177218,28.7295706529848));
#78528=CARTESIAN_POINT('Ctrl Pts',(21.6703423793899,30.4955304487274,28.4966192681895));
#78529=CARTESIAN_POINT('Ctrl Pts',(22.,30.288872715777,28.2671026036886));
#78530=CARTESIAN_POINT('',(21.3357142857143,28.7295706529848,30.7052808177218));
#78531=CARTESIAN_POINT('Ctrl Pts',(21.3357142857143,28.7295706529848,30.7052808177218));
#78532=CARTESIAN_POINT('Ctrl Pts',(21.385443740297,29.7174257353533,29.7174257353533));
#78533=CARTESIAN_POINT('Ctrl Pts',(21.3357142857143,30.7052808177218,28.7295706529848));
#78534=CARTESIAN_POINT('',(22.,28.2671026036886,30.288872715777));
#78535=CARTESIAN_POINT('Ctrl Pts',(22.,28.2671026036886,30.288872715777));
#78536=CARTESIAN_POINT('Ctrl Pts',(21.6703423804808,28.4966192674301,30.4955304480436));
#78537=CARTESIAN_POINT('Ctrl Pts',(21.3357142857143,28.7295706529848,30.7052808177218));
#78538=CARTESIAN_POINT('Origin',(22.,0.,0.));
#78539=CARTESIAN_POINT('Origin',(21.55,0.,0.));
#78540=CARTESIAN_POINT('',(21.3357142857143,25.2499610186653,33.6250199785202));
#78541=CARTESIAN_POINT('',(22.,24.9201858254425,33.0972693499844));
#78542=CARTESIAN_POINT('Ctrl Pts',(21.3357142857143,25.2499610186653,33.6250199785202));
#78543=CARTESIAN_POINT('Ctrl Pts',(21.6703423822881,25.0838488110986,33.3591848770558));
#78544=CARTESIAN_POINT('Ctrl Pts',(22.,24.9201858254425,33.0972693499844));
#78545=CARTESIAN_POINT('',(21.3357142857143,22.9611878610227,35.2276361967536));
#78546=CARTESIAN_POINT('Ctrl Pts',(21.3357142857143,22.9611878610227,35.2276361967536));
#78547=CARTESIAN_POINT('Ctrl Pts',(21.385443740297,24.105574439844,34.4263280876369));
#78548=CARTESIAN_POINT('Ctrl Pts',(21.3357142857143,25.2499610186653,33.6250199785202));
#78549=CARTESIAN_POINT('',(22.,22.5780542486238,34.7372475355518));
#78550=CARTESIAN_POINT('Ctrl Pts',(22.,22.5780542486238,34.7372475355518));
#78551=CARTESIAN_POINT('Ctrl Pts',(21.6703423746987,22.7681983032475,34.9806208271787));
#78552=CARTESIAN_POINT('Ctrl Pts',(21.3357142857143,22.9611878610227,35.2276361967536));
#78553=CARTESIAN_POINT('Origin',(22.,0.,0.));
#78554=CARTESIAN_POINT('Origin',(21.55,0.,0.));
#78555=CARTESIAN_POINT('',(21.3357142857143,19.0274339311535,37.4987900870893));
#78556=CARTESIAN_POINT('',(22.,18.7943116990243,36.9217923151073));
#78557=CARTESIAN_POINT('Ctrl Pts',(21.3357142857143,19.0274339311535,37.4987900870893));
#78558=CARTESIAN_POINT('Ctrl Pts',(21.670342376995,18.9100071240582,37.2081485406091));
#78559=CARTESIAN_POINT('Ctrl Pts',(22.,18.7943116990243,36.9217923151073));
#78560=CARTESIAN_POINT('',(21.3357142857143,16.4951409948251,38.6796176759911));
#78561=CARTESIAN_POINT('Ctrl Pts',(21.3357142857143,16.4951409948251,38.6796176759911));
#78562=CARTESIAN_POINT('Ctrl Pts',(21.385443740297,17.7612874629893,38.0892038815402));
#78563=CARTESIAN_POINT('Ctrl Pts',(21.3357142857143,19.0274339311535,37.4987900870893));
#78564=CARTESIAN_POINT('',(22.,16.2029831402613,38.1301486668542));
#78565=CARTESIAN_POINT('Ctrl Pts',(22.,16.2029831402613,38.1301486668543));
#78566=CARTESIAN_POINT('Ctrl Pts',(21.6703423781921,16.3479771493239,38.4028427370149));
#78567=CARTESIAN_POINT('Ctrl Pts',(21.3357142857143,16.4951409948251,38.6796176759911));
#78568=CARTESIAN_POINT('Origin',(22.,0.,0.));
#78569=CARTESIAN_POINT('Origin',(21.55,0.,0.));
#78570=CARTESIAN_POINT('',(21.3357142857143,12.2267678919897,40.2331784341656));
#78571=CARTESIAN_POINT('',(22.,12.097381922012,39.6244653040641));
#78572=CARTESIAN_POINT('Ctrl Pts',(21.3357142857143,12.2267678919897,40.2331784341656));
#78573=CARTESIAN_POINT('Ctrl Pts',(21.6703423713064,12.1615944379593,39.9265614399951));
#78574=CARTESIAN_POINT('Ctrl Pts',(22.,12.097381922012,39.6244653040641));
#78575=CARTESIAN_POINT('',(21.3357142857143,9.5278976164438,40.9563385449745));
#78576=CARTESIAN_POINT('Ctrl Pts',(21.3357142857143,9.5278976164438,40.9563385449745));
#78577=CARTESIAN_POINT('Ctrl Pts',(21.385443740297,10.8773327542168,40.5947584895701));
#78578=CARTESIAN_POINT('Ctrl Pts',(21.3357142857143,12.2267678919897,40.2331784341656));
#78579=CARTESIAN_POINT('',(22.,9.33559258828709,40.3644845257006));
#78580=CARTESIAN_POINT('Ctrl Pts',(22.,9.33559258828708,40.3644845257006));
#78581=CARTESIAN_POINT('Ctrl Pts',(21.6703423800867,9.43103098365986,40.6582137039538));
#78582=CARTESIAN_POINT('Ctrl Pts',(21.3357142857143,9.5278976164438,40.9563385449745));
#78583=CARTESIAN_POINT('Origin',(22.,0.,0.));
#78584=CARTESIAN_POINT('Origin',(21.55,0.,0.));
#78585=CARTESIAN_POINT('',(21.3357142857143,5.05459769747092,41.7451020134904));
#78586=CARTESIAN_POINT('',(22.,5.03287931686986,41.1231689657038));
#78587=CARTESIAN_POINT('Ctrl Pts',(21.3357142857143,5.05459769747092,41.7451020134904));
#78588=CARTESIAN_POINT('Ctrl Pts',(21.6703423747022,5.04365785681953,41.4318259657226));
#78589=CARTESIAN_POINT('Ctrl Pts',(22.,5.03287931686986,41.1231689657038));
#78590=CARTESIAN_POINT('',(21.3357142857143,2.27115389033571,41.9886217921762));
#78591=CARTESIAN_POINT('Ctrl Pts',(21.3357142857143,2.27115389033571,41.9886217921762));
#78592=CARTESIAN_POINT('Ctrl Pts',(21.385443740297,3.66287579390336,41.8668619028333));
#78593=CARTESIAN_POINT('Ctrl Pts',(21.3357142857143,5.05459769747092,41.7451020134904));
#78594=CARTESIAN_POINT('',(22.,2.18454477955552,41.3723659476482));
#78595=CARTESIAN_POINT('Ctrl Pts',(22.,2.18454477955552,41.3723659476482));
#78596=CARTESIAN_POINT('Ctrl Pts',(21.670342377366,2.22752771507708,41.6782054256375));
#78597=CARTESIAN_POINT('Ctrl Pts',(21.3357142857143,2.27115389033571,41.9886217921762));
#78598=CARTESIAN_POINT('Origin',(22.,0.,0.));
#78599=CARTESIAN_POINT('Origin',(21.55,0.,0.));
#78600=CARTESIAN_POINT('',(21.3357142857143,-2.2711538903357,41.9886217921762));
#78601=CARTESIAN_POINT('',(22.,-2.18454477955551,41.3723659476482));
#78602=CARTESIAN_POINT('Ctrl Pts',(21.3357142857143,-2.2711538903357,41.9886217921762));
#78603=CARTESIAN_POINT('Ctrl Pts',(21.6703423740032,-2.22752771551545,41.6782054287567));
#78604=CARTESIAN_POINT('Ctrl Pts',(22.,-2.18454477955551,41.3723659476482));
#78605=CARTESIAN_POINT('',(21.3357142857143,-5.05459769747091,41.7451020134904));
#78606=CARTESIAN_POINT('Ctrl Pts',(21.3357142857143,-5.05459769747091,41.7451020134904));
#78607=CARTESIAN_POINT('Ctrl Pts',(21.385443740297,-3.66287579390327,41.8668619028333));
#78608=CARTESIAN_POINT('Ctrl Pts',(21.3357142857143,-2.27115389033571,41.9886217921762));
#78609=CARTESIAN_POINT('',(22.,-5.03287931686985,41.1231689657038));
#78610=CARTESIAN_POINT('Ctrl Pts',(22.,-5.03287931686985,41.1231689657038));
#78611=CARTESIAN_POINT('Ctrl Pts',(21.6703423749418,-5.04365785681169,41.4318259654982));
#78612=CARTESIAN_POINT('Ctrl Pts',(21.3357142857143,-5.05459769747091,41.7451020134904));
#78613=CARTESIAN_POINT('Origin',(22.,0.,0.));
#78614=CARTESIAN_POINT('Origin',(21.55,0.,0.));
#78615=CARTESIAN_POINT('',(21.3357142857143,-9.52789761644379,40.9563385449745));
#78616=CARTESIAN_POINT('',(22.,-9.33559258828708,40.3644845257006));
#78617=CARTESIAN_POINT('Ctrl Pts',(21.3357142857143,-9.52789761644379,40.9563385449745));
#78618=CARTESIAN_POINT('Ctrl Pts',(21.6703423801097,-9.43103098365321,40.6582137039333));
#78619=CARTESIAN_POINT('Ctrl Pts',(22.,-9.33559258828708,40.3644845257006));
#78620=CARTESIAN_POINT('',(21.3357142857143,-12.2267678919897,40.2331784341656));
#78621=CARTESIAN_POINT('Ctrl Pts',(21.3357142857143,-12.2267678919897,40.2331784341656));
#78622=CARTESIAN_POINT('Ctrl Pts',(21.385443740297,-10.8773327542167,40.5947584895701));
#78623=CARTESIAN_POINT('Ctrl Pts',(21.3357142857143,-9.52789761644379,40.9563385449745));
#78624=CARTESIAN_POINT('',(22.,-12.0973819220119,39.6244653040641));
#78625=CARTESIAN_POINT('Ctrl Pts',(22.,-12.0973819220119,39.6244653040641));
#78626=CARTESIAN_POINT('Ctrl Pts',(21.6703423772675,-12.1615944367983,39.9265614345335));
#78627=CARTESIAN_POINT('Ctrl Pts',(21.3357142857143,-12.2267678919897,40.2331784341656));
#78628=CARTESIAN_POINT('Origin',(22.,0.,0.));
#78629=CARTESIAN_POINT('Origin',(21.55,0.,0.));
#78630=CARTESIAN_POINT('',(21.3357142857143,-16.4951409948251,38.6796176759911));
#78631=CARTESIAN_POINT('',(22.,-16.2029831402613,38.1301486668543));
#78632=CARTESIAN_POINT('Ctrl Pts',(21.3357142857143,-16.4951409948251,38.6796176759911));
#78633=CARTESIAN_POINT('Ctrl Pts',(21.6703423749317,-16.3479771507576,38.4028427397114));
#78634=CARTESIAN_POINT('Ctrl Pts',(22.,-16.2029831402613,38.1301486668543));
#78635=CARTESIAN_POINT('',(21.3357142857143,-19.0274339311535,37.4987900870893));
#78636=CARTESIAN_POINT('Ctrl Pts',(21.3357142857143,-19.0274339311535,37.4987900870893));
#78637=CARTESIAN_POINT('Ctrl Pts',(21.385443740297,-17.7612874629893,38.0892038815402));
#78638=CARTESIAN_POINT('Ctrl Pts',(21.3357142857143,-16.4951409948251,38.6796176759911));
#78639=CARTESIAN_POINT('',(22.,-18.7943116990243,36.9217923151073));
#78640=CARTESIAN_POINT('Ctrl Pts',(22.,-18.7943116990243,36.9217923151073));
#78641=CARTESIAN_POINT('Ctrl Pts',(21.6703423742972,-18.9100071250049,37.2081485429521));
#78642=CARTESIAN_POINT('Ctrl Pts',(21.3357142857143,-19.0274339311535,37.4987900870893));
#78643=CARTESIAN_POINT('Origin',(22.,0.,0.));
#78644=CARTESIAN_POINT('Origin',(21.55,0.,0.));
#78645=CARTESIAN_POINT('',(21.3357142857143,-28.7295706529848,30.7052808177218));
#78646=CARTESIAN_POINT('',(22.,-28.2671026036886,30.288872715777));
#78647=CARTESIAN_POINT('Ctrl Pts',(21.3357142857143,-28.7295706529848,30.7052808177218));
#78648=CARTESIAN_POINT('Ctrl Pts',(21.6703423825864,-28.4966192659645,30.4955304467239));
#78649=CARTESIAN_POINT('Ctrl Pts',(22.,-28.2671026036886,30.288872715777));
#78650=CARTESIAN_POINT('',(21.3357142857143,-30.7052808177218,28.7295706529848));
#78651=CARTESIAN_POINT('Ctrl Pts',(21.3357142857143,-30.7052808177218,28.7295706529848));
#78652=CARTESIAN_POINT('Ctrl Pts',(21.385443740297,-29.7174257353533,29.7174257353533));
#78653=CARTESIAN_POINT('Ctrl Pts',(21.3357142857143,-28.7295706529848,30.7052808177218));
#78654=CARTESIAN_POINT('',(22.,-30.288872715777,28.2671026036886));
#78655=CARTESIAN_POINT('Ctrl Pts',(22.,-30.288872715777,28.2671026036886));
#78656=CARTESIAN_POINT('Ctrl Pts',(21.6703423803358,-30.4955304481345,28.4966192675311));
#78657=CARTESIAN_POINT('Ctrl Pts',(21.3357142857143,-30.7052808177218,28.7295706529848));
#78658=CARTESIAN_POINT('Origin',(22.,0.,0.));
#78659=CARTESIAN_POINT('Origin',(21.55,0.,0.));
#78660=CARTESIAN_POINT('',(21.3357142857143,-33.6250199785202,25.2499610186654));
#78661=CARTESIAN_POINT('',(22.,-33.0972693499844,24.9201858254425));
#78662=CARTESIAN_POINT('Ctrl Pts',(21.3357142857143,-33.6250199785202,25.2499610186654));
#78663=CARTESIAN_POINT('Ctrl Pts',(21.6703423791589,-33.3591848795415,25.0838488126518));
#78664=CARTESIAN_POINT('Ctrl Pts',(22.,-33.0972693499844,24.9201858254425));
#78665=CARTESIAN_POINT('',(21.3357142857143,-35.2276361967536,22.9611878610227));
#78666=CARTESIAN_POINT('Ctrl Pts',(21.3357142857143,-35.2276361967536,22.9611878610227));
#78667=CARTESIAN_POINT('Ctrl Pts',(21.385443740297,-34.4263280876369,24.1055744398441));
#78668=CARTESIAN_POINT('Ctrl Pts',(21.3357142857143,-33.6250199785202,25.2499610186654));
#78669=CARTESIAN_POINT('',(22.,-34.7372475355518,22.5780542486238));
#78670=CARTESIAN_POINT('Ctrl Pts',(22.,-34.7372475355518,22.5780542486238));
#78671=CARTESIAN_POINT('Ctrl Pts',(21.6703423746934,-34.9806208271825,22.7681983032506));
#78672=CARTESIAN_POINT('Ctrl Pts',(21.3357142857143,-35.2276361967536,22.9611878610227));
#78673=CARTESIAN_POINT('Origin',(22.,0.,0.));
#78674=CARTESIAN_POINT('Origin',(21.55,0.,0.));
#78675=CARTESIAN_POINT('',(21.3357142857143,-37.4987900870893,19.0274339311535));
#78676=CARTESIAN_POINT('',(22.,-36.9217923151073,18.7943116990243));
#78677=CARTESIAN_POINT('Ctrl Pts',(21.3357142857143,-37.4987900870893,19.0274339311535));
#78678=CARTESIAN_POINT('Ctrl Pts',(21.6703423777508,-37.2081485399528,18.9100071237931));
#78679=CARTESIAN_POINT('Ctrl Pts',(22.,-36.9217923151073,18.7943116990243));
#78680=CARTESIAN_POINT('',(21.3357142857143,-38.6796176759911,16.4951409948251));
#78681=CARTESIAN_POINT('Ctrl Pts',(21.3357142857143,-38.6796176759911,16.4951409948251));
#78682=CARTESIAN_POINT('Ctrl Pts',(21.385443740297,-38.0892038815402,17.7612874629893));
#78683=CARTESIAN_POINT('Ctrl Pts',(21.3357142857143,-37.4987900870893,19.0274339311535));
#78684=CARTESIAN_POINT('',(22.,-38.1301486668543,16.2029831402613));
#78685=CARTESIAN_POINT('Ctrl Pts',(22.,-38.1301486668543,16.2029831402613));
#78686=CARTESIAN_POINT('Ctrl Pts',(21.670342380746,-38.4028427349027,16.3479771482008));
#78687=CARTESIAN_POINT('Ctrl Pts',(21.3357142857143,-38.6796176759911,16.4951409948251));
#78688=CARTESIAN_POINT('Origin',(22.,0.,0.));
#78689=CARTESIAN_POINT('Origin',(21.55,0.,0.));
#78690=CARTESIAN_POINT('',(21.3357142857143,-40.2331784341656,12.2267678919897));
#78691=CARTESIAN_POINT('',(22.,-39.6244653040641,12.097381922012));
#78692=CARTESIAN_POINT('Ctrl Pts',(21.3357142857143,-40.2331784341656,12.2267678919897));
#78693=CARTESIAN_POINT('Ctrl Pts',(21.670342374299,-39.9265614372533,12.1615944373765));
#78694=CARTESIAN_POINT('Ctrl Pts',(22.,-39.6244653040641,12.097381922012));
#78695=CARTESIAN_POINT('',(21.3357142857143,-40.9563385449745,9.5278976164438));
#78696=CARTESIAN_POINT('Ctrl Pts',(21.3357142857143,-40.9563385449745,9.5278976164438));
#78697=CARTESIAN_POINT('Ctrl Pts',(21.385443740297,-40.5947584895701,10.8773327542168));
#78698=CARTESIAN_POINT('Ctrl Pts',(21.3357142857143,-40.2331784341656,12.2267678919897));
#78699=CARTESIAN_POINT('',(22.,-40.3644845257006,9.33559258828709));
#78700=CARTESIAN_POINT('Ctrl Pts',(22.,-40.3644845257006,9.33559258828709));
#78701=CARTESIAN_POINT('Ctrl Pts',(21.6703423770111,-40.6582137066937,9.4310309845501));
#78702=CARTESIAN_POINT('Ctrl Pts',(21.3357142857143,-40.9563385449745,9.5278976164438));
#78703=CARTESIAN_POINT('Origin',(22.,0.,0.));
#78704=CARTESIAN_POINT('Origin',(21.55,0.,0.));
#78705=CARTESIAN_POINT('',(21.3357142857143,-41.7451020134904,5.05459769747093));
#78706=CARTESIAN_POINT('',(22.,-41.1231689657038,5.03287931686987));
#78707=CARTESIAN_POINT('Ctrl Pts',(21.3357142857143,-41.7451020134904,5.05459769747093));
#78708=CARTESIAN_POINT('Ctrl Pts',(21.6703423749518,-41.4318259654889,5.04365785681138));
#78709=CARTESIAN_POINT('Ctrl Pts',(22.,-41.1231689657038,5.03287931686987));
#78710=CARTESIAN_POINT('',(21.3357142857143,-41.9886217921762,2.27115389033572));
#78711=CARTESIAN_POINT('Ctrl Pts',(21.3357142857143,-41.9886217921762,2.27115389033572));
#78712=CARTESIAN_POINT('Ctrl Pts',(21.385443740297,-41.8668619028333,3.66287579390337));
#78713=CARTESIAN_POINT('Ctrl Pts',(21.3357142857143,-41.7451020134904,5.05459769747093));
#78714=CARTESIAN_POINT('',(22.,-41.3723659476482,2.18454477955553));
#78715=CARTESIAN_POINT('Ctrl Pts',(22.,-41.3723659476482,2.18454477955553));
#78716=CARTESIAN_POINT('Ctrl Pts',(21.6703423713149,-41.6782054312502,2.22752771586591));
#78717=CARTESIAN_POINT('Ctrl Pts',(21.3357142857143,-41.9886217921762,2.27115389033572));
#78718=CARTESIAN_POINT('Origin',(22.,0.,0.));
#78719=CARTESIAN_POINT('Origin',(21.55,0.,0.));
#78720=CARTESIAN_POINT('',(21.3357142857143,-41.9886217921762,-2.2711538903357));
#78721=CARTESIAN_POINT('',(22.,-41.3723659476482,-2.18454477955551));
#78722=CARTESIAN_POINT('Ctrl Pts',(21.3357142857143,-41.9886217921762,-2.2711538903357));
#78723=CARTESIAN_POINT('Ctrl Pts',(21.6703423741524,-41.6782054286182,-2.22752771549599));
#78724=CARTESIAN_POINT('Ctrl Pts',(22.,-41.3723659476482,-2.18454477955551));
#78725=CARTESIAN_POINT('',(21.3357142857143,-41.7451020134904,-5.0545976974709));
#78726=CARTESIAN_POINT('Ctrl Pts',(21.3357142857143,-41.7451020134904,-5.0545976974709));
#78727=CARTESIAN_POINT('Ctrl Pts',(21.385443740297,-41.8668619028333,-3.66287579390326));
#78728=CARTESIAN_POINT('Ctrl Pts',(21.3357142857143,-41.9886217921762,-2.2711538903357));
#78729=CARTESIAN_POINT('',(22.,-41.1231689657038,-5.03287931686985));
#78730=CARTESIAN_POINT('Ctrl Pts',(22.,-41.1231689657038,-5.03287931686985));
#78731=CARTESIAN_POINT('Ctrl Pts',(21.6703423748145,-41.4318259656174,-5.04365785681585));
#78732=CARTESIAN_POINT('Ctrl Pts',(21.3357142857143,-41.7451020134904,-5.0545976974709));
#78733=CARTESIAN_POINT('Origin',(22.,0.,0.));
#78734=CARTESIAN_POINT('Origin',(21.55,0.,0.));
#78735=CARTESIAN_POINT('',(21.3357142857143,-40.9563385449745,-9.52789761644378));
#78736=CARTESIAN_POINT('',(22.,-40.3644845257006,-9.33559258828707));
#78737=CARTESIAN_POINT('Ctrl Pts',(21.3357142857143,-40.9563385449745,-9.52789761644378));
#78738=CARTESIAN_POINT('Ctrl Pts',(21.670342374081,-40.6582137093039,-9.43103098539821));
#78739=CARTESIAN_POINT('Ctrl Pts',(22.,-40.3644845257006,-9.33559258828707));
#78740=CARTESIAN_POINT('',(21.3357142857143,-40.2331784341656,-12.2267678919897));
#78741=CARTESIAN_POINT('Ctrl Pts',(21.3357142857143,-40.2331784341656,-12.2267678919897));
#78742=CARTESIAN_POINT('Ctrl Pts',(21.385443740297,-40.5947584895701,-10.8773327542167));
#78743=CARTESIAN_POINT('Ctrl Pts',(21.3357142857143,-40.9563385449745,-9.52789761644378));
#78744=CARTESIAN_POINT('',(22.,-39.6244653040641,-12.0973819220119));
#78745=CARTESIAN_POINT('Ctrl Pts',(22.,-39.6244653040641,-12.0973819220119));
#78746=CARTESIAN_POINT('Ctrl Pts',(21.6703423801992,-39.9265614318475,-12.1615944362274));
#78747=CARTESIAN_POINT('Ctrl Pts',(21.3357142857143,-40.2331784341656,-12.2267678919897));
#78748=CARTESIAN_POINT('Origin',(22.,0.,0.));
#78749=CARTESIAN_POINT('Origin',(21.55,0.,0.));
#78750=CARTESIAN_POINT('',(21.3357142857143,-38.6796176759911,-16.4951409948251));
#78751=CARTESIAN_POINT('',(22.,-38.1301486668543,-16.2029831402613));
#78752=CARTESIAN_POINT('Ctrl Pts',(21.3357142857143,-38.6796176759911,-16.4951409948251));
#78753=CARTESIAN_POINT('Ctrl Pts',(21.670342377579,-38.402842737522,-16.3479771495935));
#78754=CARTESIAN_POINT('Ctrl Pts',(22.,-38.1301486668543,-16.2029831402613));
#78755=CARTESIAN_POINT('',(21.3357142857143,-37.4987900870893,-19.0274339311535));
#78756=CARTESIAN_POINT('Ctrl Pts',(21.3357142857143,-37.4987900870893,-19.0274339311535));
#78757=CARTESIAN_POINT('Ctrl Pts',(21.385443740297,-38.0892038815402,-17.7612874629892));
#78758=CARTESIAN_POINT('Ctrl Pts',(21.3357142857143,-38.6796176759911,-16.4951409948251));
#78759=CARTESIAN_POINT('',(22.,-36.9217923151073,-18.7943116990243));
#78760=CARTESIAN_POINT('Ctrl Pts',(22.,-36.9217923151073,-18.7943116990243));
#78761=CARTESIAN_POINT('Ctrl Pts',(21.6703423805662,-37.2081485375077,-18.9100071228052));
#78762=CARTESIAN_POINT('Ctrl Pts',(21.3357142857143,-37.4987900870893,-19.0274339311535));
#78763=CARTESIAN_POINT('Origin',(22.,0.,0.));
#78764=CARTESIAN_POINT('Origin',(21.55,0.,0.));
#78765=CARTESIAN_POINT('',(21.3357142857143,-35.2276361967536,-22.9611878610227));
#78766=CARTESIAN_POINT('',(22.,-34.7372475355518,-22.5780542486238));
#78767=CARTESIAN_POINT('Ctrl Pts',(21.3357142857143,-35.2276361967536,-22.9611878610227));
#78768=CARTESIAN_POINT('Ctrl Pts',(21.6703423786233,-34.9806208242819,-22.7681983009843));
#78769=CARTESIAN_POINT('Ctrl Pts',(22.,-34.7372475355518,-22.5780542486238));
#78770=CARTESIAN_POINT('',(21.3357142857143,-33.6250199785202,-25.2499610186653));
#78771=CARTESIAN_POINT('Ctrl Pts',(21.3357142857143,-33.6250199785202,-25.2499610186653));
#78772=CARTESIAN_POINT('Ctrl Pts',(21.385443740297,-34.4263280876369,-24.105574439844));
#78773=CARTESIAN_POINT('Ctrl Pts',(21.3357142857143,-35.2276361967536,-22.9611878610227));
#78774=CARTESIAN_POINT('',(22.,-33.0972693499844,-24.9201858254425));
#78775=CARTESIAN_POINT('Ctrl Pts',(22.,-33.0972693499844,-24.9201858254425));
#78776=CARTESIAN_POINT('Ctrl Pts',(21.670342369686,-33.3591848870663,-25.0838488173538));
#78777=CARTESIAN_POINT('Ctrl Pts',(21.3357142857143,-33.6250199785202,-25.2499610186653));
#78778=CARTESIAN_POINT('Origin',(22.,0.,0.));
#78779=CARTESIAN_POINT('Origin',(21.55,0.,0.));
#78780=CARTESIAN_POINT('',(21.3357142857143,-30.7052808177218,-28.7295706529848));
#78781=CARTESIAN_POINT('',(22.,-30.288872715777,-28.2671026036886));
#78782=CARTESIAN_POINT('Ctrl Pts',(21.3357142857143,-30.7052808177218,-28.7295706529848));
#78783=CARTESIAN_POINT('Ctrl Pts',(21.6703423793899,-30.4955304487274,-28.4966192681895));
#78784=CARTESIAN_POINT('Ctrl Pts',(22.,-30.288872715777,-28.2671026036886));
#78785=CARTESIAN_POINT('',(21.3357142857143,-28.7295706529848,-30.7052808177218));
#78786=CARTESIAN_POINT('Ctrl Pts',(21.3357142857143,-28.7295706529848,-30.7052808177218));
#78787=CARTESIAN_POINT('Ctrl Pts',(21.385443740297,-29.7174257353533,-29.7174257353533));
#78788=CARTESIAN_POINT('Ctrl Pts',(21.3357142857143,-30.7052808177218,-28.7295706529848));
#78789=CARTESIAN_POINT('',(22.,-28.2671026036886,-30.288872715777));
#78790=CARTESIAN_POINT('Ctrl Pts',(22.,-28.2671026036886,-30.288872715777));
#78791=CARTESIAN_POINT('Ctrl Pts',(21.6703423804808,-28.4966192674301,-30.4955304480436));
#78792=CARTESIAN_POINT('Ctrl Pts',(21.3357142857143,-28.7295706529848,-30.7052808177218));
#78793=CARTESIAN_POINT('Origin',(22.,0.,0.));
#78794=CARTESIAN_POINT('Origin',(21.55,0.,0.));
#78795=CARTESIAN_POINT('',(21.3357142857143,-25.2499610186654,-33.6250199785202));
#78796=CARTESIAN_POINT('',(22.,-24.9201858254425,-33.0972693499844));
#78797=CARTESIAN_POINT('Ctrl Pts',(21.3357142857143,-25.2499610186654,-33.6250199785202));
#78798=CARTESIAN_POINT('Ctrl Pts',(21.6703423798578,-25.0838488123049,-33.3591848789864));
#78799=CARTESIAN_POINT('Ctrl Pts',(22.,-24.9201858254425,-33.0972693499844));
#78800=CARTESIAN_POINT('',(21.3357142857143,-22.9611878610227,-35.2276361967536));
#78801=CARTESIAN_POINT('Ctrl Pts',(21.3357142857143,-22.9611878610227,-35.2276361967536));
#78802=CARTESIAN_POINT('Ctrl Pts',(21.385443740297,-24.1055744398441,-34.4263280876369));
#78803=CARTESIAN_POINT('Ctrl Pts',(21.3357142857143,-25.2499610186654,-33.6250199785202));
#78804=CARTESIAN_POINT('',(22.,-22.5780542486238,-34.7372475355518));
#78805=CARTESIAN_POINT('Ctrl Pts',(22.,-22.5780542486238,-34.7372475355518));
#78806=CARTESIAN_POINT('Ctrl Pts',(21.670342374658,-22.768198303271,-34.9806208272087));
#78807=CARTESIAN_POINT('Ctrl Pts',(21.3357142857143,-22.9611878610227,-35.2276361967536));
#78808=CARTESIAN_POINT('Origin',(22.,0.,0.));
#78809=CARTESIAN_POINT('Origin',(21.55,0.,0.));
#78810=CARTESIAN_POINT('',(21.3357142857143,-12.2267678919898,-40.2331784341656));
#78811=CARTESIAN_POINT('',(22.,-12.097381922012,-39.6244653040641));
#78812=CARTESIAN_POINT('Ctrl Pts',(21.3357142857143,-12.2267678919898,-40.2331784341656));
#78813=CARTESIAN_POINT('Ctrl Pts',(21.6703423804963,-12.1615944361696,-39.9265614315752));
#78814=CARTESIAN_POINT('Ctrl Pts',(22.,-12.097381922012,-39.6244653040641));
#78815=CARTESIAN_POINT('',(21.3357142857143,-9.52789761644383,-40.9563385449745));
#78816=CARTESIAN_POINT('Ctrl Pts',(21.3357142857143,-9.52789761644383,-40.9563385449745));
#78817=CARTESIAN_POINT('Ctrl Pts',(21.385443740297,-10.8773327542168,-40.5947584895701));
#78818=CARTESIAN_POINT('Ctrl Pts',(21.3357142857143,-12.2267678919898,-40.2331784341656));
#78819=CARTESIAN_POINT('',(22.,-9.33559258828711,-40.3644845257006));
#78820=CARTESIAN_POINT('Ctrl Pts',(22.,-9.3355925882871,-40.3644845257006));
#78821=CARTESIAN_POINT('Ctrl Pts',(21.6703423830878,-9.43103098279123,-40.6582137012803));
#78822=CARTESIAN_POINT('Ctrl Pts',(21.3357142857143,-9.52789761644383,-40.9563385449745));
#78823=CARTESIAN_POINT('Origin',(22.,0.,0.));
#78824=CARTESIAN_POINT('Origin',(21.55,0.,0.));
#78825=CARTESIAN_POINT('',(21.3357142857143,-5.05459769747091,-41.7451020134904));
#78826=CARTESIAN_POINT('',(22.,-5.03287931686986,-41.1231689657038));
#78827=CARTESIAN_POINT('Ctrl Pts',(21.3357142857143,-5.05459769747091,-41.7451020134904));
#78828=CARTESIAN_POINT('Ctrl Pts',(21.6703423808798,-5.04365785661758,-41.4318259599396));
#78829=CARTESIAN_POINT('Ctrl Pts',(22.,-5.03287931686986,-41.1231689657038));
#78830=CARTESIAN_POINT('',(21.3357142857143,-2.27115389033571,-41.9886217921762));
#78831=CARTESIAN_POINT('Ctrl Pts',(21.3357142857143,-2.27115389033571,-41.9886217921762));
#78832=CARTESIAN_POINT('Ctrl Pts',(21.385443740297,-3.66287579390335,-41.8668619028333));
#78833=CARTESIAN_POINT('Ctrl Pts',(21.3357142857143,-5.05459769747091,-41.7451020134904));
#78834=CARTESIAN_POINT('',(22.,-2.18454477955551,-41.3723659476482));
#78835=CARTESIAN_POINT('Ctrl Pts',(22.,-2.18454477955551,-41.3723659476482));
#78836=CARTESIAN_POINT('Ctrl Pts',(21.670342377365,-2.2275277150772,-41.6782054256383));
#78837=CARTESIAN_POINT('Ctrl Pts',(21.3357142857143,-2.27115389033571,-41.9886217921762));
#78838=CARTESIAN_POINT('Origin',(22.,0.,0.));
#78839=CARTESIAN_POINT('Origin',(21.55,0.,0.));
#78840=CARTESIAN_POINT('',(21.3357142857143,2.2711538903357,-41.9886217921762));
#78841=CARTESIAN_POINT('',(22.,2.1845447795555,-41.3723659476482));
#78842=CARTESIAN_POINT('Ctrl Pts',(21.3357142857143,2.2711538903357,-41.9886217921762));
#78843=CARTESIAN_POINT('Ctrl Pts',(21.6703423741031,2.22752771550241,-41.678205428664));
#78844=CARTESIAN_POINT('Ctrl Pts',(22.,2.1845447795555,-41.3723659476482));
#78845=CARTESIAN_POINT('',(21.3357142857143,5.0545976974709,-41.7451020134904));
#78846=CARTESIAN_POINT('Ctrl Pts',(21.3357142857143,5.0545976974709,-41.7451020134904));
#78847=CARTESIAN_POINT('Ctrl Pts',(21.385443740297,3.66287579390326,-41.8668619028333));
#78848=CARTESIAN_POINT('Ctrl Pts',(21.3357142857143,2.2711538903357,-41.9886217921762));
#78849=CARTESIAN_POINT('',(22.,5.03287931686985,-41.1231689657038));
#78850=CARTESIAN_POINT('Ctrl Pts',(22.,5.03287931686985,-41.1231689657038));
#78851=CARTESIAN_POINT('Ctrl Pts',(21.6703423747918,5.04365785681659,-41.4318259656387));
#78852=CARTESIAN_POINT('Ctrl Pts',(21.3357142857143,5.0545976974709,-41.7451020134904));
#78853=CARTESIAN_POINT('Origin',(22.,0.,0.));
#78854=CARTESIAN_POINT('Origin',(21.55,0.,0.));
#78855=CARTESIAN_POINT('',(21.3357142857143,9.52789761644378,-40.9563385449745));
#78856=CARTESIAN_POINT('',(22.,9.33559258828707,-40.3644845257006));
#78857=CARTESIAN_POINT('Ctrl Pts',(21.3357142857143,9.52789761644378,-40.9563385449745));
#78858=CARTESIAN_POINT('Ctrl Pts',(21.670342374061,9.43103098540399,-40.6582137093217));
#78859=CARTESIAN_POINT('Ctrl Pts',(22.,9.33559258828707,-40.3644845257006));
#78860=CARTESIAN_POINT('',(21.3357142857143,12.2267678919897,-40.2331784341656));
#78861=CARTESIAN_POINT('Ctrl Pts',(21.3357142857143,12.2267678919897,-40.2331784341656));
#78862=CARTESIAN_POINT('Ctrl Pts',(21.385443740297,10.8773327542167,-40.5947584895701));
#78863=CARTESIAN_POINT('Ctrl Pts',(21.3357142857143,9.52789761644378,-40.9563385449745));
#78864=CARTESIAN_POINT('',(22.,12.0973819220119,-39.6244653040641));
#78865=CARTESIAN_POINT('Ctrl Pts',(22.,12.0973819220119,-39.6244653040641));
#78866=CARTESIAN_POINT('Ctrl Pts',(21.6703423744266,12.1615944373516,-39.9265614371364));
#78867=CARTESIAN_POINT('Ctrl Pts',(21.3357142857143,12.2267678919897,-40.2331784341656));
#78868=CARTESIAN_POINT('Origin',(22.,0.,0.));
#78869=CARTESIAN_POINT('Origin',(21.55,0.,0.));
#78870=CARTESIAN_POINT('',(21.3357142857143,16.4951409948251,-38.6796176759911));
#78871=CARTESIAN_POINT('',(22.,16.2029831402613,-38.1301486668543));
#78872=CARTESIAN_POINT('Ctrl Pts',(21.3357142857143,16.495140994825,-38.6796176759911));
#78873=CARTESIAN_POINT('Ctrl Pts',(21.6703423780787,16.3479771493738,-38.4028427371088));
#78874=CARTESIAN_POINT('Ctrl Pts',(22.,16.2029831402613,-38.1301486668543));
#78875=CARTESIAN_POINT('',(21.3357142857143,19.0274339311535,-37.4987900870893));
#78876=CARTESIAN_POINT('Ctrl Pts',(21.3357142857143,19.0274339311535,-37.4987900870893));
#78877=CARTESIAN_POINT('Ctrl Pts',(21.385443740297,17.7612874629892,-38.0892038815402));
#78878=CARTESIAN_POINT('Ctrl Pts',(21.3357142857143,16.4951409948251,-38.6796176759911));
#78879=CARTESIAN_POINT('',(22.,18.7943116990243,-36.9217923151073));
#78880=CARTESIAN_POINT('Ctrl Pts',(22.,18.7943116990243,-36.9217923151073));
#78881=CARTESIAN_POINT('Ctrl Pts',(21.6703423777322,18.9100071237995,-37.2081485399689));
#78882=CARTESIAN_POINT('Ctrl Pts',(21.3357142857143,19.0274339311535,-37.4987900870893));
#78883=CARTESIAN_POINT('Origin',(22.,0.,0.));
#78884=CARTESIAN_POINT('Origin',(21.55,0.,0.));
#78885=CARTESIAN_POINT('',(21.3357142857143,22.9611878610227,-35.2276361967536));
#78886=CARTESIAN_POINT('',(22.,22.5780542486238,-34.7372475355518));
#78887=CARTESIAN_POINT('Ctrl Pts',(21.3357142857143,22.9611878610227,-35.2276361967536));
#78888=CARTESIAN_POINT('Ctrl Pts',(21.6703423755923,22.7681983027322,-34.9806208265191));
#78889=CARTESIAN_POINT('Ctrl Pts',(22.,22.5780542486238,-34.7372475355518));
#78890=CARTESIAN_POINT('',(21.3357142857143,25.2499610186654,-33.6250199785202));
#78891=CARTESIAN_POINT('Ctrl Pts',(21.3357142857143,25.2499610186654,-33.6250199785202));
#78892=CARTESIAN_POINT('Ctrl Pts',(21.385443740297,24.105574439844,-34.4263280876369));
#78893=CARTESIAN_POINT('Ctrl Pts',(21.3357142857143,22.9611878610227,-35.2276361967536));
#78894=CARTESIAN_POINT('',(22.,24.9201858254425,-33.0972693499844));
#78895=CARTESIAN_POINT('Ctrl Pts',(22.,24.9201858254425,-33.0972693499844));
#78896=CARTESIAN_POINT('Ctrl Pts',(21.6703423766858,25.0838488138794,-33.359184881506));
#78897=CARTESIAN_POINT('Ctrl Pts',(21.3357142857143,25.2499610186654,-33.6250199785202));
#78898=CARTESIAN_POINT('Origin',(22.,0.,0.));
#78899=CARTESIAN_POINT('Origin',(21.55,0.,0.));
#78900=CARTESIAN_POINT('',(21.3357142857143,28.7295706529848,-30.7052808177218));
#78901=CARTESIAN_POINT('',(22.,28.2671026036886,-30.288872715777));
#78902=CARTESIAN_POINT('Ctrl Pts',(21.3357142857143,28.7295706529848,-30.7052808177218));
#78903=CARTESIAN_POINT('Ctrl Pts',(21.6703423805549,28.4966192673785,-30.4955304479972));
#78904=CARTESIAN_POINT('Ctrl Pts',(22.,28.2671026036886,-30.288872715777));
#78905=CARTESIAN_POINT('',(21.3357142857143,30.7052808177218,-28.7295706529848));
#78906=CARTESIAN_POINT('Ctrl Pts',(21.3357142857143,30.7052808177218,-28.7295706529848));
#78907=CARTESIAN_POINT('Ctrl Pts',(21.385443740297,29.7174257353533,-29.7174257353533));
#78908=CARTESIAN_POINT('Ctrl Pts',(21.3357142857143,28.7295706529848,-30.7052808177218));
#78909=CARTESIAN_POINT('',(22.,30.288872715777,-28.2671026036886));
#78910=CARTESIAN_POINT('Ctrl Pts',(22.,30.288872715777,-28.2671026036886));
#78911=CARTESIAN_POINT('Ctrl Pts',(21.6703423826323,30.4955304466952,-28.4966192659325));
#78912=CARTESIAN_POINT('Ctrl Pts',(21.3357142857143,30.7052808177218,-28.7295706529848));
#78913=CARTESIAN_POINT('Origin',(22.,0.,0.));
#78914=CARTESIAN_POINT('Origin',(21.55,0.,0.));
#78915=CARTESIAN_POINT('',(21.3357142857143,33.6250199785202,-25.2499610186654));
#78916=CARTESIAN_POINT('',(22.,33.0972693499844,-24.9201858254425));
#78917=CARTESIAN_POINT('Ctrl Pts',(21.3357142857143,33.6250199785202,-25.2499610186654));
#78918=CARTESIAN_POINT('Ctrl Pts',(21.6703423759705,33.3591848820742,-25.0838488142344));
#78919=CARTESIAN_POINT('Ctrl Pts',(22.,33.0972693499844,-24.9201858254425));
#78920=CARTESIAN_POINT('',(21.3357142857143,35.2276361967536,-22.9611878610227));
#78921=CARTESIAN_POINT('Ctrl Pts',(21.3357142857143,35.2276361967536,-22.9611878610227));
#78922=CARTESIAN_POINT('Ctrl Pts',(21.385443740297,34.4263280876368,-24.1055744398441));
#78923=CARTESIAN_POINT('Ctrl Pts',(21.3357142857143,33.6250199785202,-25.2499610186654));
#78924=CARTESIAN_POINT('',(22.,34.7372475355518,-22.5780542486238));
#78925=CARTESIAN_POINT('Ctrl Pts',(22.,34.7372475355518,-22.5780542486238));
#78926=CARTESIAN_POINT('Ctrl Pts',(21.6703423724652,34.9806208288272,-22.7681983045355));
#78927=CARTESIAN_POINT('Ctrl Pts',(21.3357142857143,35.2276361967536,-22.9611878610227));
#78928=CARTESIAN_POINT('Origin',(22.,0.,0.));
#78929=CARTESIAN_POINT('Origin',(21.55,0.,0.));
#78930=CARTESIAN_POINT('',(21.3357142857143,37.4987900870893,-19.0274339311535));
#78931=CARTESIAN_POINT('',(22.,36.9217923151073,-18.7943116990244));
#78932=CARTESIAN_POINT('Ctrl Pts',(21.3357142857143,37.4987900870893,-19.0274339311535));
#78933=CARTESIAN_POINT('Ctrl Pts',(21.6703423745627,37.2081485427215,-18.9100071249117));
#78934=CARTESIAN_POINT('Ctrl Pts',(22.,36.9217923151073,-18.7943116990244));
#78935=CARTESIAN_POINT('',(21.3357142857143,38.6796176759911,-16.4951409948251));
#78936=CARTESIAN_POINT('Ctrl Pts',(21.3357142857143,38.6796176759911,-16.4951409948251));
#78937=CARTESIAN_POINT('Ctrl Pts',(21.385443740297,38.0892038815402,-17.7612874629894));
#78938=CARTESIAN_POINT('Ctrl Pts',(21.3357142857143,37.4987900870893,-19.0274339311535));
#78939=CARTESIAN_POINT('',(22.,38.1301486668542,-16.2029831402614));
#78940=CARTESIAN_POINT('Ctrl Pts',(22.,38.1301486668542,-16.2029831402613));
#78941=CARTESIAN_POINT('Ctrl Pts',(21.670342378402,38.4028427368413,-16.3479771492316));
#78942=CARTESIAN_POINT('Ctrl Pts',(21.3357142857143,38.6796176759911,-16.4951409948251));
#78943=CARTESIAN_POINT('Origin',(22.,0.,0.));
#78944=CARTESIAN_POINT('Origin',(21.55,0.,0.));
#78945=CARTESIAN_POINT('',(21.3357142857143,40.2331784341656,-12.2267678919898));
#78946=CARTESIAN_POINT('',(22.,39.6244653040641,-12.097381922012));
#78947=CARTESIAN_POINT('Ctrl Pts',(21.3357142857143,40.2331784341656,-12.2267678919898));
#78948=CARTESIAN_POINT('Ctrl Pts',(21.6703423772556,39.9265614345444,-12.1615944368007));
#78949=CARTESIAN_POINT('Ctrl Pts',(22.,39.6244653040641,-12.097381922012));
#78950=CARTESIAN_POINT('',(21.3357142857143,40.9563385449745,-9.52789761644383));
#78951=CARTESIAN_POINT('Ctrl Pts',(21.3357142857143,40.9563385449745,-9.52789761644383));
#78952=CARTESIAN_POINT('Ctrl Pts',(21.385443740297,40.59475848957,-10.8773327542168));
#78953=CARTESIAN_POINT('Ctrl Pts',(21.3357142857143,40.2331784341656,-12.2267678919898));
#78954=CARTESIAN_POINT('',(22.,40.3644845257005,-9.33559258828711));
#78955=CARTESIAN_POINT('Ctrl Pts',(22.,40.3644845257005,-9.33559258828712));
#78956=CARTESIAN_POINT('Ctrl Pts',(21.6703423769138,40.6582137067803,-9.43103098457829));
#78957=CARTESIAN_POINT('Ctrl Pts',(21.3357142857143,40.9563385449745,-9.52789761644383));
#78958=CARTESIAN_POINT('Origin',(22.,0.,0.));
#78959=CARTESIAN_POINT('Origin',(21.55,0.,0.));
#78960=CARTESIAN_POINT('',(21.3357142857143,41.7451020134904,-5.05459769747091));
#78961=CARTESIAN_POINT('',(22.,41.1231689657038,-5.03287931686986));
#78962=CARTESIAN_POINT('Ctrl Pts',(21.3357142857143,41.7451020134904,-5.05459769747091));
#78963=CARTESIAN_POINT('Ctrl Pts',(21.6703423779714,41.4318259626622,-5.04365785671265));
#78964=CARTESIAN_POINT('Ctrl Pts',(22.,41.1231689657038,-5.03287931686986));
#78965=CARTESIAN_POINT('',(21.3357142857143,41.9886217921762,-2.27115389033571));
#78966=CARTESIAN_POINT('Ctrl Pts',(21.3357142857143,41.9886217921762,-2.27115389033571));
#78967=CARTESIAN_POINT('Ctrl Pts',(21.385443740297,41.8668619028333,-3.66287579390335));
#78968=CARTESIAN_POINT('Ctrl Pts',(21.3357142857143,41.7451020134904,-5.05459769747091));
#78969=CARTESIAN_POINT('',(22.,41.3723659476482,-2.18454477955551));
#78970=CARTESIAN_POINT('Ctrl Pts',(22.,41.3723659476482,-2.18454477955551));
#78971=CARTESIAN_POINT('Ctrl Pts',(21.6703423741537,41.678205428617,-2.22752771549582));
#78972=CARTESIAN_POINT('Ctrl Pts',(21.3357142857143,41.9886217921762,-2.27115389033571));
#78973=CARTESIAN_POINT('Origin',(22.,0.,0.));
#78974=CARTESIAN_POINT('Origin',(0.,41.9886217921762,-2.27115389033571));
#78975=CARTESIAN_POINT('',(0.66428571428571,41.9886217921762,-2.27115389033571));
#78976=CARTESIAN_POINT('',(0.,41.9886217921762,-2.27115389033571));
#78977=CARTESIAN_POINT('',(-6.93889390390723E-17,41.3723659476482,-2.18454477955551));
#78978=CARTESIAN_POINT('Ctrl Pts',(0.66428571428571,41.9886217921762,-2.27115389033571));
#78979=CARTESIAN_POINT('Ctrl Pts',(0.329657625802016,41.678205428576,-2.22752771549006));
#78980=CARTESIAN_POINT('Ctrl Pts',(6.93889390390723E-17,41.3723659476482,
-2.18454477955552));
#78981=CARTESIAN_POINT('',(0.,37.4643267032267,-1.63530568209483));
#78982=CARTESIAN_POINT('',(0.,41.9886217921762,-2.27115389033571));
#78983=CARTESIAN_POINT('',(0.,37.4643267032267,-1.63530568209483));
#78984=CARTESIAN_POINT('',(11.,37.7627704896084,-1.67724922094465));
#78985=CARTESIAN_POINT('',(22.,37.4643267032267,-1.63530568209483));
#78986=CARTESIAN_POINT('',(0.,37.4643267032267,-1.63530568209483));
#78987=CARTESIAN_POINT('',(22.,41.9886217921762,-2.27115389033571));
#78988=CARTESIAN_POINT('Origin',(0.,41.7451020134904,-5.05459769747091));
#78989=CARTESIAN_POINT('',(0.664285714285704,41.7451020134904,-5.05459769747091));
#78990=CARTESIAN_POINT('',(0.,41.7451020134904,-5.05459769747091));
#78991=CARTESIAN_POINT('Ctrl Pts',(0.664285714285704,41.7451020134904,-5.05459769747091));
#78992=CARTESIAN_POINT('Ctrl Pts',(0.614556259703002,41.8668619028333,-3.66287579390327));
#78993=CARTESIAN_POINT('Ctrl Pts',(0.66428571428571,41.9886217921762,-2.27115389033571));
#78994=CARTESIAN_POINT('Origin',(0.,40.9563385449745,-9.52789761644383));
#78995=CARTESIAN_POINT('',(0.664285714285704,40.9563385449745,-9.52789761644383));
#78996=CARTESIAN_POINT('',(0.,40.9563385449745,-9.52789761644383));
#78997=CARTESIAN_POINT('',(2.08166817117217E-16,40.3644845257005,-9.33559258828711));
#78998=CARTESIAN_POINT('Ctrl Pts',(0.664285714285704,40.9563385449745,-9.52789761644383));
#78999=CARTESIAN_POINT('Ctrl Pts',(0.329657628901705,40.658213711961,-9.43103098626159));
#79000=CARTESIAN_POINT('Ctrl Pts',(4.16333634234434E-16,40.3644845257005,
-9.33559258828712));
#79001=CARTESIAN_POINT('',(0.,36.6111915470958,-8.11607377380577));
#79002=CARTESIAN_POINT('',(0.,40.9563385449745,-9.52789761644383));
#79003=CARTESIAN_POINT('',(0.,36.6111915470958,-8.11607377380577));
#79004=CARTESIAN_POINT('',(11.,36.8978178826767,-8.20920431569504));
#79005=CARTESIAN_POINT('',(22.,36.6111915470958,-8.11607377380577));
#79006=CARTESIAN_POINT('',(0.,36.6111915470958,-8.11607377380577));
#79007=CARTESIAN_POINT('',(22.,40.9563385449745,-9.52789761644383));
#79008=CARTESIAN_POINT('Origin',(0.,40.2331784341656,-12.2267678919898));
#79009=CARTESIAN_POINT('',(0.664285714285704,40.2331784341656,-12.2267678919898));
#79010=CARTESIAN_POINT('',(0.,40.2331784341656,-12.2267678919898));
#79011=CARTESIAN_POINT('Ctrl Pts',(0.664285714285704,40.2331784341656,-12.2267678919898));
#79012=CARTESIAN_POINT('Ctrl Pts',(0.614556259703,40.5947584895701,-10.8773327542167));
#79013=CARTESIAN_POINT('Ctrl Pts',(0.664285714285704,40.9563385449745,-9.52789761644383));
#79014=CARTESIAN_POINT('Origin',(0.,38.6796176759911,-16.4951409948251));
#79015=CARTESIAN_POINT('',(0.664285714285706,38.6796176759911,-16.4951409948251));
#79016=CARTESIAN_POINT('',(0.,38.6796176759911,-16.4951409948251));
#79017=CARTESIAN_POINT('',(6.93889390390723E-17,38.1301486668542,-16.2029831402614));
#79018=CARTESIAN_POINT('Ctrl Pts',(0.664285714285706,38.6796176759911,-16.4951409948251));
#79019=CARTESIAN_POINT('Ctrl Pts',(0.329657628291304,38.402842742377,-16.347977152175));
#79020=CARTESIAN_POINT('Ctrl Pts',(-6.93889390390723E-17,38.1301486668542,
-16.2029831402614));
#79021=CARTESIAN_POINT('',(0.,34.6456438619633,-14.3502390708311));
#79022=CARTESIAN_POINT('',(0.,38.6796176759911,-16.4951409948251));
#79023=CARTESIAN_POINT('',(0.,34.6456438619633,-14.3502390708311));
#79024=CARTESIAN_POINT('',(11.,34.9117437505765,-14.4917268913708));
#79025=CARTESIAN_POINT('',(22.,34.6456438619633,-14.3502390708311));
#79026=CARTESIAN_POINT('',(0.,34.6456438619633,-14.3502390708311));
#79027=CARTESIAN_POINT('',(22.,38.6796176759911,-16.4951409948251));
#79028=CARTESIAN_POINT('Origin',(0.,37.4987900870893,-19.0274339311535));
#79029=CARTESIAN_POINT('',(0.664285714285706,37.4987900870893,-19.0274339311535));
#79030=CARTESIAN_POINT('',(0.,37.4987900870893,-19.0274339311535));
#79031=CARTESIAN_POINT('Ctrl Pts',(0.664285714285706,37.4987900870893,-19.0274339311535));
#79032=CARTESIAN_POINT('Ctrl Pts',(0.614556259703001,38.0892038815402,-17.7612874629893));
#79033=CARTESIAN_POINT('Ctrl Pts',(0.664285714285706,38.6796176759911,-16.4951409948251));
#79034=CARTESIAN_POINT('Origin',(0.,35.2276361967536,-22.9611878610227));
#79035=CARTESIAN_POINT('',(0.664285714285706,35.2276361967536,-22.9611878610227));
#79036=CARTESIAN_POINT('',(0.,35.2276361967536,-22.9611878610227));
#79037=CARTESIAN_POINT('',(7.63278329429795E-16,34.7372475355518,-22.5780542486238));
#79038=CARTESIAN_POINT('Ctrl Pts',(0.664285714285706,35.2276361967536,-22.9611878610227));
#79039=CARTESIAN_POINT('Ctrl Pts',(0.329657624533208,34.9806208266117,-22.7681983028046));
#79040=CARTESIAN_POINT('Ctrl Pts',(6.24500451351651E-16,34.7372475355518,
-22.5780542486238));
#79041=CARTESIAN_POINT('',(0.,31.6274058196267,-20.1483796152605));
#79042=CARTESIAN_POINT('',(0.,35.2276361967536,-22.9611878610227));
#79043=CARTESIAN_POINT('',(0.,31.6274058196267,-20.1483796152605));
#79044=CARTESIAN_POINT('',(11.,31.8648939508099,-20.3339256786199));
#79045=CARTESIAN_POINT('',(22.,31.6274058196267,-20.1483796152605));
#79046=CARTESIAN_POINT('',(0.,31.6274058196267,-20.1483796152605));
#79047=CARTESIAN_POINT('',(22.,35.2276361967536,-22.9611878610227));
#79048=CARTESIAN_POINT('Origin',(0.,33.6250199785202,-25.2499610186654));
#79049=CARTESIAN_POINT('',(0.66428571428571,33.6250199785202,-25.2499610186654));
#79050=CARTESIAN_POINT('',(0.,33.6250199785202,-25.2499610186654));
#79051=CARTESIAN_POINT('Ctrl Pts',(0.66428571428571,33.6250199785202,-25.2499610186654));
#79052=CARTESIAN_POINT('Ctrl Pts',(0.614556259703001,34.4263280876369,-24.105574439844));
#79053=CARTESIAN_POINT('Ctrl Pts',(0.664285714285706,35.2276361967536,-22.9611878610227));
#79054=CARTESIAN_POINT('Origin',(0.,30.7052808177218,-28.7295706529848));
#79055=CARTESIAN_POINT('',(0.664285714285712,30.7052808177218,-28.7295706529848));
#79056=CARTESIAN_POINT('',(0.,30.7052808177218,-28.7295706529848));
#79057=CARTESIAN_POINT('',(2.08166817117217E-16,30.288872715777,-28.2671026036886));
#79058=CARTESIAN_POINT('Ctrl Pts',(0.664285714285712,30.7052808177218,-28.7295706529848));
#79059=CARTESIAN_POINT('Ctrl Pts',(0.329657623601863,30.4955304506025,-28.4966192702721));
#79060=CARTESIAN_POINT('Ctrl Pts',(2.08166817117217E-16,30.288872715777,
-28.2671026036886));
#79061=CARTESIAN_POINT('',(0.,27.6481850557002,-25.3343218406523));
#79062=CARTESIAN_POINT('',(0.,30.7052808177218,-28.7295706529848));
#79063=CARTESIAN_POINT('',(0.,27.6481850557002,-25.3343218406523));
#79064=CARTESIAN_POINT('',(11.,27.8498454727622,-25.5582884235871));
#79065=CARTESIAN_POINT('',(22.,27.6481850557002,-25.3343218406523));
#79066=CARTESIAN_POINT('',(0.,27.6481850557002,-25.3343218406523));
#79067=CARTESIAN_POINT('',(22.,30.7052808177218,-28.7295706529848));
#79068=CARTESIAN_POINT('Origin',(0.,28.7295706529848,-30.7052808177218));
#79069=CARTESIAN_POINT('',(0.664285714285712,28.7295706529848,-30.7052808177218));
#79070=CARTESIAN_POINT('',(0.,28.7295706529848,-30.7052808177218));
#79071=CARTESIAN_POINT('Ctrl Pts',(0.664285714285712,28.7295706529848,-30.7052808177218));
#79072=CARTESIAN_POINT('Ctrl Pts',(0.614556259703005,29.7174257353533,-29.7174257353533));
#79073=CARTESIAN_POINT('Ctrl Pts',(0.664285714285712,30.7052808177218,-28.7295706529848));
#79074=CARTESIAN_POINT('Origin',(0.,25.2499610186654,-33.6250199785202));
#79075=CARTESIAN_POINT('',(0.664285714285713,25.2499610186654,-33.6250199785202));
#79076=CARTESIAN_POINT('',(0.,25.2499610186654,-33.6250199785202));
#79077=CARTESIAN_POINT('',(4.16333634234434E-16,24.9201858254425,-33.0972693499844));
#79078=CARTESIAN_POINT('Ctrl Pts',(0.664285714285713,25.2499610186654,-33.6250199785202));
#79079=CARTESIAN_POINT('Ctrl Pts',(0.329657620247448,25.0838488123571,-33.3591848790699));
#79080=CARTESIAN_POINT('Ctrl Pts',(3.46944695195361E-16,24.9201858254425,
-33.0972693499844));
#79081=CARTESIAN_POINT('',(0.,22.8288881795131,-29.7504935167013));
#79082=CARTESIAN_POINT('',(0.,25.2499610186654,-33.6250199785202));
#79083=CARTESIAN_POINT('',(0.,22.8288881795131,-29.7504935167013));
#79084=CARTESIAN_POINT('',(11.,22.9885935327265,-30.0060755079215));
#79085=CARTESIAN_POINT('',(22.,22.8288881795131,-29.7504935167013));
#79086=CARTESIAN_POINT('',(0.,22.8288881795131,-29.7504935167013));
#79087=CARTESIAN_POINT('',(22.,25.2499610186654,-33.6250199785202));
#79088=CARTESIAN_POINT('Origin',(0.,22.9611878610227,-35.2276361967536));
#79089=CARTESIAN_POINT('',(0.664285714285709,22.9611878610227,-35.2276361967536));
#79090=CARTESIAN_POINT('',(0.,22.9611878610227,-35.2276361967536));
#79091=CARTESIAN_POINT('Ctrl Pts',(0.664285714285709,22.9611878610227,-35.2276361967536));
#79092=CARTESIAN_POINT('Ctrl Pts',(0.614556259703007,24.105574439844,-34.4263280876369));
#79093=CARTESIAN_POINT('Ctrl Pts',(0.664285714285713,25.2499610186654,-33.6250199785202));
#79094=CARTESIAN_POINT('Origin',(0.,19.0274339311535,-37.4987900870893));
#79095=CARTESIAN_POINT('',(0.664285714285708,19.0274339311535,-37.4987900870893));
#79096=CARTESIAN_POINT('',(0.,19.0274339311535,-37.4987900870893));
#79097=CARTESIAN_POINT('',(6.93889390390723E-17,18.7943116990243,-36.9217923151073));
#79098=CARTESIAN_POINT('Ctrl Pts',(0.664285714285708,19.0274339311535,-37.4987900870893));
#79099=CARTESIAN_POINT('Ctrl Pts',(0.329657620121465,18.9100071230464,-37.2081485381049));
#79100=CARTESIAN_POINT('Ctrl Pts',(6.93889390390723E-17,18.7943116990243,
-36.9217923151073));
#79101=CARTESIAN_POINT('',(0.,17.3159470879662,-33.2627115017215));
#79102=CARTESIAN_POINT('',(0.,19.0274339311535,-37.4987900870893));
#79103=CARTESIAN_POINT('',(0.,17.3159470879662,-33.2627115017215));
#79104=CARTESIAN_POINT('',(11.,17.4288448109885,-33.5421431717545));
#79105=CARTESIAN_POINT('',(22.,17.3159470879662,-33.2627115017215));
#79106=CARTESIAN_POINT('',(0.,17.3159470879662,-33.2627115017215));
#79107=CARTESIAN_POINT('',(22.,19.0274339311535,-37.4987900870893));
#79108=CARTESIAN_POINT('Origin',(0.,16.4951409948251,-38.6796176759911));
#79109=CARTESIAN_POINT('',(0.664285714285715,16.4951409948251,-38.6796176759911));
#79110=CARTESIAN_POINT('',(0.,16.4951409948251,-38.6796176759911));
#79111=CARTESIAN_POINT('Ctrl Pts',(0.664285714285715,16.4951409948251,-38.6796176759911));
#79112=CARTESIAN_POINT('Ctrl Pts',(0.614556259703004,17.7612874629893,-38.0892038815402));
#79113=CARTESIAN_POINT('Ctrl Pts',(0.664285714285708,19.0274339311535,-37.4987900870893));
#79114=CARTESIAN_POINT('Origin',(0.,12.2267678919897,-40.2331784341656));
#79115=CARTESIAN_POINT('',(0.664285714285713,12.2267678919897,-40.2331784341656));
#79116=CARTESIAN_POINT('',(0.,12.2267678919897,-40.2331784341656));
#79117=CARTESIAN_POINT('',(6.93889390390723E-17,12.0973819220119,-39.6244653040641));
#79118=CARTESIAN_POINT('Ctrl Pts',(0.664285714285713,12.2267678919897,-40.2331784341656));
#79119=CARTESIAN_POINT('Ctrl Pts',(0.329657622858237,12.1615944368228,-39.9265614346487));
#79120=CARTESIAN_POINT('Ctrl Pts',(-1.38777878078145E-16,12.0973819220119,
-39.6244653040641));
#79121=CARTESIAN_POINT('',(0.,11.2768697064435,-35.764258829506));
#79122=CARTESIAN_POINT('',(0.,12.2267678919897,-40.2331784341656));
#79123=CARTESIAN_POINT('',(0.,11.2768697064435,-35.764258829506));
#79124=CARTESIAN_POINT('',(11.,11.3395294590896,-36.0590497884573));
#79125=CARTESIAN_POINT('',(22.,11.2768697064435,-35.764258829506));
#79126=CARTESIAN_POINT('',(0.,11.2768697064435,-35.764258829506));
#79127=CARTESIAN_POINT('',(22.,12.2267678919897,-40.2331784341656));
#79128=CARTESIAN_POINT('Origin',(0.,9.52789761644378,-40.9563385449745));
#79129=CARTESIAN_POINT('',(0.664285714285714,9.52789761644378,-40.9563385449745));
#79130=CARTESIAN_POINT('',(0.,9.52789761644378,-40.9563385449745));
#79131=CARTESIAN_POINT('Ctrl Pts',(0.664285714285714,9.52789761644378,-40.9563385449745));
#79132=CARTESIAN_POINT('Ctrl Pts',(0.614556259703009,10.8773327542168,-40.5947584895701));
#79133=CARTESIAN_POINT('Ctrl Pts',(0.664285714285713,12.2267678919897,-40.2331784341656));
#79134=CARTESIAN_POINT('Origin',(0.,5.0545976974709,-41.7451020134904));
#79135=CARTESIAN_POINT('',(0.664285714285704,5.0545976974709,-41.7451020134904));
#79136=CARTESIAN_POINT('',(0.,5.0545976974709,-41.7451020134904));
#79137=CARTESIAN_POINT('',(6.93889390390723E-17,5.03287931686985,-41.1231689657038));
#79138=CARTESIAN_POINT('Ctrl Pts',(0.664285714285704,5.0545976974709,-41.7451020134904));
#79139=CARTESIAN_POINT('Ctrl Pts',(0.329657625028856,5.04365785681072,-41.4318259654708));
#79140=CARTESIAN_POINT('Ctrl Pts',(-6.93889390390723E-17,5.03287931686985,
-41.1231689657038));
#79141=CARTESIAN_POINT('',(0.,4.89515034526193,-37.1791272503441));
#79142=CARTESIAN_POINT('',(0.,5.0545976974709,-41.7451020134904));
#79143=CARTESIAN_POINT('',(0.,4.89515034526193,-37.1791272503441));
#79144=CARTESIAN_POINT('',(11.,4.90566824265506,-37.4803204240973));
#79145=CARTESIAN_POINT('',(22.,4.89515034526193,-37.1791272503441));
#79146=CARTESIAN_POINT('',(0.,4.89515034526193,-37.1791272503441));
#79147=CARTESIAN_POINT('',(22.,5.0545976974709,-41.7451020134904));
#79148=CARTESIAN_POINT('Origin',(0.,2.2711538903357,-41.9886217921762));
#79149=CARTESIAN_POINT('',(0.6642857142857,2.2711538903357,-41.9886217921762));
#79150=CARTESIAN_POINT('',(0.,2.2711538903357,-41.9886217921762));
#79151=CARTESIAN_POINT('Ctrl Pts',(0.6642857142857,2.2711538903357,-41.9886217921762));
#79152=CARTESIAN_POINT('Ctrl Pts',(0.614556259702998,3.66287579390334,-41.8668619028333));
#79153=CARTESIAN_POINT('Ctrl Pts',(0.664285714285704,5.0545976974709,-41.7451020134904));
#79154=CARTESIAN_POINT('Origin',(0.,-2.27115389033571,-41.9886217921762));
#79155=CARTESIAN_POINT('',(0.6642857142857,-2.27115389033571,-41.9886217921762));
#79156=CARTESIAN_POINT('',(0.,-2.27115389033571,-41.9886217921762));
#79157=CARTESIAN_POINT('',(-6.93889390390723E-17,-2.18454477955551,-41.3723659476482));
#79158=CARTESIAN_POINT('Ctrl Pts',(0.6642857142857,-2.27115389033571,-41.9886217921762));
#79159=CARTESIAN_POINT('Ctrl Pts',(0.329657622906579,-2.2275277151126,-41.6782054258903));
#79160=CARTESIAN_POINT('Ctrl Pts',(-6.93889390390723E-17,-2.18454477955551,
-41.3723659476482));
#79161=CARTESIAN_POINT('',(0.,-1.63530568209482,-37.4643267032267));
#79162=CARTESIAN_POINT('',(0.,-2.27115389033571,-41.9886217921762));
#79163=CARTESIAN_POINT('',(0.,-1.63530568209482,-37.4643267032267));
#79164=CARTESIAN_POINT('',(11.,-1.67724922094465,-37.7627704896084));
#79165=CARTESIAN_POINT('',(22.,-1.63530568209482,-37.4643267032267));
#79166=CARTESIAN_POINT('',(0.,-1.63530568209482,-37.4643267032267));
#79167=CARTESIAN_POINT('',(22.,-2.27115389033571,-41.9886217921762));
#79168=CARTESIAN_POINT('Origin',(0.,-5.05459769747091,-41.7451020134904));
#79169=CARTESIAN_POINT('',(0.664285714285704,-5.05459769747091,-41.7451020134904));
#79170=CARTESIAN_POINT('',(0.,-5.05459769747091,-41.7451020134904));
#79171=CARTESIAN_POINT('Ctrl Pts',(0.664285714285704,-5.05459769747091,
-41.7451020134904));
#79172=CARTESIAN_POINT('Ctrl Pts',(0.614556259702995,-3.66287579390326,
-41.8668619028333));
#79173=CARTESIAN_POINT('Ctrl Pts',(0.6642857142857,-2.27115389033571,-41.9886217921762));
#79174=CARTESIAN_POINT('Origin',(0.,-9.52789761644383,-40.9563385449745));
#79175=CARTESIAN_POINT('',(0.664285714285723,-9.52789761644383,-40.9563385449745));
#79176=CARTESIAN_POINT('',(0.,-9.52789761644383,-40.9563385449745));
#79177=CARTESIAN_POINT('',(-1.38777878078145E-16,-9.33559258828711,-40.3644845257006));
#79178=CARTESIAN_POINT('Ctrl Pts',(0.664285714285723,-9.52789761644383,
-40.9563385449745));
#79179=CARTESIAN_POINT('Ctrl Pts',(0.329657616731471,-9.4310309827389,-40.6582137011193));
#79180=CARTESIAN_POINT('Ctrl Pts',(-2.08166817117217E-16,-9.3355925882871,
-40.3644845257006));
#79181=CARTESIAN_POINT('',(0.,-8.11607377380577,-36.6111915470959));
#79182=CARTESIAN_POINT('',(0.,-9.52789761644383,-40.9563385449745));
#79183=CARTESIAN_POINT('',(0.,-8.11607377380577,-36.6111915470959));
#79184=CARTESIAN_POINT('',(11.,-8.20920431569503,-36.8978178826767));
#79185=CARTESIAN_POINT('',(22.,-8.11607377380577,-36.6111915470959));
#79186=CARTESIAN_POINT('',(0.,-8.11607377380577,-36.6111915470959));
#79187=CARTESIAN_POINT('',(22.,-9.52789761644383,-40.9563385449745));
#79188=CARTESIAN_POINT('Origin',(0.,-12.2267678919898,-40.2331784341656));
#79189=CARTESIAN_POINT('',(0.664285714285714,-12.2267678919898,-40.2331784341656));
#79190=CARTESIAN_POINT('',(0.,-12.2267678919898,-40.2331784341656));
#79191=CARTESIAN_POINT('Ctrl Pts',(0.664285714285714,-12.2267678919898,
-40.2331784341656));
#79192=CARTESIAN_POINT('Ctrl Pts',(0.614556259703017,-10.8773327542167,
-40.5947584895701));
#79193=CARTESIAN_POINT('Ctrl Pts',(0.664285714285723,-9.52789761644383,
-40.9563385449745));
#79194=CARTESIAN_POINT('Origin',(0.,-22.9611878610227,-35.2276361967536));
#79195=CARTESIAN_POINT('',(0.664285714285713,-22.9611878610227,-35.2276361967536));
#79196=CARTESIAN_POINT('',(0.,-22.9611878610227,-35.2276361967536));
#79197=CARTESIAN_POINT('',(2.08166817117217E-16,-22.5780542486238,-34.7372475355518));
#79198=CARTESIAN_POINT('Ctrl Pts',(0.664285714285713,-22.9611878610227,
-35.2276361967536));
#79199=CARTESIAN_POINT('Ctrl Pts',(0.329657622232873,-22.768198301478,-34.9806208249138));
#79200=CARTESIAN_POINT('Ctrl Pts',(-1.38777878078145E-16,-22.5780542486238,
-34.7372475355518));
#79201=CARTESIAN_POINT('',(0.,-20.1483796152605,-31.6274058196267));
#79202=CARTESIAN_POINT('',(0.,-22.9611878610227,-35.2276361967536));
#79203=CARTESIAN_POINT('',(0.,-20.1483796152605,-31.6274058196267));
#79204=CARTESIAN_POINT('',(11.,-20.3339256786199,-31.8648939508099));
#79205=CARTESIAN_POINT('',(22.,-20.1483796152605,-31.6274058196267));
#79206=CARTESIAN_POINT('',(0.,-20.1483796152605,-31.6274058196267));
#79207=CARTESIAN_POINT('',(22.,-22.9611878610227,-35.2276361967536));
#79208=CARTESIAN_POINT('Origin',(0.,-25.2499610186654,-33.6250199785202));
#79209=CARTESIAN_POINT('',(0.664285714285703,-25.2499610186654,-33.6250199785202));
#79210=CARTESIAN_POINT('',(0.,-25.2499610186654,-33.6250199785202));
#79211=CARTESIAN_POINT('Ctrl Pts',(0.664285714285703,-25.2499610186654,
-33.6250199785202));
#79212=CARTESIAN_POINT('Ctrl Pts',(0.614556259703008,-24.105574439844,-34.4263280876369));
#79213=CARTESIAN_POINT('Ctrl Pts',(0.664285714285713,-22.9611878610227,
-35.2276361967536));
#79214=CARTESIAN_POINT('Origin',(0.,-28.7295706529848,-30.7052808177218));
#79215=CARTESIAN_POINT('',(0.664285714285715,-28.7295706529848,-30.7052808177218));
#79216=CARTESIAN_POINT('',(0.,-28.7295706529848,-30.7052808177218));
#79217=CARTESIAN_POINT('',(0.,-28.2671026036886,-30.288872715777));
#79218=CARTESIAN_POINT('Ctrl Pts',(0.664285714285715,-28.7295706529848,
-30.7052808177218));
#79219=CARTESIAN_POINT('Ctrl Pts',(0.329657620568989,-28.4966192681609,
-30.4955304487016));
#79220=CARTESIAN_POINT('Ctrl Pts',(-2.77555756156289E-16,-28.2671026036886,
-30.288872715777));
#79221=CARTESIAN_POINT('',(0.,-25.3343218406523,-27.6481850557002));
#79222=CARTESIAN_POINT('',(0.,-28.7295706529848,-30.7052808177218));
#79223=CARTESIAN_POINT('',(0.,-25.3343218406523,-27.6481850557002));
#79224=CARTESIAN_POINT('',(11.,-25.5582884235871,-27.8498454727622));
#79225=CARTESIAN_POINT('',(22.,-25.3343218406523,-27.6481850557002));
#79226=CARTESIAN_POINT('',(0.,-25.3343218406523,-27.6481850557002));
#79227=CARTESIAN_POINT('',(22.,-28.7295706529848,-30.7052808177218));
#79228=CARTESIAN_POINT('Origin',(0.,-30.7052808177218,-28.7295706529848));
#79229=CARTESIAN_POINT('',(0.664285714285712,-30.7052808177218,-28.7295706529848));
#79230=CARTESIAN_POINT('',(0.,-30.7052808177218,-28.7295706529848));
#79231=CARTESIAN_POINT('Ctrl Pts',(0.664285714285712,-30.7052808177218,
-28.7295706529848));
#79232=CARTESIAN_POINT('Ctrl Pts',(0.614556259703008,-29.7174257353533,
-29.7174257353533));
#79233=CARTESIAN_POINT('Ctrl Pts',(0.664285714285715,-28.7295706529848,
-30.7052808177218));
#79234=CARTESIAN_POINT('Origin',(0.,-33.6250199785202,-25.2499610186653));
#79235=CARTESIAN_POINT('',(0.664285714285705,-33.6250199785202,-25.2499610186653));
#79236=CARTESIAN_POINT('',(0.,-33.6250199785202,-25.2499610186653));
#79237=CARTESIAN_POINT('',(1.38777878078145E-16,-33.0972693499844,-24.9201858254425));
#79238=CARTESIAN_POINT('Ctrl Pts',(0.664285714285705,-33.6250199785202,
-25.2499610186653));
#79239=CARTESIAN_POINT('Ctrl Pts',(0.329657617838466,-33.3591848771564,
-25.0838488111614));
#79240=CARTESIAN_POINT('Ctrl Pts',(0.,-33.0972693499844,-24.9201858254425));
#79241=CARTESIAN_POINT('',(0.,-29.7504935167013,-22.8288881795131));
#79242=CARTESIAN_POINT('',(0.,-33.6250199785202,-25.2499610186653));
#79243=CARTESIAN_POINT('',(0.,-29.7504935167013,-22.8288881795131));
#79244=CARTESIAN_POINT('',(11.,-30.0060755079215,-22.9885935327265));
#79245=CARTESIAN_POINT('',(22.,-29.7504935167013,-22.8288881795131));
#79246=CARTESIAN_POINT('',(0.,-29.7504935167013,-22.8288881795131));
#79247=CARTESIAN_POINT('',(22.,-33.6250199785202,-25.2499610186653));
#79248=CARTESIAN_POINT('Origin',(0.,-35.2276361967536,-22.9611878610227));
#79249=CARTESIAN_POINT('',(0.664285714285712,-35.2276361967536,-22.9611878610227));
#79250=CARTESIAN_POINT('',(0.,-35.2276361967536,-22.9611878610227));
#79251=CARTESIAN_POINT('Ctrl Pts',(0.664285714285712,-35.2276361967536,
-22.9611878610227));
#79252=CARTESIAN_POINT('Ctrl Pts',(0.614556259703,-34.4263280876369,-24.105574439844));
#79253=CARTESIAN_POINT('Ctrl Pts',(0.664285714285705,-33.6250199785202,
-25.2499610186653));
#79254=CARTESIAN_POINT('Origin',(0.,-37.4987900870893,-19.0274339311535));
#79255=CARTESIAN_POINT('',(0.664285714285717,-37.4987900870893,-19.0274339311535));
#79256=CARTESIAN_POINT('',(0.,-37.4987900870893,-19.0274339311535));
#79257=CARTESIAN_POINT('',(0.,-36.9217923151073,-18.7943116990243));
#79258=CARTESIAN_POINT('Ctrl Pts',(0.664285714285717,-37.4987900870893,
-19.0274339311535));
#79259=CARTESIAN_POINT('Ctrl Pts',(0.329657623220786,-37.2081485407966,
-18.910007124134));
#79260=CARTESIAN_POINT('Ctrl Pts',(-6.93889390390723E-17,-36.9217923151073,
-18.7943116990243));
#79261=CARTESIAN_POINT('',(0.,-33.2627115017215,-17.3159470879662));
#79262=CARTESIAN_POINT('',(0.,-37.4987900870893,-19.0274339311535));
#79263=CARTESIAN_POINT('',(0.,-33.2627115017215,-17.3159470879662));
#79264=CARTESIAN_POINT('',(11.,-33.5421431717545,-17.4288448109885));
#79265=CARTESIAN_POINT('',(22.,-33.2627115017215,-17.3159470879662));
#79266=CARTESIAN_POINT('',(0.,-33.2627115017215,-17.3159470879662));
#79267=CARTESIAN_POINT('',(22.,-37.4987900870893,-19.0274339311535));
#79268=CARTESIAN_POINT('Origin',(0.,-38.6796176759911,-16.4951409948251));
#79269=CARTESIAN_POINT('',(0.664285714285701,-38.6796176759911,-16.4951409948251));
#79270=CARTESIAN_POINT('',(0.,-38.6796176759911,-16.4951409948251));
#79271=CARTESIAN_POINT('Ctrl Pts',(0.664285714285701,-38.6796176759911,
-16.4951409948251));
#79272=CARTESIAN_POINT('Ctrl Pts',(0.614556259703013,-38.0892038815402,
-17.7612874629893));
#79273=CARTESIAN_POINT('Ctrl Pts',(0.664285714285718,-37.4987900870893,
-19.0274339311535));
#79274=CARTESIAN_POINT('Origin',(0.,-40.2331784341656,-12.2267678919897));
#79275=CARTESIAN_POINT('',(0.664285714285713,-40.2331784341656,-12.2267678919897));
#79276=CARTESIAN_POINT('',(0.,-40.2331784341656,-12.2267678919897));
#79277=CARTESIAN_POINT('',(6.93889390390723E-17,-39.6244653040641,-12.0973819220119));
#79278=CARTESIAN_POINT('Ctrl Pts',(0.664285714285713,-40.2331784341656,
-12.2267678919897));
#79279=CARTESIAN_POINT('Ctrl Pts',(0.329657622776605,-39.9265614345739,
-12.1615944368069));
#79280=CARTESIAN_POINT('Ctrl Pts',(0.,-39.6244653040641,-12.0973819220119));
#79281=CARTESIAN_POINT('',(0.,-35.764258829506,-11.2768697064435));
#79282=CARTESIAN_POINT('',(0.,-40.2331784341656,-12.2267678919897));
#79283=CARTESIAN_POINT('',(0.,-35.764258829506,-11.2768697064435));
#79284=CARTESIAN_POINT('',(11.,-36.0590497884573,-11.3395294590896));
#79285=CARTESIAN_POINT('',(22.,-35.764258829506,-11.2768697064435));
#79286=CARTESIAN_POINT('',(0.,-35.764258829506,-11.2768697064435));
#79287=CARTESIAN_POINT('',(22.,-40.2331784341656,-12.2267678919897));
#79288=CARTESIAN_POINT('Origin',(0.,-40.9563385449745,-9.52789761644378));
#79289=CARTESIAN_POINT('',(0.664285714285713,-40.9563385449745,-9.52789761644378));
#79290=CARTESIAN_POINT('',(0.,-40.9563385449745,-9.52789761644378));
#79291=CARTESIAN_POINT('Ctrl Pts',(0.664285714285713,-40.9563385449745,
-9.52789761644378));
#79292=CARTESIAN_POINT('Ctrl Pts',(0.614556259703007,-40.5947584895701,
-10.8773327542168));
#79293=CARTESIAN_POINT('Ctrl Pts',(0.664285714285713,-40.2331784341656,
-12.2267678919897));
#79294=CARTESIAN_POINT('Origin',(0.,-41.7451020134904,-5.05459769747091));
#79295=CARTESIAN_POINT('',(0.664285714285704,-41.7451020134904,-5.0545976974709));
#79296=CARTESIAN_POINT('',(0.,-41.7451020134904,-5.05459769747091));
#79297=CARTESIAN_POINT('',(6.93889390390723E-17,-41.1231689657038,-5.03287931686985));
#79298=CARTESIAN_POINT('Ctrl Pts',(0.664285714285704,-41.7451020134904,
-5.0545976974709));
#79299=CARTESIAN_POINT('Ctrl Pts',(0.329657625220838,-41.4318259656505,
-5.043657856817));
#79300=CARTESIAN_POINT('Ctrl Pts',(-6.93889390390723E-17,-41.1231689657038,
-5.03287931686985));
#79301=CARTESIAN_POINT('',(0.,-37.1791272503441,-4.89515034526194));
#79302=CARTESIAN_POINT('',(0.,-41.7451020134904,-5.05459769747091));
#79303=CARTESIAN_POINT('',(0.,-37.1791272503441,-4.89515034526194));
#79304=CARTESIAN_POINT('',(11.,-37.4803204240973,-4.90566824265506));
#79305=CARTESIAN_POINT('',(22.,-37.1791272503441,-4.89515034526194));
#79306=CARTESIAN_POINT('',(0.,-37.1791272503441,-4.89515034526194));
#79307=CARTESIAN_POINT('',(22.,-41.7451020134904,-5.05459769747091));
#79308=CARTESIAN_POINT('Origin',(0.,-41.9886217921762,-2.2711538903357));
#79309=CARTESIAN_POINT('',(0.6642857142857,-41.9886217921762,-2.2711538903357));
#79310=CARTESIAN_POINT('',(0.,-41.9886217921762,-2.2711538903357));
#79311=CARTESIAN_POINT('Ctrl Pts',(0.6642857142857,-41.9886217921762,-2.2711538903357));
#79312=CARTESIAN_POINT('Ctrl Pts',(0.614556259702998,-41.8668619028333,
-3.66287579390334));
#79313=CARTESIAN_POINT('Ctrl Pts',(0.664285714285704,-41.7451020134904,
-5.0545976974709));
#79314=CARTESIAN_POINT('Origin',(0.,-41.9886217921762,2.27115389033572));
#79315=CARTESIAN_POINT('',(0.66428571428571,-41.9886217921762,2.27115389033572));
#79316=CARTESIAN_POINT('',(0.,-41.9886217921762,2.27115389033572));
#79317=CARTESIAN_POINT('',(0.,-41.3723659476482,2.18454477955553));
#79318=CARTESIAN_POINT('Ctrl Pts',(0.66428571428571,-41.9886217921762,2.27115389033572));
#79319=CARTESIAN_POINT('Ctrl Pts',(0.329657628630436,-41.6782054311995,
2.22752771585878));
#79320=CARTESIAN_POINT('Ctrl Pts',(0.,-41.3723659476482,2.18454477955553));
#79321=CARTESIAN_POINT('',(0.,-37.4643267032267,1.63530568209484));
#79322=CARTESIAN_POINT('',(0.,-41.9886217921762,2.27115389033572));
#79323=CARTESIAN_POINT('',(0.,-37.4643267032267,1.63530568209484));
#79324=CARTESIAN_POINT('',(11.,-37.7627704896084,1.67724922094466));
#79325=CARTESIAN_POINT('',(22.,-37.4643267032267,1.63530568209484));
#79326=CARTESIAN_POINT('',(0.,-37.4643267032267,1.63530568209484));
#79327=CARTESIAN_POINT('',(22.,-41.9886217921762,2.27115389033572));
#79328=CARTESIAN_POINT('Origin',(0.,-41.7451020134904,5.05459769747093));
#79329=CARTESIAN_POINT('',(0.664285714285704,-41.7451020134904,5.05459769747093));
#79330=CARTESIAN_POINT('',(0.,-41.7451020134904,5.05459769747093));
#79331=CARTESIAN_POINT('Ctrl Pts',(0.664285714285704,-41.7451020134904,
5.05459769747093));
#79332=CARTESIAN_POINT('Ctrl Pts',(0.614556259703005,-41.8668619028333,
3.66287579390328));
#79333=CARTESIAN_POINT('Ctrl Pts',(0.66428571428571,-41.9886217921762,2.27115389033572));
#79334=CARTESIAN_POINT('Origin',(0.,-40.9563385449745,9.52789761644381));
#79335=CARTESIAN_POINT('',(0.664285714285704,-40.9563385449745,9.5278976164438));
#79336=CARTESIAN_POINT('',(0.,-40.9563385449745,9.52789761644381));
#79337=CARTESIAN_POINT('',(0.,-40.3644845257006,9.33559258828709));
#79338=CARTESIAN_POINT('Ctrl Pts',(0.664285714285704,-40.9563385449745,
9.5278976164438));
#79339=CARTESIAN_POINT('Ctrl Pts',(0.329657625908044,-40.6582137092941,
9.43103098539505));
#79340=CARTESIAN_POINT('Ctrl Pts',(-1.38777878078145E-16,-40.3644845257006,
9.33559258828709));
#79341=CARTESIAN_POINT('',(0.,-36.6111915470959,8.11607377380575));
#79342=CARTESIAN_POINT('',(0.,-40.9563385449745,9.52789761644381));
#79343=CARTESIAN_POINT('',(0.,-36.6111915470959,8.11607377380575));
#79344=CARTESIAN_POINT('',(11.,-36.8978178826767,8.20920431569502));
#79345=CARTESIAN_POINT('',(22.,-36.6111915470959,8.11607377380575));
#79346=CARTESIAN_POINT('',(0.,-36.6111915470959,8.11607377380575));
#79347=CARTESIAN_POINT('',(22.,-40.9563385449745,9.52789761644381));
#79348=CARTESIAN_POINT('Origin',(0.,-40.2331784341656,12.2267678919897));
#79349=CARTESIAN_POINT('',(0.664285714285703,-40.2331784341656,12.2267678919897));
#79350=CARTESIAN_POINT('',(0.,-40.2331784341656,12.2267678919897));
#79351=CARTESIAN_POINT('Ctrl Pts',(0.664285714285703,-40.2331784341656,
12.2267678919897));
#79352=CARTESIAN_POINT('Ctrl Pts',(0.614556259703,-40.5947584895701,10.8773327542167));
#79353=CARTESIAN_POINT('Ctrl Pts',(0.664285714285704,-40.9563385449745,
9.5278976164438));
#79354=CARTESIAN_POINT('Origin',(0.,-38.6796176759911,16.4951409948251));
#79355=CARTESIAN_POINT('',(0.664285714285705,-38.6796176759911,16.4951409948251));
#79356=CARTESIAN_POINT('',(0.,-38.6796176759911,16.4951409948251));
#79357=CARTESIAN_POINT('',(-1.38777878078145E-16,-38.1301486668543,16.2029831402613));
#79358=CARTESIAN_POINT('Ctrl Pts',(0.664285714285705,-38.6796176759911,
16.4951409948251));
#79359=CARTESIAN_POINT('Ctrl Pts',(0.329657624919205,-38.4028427395881,
16.3479771506921));
#79360=CARTESIAN_POINT('Ctrl Pts',(-6.93889390390723E-17,-38.1301486668543,
16.2029831402613));
#79361=CARTESIAN_POINT('',(0.,-34.6456438619633,14.3502390708311));
#79362=CARTESIAN_POINT('',(0.,-38.6796176759911,16.4951409948251));
#79363=CARTESIAN_POINT('',(0.,-34.6456438619633,14.3502390708311));
#79364=CARTESIAN_POINT('',(11.,-34.9117437505765,14.4917268913708));
#79365=CARTESIAN_POINT('',(22.,-34.6456438619633,14.3502390708311));
#79366=CARTESIAN_POINT('',(0.,-34.6456438619633,14.3502390708311));
#79367=CARTESIAN_POINT('',(22.,-38.6796176759911,16.4951409948251));
#79368=CARTESIAN_POINT('Origin',(0.,-37.4987900870893,19.0274339311535));
#79369=CARTESIAN_POINT('',(0.664285714285704,-37.4987900870893,19.0274339311535));
#79370=CARTESIAN_POINT('',(0.,-37.4987900870893,19.0274339311535));
#79371=CARTESIAN_POINT('Ctrl Pts',(0.664285714285704,-37.4987900870893,
19.0274339311535));
#79372=CARTESIAN_POINT('Ctrl Pts',(0.614556259702999,-38.0892038815402,
17.7612874629892));
#79373=CARTESIAN_POINT('Ctrl Pts',(0.664285714285705,-38.6796176759911,
16.4951409948251));
#79374=CARTESIAN_POINT('Origin',(0.,-35.2276361967536,22.9611878610227));
#79375=CARTESIAN_POINT('',(0.664285714285713,-35.2276361967536,22.9611878610227));
#79376=CARTESIAN_POINT('',(0.,-35.2276361967536,22.9611878610227));
#79377=CARTESIAN_POINT('',(4.16333634234434E-16,-34.7372475355518,22.5780542486238));
#79378=CARTESIAN_POINT('Ctrl Pts',(0.664285714285713,-35.2276361967536,
22.9611878610227));
#79379=CARTESIAN_POINT('Ctrl Pts',(0.329657622235105,-34.9806208249155,
22.7681983014793));
#79380=CARTESIAN_POINT('Ctrl Pts',(-6.93889390390723E-17,-34.7372475355518,
22.5780542486238));
#79381=CARTESIAN_POINT('',(0.,-31.6274058196267,20.1483796152605));
#79382=CARTESIAN_POINT('',(0.,-35.2276361967536,22.9611878610227));
#79383=CARTESIAN_POINT('',(0.,-31.6274058196267,20.1483796152605));
#79384=CARTESIAN_POINT('',(11.,-31.8648939508099,20.3339256786199));
#79385=CARTESIAN_POINT('',(22.,-31.6274058196267,20.1483796152605));
#79386=CARTESIAN_POINT('',(0.,-31.6274058196267,20.1483796152605));
#79387=CARTESIAN_POINT('',(22.,-35.2276361967536,22.9611878610227));
#79388=CARTESIAN_POINT('Origin',(0.,-33.6250199785202,25.2499610186654));
#79389=CARTESIAN_POINT('',(0.664285714285703,-33.6250199785202,25.2499610186654));
#79390=CARTESIAN_POINT('',(0.,-33.6250199785202,25.2499610186654));
#79391=CARTESIAN_POINT('Ctrl Pts',(0.664285714285703,-33.6250199785202,
25.2499610186654));
#79392=CARTESIAN_POINT('Ctrl Pts',(0.614556259703008,-34.4263280876369,
24.105574439844));
#79393=CARTESIAN_POINT('Ctrl Pts',(0.664285714285713,-35.2276361967536,
22.9611878610227));
#79394=CARTESIAN_POINT('Origin',(0.,-30.7052808177218,28.7295706529848));
#79395=CARTESIAN_POINT('',(0.664285714285712,-30.7052808177218,28.7295706529848));
#79396=CARTESIAN_POINT('',(0.,-30.7052808177218,28.7295706529848));
#79397=CARTESIAN_POINT('',(2.08166817117217E-16,-30.288872715777,28.2671026036886));
#79398=CARTESIAN_POINT('Ctrl Pts',(0.664285714285712,-30.7052808177218,
28.7295706529848));
#79399=CARTESIAN_POINT('Ctrl Pts',(0.329657619482983,-30.495530448021,28.496619267405));
#79400=CARTESIAN_POINT('Ctrl Pts',(6.93889390390723E-17,-30.288872715777,
28.2671026036886));
#79401=CARTESIAN_POINT('',(0.,-27.6481850557002,25.3343218406523));
#79402=CARTESIAN_POINT('',(0.,-30.7052808177218,28.7295706529848));
#79403=CARTESIAN_POINT('',(0.,-27.6481850557002,25.3343218406523));
#79404=CARTESIAN_POINT('',(11.,-27.8498454727622,25.5582884235871));
#79405=CARTESIAN_POINT('',(22.,-27.6481850557002,25.3343218406523));
#79406=CARTESIAN_POINT('',(0.,-27.6481850557002,25.3343218406523));
#79407=CARTESIAN_POINT('',(22.,-30.7052808177218,28.7295706529848));
#79408=CARTESIAN_POINT('Origin',(0.,-28.7295706529848,30.7052808177218));
#79409=CARTESIAN_POINT('',(0.664285714285709,-28.7295706529848,30.7052808177218));
#79410=CARTESIAN_POINT('',(0.,-28.7295706529848,30.7052808177218));
#79411=CARTESIAN_POINT('Ctrl Pts',(0.664285714285709,-28.7295706529848,
30.7052808177218));
#79412=CARTESIAN_POINT('Ctrl Pts',(0.614556259703005,-29.7174257353533,
29.7174257353533));
#79413=CARTESIAN_POINT('Ctrl Pts',(0.664285714285712,-30.7052808177218,
28.7295706529848));
#79414=CARTESIAN_POINT('Origin',(0.,-19.0274339311535,37.4987900870893));
#79415=CARTESIAN_POINT('',(0.664285714285711,-19.0274339311535,37.4987900870893));
#79416=CARTESIAN_POINT('',(0.,-19.0274339311535,37.4987900870893));
#79417=CARTESIAN_POINT('',(-1.38777878078145E-16,-18.7943116990243,36.9217923151073));
#79418=CARTESIAN_POINT('Ctrl Pts',(0.664285714285711,-19.0274339311535,
37.4987900870893));
#79419=CARTESIAN_POINT('Ctrl Pts',(0.329657619504279,-18.9100071228299,
37.2081485375689));
#79420=CARTESIAN_POINT('Ctrl Pts',(2.08166817117217E-16,-18.7943116990243,
36.9217923151073));
#79421=CARTESIAN_POINT('',(0.,-17.3159470879662,33.2627115017215));
#79422=CARTESIAN_POINT('',(0.,-19.0274339311535,37.4987900870893));
#79423=CARTESIAN_POINT('',(0.,-17.3159470879662,33.2627115017215));
#79424=CARTESIAN_POINT('',(11.,-17.4288448109885,33.5421431717545));
#79425=CARTESIAN_POINT('',(22.,-17.3159470879662,33.2627115017215));
#79426=CARTESIAN_POINT('',(0.,-17.3159470879662,33.2627115017215));
#79427=CARTESIAN_POINT('',(22.,-19.0274339311535,37.4987900870893));
#79428=CARTESIAN_POINT('Origin',(0.,-16.4951409948251,38.6796176759911));
#79429=CARTESIAN_POINT('',(0.66428571428571,-16.4951409948251,38.6796176759911));
#79430=CARTESIAN_POINT('',(0.,-16.4951409948251,38.6796176759911));
#79431=CARTESIAN_POINT('Ctrl Pts',(0.66428571428571,-16.4951409948251,38.6796176759911));
#79432=CARTESIAN_POINT('Ctrl Pts',(0.614556259703007,-17.7612874629893,
38.0892038815402));
#79433=CARTESIAN_POINT('Ctrl Pts',(0.664285714285711,-19.0274339311535,
37.4987900870893));
#79434=CARTESIAN_POINT('Origin',(0.,-12.2267678919897,40.2331784341656));
#79435=CARTESIAN_POINT('',(0.664285714285714,-12.2267678919897,40.2331784341656));
#79436=CARTESIAN_POINT('',(0.,-12.2267678919897,40.2331784341656));
#79437=CARTESIAN_POINT('',(0.,-12.0973819220119,39.6244653040641));
#79438=CARTESIAN_POINT('Ctrl Pts',(0.664285714285714,-12.2267678919897,
40.2331784341656));
#79439=CARTESIAN_POINT('Ctrl Pts',(0.329657619831027,-12.1615944362333,
39.9265614318751));
#79440=CARTESIAN_POINT('Ctrl Pts',(0.,-12.0973819220119,39.6244653040641));
#79441=CARTESIAN_POINT('',(0.,-11.2768697064435,35.764258829506));
#79442=CARTESIAN_POINT('',(0.,-12.2267678919897,40.2331784341656));
#79443=CARTESIAN_POINT('',(0.,-11.2768697064435,35.764258829506));
#79444=CARTESIAN_POINT('',(11.,-11.3395294590896,36.0590497884573));
#79445=CARTESIAN_POINT('',(22.,-11.2768697064435,35.764258829506));
#79446=CARTESIAN_POINT('',(0.,-11.2768697064435,35.764258829506));
#79447=CARTESIAN_POINT('',(22.,-12.2267678919897,40.2331784341656));
#79448=CARTESIAN_POINT('Origin',(0.,-9.52789761644379,40.9563385449745));
#79449=CARTESIAN_POINT('',(0.664285714285714,-9.52789761644379,40.9563385449745));
#79450=CARTESIAN_POINT('',(0.,-9.52789761644379,40.9563385449745));
#79451=CARTESIAN_POINT('Ctrl Pts',(0.664285714285714,-9.52789761644379,
40.9563385449745));
#79452=CARTESIAN_POINT('Ctrl Pts',(0.614556259703009,-10.8773327542168,
40.5947584895701));
#79453=CARTESIAN_POINT('Ctrl Pts',(0.664285714285714,-12.2267678919897,
40.2331784341656));
#79454=CARTESIAN_POINT('Origin',(0.,-5.05459769747091,41.7451020134904));
#79455=CARTESIAN_POINT('',(0.664285714285704,-5.05459769747091,41.7451020134904));
#79456=CARTESIAN_POINT('',(0.,-5.05459769747091,41.7451020134904));
#79457=CARTESIAN_POINT('',(6.93889390390723E-17,-5.03287931686985,41.1231689657038));
#79458=CARTESIAN_POINT('Ctrl Pts',(0.664285714285704,-5.05459769747091,
41.7451020134904));
#79459=CARTESIAN_POINT('Ctrl Pts',(0.329657625021025,-5.04365785681047,
41.4318259654634));
#79460=CARTESIAN_POINT('Ctrl Pts',(6.93889390390723E-17,-5.03287931686985,
41.1231689657038));
#79461=CARTESIAN_POINT('',(0.,-4.89515034526194,37.1791272503441));
#79462=CARTESIAN_POINT('',(0.,-5.05459769747091,41.7451020134904));
#79463=CARTESIAN_POINT('',(0.,-4.89515034526194,37.1791272503441));
#79464=CARTESIAN_POINT('',(11.,-4.90566824265506,37.4803204240973));
#79465=CARTESIAN_POINT('',(22.,-4.89515034526194,37.1791272503441));
#79466=CARTESIAN_POINT('',(0.,-4.89515034526194,37.1791272503441));
#79467=CARTESIAN_POINT('',(22.,-5.05459769747091,41.7451020134904));
#79468=CARTESIAN_POINT('Origin',(0.,-2.2711538903357,41.9886217921762));
#79469=CARTESIAN_POINT('',(0.6642857142857,-2.2711538903357,41.9886217921762));
#79470=CARTESIAN_POINT('',(0.,-2.2711538903357,41.9886217921762));
#79471=CARTESIAN_POINT('Ctrl Pts',(0.6642857142857,-2.2711538903357,41.9886217921762));
#79472=CARTESIAN_POINT('Ctrl Pts',(0.614556259702998,-3.66287579390335,
41.8668619028333));
#79473=CARTESIAN_POINT('Ctrl Pts',(0.664285714285704,-5.05459769747091,
41.7451020134904));
#79474=CARTESIAN_POINT('Origin',(0.,2.27115389033571,41.9886217921762));
#79475=CARTESIAN_POINT('',(0.66428571428571,2.27115389033571,41.9886217921762));
#79476=CARTESIAN_POINT('',(0.,2.27115389033571,41.9886217921762));
#79477=CARTESIAN_POINT('',(-6.93889390390723E-17,2.18454477955552,41.3723659476482));
#79478=CARTESIAN_POINT('Ctrl Pts',(0.66428571428571,2.27115389033571,41.9886217921762));
#79479=CARTESIAN_POINT('Ctrl Pts',(0.329657622668474,2.22752771508157,41.6782054256694));
#79480=CARTESIAN_POINT('Ctrl Pts',(-6.93889390390723E-17,2.18454477955552,
41.3723659476482));
#79481=CARTESIAN_POINT('',(0.,1.63530568209483,37.4643267032268));
#79482=CARTESIAN_POINT('',(0.,2.27115389033571,41.9886217921762));
#79483=CARTESIAN_POINT('',(0.,1.63530568209483,37.4643267032268));
#79484=CARTESIAN_POINT('',(11.,1.67724922094465,37.7627704896084));
#79485=CARTESIAN_POINT('',(22.,1.63530568209483,37.4643267032268));
#79486=CARTESIAN_POINT('',(0.,1.63530568209483,37.4643267032268));
#79487=CARTESIAN_POINT('',(22.,2.27115389033571,41.9886217921762));
#79488=CARTESIAN_POINT('Origin',(0.,5.05459769747092,41.7451020134904));
#79489=CARTESIAN_POINT('',(0.664285714285704,5.05459769747092,41.7451020134904));
#79490=CARTESIAN_POINT('',(0.,5.05459769747092,41.7451020134904));
#79491=CARTESIAN_POINT('Ctrl Pts',(0.664285714285704,5.05459769747092,41.7451020134904));
#79492=CARTESIAN_POINT('Ctrl Pts',(0.614556259703005,3.66287579390327,41.8668619028333));
#79493=CARTESIAN_POINT('Ctrl Pts',(0.66428571428571,2.27115389033571,41.9886217921762));
#79494=CARTESIAN_POINT('Origin',(0.,9.5278976164438,40.9563385449745));
#79495=CARTESIAN_POINT('',(0.664285714285704,9.5278976164438,40.9563385449745));
#79496=CARTESIAN_POINT('',(0.,9.5278976164438,40.9563385449745));
#79497=CARTESIAN_POINT('',(0.,9.33559258828709,40.3644845257006));
#79498=CARTESIAN_POINT('Ctrl Pts',(0.664285714285704,9.5278976164438,40.9563385449745));
#79499=CARTESIAN_POINT('Ctrl Pts',(0.329657623132566,9.43103098459169,40.6582137068217));
#79500=CARTESIAN_POINT('Ctrl Pts',(-6.93889390390723E-17,9.33559258828709,
40.3644845257006));
#79501=CARTESIAN_POINT('',(0.,8.11607377380574,36.6111915470959));
#79502=CARTESIAN_POINT('',(0.,9.5278976164438,40.9563385449745));
#79503=CARTESIAN_POINT('',(0.,8.11607377380574,36.6111915470959));
#79504=CARTESIAN_POINT('',(11.,8.20920431569501,36.8978178826767));
#79505=CARTESIAN_POINT('',(22.,8.11607377380574,36.6111915470959));
#79506=CARTESIAN_POINT('',(0.,8.11607377380574,36.6111915470959));
#79507=CARTESIAN_POINT('',(22.,9.5278976164438,40.9563385449745));
#79508=CARTESIAN_POINT('Origin',(0.,12.2267678919897,40.2331784341656));
#79509=CARTESIAN_POINT('',(0.664285714285704,12.2267678919897,40.2331784341656));
#79510=CARTESIAN_POINT('',(0.,12.2267678919897,40.2331784341656));
#79511=CARTESIAN_POINT('Ctrl Pts',(0.664285714285704,12.2267678919897,40.2331784341656));
#79512=CARTESIAN_POINT('Ctrl Pts',(0.614556259702999,10.8773327542167,40.5947584895701));
#79513=CARTESIAN_POINT('Ctrl Pts',(0.664285714285704,9.5278976164438,40.9563385449745));
#79514=CARTESIAN_POINT('Origin',(0.,16.4951409948251,38.6796176759911));
#79515=CARTESIAN_POINT('',(0.66428571428571,16.4951409948251,38.6796176759911));
#79516=CARTESIAN_POINT('',(0.,16.4951409948251,38.6796176759911));
#79517=CARTESIAN_POINT('',(6.93889390390723E-17,16.2029831402613,38.1301486668542));
#79518=CARTESIAN_POINT('Ctrl Pts',(0.66428571428571,16.4951409948251,38.6796176759911));
#79519=CARTESIAN_POINT('Ctrl Pts',(0.329657621910239,16.3479771493689,38.4028427370996));
#79520=CARTESIAN_POINT('Ctrl Pts',(0.,16.2029831402613,38.1301486668543));
#79521=CARTESIAN_POINT('',(0.,14.3502390708311,34.6456438619633));
#79522=CARTESIAN_POINT('',(0.,16.4951409948251,38.6796176759911));
#79523=CARTESIAN_POINT('',(0.,14.3502390708311,34.6456438619633));
#79524=CARTESIAN_POINT('',(11.,14.4917268913708,34.9117437505765));
#79525=CARTESIAN_POINT('',(22.,14.3502390708311,34.6456438619633));
#79526=CARTESIAN_POINT('',(0.,14.3502390708311,34.6456438619633));
#79527=CARTESIAN_POINT('',(22.,16.4951409948251,38.6796176759911));
#79528=CARTESIAN_POINT('Origin',(0.,19.0274339311535,37.4987900870893));
#79529=CARTESIAN_POINT('',(0.664285714285716,19.0274339311535,37.4987900870893));
#79530=CARTESIAN_POINT('',(0.,19.0274339311535,37.4987900870893));
#79531=CARTESIAN_POINT('Ctrl Pts',(0.664285714285716,19.0274339311535,37.4987900870893));
#79532=CARTESIAN_POINT('Ctrl Pts',(0.614556259703006,17.7612874629893,38.0892038815402));
#79533=CARTESIAN_POINT('Ctrl Pts',(0.66428571428571,16.4951409948251,38.6796176759911));
#79534=CARTESIAN_POINT('Origin',(0.,22.9611878610227,35.2276361967536));
#79535=CARTESIAN_POINT('',(0.664285714285716,22.9611878610227,35.2276361967536));
#79536=CARTESIAN_POINT('',(0.,22.9611878610227,35.2276361967536));
#79537=CARTESIAN_POINT('',(-2.77555756156289E-16,22.5780542486238,34.7372475355518));
#79538=CARTESIAN_POINT('Ctrl Pts',(0.664285714285716,22.9611878610227,35.2276361967536));
#79539=CARTESIAN_POINT('Ctrl Pts',(0.329657619188245,22.7681982997223,34.9806208226665));
#79540=CARTESIAN_POINT('Ctrl Pts',(-2.77555756156289E-16,22.5780542486238,
34.7372475355518));
#79541=CARTESIAN_POINT('',(0.,20.1483796152605,31.6274058196267));
#79542=CARTESIAN_POINT('',(0.,22.9611878610227,35.2276361967536));
#79543=CARTESIAN_POINT('',(0.,20.1483796152605,31.6274058196267));
#79544=CARTESIAN_POINT('',(11.,20.3339256786199,31.8648939508099));
#79545=CARTESIAN_POINT('',(22.,20.1483796152605,31.6274058196267));
#79546=CARTESIAN_POINT('',(0.,20.1483796152605,31.6274058196267));
#79547=CARTESIAN_POINT('',(22.,22.9611878610227,35.2276361967536));
#79548=CARTESIAN_POINT('Origin',(0.,25.2499610186653,33.6250199785202));
#79549=CARTESIAN_POINT('',(0.664285714285713,25.2499610186653,33.6250199785202));
#79550=CARTESIAN_POINT('',(0.,25.2499610186653,33.6250199785202));
#79551=CARTESIAN_POINT('Ctrl Pts',(0.664285714285713,25.2499610186653,33.6250199785202));
#79552=CARTESIAN_POINT('Ctrl Pts',(0.614556259703012,24.105574439844,34.4263280876369));
#79553=CARTESIAN_POINT('Ctrl Pts',(0.664285714285716,22.9611878610227,35.2276361967536));
#79554=CARTESIAN_POINT('Origin',(0.,28.7295706529848,30.7052808177218));
#79555=CARTESIAN_POINT('',(0.664285714285715,28.7295706529848,30.7052808177218));
#79556=CARTESIAN_POINT('',(0.,28.7295706529848,30.7052808177218));
#79557=CARTESIAN_POINT('',(0.,28.2671026036886,30.288872715777));
#79558=CARTESIAN_POINT('Ctrl Pts',(0.664285714285715,28.7295706529848,30.7052808177218));
#79559=CARTESIAN_POINT('Ctrl Pts',(0.329657620568989,28.4966192681609,30.4955304487016));
#79560=CARTESIAN_POINT('Ctrl Pts',(-2.77555756156289E-16,28.2671026036886,
30.288872715777));
#79561=CARTESIAN_POINT('',(0.,25.3343218406523,27.6481850557002));
#79562=CARTESIAN_POINT('',(0.,28.7295706529848,30.7052808177218));
#79563=CARTESIAN_POINT('',(0.,25.3343218406523,27.6481850557002));
#79564=CARTESIAN_POINT('',(11.,25.5582884235871,27.8498454727622));
#79565=CARTESIAN_POINT('',(22.,25.3343218406523,27.6481850557002));
#79566=CARTESIAN_POINT('',(0.,25.3343218406523,27.6481850557002));
#79567=CARTESIAN_POINT('',(22.,28.7295706529848,30.7052808177218));
#79568=CARTESIAN_POINT('Origin',(0.,30.7052808177218,28.7295706529848));
#79569=CARTESIAN_POINT('',(0.664285714285712,30.7052808177218,28.7295706529848));
#79570=CARTESIAN_POINT('',(0.,30.7052808177218,28.7295706529848));
#79571=CARTESIAN_POINT('Ctrl Pts',(0.664285714285712,30.7052808177218,28.7295706529848));
#79572=CARTESIAN_POINT('Ctrl Pts',(0.614556259703008,29.7174257353533,29.7174257353533));
#79573=CARTESIAN_POINT('Ctrl Pts',(0.664285714285715,28.7295706529848,30.7052808177218));
#79574=CARTESIAN_POINT('Origin',(0.,33.6250199785202,25.2499610186653));
#79575=CARTESIAN_POINT('',(0.664285714285709,33.6250199785202,25.2499610186653));
#79576=CARTESIAN_POINT('',(0.,33.6250199785202,25.2499610186653));
#79577=CARTESIAN_POINT('',(1.38777878078145E-16,33.0972693499844,24.9201858254425));
#79578=CARTESIAN_POINT('Ctrl Pts',(0.664285714285709,33.6250199785202,25.2499610186653));
#79579=CARTESIAN_POINT('Ctrl Pts',(0.329657623920708,33.3591848819878,25.0838488141804));
#79580=CARTESIAN_POINT('Ctrl Pts',(4.16333634234434E-16,33.0972693499844,
24.9201858254425));
#79581=CARTESIAN_POINT('',(0.,29.7504935167013,22.8288881795131));
#79582=CARTESIAN_POINT('',(0.,33.6250199785202,25.2499610186653));
#79583=CARTESIAN_POINT('',(0.,29.7504935167013,22.8288881795131));
#79584=CARTESIAN_POINT('',(11.,30.0060755079215,22.9885935327265));
#79585=CARTESIAN_POINT('',(22.,29.7504935167013,22.8288881795131));
#79586=CARTESIAN_POINT('',(0.,29.7504935167013,22.8288881795131));
#79587=CARTESIAN_POINT('',(22.,33.6250199785202,25.2499610186653));
#79588=CARTESIAN_POINT('Origin',(0.,35.2276361967536,22.9611878610227));
#79589=CARTESIAN_POINT('',(0.664285714285705,35.2276361967536,22.9611878610227));
#79590=CARTESIAN_POINT('',(0.,35.2276361967536,22.9611878610227));
#79591=CARTESIAN_POINT('Ctrl Pts',(0.664285714285705,35.2276361967536,22.9611878610227));
#79592=CARTESIAN_POINT('Ctrl Pts',(0.614556259703003,34.4263280876369,24.105574439844));
#79593=CARTESIAN_POINT('Ctrl Pts',(0.664285714285709,33.6250199785202,25.2499610186653));
#79594=CARTESIAN_POINT('Origin',(0.,37.4987900870893,19.0274339311535));
#79595=CARTESIAN_POINT('',(0.664285714285711,37.4987900870893,19.0274339311535));
#79596=CARTESIAN_POINT('',(0.,37.4987900870893,19.0274339311535));
#79597=CARTESIAN_POINT('',(-1.38777878078145E-16,36.9217923151073,18.7943116990243));
#79598=CARTESIAN_POINT('Ctrl Pts',(0.664285714285711,37.4987900870893,19.0274339311535));
#79599=CARTESIAN_POINT('Ctrl Pts',(0.329657629073952,37.2081485458799,18.9100071261878));
#79600=CARTESIAN_POINT('Ctrl Pts',(2.08166817117217E-16,36.9217923151073,
18.7943116990243));
#79601=CARTESIAN_POINT('',(0.,33.2627115017215,17.3159470879662));
#79602=CARTESIAN_POINT('',(0.,37.4987900870893,19.0274339311535));
#79603=CARTESIAN_POINT('',(0.,33.2627115017215,17.3159470879662));
#79604=CARTESIAN_POINT('',(11.,33.5421431717545,17.4288448109885));
#79605=CARTESIAN_POINT('',(22.,33.2627115017215,17.3159470879662));
#79606=CARTESIAN_POINT('',(0.,33.2627115017215,17.3159470879662));
#79607=CARTESIAN_POINT('',(22.,37.4987900870893,19.0274339311535));
#79608=CARTESIAN_POINT('Origin',(0.,38.6796176759911,16.4951409948251));
#79609=CARTESIAN_POINT('',(0.66428571428571,38.6796176759911,16.4951409948251));
#79610=CARTESIAN_POINT('',(0.,38.6796176759911,16.4951409948251));
#79611=CARTESIAN_POINT('Ctrl Pts',(0.66428571428571,38.6796176759911,16.4951409948251));
#79612=CARTESIAN_POINT('Ctrl Pts',(0.614556259703007,38.0892038815402,17.7612874629893));
#79613=CARTESIAN_POINT('Ctrl Pts',(0.664285714285711,37.4987900870893,19.0274339311535));
#79614=CARTESIAN_POINT('Origin',(0.,40.2331784341656,12.2267678919897));
#79615=CARTESIAN_POINT('',(0.664285714285714,40.2331784341656,12.2267678919897));
#79616=CARTESIAN_POINT('',(0.,40.2331784341656,12.2267678919897));
#79617=CARTESIAN_POINT('',(0.,39.6244653040641,12.0973819220119));
#79618=CARTESIAN_POINT('Ctrl Pts',(0.664285714285714,40.2331784341656,12.2267678919897));
#79619=CARTESIAN_POINT('Ctrl Pts',(0.329657622780289,39.9265614345773,12.1615944368077));
#79620=CARTESIAN_POINT('Ctrl Pts',(-6.93889390390723E-17,39.6244653040641,
12.0973819220119));
#79621=CARTESIAN_POINT('',(0.,35.764258829506,11.2768697064435));
#79622=CARTESIAN_POINT('',(0.,40.2331784341656,12.2267678919897));
#79623=CARTESIAN_POINT('',(0.,35.764258829506,11.2768697064435));
#79624=CARTESIAN_POINT('',(11.,36.0590497884573,11.3395294590896));
#79625=CARTESIAN_POINT('',(22.,35.764258829506,11.2768697064435));
#79626=CARTESIAN_POINT('',(0.,35.764258829506,11.2768697064435));
#79627=CARTESIAN_POINT('',(22.,40.2331784341656,12.2267678919897));
#79628=CARTESIAN_POINT('Origin',(0.,40.9563385449745,9.5278976164438));
#79629=CARTESIAN_POINT('',(0.664285714285714,40.9563385449745,9.52789761644379));
#79630=CARTESIAN_POINT('',(0.,40.9563385449745,9.5278976164438));
#79631=CARTESIAN_POINT('Ctrl Pts',(0.664285714285714,40.9563385449745,9.52789761644379));
#79632=CARTESIAN_POINT('Ctrl Pts',(0.614556259703009,40.5947584895701,10.8773327542168));
#79633=CARTESIAN_POINT('Ctrl Pts',(0.664285714285714,40.2331784341656,12.2267678919897));
#79634=CARTESIAN_POINT('Origin',(0.45,0.,0.));
#79635=CARTESIAN_POINT('',(0.,40.3644845257006,9.33559258828708));
#79636=CARTESIAN_POINT('Ctrl Pts',(6.93889390390723E-17,40.3644845257006,
9.33559258828708));
#79637=CARTESIAN_POINT('Ctrl Pts',(0.32965762598791,40.6582137093653,9.43103098541816));
#79638=CARTESIAN_POINT('Ctrl Pts',(0.664285714285714,40.9563385449745,9.52789761644379));
#79639=CARTESIAN_POINT('Origin',(0.,0.,0.));
#79640=CARTESIAN_POINT('Origin',(0.45,0.,0.));
#79641=CARTESIAN_POINT('',(0.,38.1301486668543,16.2029831402613));
#79642=CARTESIAN_POINT('Ctrl Pts',(-2.08166817117217E-16,38.1301486668543,
16.2029831402613));
#79643=CARTESIAN_POINT('Ctrl Pts',(0.32965762185849,38.4028427370567,16.3479771493462));
#79644=CARTESIAN_POINT('Ctrl Pts',(0.66428571428571,38.6796176759911,16.4951409948251));
#79645=CARTESIAN_POINT('Origin',(0.,0.,0.));
#79646=CARTESIAN_POINT('Origin',(0.45,0.,0.));
#79647=CARTESIAN_POINT('',(-3.46944695195361E-16,34.7372475355518,22.5780542486238));
#79648=CARTESIAN_POINT('Ctrl Pts',(-3.46944695195361E-16,34.7372475355518,
22.5780542486238));
#79649=CARTESIAN_POINT('Ctrl Pts',(0.329657620646495,34.9806208237429,22.7681983005632));
#79650=CARTESIAN_POINT('Ctrl Pts',(0.664285714285705,35.2276361967536,22.9611878610227));
#79651=CARTESIAN_POINT('Origin',(0.,0.,0.));
#79652=CARTESIAN_POINT('Origin',(0.45,0.,0.));
#79653=CARTESIAN_POINT('',(5.55111512312578E-16,30.288872715777,28.2671026036886));
#79654=CARTESIAN_POINT('Ctrl Pts',(6.93889390390723E-17,30.288872715777,
28.2671026036886));
#79655=CARTESIAN_POINT('Ctrl Pts',(0.329657619423762,30.4955304479838,28.4966192673637));
#79656=CARTESIAN_POINT('Ctrl Pts',(0.664285714285712,30.7052808177218,28.7295706529848));
#79657=CARTESIAN_POINT('Origin',(0.,0.,0.));
#79658=CARTESIAN_POINT('Origin',(0.45,0.,0.));
#79659=CARTESIAN_POINT('',(0.,24.9201858254425,33.0972693499844));
#79660=CARTESIAN_POINT('Ctrl Pts',(2.08166817117217E-16,24.9201858254425,
33.0972693499844));
#79661=CARTESIAN_POINT('Ctrl Pts',(0.329657620988788,25.0838488127251,33.3591848796588));
#79662=CARTESIAN_POINT('Ctrl Pts',(0.664285714285713,25.2499610186653,33.6250199785202));
#79663=CARTESIAN_POINT('Origin',(0.,0.,0.));
#79664=CARTESIAN_POINT('Origin',(0.45,0.,0.));
#79665=CARTESIAN_POINT('',(1.38777878078145E-16,18.7943116990243,36.9217923151073));
#79666=CARTESIAN_POINT('Ctrl Pts',(-6.93889390390723E-17,18.7943116990243,
36.9217923151073));
#79667=CARTESIAN_POINT('Ctrl Pts',(0.329657618925708,18.9100071226269,37.2081485370664));
#79668=CARTESIAN_POINT('Ctrl Pts',(0.664285714285716,19.0274339311535,37.4987900870893));
#79669=CARTESIAN_POINT('Origin',(0.,0.,0.));
#79670=CARTESIAN_POINT('Origin',(0.45,0.,0.));
#79671=CARTESIAN_POINT('',(6.93889390390723E-17,12.097381922012,39.6244653040641));
#79672=CARTESIAN_POINT('Ctrl Pts',(1.38777878078145E-16,12.097381922012,
39.6244653040641));
#79673=CARTESIAN_POINT('Ctrl Pts',(0.329657622650879,12.1615944367825,39.9265614344587));
#79674=CARTESIAN_POINT('Ctrl Pts',(0.664285714285704,12.2267678919897,40.2331784341656));
#79675=CARTESIAN_POINT('Origin',(0.,0.,0.));
#79676=CARTESIAN_POINT('Origin',(0.45,0.,0.));
#79677=CARTESIAN_POINT('',(6.93889390390723E-17,5.03287931686986,41.1231689657038));
#79678=CARTESIAN_POINT('Ctrl Pts',(0.,5.03287931686986,41.1231689657038));
#79679=CARTESIAN_POINT('Ctrl Pts',(0.329657625188712,5.04365785681596,41.4318259656204));
#79680=CARTESIAN_POINT('Ctrl Pts',(0.664285714285704,5.05459769747092,41.7451020134904));
#79681=CARTESIAN_POINT('Origin',(0.,0.,0.));
#79682=CARTESIAN_POINT('Origin',(0.45,0.,0.));
#79683=CARTESIAN_POINT('',(-6.93889390390723E-17,-2.18454477955551,41.3723659476482));
#79684=CARTESIAN_POINT('Ctrl Pts',(0.,-2.18454477955551,41.3723659476482));
#79685=CARTESIAN_POINT('Ctrl Pts',(0.32965762278925,-2.2275277150973,41.6782054257814));
#79686=CARTESIAN_POINT('Ctrl Pts',(0.6642857142857,-2.2711538903357,41.9886217921762));
#79687=CARTESIAN_POINT('Origin',(0.,0.,0.));
#79688=CARTESIAN_POINT('Origin',(0.45,0.,0.));
#79689=CARTESIAN_POINT('',(1.38777878078145E-16,-9.33559258828708,40.3644845257006));
#79690=CARTESIAN_POINT('Ctrl Pts',(0.,-9.33559258828708,40.3644845257006));
#79691=CARTESIAN_POINT('Ctrl Pts',(0.329657625964886,-9.43103098541149,
40.6582137093448));
#79692=CARTESIAN_POINT('Ctrl Pts',(0.664285714285714,-9.52789761644379,
40.9563385449745));
#79693=CARTESIAN_POINT('Origin',(0.,0.,0.));
#79694=CARTESIAN_POINT('Origin',(0.45,0.,0.));
#79695=CARTESIAN_POINT('',(0.,-16.2029831402613,38.1301486668543));
#79696=CARTESIAN_POINT('Ctrl Pts',(-1.38777878078145E-16,-16.2029831402613,
38.1301486668543));
#79697=CARTESIAN_POINT('Ctrl Pts',(0.329657621211232,-16.3479771490615,
38.4028427365214));
#79698=CARTESIAN_POINT('Ctrl Pts',(0.66428571428571,-16.4951409948251,38.6796176759911));
#79699=CARTESIAN_POINT('Origin',(0.,0.,0.));
#79700=CARTESIAN_POINT('Origin',(0.45,0.,0.));
#79701=CARTESIAN_POINT('',(3.46944695195361E-16,-28.2671026036886,30.288872715777));
#79702=CARTESIAN_POINT('Ctrl Pts',(1.38777878078145E-16,-28.2671026036886,
30.288872715777));
#79703=CARTESIAN_POINT('Ctrl Pts',(0.329657622690223,-28.4966192696375,
30.4955304500311));
#79704=CARTESIAN_POINT('Ctrl Pts',(0.664285714285709,-28.7295706529848,
30.7052808177218));
#79705=CARTESIAN_POINT('Origin',(0.,0.,0.));
#79706=CARTESIAN_POINT('Origin',(0.45,0.,0.));
#79707=CARTESIAN_POINT('',(6.93889390390723E-17,-33.0972693499844,24.9201858254425));
#79708=CARTESIAN_POINT('Ctrl Pts',(4.16333634234434E-16,-33.0972693499844,
24.9201858254425));
#79709=CARTESIAN_POINT('Ctrl Pts',(0.329657624090997,-33.3591848821231,
25.0838488142649));
#79710=CARTESIAN_POINT('Ctrl Pts',(0.664285714285703,-33.6250199785202,
25.2499610186654));
#79711=CARTESIAN_POINT('Origin',(0.,0.,0.));
#79712=CARTESIAN_POINT('Origin',(0.45,0.,0.));
#79713=CARTESIAN_POINT('',(-1.38777878078145E-16,-36.9217923151073,18.7943116990243));
#79714=CARTESIAN_POINT('Ctrl Pts',(1.38777878078145E-16,-36.9217923151073,
18.7943116990243));
#79715=CARTESIAN_POINT('Ctrl Pts',(0.329657619578977,-37.2081485376338,
18.9100071228561));
#79716=CARTESIAN_POINT('Ctrl Pts',(0.664285714285704,-37.4987900870893,
19.0274339311535));
#79717=CARTESIAN_POINT('Origin',(0.,0.,0.));
#79718=CARTESIAN_POINT('Origin',(0.45,0.,0.));
#79719=CARTESIAN_POINT('',(0.,-39.6244653040641,12.097381922012));
#79720=CARTESIAN_POINT('Ctrl Pts',(0.,-39.6244653040641,12.097381922012));
#79721=CARTESIAN_POINT('Ctrl Pts',(0.329657619736489,-39.9265614317885,
12.1615944362149));
#79722=CARTESIAN_POINT('Ctrl Pts',(0.664285714285703,-40.2331784341656,
12.2267678919897));
#79723=CARTESIAN_POINT('Origin',(0.,0.,0.));
#79724=CARTESIAN_POINT('Origin',(0.45,0.,0.));
#79725=CARTESIAN_POINT('',(-6.93889390390723E-17,-41.1231689657038,5.03287931686987));
#79726=CARTESIAN_POINT('Ctrl Pts',(0.,-41.1231689657038,5.03287931686987));
#79727=CARTESIAN_POINT('Ctrl Pts',(0.329657625064268,-41.4318259655039,
5.0436578568119));
#79728=CARTESIAN_POINT('Ctrl Pts',(0.664285714285704,-41.7451020134904,
5.05459769747093));
#79729=CARTESIAN_POINT('Origin',(0.,0.,0.));
#79730=CARTESIAN_POINT('Origin',(0.45,0.,0.));
#79731=CARTESIAN_POINT('',(-6.93889390390723E-17,-41.3723659476482,-2.18454477955551));
#79732=CARTESIAN_POINT('Ctrl Pts',(6.93889390390723E-17,-41.3723659476482,
-2.18454477955551));
#79733=CARTESIAN_POINT('Ctrl Pts',(0.329657625843401,-41.6782054286144,
-2.22752771549544));
#79734=CARTESIAN_POINT('Ctrl Pts',(0.6642857142857,-41.9886217921762,-2.2711538903357));
#79735=CARTESIAN_POINT('Origin',(0.,0.,0.));
#79736=CARTESIAN_POINT('Origin',(0.45,0.,0.));
#79737=CARTESIAN_POINT('',(1.38777878078145E-16,-40.3644845257006,-9.33559258828707));
#79738=CARTESIAN_POINT('Ctrl Pts',(2.77555756156289E-16,-40.3644845257006,
-9.33559258828707));
#79739=CARTESIAN_POINT('Ctrl Pts',(0.329657625997959,-40.6582137093743,
-9.43103098542106));
#79740=CARTESIAN_POINT('Ctrl Pts',(0.664285714285713,-40.9563385449745,
-9.52789761644378));
#79741=CARTESIAN_POINT('Origin',(0.,0.,0.));
#79742=CARTESIAN_POINT('Origin',(0.45,0.,0.));
#79743=CARTESIAN_POINT('',(-2.08166817117217E-16,-38.1301486668543,-16.2029831402613));
#79744=CARTESIAN_POINT('Ctrl Pts',(1.38777878078145E-16,-38.1301486668543,
-16.2029831402613));
#79745=CARTESIAN_POINT('Ctrl Pts',(0.329657621863082,-38.4028427370606,
-16.3479771493482));
#79746=CARTESIAN_POINT('Ctrl Pts',(0.664285714285701,-38.6796176759911,
-16.4951409948251));
#79747=CARTESIAN_POINT('Origin',(0.,0.,0.));
#79748=CARTESIAN_POINT('Origin',(0.45,0.,0.));
#79749=CARTESIAN_POINT('',(-2.08166817117217E-16,-34.7372475355518,-22.5780542486238));
#79750=CARTESIAN_POINT('Ctrl Pts',(-4.16333634234434E-16,-34.7372475355518,
-22.5780542486238));
#79751=CARTESIAN_POINT('Ctrl Pts',(0.329657621436075,-34.9806208243257,
-22.7681983010185));
#79752=CARTESIAN_POINT('Ctrl Pts',(0.664285714285711,-35.2276361967536,
-22.9611878610227));
#79753=CARTESIAN_POINT('Origin',(0.,0.,0.));
#79754=CARTESIAN_POINT('Origin',(0.45,0.,0.));
#79755=CARTESIAN_POINT('',(5.55111512312578E-16,-30.288872715777,-28.2671026036886));
#79756=CARTESIAN_POINT('Ctrl Pts',(6.93889390390723E-17,-30.288872715777,
-28.2671026036886));
#79757=CARTESIAN_POINT('Ctrl Pts',(0.329657619423762,-30.4955304479838,
-28.4966192673637));
#79758=CARTESIAN_POINT('Ctrl Pts',(0.664285714285712,-30.7052808177218,
-28.7295706529848));
#79759=CARTESIAN_POINT('Origin',(0.,0.,0.));
#79760=CARTESIAN_POINT('Origin',(0.45,0.,0.));
#79761=CARTESIAN_POINT('',(0.,-24.9201858254425,-33.0972693499844));
#79762=CARTESIAN_POINT('Ctrl Pts',(2.77555756156289E-16,-24.9201858254425,
-33.0972693499844));
#79763=CARTESIAN_POINT('Ctrl Pts',(0.329657623996619,-25.0838488142181,
-33.3591848820481));
#79764=CARTESIAN_POINT('Ctrl Pts',(0.664285714285703,-25.2499610186654,
-33.6250199785202));
#79765=CARTESIAN_POINT('Origin',(0.,0.,0.));
#79766=CARTESIAN_POINT('Origin',(0.45,0.,0.));
#79767=CARTESIAN_POINT('',(-6.93889390390723E-17,-12.097381922012,-39.6244653040641));
#79768=CARTESIAN_POINT('Ctrl Pts',(-6.93889390390723E-17,-12.097381922012,
-39.6244653040641));
#79769=CARTESIAN_POINT('Ctrl Pts',(0.329657619756358,-12.1615944362188,
-39.9265614318067));
#79770=CARTESIAN_POINT('Ctrl Pts',(0.664285714285714,-12.2267678919898,
-40.2331784341656));
#79771=CARTESIAN_POINT('Origin',(0.,0.,0.));
#79772=CARTESIAN_POINT('Origin',(0.45,0.,0.));
#79773=CARTESIAN_POINT('',(-6.93889390390723E-17,-5.03287931686986,-41.1231689657038));
#79774=CARTESIAN_POINT('Ctrl Pts',(0.,-5.03287931686986,-41.1231689657038));
#79775=CARTESIAN_POINT('Ctrl Pts',(0.329657619114913,-5.04365785661741,
-41.4318259599347));
#79776=CARTESIAN_POINT('Ctrl Pts',(0.664285714285704,-5.05459769747091,
-41.7451020134904));
#79777=CARTESIAN_POINT('Origin',(0.,0.,0.));
#79778=CARTESIAN_POINT('Origin',(0.45,0.,0.));
#79779=CARTESIAN_POINT('',(0.,2.1845447795555,-41.3723659476482));
#79780=CARTESIAN_POINT('Ctrl Pts',(6.93889390390723E-17,2.1845447795555,
-41.3723659476482));
#79781=CARTESIAN_POINT('Ctrl Pts',(0.32965762590867,2.22752771550395,-41.6782054286749));
#79782=CARTESIAN_POINT('Ctrl Pts',(0.6642857142857,2.2711538903357,-41.9886217921762));
#79783=CARTESIAN_POINT('Origin',(0.,0.,0.));
#79784=CARTESIAN_POINT('Origin',(0.45,0.,0.));
#79785=CARTESIAN_POINT('',(2.77555756156289E-16,9.33559258828707,-40.3644845257006));
#79786=CARTESIAN_POINT('Ctrl Pts',(2.77555756156289E-16,9.33559258828707,
-40.3644845257006));
#79787=CARTESIAN_POINT('Ctrl Pts',(0.329657625970749,9.43103098541318,-40.65821370935));
#79788=CARTESIAN_POINT('Ctrl Pts',(0.664285714285714,9.52789761644378,-40.9563385449745));
#79789=CARTESIAN_POINT('Origin',(0.,0.,0.));
#79790=CARTESIAN_POINT('Origin',(0.45,0.,0.));
#79791=CARTESIAN_POINT('',(0.,16.2029831402613,-38.1301486668543));
#79792=CARTESIAN_POINT('Ctrl Pts',(1.38777878078145E-16,16.2029831402613,
-38.1301486668543));
#79793=CARTESIAN_POINT('Ctrl Pts',(0.329657621074924,16.3479771490016,-38.4028427364087));
#79794=CARTESIAN_POINT('Ctrl Pts',(0.664285714285715,16.4951409948251,-38.6796176759911));
#79795=CARTESIAN_POINT('Origin',(0.,0.,0.));
#79796=CARTESIAN_POINT('Origin',(0.45,0.,0.));
#79797=CARTESIAN_POINT('',(3.46944695195361E-16,22.5780542486238,-34.7372475355518));
#79798=CARTESIAN_POINT('Ctrl Pts',(4.16333634234434E-16,22.5780542486238,
-34.7372475355518));
#79799=CARTESIAN_POINT('Ctrl Pts',(0.329657618264121,22.7681982991893,-34.9806208219844));
#79800=CARTESIAN_POINT('Ctrl Pts',(0.664285714285709,22.9611878610227,-35.2276361967536));
#79801=CARTESIAN_POINT('Origin',(0.,0.,0.));
#79802=CARTESIAN_POINT('Origin',(0.45,0.,0.));
#79803=CARTESIAN_POINT('',(-4.16333634234434E-16,28.2671026036886,-30.288872715777));
#79804=CARTESIAN_POINT('Ctrl Pts',(-2.77555756156289E-16,28.2671026036886,
-30.288872715777));
#79805=CARTESIAN_POINT('Ctrl Pts',(0.329657616385251,28.4966192652486,-30.4955304460794));
#79806=CARTESIAN_POINT('Ctrl Pts',(0.664285714285712,28.7295706529848,-30.7052808177218));
#79807=CARTESIAN_POINT('Origin',(0.,0.,0.));
#79808=CARTESIAN_POINT('Origin',(0.45,0.,0.));
#79809=CARTESIAN_POINT('',(6.93889390390723E-17,33.0972693499844,-24.9201858254425));
#79810=CARTESIAN_POINT('Ctrl Pts',(0.,33.0972693499844,-24.9201858254425));
#79811=CARTESIAN_POINT('Ctrl Pts',(0.329657624117467,33.3591848821441,-25.0838488142781));
#79812=CARTESIAN_POINT('Ctrl Pts',(0.66428571428571,33.6250199785202,-25.2499610186654));
#79813=CARTESIAN_POINT('Origin',(0.,0.,0.));
#79814=CARTESIAN_POINT('Origin',(0.45,0.,0.));
#79815=CARTESIAN_POINT('',(6.93889390390723E-17,36.9217923151073,-18.7943116990244));
#79816=CARTESIAN_POINT('Ctrl Pts',(1.38777878078145E-16,36.9217923151073,
-18.7943116990244));
#79817=CARTESIAN_POINT('Ctrl Pts',(0.329657623048166,37.2081485406466,-18.9100071240734));
#79818=CARTESIAN_POINT('Ctrl Pts',(0.664285714285706,37.4987900870893,-19.0274339311535));
#79819=CARTESIAN_POINT('Origin',(0.,0.,0.));
#79820=CARTESIAN_POINT('Origin',(0.45,0.,0.));
#79821=CARTESIAN_POINT('',(6.93889390390723E-17,39.6244653040641,-12.097381922012));
#79822=CARTESIAN_POINT('Ctrl Pts',(6.93889390390723E-17,39.6244653040641,
-12.097381922012));
#79823=CARTESIAN_POINT('Ctrl Pts',(0.32965762272503,39.9265614345266,-12.1615944367969));
#79824=CARTESIAN_POINT('Ctrl Pts',(0.664285714285704,40.2331784341656,-12.2267678919898));
#79825=CARTESIAN_POINT('Origin',(0.,0.,0.));
#79826=CARTESIAN_POINT('Origin',(0.45,0.,0.));
#79827=CARTESIAN_POINT('',(6.93889390390723E-17,41.1231689657038,-5.03287931686986));
#79828=CARTESIAN_POINT('Ctrl Pts',(0.,41.1231689657038,-5.03287931686986));
#79829=CARTESIAN_POINT('Ctrl Pts',(0.329657622067524,41.4318259626987,-5.04365785671393));
#79830=CARTESIAN_POINT('Ctrl Pts',(0.664285714285704,41.7451020134904,-5.05459769747091));
#79831=CARTESIAN_POINT('Origin',(0.,0.,0.));
#79832=CARTESIAN_POINT('Origin',(0.,37.1791272503441,-4.89515034526195));
#79833=CARTESIAN_POINT('',(22.,37.1791272503441,-4.89515034526195));
#79834=CARTESIAN_POINT('',(22.,37.1791272503441,-4.89515034526195));
#79835=CARTESIAN_POINT('',(0.,37.1791272503441,-4.89515034526195));
#79836=CARTESIAN_POINT('',(11.,37.4803204240973,-4.90566824265507));
#79837=CARTESIAN_POINT('',(0.,37.1791272503441,-4.89515034526195));
#79838=CARTESIAN_POINT('',(0.,37.1791272503441,-4.89515034526195));
#79839=CARTESIAN_POINT('',(0.,37.1791272503441,-4.89515034526195));
#79840=CARTESIAN_POINT('Origin',(0.,35.764258829506,-11.2768697064435));
#79841=CARTESIAN_POINT('',(22.,35.764258829506,-11.2768697064435));
#79842=CARTESIAN_POINT('',(22.,35.764258829506,-11.2768697064435));
#79843=CARTESIAN_POINT('',(0.,35.764258829506,-11.2768697064435));
#79844=CARTESIAN_POINT('',(11.,36.0590497884572,-11.3395294590896));
#79845=CARTESIAN_POINT('',(0.,35.764258829506,-11.2768697064435));
#79846=CARTESIAN_POINT('',(0.,35.764258829506,-11.2768697064435));
#79847=CARTESIAN_POINT('',(0.,35.764258829506,-11.2768697064435));
#79848=CARTESIAN_POINT('Origin',(0.,33.2627115017215,-17.3159470879662));
#79849=CARTESIAN_POINT('',(22.,33.2627115017215,-17.3159470879662));
#79850=CARTESIAN_POINT('',(22.,33.2627115017215,-17.3159470879662));
#79851=CARTESIAN_POINT('',(0.,33.2627115017215,-17.3159470879662));
#79852=CARTESIAN_POINT('',(11.,33.5421431717545,-17.4288448109885));
#79853=CARTESIAN_POINT('',(0.,33.2627115017215,-17.3159470879662));
#79854=CARTESIAN_POINT('',(0.,33.2627115017215,-17.3159470879662));
#79855=CARTESIAN_POINT('',(0.,33.2627115017215,-17.3159470879662));
#79856=CARTESIAN_POINT('Origin',(0.,29.7504935167013,-22.8288881795131));
#79857=CARTESIAN_POINT('',(22.,29.7504935167013,-22.8288881795131));
#79858=CARTESIAN_POINT('',(22.,29.7504935167013,-22.8288881795131));
#79859=CARTESIAN_POINT('',(0.,29.7504935167013,-22.8288881795131));
#79860=CARTESIAN_POINT('',(11.,30.0060755079215,-22.9885935327265));
#79861=CARTESIAN_POINT('',(0.,29.7504935167013,-22.8288881795131));
#79862=CARTESIAN_POINT('',(0.,29.7504935167013,-22.8288881795131));
#79863=CARTESIAN_POINT('',(0.,29.7504935167013,-22.8288881795131));
#79864=CARTESIAN_POINT('Origin',(0.,25.3343218406523,-27.6481850557002));
#79865=CARTESIAN_POINT('',(22.,25.3343218406523,-27.6481850557002));
#79866=CARTESIAN_POINT('',(22.,25.3343218406523,-27.6481850557002));
#79867=CARTESIAN_POINT('',(0.,25.3343218406523,-27.6481850557002));
#79868=CARTESIAN_POINT('',(11.,25.5582884235871,-27.8498454727622));
#79869=CARTESIAN_POINT('',(0.,25.3343218406523,-27.6481850557002));
#79870=CARTESIAN_POINT('',(0.,25.3343218406523,-27.6481850557002));
#79871=CARTESIAN_POINT('',(0.,25.3343218406523,-27.6481850557002));
#79872=CARTESIAN_POINT('Origin',(0.,20.1483796152605,-31.6274058196267));
#79873=CARTESIAN_POINT('',(22.,20.1483796152605,-31.6274058196267));
#79874=CARTESIAN_POINT('',(22.,20.1483796152605,-31.6274058196267));
#79875=CARTESIAN_POINT('',(0.,20.1483796152605,-31.6274058196267));
#79876=CARTESIAN_POINT('',(11.,20.3339256786199,-31.8648939508099));
#79877=CARTESIAN_POINT('',(0.,20.1483796152605,-31.6274058196267));
#79878=CARTESIAN_POINT('',(0.,20.1483796152605,-31.6274058196267));
#79879=CARTESIAN_POINT('',(0.,20.1483796152605,-31.6274058196267));
#79880=CARTESIAN_POINT('Origin',(0.,14.350239070831,-34.6456438619633));
#79881=CARTESIAN_POINT('',(22.,14.350239070831,-34.6456438619633));
#79882=CARTESIAN_POINT('',(22.,14.350239070831,-34.6456438619633));
#79883=CARTESIAN_POINT('',(0.,14.350239070831,-34.6456438619633));
#79884=CARTESIAN_POINT('',(11.,14.4917268913708,-34.9117437505765));
#79885=CARTESIAN_POINT('',(0.,14.350239070831,-34.6456438619633));
#79886=CARTESIAN_POINT('',(0.,14.350239070831,-34.6456438619633));
#79887=CARTESIAN_POINT('',(0.,14.350239070831,-34.6456438619633));
#79888=CARTESIAN_POINT('Origin',(0.,8.11607377380573,-36.6111915470959));
#79889=CARTESIAN_POINT('',(22.,8.11607377380573,-36.6111915470959));
#79890=CARTESIAN_POINT('',(22.,8.11607377380573,-36.6111915470959));
#79891=CARTESIAN_POINT('',(0.,8.11607377380573,-36.6111915470959));
#79892=CARTESIAN_POINT('',(11.,8.209204315695,-36.8978178826767));
#79893=CARTESIAN_POINT('',(0.,8.11607377380573,-36.6111915470959));
#79894=CARTESIAN_POINT('',(0.,8.11607377380573,-36.6111915470959));
#79895=CARTESIAN_POINT('',(0.,8.11607377380573,-36.6111915470959));
#79896=CARTESIAN_POINT('Origin',(0.,1.63530568209482,-37.4643267032267));
#79897=CARTESIAN_POINT('',(22.,1.63530568209482,-37.4643267032267));
#79898=CARTESIAN_POINT('',(22.,1.63530568209482,-37.4643267032267));
#79899=CARTESIAN_POINT('',(0.,1.63530568209482,-37.4643267032267));
#79900=CARTESIAN_POINT('',(11.,1.67724922094464,-37.7627704896084));
#79901=CARTESIAN_POINT('',(0.,1.63530568209482,-37.4643267032267));
#79902=CARTESIAN_POINT('',(0.,1.63530568209482,-37.4643267032267));
#79903=CARTESIAN_POINT('',(0.,1.63530568209482,-37.4643267032267));
#79904=CARTESIAN_POINT('Origin',(0.,-4.89515034526194,-37.1791272503441));
#79905=CARTESIAN_POINT('',(22.,-4.89515034526194,-37.1791272503441));
#79906=CARTESIAN_POINT('',(22.,-4.89515034526194,-37.1791272503441));
#79907=CARTESIAN_POINT('',(0.,-4.89515034526194,-37.1791272503441));
#79908=CARTESIAN_POINT('',(11.,-4.90566824265507,-37.4803204240973));
#79909=CARTESIAN_POINT('',(0.,-4.89515034526194,-37.1791272503441));
#79910=CARTESIAN_POINT('',(0.,-4.89515034526194,-37.1791272503441));
#79911=CARTESIAN_POINT('',(0.,-4.89515034526194,-37.1791272503441));
#79912=CARTESIAN_POINT('Origin',(0.,-11.2768697064435,-35.764258829506));
#79913=CARTESIAN_POINT('',(22.,-11.2768697064435,-35.764258829506));
#79914=CARTESIAN_POINT('',(22.,-11.2768697064435,-35.764258829506));
#79915=CARTESIAN_POINT('',(0.,-11.2768697064435,-35.764258829506));
#79916=CARTESIAN_POINT('',(0.,-11.2768697064435,-35.764258829506));
#79917=CARTESIAN_POINT('',(0.,-11.2768697064435,-35.764258829506));
#79918=CARTESIAN_POINT('',(0.,-11.2768697064435,-35.764258829506));
#79919=CARTESIAN_POINT('Origin',(0.,-22.8288881795131,-29.7504935167013));
#79920=CARTESIAN_POINT('',(22.,-22.8288881795131,-29.7504935167013));
#79921=CARTESIAN_POINT('',(22.,-22.8288881795131,-29.7504935167013));
#79922=CARTESIAN_POINT('',(0.,-22.8288881795131,-29.7504935167013));
#79923=CARTESIAN_POINT('',(11.,-22.9885935327265,-30.0060755079215));
#79924=CARTESIAN_POINT('',(0.,-22.8288881795131,-29.7504935167013));
#79925=CARTESIAN_POINT('',(0.,-22.8288881795131,-29.7504935167013));
#79926=CARTESIAN_POINT('',(0.,-22.8288881795131,-29.7504935167013));
#79927=CARTESIAN_POINT('Origin',(0.,-27.6481850557002,-25.3343218406523));
#79928=CARTESIAN_POINT('',(22.,-27.6481850557002,-25.3343218406523));
#79929=CARTESIAN_POINT('',(22.,-27.6481850557002,-25.3343218406523));
#79930=CARTESIAN_POINT('',(0.,-27.6481850557002,-25.3343218406523));
#79931=CARTESIAN_POINT('',(11.,-27.8498454727622,-25.5582884235871));
#79932=CARTESIAN_POINT('',(0.,-27.6481850557002,-25.3343218406523));
#79933=CARTESIAN_POINT('',(0.,-27.6481850557002,-25.3343218406523));
#79934=CARTESIAN_POINT('',(0.,-27.6481850557002,-25.3343218406523));
#79935=CARTESIAN_POINT('Origin',(0.,-31.6274058196267,-20.1483796152605));
#79936=CARTESIAN_POINT('',(22.,-31.6274058196267,-20.1483796152605));
#79937=CARTESIAN_POINT('',(22.,-31.6274058196267,-20.1483796152605));
#79938=CARTESIAN_POINT('',(0.,-31.6274058196267,-20.1483796152605));
#79939=CARTESIAN_POINT('',(11.,-31.8648939508099,-20.3339256786199));
#79940=CARTESIAN_POINT('',(0.,-31.6274058196267,-20.1483796152605));
#79941=CARTESIAN_POINT('',(0.,-31.6274058196267,-20.1483796152605));
#79942=CARTESIAN_POINT('',(0.,-31.6274058196267,-20.1483796152605));
#79943=CARTESIAN_POINT('Origin',(0.,-34.6456438619633,-14.3502390708311));
#79944=CARTESIAN_POINT('',(22.,-34.6456438619633,-14.3502390708311));
#79945=CARTESIAN_POINT('',(22.,-34.6456438619633,-14.3502390708311));
#79946=CARTESIAN_POINT('',(0.,-34.6456438619633,-14.3502390708311));
#79947=CARTESIAN_POINT('',(11.,-34.9117437505765,-14.4917268913708));
#79948=CARTESIAN_POINT('',(0.,-34.6456438619633,-14.3502390708311));
#79949=CARTESIAN_POINT('',(0.,-34.6456438619633,-14.3502390708311));
#79950=CARTESIAN_POINT('',(0.,-34.6456438619633,-14.3502390708311));
#79951=CARTESIAN_POINT('Origin',(0.,-36.6111915470959,-8.11607377380573));
#79952=CARTESIAN_POINT('',(22.,-36.6111915470959,-8.11607377380573));
#79953=CARTESIAN_POINT('',(22.,-36.6111915470959,-8.11607377380573));
#79954=CARTESIAN_POINT('',(0.,-36.6111915470959,-8.11607377380573));
#79955=CARTESIAN_POINT('',(11.,-36.8978178826767,-8.209204315695));
#79956=CARTESIAN_POINT('',(0.,-36.6111915470959,-8.11607377380573));
#79957=CARTESIAN_POINT('',(0.,-36.6111915470959,-8.11607377380573));
#79958=CARTESIAN_POINT('',(0.,-36.6111915470959,-8.11607377380573));
#79959=CARTESIAN_POINT('Origin',(0.,-37.4643267032267,-1.63530568209482));
#79960=CARTESIAN_POINT('',(22.,-37.4643267032267,-1.63530568209482));
#79961=CARTESIAN_POINT('',(22.,-37.4643267032267,-1.63530568209482));
#79962=CARTESIAN_POINT('',(0.,-37.4643267032267,-1.63530568209482));
#79963=CARTESIAN_POINT('',(11.,-37.7627704896084,-1.67724922094464));
#79964=CARTESIAN_POINT('',(0.,-37.4643267032267,-1.63530568209482));
#79965=CARTESIAN_POINT('',(0.,-37.4643267032267,-1.63530568209482));
#79966=CARTESIAN_POINT('',(0.,-37.4643267032267,-1.63530568209482));
#79967=CARTESIAN_POINT('Origin',(0.,-37.1791272503441,4.89515034526196));
#79968=CARTESIAN_POINT('',(22.,-37.1791272503441,4.89515034526196));
#79969=CARTESIAN_POINT('',(22.,-37.1791272503441,4.89515034526196));
#79970=CARTESIAN_POINT('',(0.,-37.1791272503441,4.89515034526196));
#79971=CARTESIAN_POINT('',(11.,-37.4803204240973,4.90566824265508));
#79972=CARTESIAN_POINT('',(0.,-37.1791272503441,4.89515034526196));
#79973=CARTESIAN_POINT('',(0.,-37.1791272503441,4.89515034526196));
#79974=CARTESIAN_POINT('',(0.,-37.1791272503441,4.89515034526196));
#79975=CARTESIAN_POINT('Origin',(0.,-35.764258829506,11.2768697064435));
#79976=CARTESIAN_POINT('',(22.,-35.764258829506,11.2768697064435));
#79977=CARTESIAN_POINT('',(22.,-35.764258829506,11.2768697064435));
#79978=CARTESIAN_POINT('',(0.,-35.764258829506,11.2768697064435));
#79979=CARTESIAN_POINT('',(11.,-36.0590497884572,11.3395294590896));
#79980=CARTESIAN_POINT('',(0.,-35.764258829506,11.2768697064435));
#79981=CARTESIAN_POINT('',(0.,-35.764258829506,11.2768697064435));
#79982=CARTESIAN_POINT('',(0.,-35.764258829506,11.2768697064435));
#79983=CARTESIAN_POINT('Origin',(0.,-33.2627115017215,17.3159470879662));
#79984=CARTESIAN_POINT('',(22.,-33.2627115017215,17.3159470879662));
#79985=CARTESIAN_POINT('',(22.,-33.2627115017215,17.3159470879662));
#79986=CARTESIAN_POINT('',(0.,-33.2627115017215,17.3159470879662));
#79987=CARTESIAN_POINT('',(11.,-33.5421431717545,17.4288448109885));
#79988=CARTESIAN_POINT('',(0.,-33.2627115017215,17.3159470879662));
#79989=CARTESIAN_POINT('',(0.,-33.2627115017215,17.3159470879662));
#79990=CARTESIAN_POINT('',(0.,-33.2627115017215,17.3159470879662));
#79991=CARTESIAN_POINT('Origin',(0.,-29.7504935167013,22.8288881795131));
#79992=CARTESIAN_POINT('',(22.,-29.7504935167013,22.8288881795131));
#79993=CARTESIAN_POINT('',(22.,-29.7504935167013,22.8288881795131));
#79994=CARTESIAN_POINT('',(0.,-29.7504935167013,22.8288881795131));
#79995=CARTESIAN_POINT('',(11.,-30.0060755079215,22.9885935327265));
#79996=CARTESIAN_POINT('',(0.,-29.7504935167013,22.8288881795131));
#79997=CARTESIAN_POINT('',(0.,-29.7504935167013,22.8288881795131));
#79998=CARTESIAN_POINT('',(0.,-29.7504935167013,22.8288881795131));
#79999=CARTESIAN_POINT('Origin',(0.,-25.3343218406523,27.6481850557002));
#80000=CARTESIAN_POINT('',(22.,-25.3343218406523,27.6481850557002));
#80001=CARTESIAN_POINT('',(22.,-25.3343218406523,27.6481850557002));
#80002=CARTESIAN_POINT('',(0.,-25.3343218406523,27.6481850557002));
#80003=CARTESIAN_POINT('',(0.,-25.3343218406523,27.6481850557002));
#80004=CARTESIAN_POINT('',(0.,-25.3343218406523,27.6481850557002));
#80005=CARTESIAN_POINT('',(0.,-25.3343218406523,27.6481850557002));
#80006=CARTESIAN_POINT('Origin',(0.,-14.3502390708311,34.6456438619633));
#80007=CARTESIAN_POINT('',(22.,-14.3502390708311,34.6456438619633));
#80008=CARTESIAN_POINT('',(22.,-14.3502390708311,34.6456438619633));
#80009=CARTESIAN_POINT('',(0.,-14.3502390708311,34.6456438619633));
#80010=CARTESIAN_POINT('',(11.,-14.4917268913708,34.9117437505765));
#80011=CARTESIAN_POINT('',(0.,-14.3502390708311,34.6456438619633));
#80012=CARTESIAN_POINT('',(0.,-14.3502390708311,34.6456438619633));
#80013=CARTESIAN_POINT('',(0.,-14.3502390708311,34.6456438619633));
#80014=CARTESIAN_POINT('Origin',(0.,-8.11607377380574,36.6111915470959));
#80015=CARTESIAN_POINT('',(22.,-8.11607377380574,36.6111915470959));
#80016=CARTESIAN_POINT('',(22.,-8.11607377380574,36.6111915470959));
#80017=CARTESIAN_POINT('',(0.,-8.11607377380574,36.6111915470959));
#80018=CARTESIAN_POINT('',(11.,-8.20920431569501,36.8978178826767));
#80019=CARTESIAN_POINT('',(0.,-8.11607377380574,36.6111915470959));
#80020=CARTESIAN_POINT('',(0.,-8.11607377380574,36.6111915470959));
#80021=CARTESIAN_POINT('',(0.,-8.11607377380574,36.6111915470959));
#80022=CARTESIAN_POINT('Origin',(0.,-1.63530568209482,37.4643267032267));
#80023=CARTESIAN_POINT('',(22.,-1.63530568209482,37.4643267032267));
#80024=CARTESIAN_POINT('',(22.,-1.63530568209482,37.4643267032267));
#80025=CARTESIAN_POINT('',(0.,-1.63530568209482,37.4643267032267));
#80026=CARTESIAN_POINT('',(11.,-1.67724922094464,37.7627704896084));
#80027=CARTESIAN_POINT('',(0.,-1.63530568209482,37.4643267032267));
#80028=CARTESIAN_POINT('',(0.,-1.63530568209482,37.4643267032267));
#80029=CARTESIAN_POINT('',(0.,-1.63530568209482,37.4643267032267));
#80030=CARTESIAN_POINT('Origin',(0.,4.89515034526195,37.1791272503441));
#80031=CARTESIAN_POINT('',(22.,4.89515034526195,37.1791272503441));
#80032=CARTESIAN_POINT('',(22.,4.89515034526195,37.1791272503441));
#80033=CARTESIAN_POINT('',(0.,4.89515034526195,37.1791272503441));
#80034=CARTESIAN_POINT('',(11.,4.90566824265507,37.4803204240973));
#80035=CARTESIAN_POINT('',(0.,4.89515034526195,37.1791272503441));
#80036=CARTESIAN_POINT('',(0.,4.89515034526195,37.1791272503441));
#80037=CARTESIAN_POINT('',(0.,4.89515034526195,37.1791272503441));
#80038=CARTESIAN_POINT('Origin',(0.,11.2768697064435,35.764258829506));
#80039=CARTESIAN_POINT('',(22.,11.2768697064435,35.764258829506));
#80040=CARTESIAN_POINT('',(22.,11.2768697064435,35.764258829506));
#80041=CARTESIAN_POINT('',(0.,11.2768697064435,35.764258829506));
#80042=CARTESIAN_POINT('',(11.,11.3395294590896,36.0590497884572));
#80043=CARTESIAN_POINT('',(0.,11.2768697064435,35.764258829506));
#80044=CARTESIAN_POINT('',(0.,11.2768697064435,35.764258829506));
#80045=CARTESIAN_POINT('',(0.,11.2768697064435,35.764258829506));
#80046=CARTESIAN_POINT('Origin',(0.,17.3159470879662,33.2627115017215));
#80047=CARTESIAN_POINT('',(22.,17.3159470879662,33.2627115017215));
#80048=CARTESIAN_POINT('',(22.,17.3159470879662,33.2627115017215));
#80049=CARTESIAN_POINT('',(0.,17.3159470879662,33.2627115017215));
#80050=CARTESIAN_POINT('',(11.,17.4288448109885,33.5421431717545));
#80051=CARTESIAN_POINT('',(0.,17.3159470879662,33.2627115017215));
#80052=CARTESIAN_POINT('',(0.,17.3159470879662,33.2627115017215));
#80053=CARTESIAN_POINT('',(0.,17.3159470879662,33.2627115017215));
#80054=CARTESIAN_POINT('Origin',(0.,22.8288881795131,29.7504935167013));
#80055=CARTESIAN_POINT('',(22.,22.8288881795131,29.7504935167013));
#80056=CARTESIAN_POINT('',(22.,22.8288881795131,29.7504935167013));
#80057=CARTESIAN_POINT('',(0.,22.8288881795131,29.7504935167013));
#80058=CARTESIAN_POINT('',(11.,22.9885935327265,30.0060755079215));
#80059=CARTESIAN_POINT('',(0.,22.8288881795131,29.7504935167013));
#80060=CARTESIAN_POINT('',(0.,22.8288881795131,29.7504935167013));
#80061=CARTESIAN_POINT('',(0.,22.8288881795131,29.7504935167013));
#80062=CARTESIAN_POINT('Origin',(0.,27.6481850557002,25.3343218406523));
#80063=CARTESIAN_POINT('',(22.,27.6481850557002,25.3343218406523));
#80064=CARTESIAN_POINT('',(22.,27.6481850557002,25.3343218406523));
#80065=CARTESIAN_POINT('',(0.,27.6481850557002,25.3343218406523));
#80066=CARTESIAN_POINT('',(11.,27.8498454727622,25.5582884235871));
#80067=CARTESIAN_POINT('',(0.,27.6481850557002,25.3343218406523));
#80068=CARTESIAN_POINT('',(0.,27.6481850557002,25.3343218406523));
#80069=CARTESIAN_POINT('',(0.,27.6481850557002,25.3343218406523));
#80070=CARTESIAN_POINT('Origin',(0.,31.6274058196267,20.1483796152605));
#80071=CARTESIAN_POINT('',(22.,31.6274058196267,20.1483796152605));
#80072=CARTESIAN_POINT('',(22.,31.6274058196267,20.1483796152605));
#80073=CARTESIAN_POINT('',(0.,31.6274058196267,20.1483796152605));
#80074=CARTESIAN_POINT('',(11.,31.8648939508099,20.3339256786199));
#80075=CARTESIAN_POINT('',(0.,31.6274058196267,20.1483796152605));
#80076=CARTESIAN_POINT('',(0.,31.6274058196267,20.1483796152605));
#80077=CARTESIAN_POINT('',(0.,31.6274058196267,20.1483796152605));
#80078=CARTESIAN_POINT('Origin',(0.,34.6456438619633,14.3502390708311));
#80079=CARTESIAN_POINT('',(22.,34.6456438619633,14.3502390708311));
#80080=CARTESIAN_POINT('',(22.,34.6456438619633,14.3502390708311));
#80081=CARTESIAN_POINT('',(0.,34.6456438619633,14.3502390708311));
#80082=CARTESIAN_POINT('',(11.,34.9117437505765,14.4917268913708));
#80083=CARTESIAN_POINT('',(0.,34.6456438619633,14.3502390708311));
#80084=CARTESIAN_POINT('',(0.,34.6456438619633,14.3502390708311));
#80085=CARTESIAN_POINT('',(0.,34.6456438619633,14.3502390708311));
#80086=CARTESIAN_POINT('Origin',(0.,36.6111915470959,8.11607377380574));
#80087=CARTESIAN_POINT('',(22.,36.6111915470959,8.11607377380574));
#80088=CARTESIAN_POINT('',(22.,36.6111915470959,8.11607377380574));
#80089=CARTESIAN_POINT('',(0.,36.6111915470959,8.11607377380574));
#80090=CARTESIAN_POINT('',(0.,36.6111915470959,8.11607377380574));
#80091=CARTESIAN_POINT('',(0.,36.6111915470959,8.11607377380574));
#80092=CARTESIAN_POINT('',(0.,36.6111915470959,8.11607377380574));
#80093=CARTESIAN_POINT('Origin',(0.,37.4643267032267,-1.63530568209483));
#80094=CARTESIAN_POINT('',(0.,37.4643267032267,-1.63530568209483));
#80095=CARTESIAN_POINT('Origin',(0.,37.4643267032267,-1.63530568209483));
#80096=CARTESIAN_POINT('',(22.,37.4643267032267,-1.63530568209483));
#80097=CARTESIAN_POINT('Origin',(22.,39.5633512881141,-3.57953331806381));
#80098=CARTESIAN_POINT('Origin',(0.,39.5633512881141,-3.57953331806381));
#80099=CARTESIAN_POINT('Origin',(11.,0.,0.));
#80100=CARTESIAN_POINT('Origin',(11.,0.,0.));
#80101=CARTESIAN_POINT('Origin',(0.,36.6111915470958,-8.11607377380577));
#80102=CARTESIAN_POINT('',(0.,36.6111915470958,-8.11607377380577));
#80103=CARTESIAN_POINT('Origin',(0.,36.6111915470958,-8.11607377380577));
#80104=CARTESIAN_POINT('',(22.,36.6111915470958,-8.11607377380577));
#80105=CARTESIAN_POINT('Origin',(22.,38.3407156461005,-10.3952560173724));
#80106=CARTESIAN_POINT('Origin',(0.,38.3407156461005,-10.3952560173724));
#80107=CARTESIAN_POINT('Origin',(11.,0.,0.));
#80108=CARTESIAN_POINT('Origin',(0.,34.6456438619633,-14.3502390708311));
#80109=CARTESIAN_POINT('',(0.,34.6456438619633,-14.3502390708311));
#80110=CARTESIAN_POINT('Origin',(0.,34.6456438619633,-14.3502390708311));
#80111=CARTESIAN_POINT('',(22.,34.6456438619633,-14.3502390708311));
#80112=CARTESIAN_POINT('Origin',(22.,35.9531167605183,-16.8951241228465));
#80113=CARTESIAN_POINT('Origin',(0.,35.9531167605183,-16.8951241228465));
#80114=CARTESIAN_POINT('Origin',(11.,0.,0.));
#80115=CARTESIAN_POINT('Origin',(0.,31.6274058196267,-20.1483796152605));
#80116=CARTESIAN_POINT('',(0.,31.6274058196267,-20.1483796152605));
#80117=CARTESIAN_POINT('Origin',(0.,31.6274058196267,-20.1483796152605));
#80118=CARTESIAN_POINT('',(22.,31.6274058196267,-20.1483796152605));
#80119=CARTESIAN_POINT('Origin',(22.,32.4731006153227,-22.8816424311931));
#80120=CARTESIAN_POINT('Origin',(0.,32.4731006153227,-22.8816424311931));
#80121=CARTESIAN_POINT('Origin',(11.,0.,0.));
#80122=CARTESIAN_POINT('Origin',(0.,27.6481850557002,-25.3343218406523));
#80123=CARTESIAN_POINT('',(0.,27.6481850557002,-25.3343218406523));
#80124=CARTESIAN_POINT('Origin',(0.,27.6481850557002,-25.3343218406523));
#80125=CARTESIAN_POINT('',(22.,27.6481850557002,-25.3343218406523));
#80126=CARTESIAN_POINT('Origin',(22.,28.0064057401123,-28.1729136129378));
#80127=CARTESIAN_POINT('Origin',(0.,28.0064057401123,-28.1729136129378));
#80128=CARTESIAN_POINT('Origin',(11.,0.,0.));
#80129=CARTESIAN_POINT('Origin',(0.,22.8288881795131,-29.7504935167013));
#80130=CARTESIAN_POINT('',(0.,22.8288881795131,-29.7504935167013));
#80131=CARTESIAN_POINT('Origin',(0.,22.8288881795131,-29.7504935167013));
#80132=CARTESIAN_POINT('',(22.,22.8288881795131,-29.7504935167013));
#80133=CARTESIAN_POINT('Origin',(22.,22.6887503984137,-32.6081650707355));
#80134=CARTESIAN_POINT('Origin',(0.,22.6887503984137,-32.6081650707355));
#80135=CARTESIAN_POINT('Origin',(11.,0.,0.));
#80136=CARTESIAN_POINT('Origin',(0.,17.3159470879662,-33.2627115017215));
#80137=CARTESIAN_POINT('',(0.,17.3159470879662,-33.2627115017215));
#80138=CARTESIAN_POINT('Origin',(0.,17.3159470879662,-33.2627115017215));
#80139=CARTESIAN_POINT('',(22.,17.3159470879662,-33.2627115017215));
#80140=CARTESIAN_POINT('Origin',(22.,16.681708856921,-36.0526339333865));
#80141=CARTESIAN_POINT('Origin',(0.,16.681708856921,-36.0526339333865));
#80142=CARTESIAN_POINT('Origin',(11.,0.,0.));
#80143=CARTESIAN_POINT('Origin',(0.,11.2768697064435,-35.764258829506));
#80144=CARTESIAN_POINT('',(0.,11.2768697064435,-35.764258829506));
#80145=CARTESIAN_POINT('Origin',(0.,11.2768697064435,-35.764258829506));
#80146=CARTESIAN_POINT('',(22.,11.2768697064435,-35.764258829506));
#80147=CARTESIAN_POINT('Origin',(22.,10.1678020331627,-38.4016617574847));
#80148=CARTESIAN_POINT('Origin',(0.,10.1678020331627,-38.4016617574847));
#80149=CARTESIAN_POINT('Origin',(11.,0.,0.));
#80150=CARTESIAN_POINT('Origin',(0.,4.89515034526193,-37.1791272503441));
#80151=CARTESIAN_POINT('',(0.,4.89515034526193,-37.1791272503441));
#80152=CARTESIAN_POINT('Origin',(0.,4.89515034526193,-37.1791272503441));
#80153=CARTESIAN_POINT('',(22.,4.89515034526193,-37.1791272503441));
#80154=CARTESIAN_POINT('Origin',(22.,3.34495168978286,-39.5838745212602));
#80155=CARTESIAN_POINT('Origin',(0.,3.34495168978286,-39.5838745212602));
#80156=CARTESIAN_POINT('Origin',(11.,0.,0.));
#80157=CARTESIAN_POINT('Origin',(0.,-1.63530568209482,-37.4643267032267));
#80158=CARTESIAN_POINT('',(0.,-1.63530568209482,-37.4643267032267));
#80159=CARTESIAN_POINT('Origin',(0.,-1.63530568209482,-37.4643267032267));
#80160=CARTESIAN_POINT('',(22.,-1.63530568209482,-37.4643267032267));
#80161=CARTESIAN_POINT('Origin',(22.,-3.57953331806381,-39.5633512881141));
#80162=CARTESIAN_POINT('Origin',(0.,-3.57953331806381,-39.5633512881141));
#80163=CARTESIAN_POINT('Origin',(11.,0.,0.));
#80164=CARTESIAN_POINT('Origin',(0.,-8.11607377380577,-36.6111915470959));
#80165=CARTESIAN_POINT('',(0.,-8.11607377380577,-36.6111915470959));
#80166=CARTESIAN_POINT('Origin',(0.,-8.11607377380577,-36.6111915470959));
#80167=CARTESIAN_POINT('',(22.,-8.11607377380577,-36.6111915470959));
#80168=CARTESIAN_POINT('Origin',(22.,-10.3952560173724,-38.3407156461005));
#80169=CARTESIAN_POINT('Origin',(0.,-10.3952560173724,-38.3407156461005));
#80170=CARTESIAN_POINT('Origin',(11.,0.,0.));
#80171=CARTESIAN_POINT('Origin',(0.,-20.1483796152605,-31.6274058196267));
#80172=CARTESIAN_POINT('',(0.,-20.1483796152605,-31.6274058196267));
#80173=CARTESIAN_POINT('Origin',(0.,-20.1483796152605,-31.6274058196267));
#80174=CARTESIAN_POINT('',(22.,-20.1483796152605,-31.6274058196267));
#80175=CARTESIAN_POINT('Origin',(22.,-22.8816424311931,-32.4731006153227));
#80176=CARTESIAN_POINT('Origin',(0.,-22.8816424311931,-32.4731006153227));
#80177=CARTESIAN_POINT('Origin',(11.,0.,0.));
#80178=CARTESIAN_POINT('Origin',(0.,-25.3343218406523,-27.6481850557002));
#80179=CARTESIAN_POINT('',(0.,-25.3343218406523,-27.6481850557002));
#80180=CARTESIAN_POINT('Origin',(0.,-25.3343218406523,-27.6481850557002));
#80181=CARTESIAN_POINT('',(22.,-25.3343218406523,-27.6481850557002));
#80182=CARTESIAN_POINT('Origin',(22.,-28.1729136129378,-28.0064057401123));
#80183=CARTESIAN_POINT('Origin',(0.,-28.1729136129378,-28.0064057401123));
#80184=CARTESIAN_POINT('Origin',(11.,0.,0.));
#80185=CARTESIAN_POINT('Origin',(0.,-29.7504935167013,-22.8288881795131));
#80186=CARTESIAN_POINT('',(0.,-29.7504935167013,-22.8288881795131));
#80187=CARTESIAN_POINT('Origin',(0.,-29.7504935167013,-22.8288881795131));
#80188=CARTESIAN_POINT('',(22.,-29.7504935167013,-22.8288881795131));
#80189=CARTESIAN_POINT('Origin',(22.,-32.6081650707355,-22.6887503984137));
#80190=CARTESIAN_POINT('Origin',(0.,-32.6081650707355,-22.6887503984137));
#80191=CARTESIAN_POINT('Origin',(11.,0.,0.));
#80192=CARTESIAN_POINT('Origin',(0.,-33.2627115017215,-17.3159470879662));
#80193=CARTESIAN_POINT('',(0.,-33.2627115017215,-17.3159470879662));
#80194=CARTESIAN_POINT('Origin',(0.,-33.2627115017215,-17.3159470879662));
#80195=CARTESIAN_POINT('',(22.,-33.2627115017215,-17.3159470879662));
#80196=CARTESIAN_POINT('Origin',(22.,-36.0526339333865,-16.681708856921));
#80197=CARTESIAN_POINT('Origin',(0.,-36.0526339333865,-16.681708856921));
#80198=CARTESIAN_POINT('Origin',(11.,0.,0.));
#80199=CARTESIAN_POINT('Origin',(0.,-35.764258829506,-11.2768697064435));
#80200=CARTESIAN_POINT('',(0.,-35.764258829506,-11.2768697064435));
#80201=CARTESIAN_POINT('Origin',(0.,-35.764258829506,-11.2768697064435));
#80202=CARTESIAN_POINT('',(22.,-35.764258829506,-11.2768697064435));
#80203=CARTESIAN_POINT('Origin',(22.,-38.4016617574847,-10.1678020331627));
#80204=CARTESIAN_POINT('Origin',(0.,-38.4016617574847,-10.1678020331627));
#80205=CARTESIAN_POINT('Origin',(11.,0.,0.));
#80206=CARTESIAN_POINT('Origin',(0.,-37.1791272503441,-4.89515034526194));
#80207=CARTESIAN_POINT('',(0.,-37.1791272503441,-4.89515034526194));
#80208=CARTESIAN_POINT('Origin',(0.,-37.1791272503441,-4.89515034526194));
#80209=CARTESIAN_POINT('',(22.,-37.1791272503441,-4.89515034526194));
#80210=CARTESIAN_POINT('Origin',(22.,-39.5838745212602,-3.34495168978286));
#80211=CARTESIAN_POINT('Origin',(0.,-39.5838745212602,-3.34495168978286));
#80212=CARTESIAN_POINT('Origin',(11.,0.,0.));
#80213=CARTESIAN_POINT('Origin',(0.,-37.4643267032267,1.63530568209484));
#80214=CARTESIAN_POINT('',(0.,-37.4643267032267,1.63530568209484));
#80215=CARTESIAN_POINT('Origin',(0.,-37.4643267032267,1.63530568209484));
#80216=CARTESIAN_POINT('',(22.,-37.4643267032267,1.63530568209484));
#80217=CARTESIAN_POINT('Origin',(22.,-39.5633512881141,3.57953331806382));
#80218=CARTESIAN_POINT('Origin',(0.,-39.5633512881141,3.57953331806382));
#80219=CARTESIAN_POINT('Origin',(11.,0.,0.));
#80220=CARTESIAN_POINT('Origin',(0.,-36.6111915470959,8.11607377380575));
#80221=CARTESIAN_POINT('',(0.,-36.6111915470959,8.11607377380575));
#80222=CARTESIAN_POINT('Origin',(0.,-36.6111915470959,8.11607377380575));
#80223=CARTESIAN_POINT('',(22.,-36.6111915470959,8.11607377380575));
#80224=CARTESIAN_POINT('Origin',(22.,-38.3407156461005,10.3952560173724));
#80225=CARTESIAN_POINT('Origin',(0.,-38.3407156461005,10.3952560173724));
#80226=CARTESIAN_POINT('Origin',(11.,0.,0.));
#80227=CARTESIAN_POINT('Origin',(0.,-34.6456438619633,14.3502390708311));
#80228=CARTESIAN_POINT('',(0.,-34.6456438619633,14.3502390708311));
#80229=CARTESIAN_POINT('Origin',(0.,-34.6456438619633,14.3502390708311));
#80230=CARTESIAN_POINT('',(22.,-34.6456438619633,14.3502390708311));
#80231=CARTESIAN_POINT('Origin',(22.,-35.9531167605183,16.8951241228464));
#80232=CARTESIAN_POINT('Origin',(0.,-35.9531167605183,16.8951241228464));
#80233=CARTESIAN_POINT('Origin',(11.,0.,0.));
#80234=CARTESIAN_POINT('Origin',(0.,-31.6274058196267,20.1483796152605));
#80235=CARTESIAN_POINT('',(0.,-31.6274058196267,20.1483796152605));
#80236=CARTESIAN_POINT('Origin',(0.,-31.6274058196267,20.1483796152605));
#80237=CARTESIAN_POINT('',(22.,-31.6274058196267,20.1483796152605));
#80238=CARTESIAN_POINT('Origin',(22.,-32.4731006153227,22.8816424311931));
#80239=CARTESIAN_POINT('Origin',(0.,-32.4731006153227,22.8816424311931));
#80240=CARTESIAN_POINT('Origin',(11.,0.,0.));
#80241=CARTESIAN_POINT('Origin',(0.,-27.6481850557002,25.3343218406523));
#80242=CARTESIAN_POINT('',(0.,-27.6481850557002,25.3343218406523));
#80243=CARTESIAN_POINT('Origin',(0.,-27.6481850557002,25.3343218406523));
#80244=CARTESIAN_POINT('',(22.,-27.6481850557002,25.3343218406523));
#80245=CARTESIAN_POINT('Origin',(22.,-28.0064057401123,28.1729136129378));
#80246=CARTESIAN_POINT('Origin',(0.,-28.0064057401123,28.1729136129378));
#80247=CARTESIAN_POINT('Origin',(11.,0.,0.));
#80248=CARTESIAN_POINT('Origin',(0.,-17.3159470879662,33.2627115017215));
#80249=CARTESIAN_POINT('',(0.,-17.3159470879662,33.2627115017215));
#80250=CARTESIAN_POINT('Origin',(0.,-17.3159470879662,33.2627115017215));
#80251=CARTESIAN_POINT('',(22.,-17.3159470879662,33.2627115017215));
#80252=CARTESIAN_POINT('Origin',(22.,-16.681708856921,36.0526339333865));
#80253=CARTESIAN_POINT('Origin',(0.,-16.681708856921,36.0526339333865));
#80254=CARTESIAN_POINT('Origin',(11.,0.,0.));
#80255=CARTESIAN_POINT('Origin',(0.,-11.2768697064435,35.764258829506));
#80256=CARTESIAN_POINT('',(0.,-11.2768697064435,35.764258829506));
#80257=CARTESIAN_POINT('Origin',(0.,-11.2768697064435,35.764258829506));
#80258=CARTESIAN_POINT('',(22.,-11.2768697064435,35.764258829506));
#80259=CARTESIAN_POINT('Origin',(22.,-10.1678020331627,38.4016617574847));
#80260=CARTESIAN_POINT('Origin',(0.,-10.1678020331627,38.4016617574847));
#80261=CARTESIAN_POINT('Origin',(11.,0.,0.));
#80262=CARTESIAN_POINT('Origin',(0.,-4.89515034526194,37.1791272503441));
#80263=CARTESIAN_POINT('',(0.,-4.89515034526194,37.1791272503441));
#80264=CARTESIAN_POINT('Origin',(0.,-4.89515034526194,37.1791272503441));
#80265=CARTESIAN_POINT('',(22.,-4.89515034526194,37.1791272503441));
#80266=CARTESIAN_POINT('Origin',(22.,-3.34495168978286,39.5838745212602));
#80267=CARTESIAN_POINT('Origin',(0.,-3.34495168978286,39.5838745212602));
#80268=CARTESIAN_POINT('Origin',(11.,0.,0.));
#80269=CARTESIAN_POINT('Origin',(0.,1.63530568209483,37.4643267032268));
#80270=CARTESIAN_POINT('',(0.,1.63530568209483,37.4643267032268));
#80271=CARTESIAN_POINT('Origin',(0.,1.63530568209483,37.4643267032268));
#80272=CARTESIAN_POINT('',(22.,1.63530568209483,37.4643267032268));
#80273=CARTESIAN_POINT('Origin',(22.,3.57953331806381,39.5633512881141));
#80274=CARTESIAN_POINT('Origin',(0.,3.57953331806381,39.5633512881141));
#80275=CARTESIAN_POINT('Origin',(11.,0.,0.));
#80276=CARTESIAN_POINT('Origin',(0.,8.11607377380574,36.6111915470959));
#80277=CARTESIAN_POINT('',(0.,8.11607377380574,36.6111915470959));
#80278=CARTESIAN_POINT('Origin',(0.,8.11607377380574,36.6111915470959));
#80279=CARTESIAN_POINT('',(22.,8.11607377380574,36.6111915470959));
#80280=CARTESIAN_POINT('Origin',(22.,10.3952560173724,38.3407156461005));
#80281=CARTESIAN_POINT('Origin',(0.,10.3952560173724,38.3407156461005));
#80282=CARTESIAN_POINT('Origin',(11.,0.,0.));
#80283=CARTESIAN_POINT('Origin',(0.,14.3502390708311,34.6456438619633));
#80284=CARTESIAN_POINT('',(0.,14.3502390708311,34.6456438619633));
#80285=CARTESIAN_POINT('Origin',(0.,14.3502390708311,34.6456438619633));
#80286=CARTESIAN_POINT('',(22.,14.3502390708311,34.6456438619633));
#80287=CARTESIAN_POINT('Origin',(22.,16.8951241228464,35.9531167605183));
#80288=CARTESIAN_POINT('Origin',(0.,16.8951241228464,35.9531167605183));
#80289=CARTESIAN_POINT('Origin',(11.,0.,0.));
#80290=CARTESIAN_POINT('Origin',(0.,20.1483796152605,31.6274058196267));
#80291=CARTESIAN_POINT('',(0.,20.1483796152605,31.6274058196267));
#80292=CARTESIAN_POINT('Origin',(0.,20.1483796152605,31.6274058196267));
#80293=CARTESIAN_POINT('',(22.,20.1483796152605,31.6274058196267));
#80294=CARTESIAN_POINT('Origin',(22.,22.8816424311931,32.4731006153227));
#80295=CARTESIAN_POINT('Origin',(0.,22.8816424311931,32.4731006153227));
#80296=CARTESIAN_POINT('Origin',(11.,0.,0.));
#80297=CARTESIAN_POINT('Origin',(0.,25.3343218406523,27.6481850557002));
#80298=CARTESIAN_POINT('',(0.,25.3343218406523,27.6481850557002));
#80299=CARTESIAN_POINT('Origin',(0.,25.3343218406523,27.6481850557002));
#80300=CARTESIAN_POINT('',(22.,25.3343218406523,27.6481850557002));
#80301=CARTESIAN_POINT('Origin',(22.,28.1729136129378,28.0064057401123));
#80302=CARTESIAN_POINT('Origin',(0.,28.1729136129378,28.0064057401123));
#80303=CARTESIAN_POINT('Origin',(11.,0.,0.));
#80304=CARTESIAN_POINT('Origin',(0.,29.7504935167013,22.8288881795131));
#80305=CARTESIAN_POINT('',(0.,29.7504935167013,22.8288881795131));
#80306=CARTESIAN_POINT('Origin',(0.,29.7504935167013,22.8288881795131));
#80307=CARTESIAN_POINT('',(22.,29.7504935167013,22.8288881795131));
#80308=CARTESIAN_POINT('Origin',(22.,32.6081650707355,22.6887503984137));
#80309=CARTESIAN_POINT('Origin',(0.,32.6081650707355,22.6887503984137));
#80310=CARTESIAN_POINT('Origin',(11.,0.,0.));
#80311=CARTESIAN_POINT('Origin',(0.,33.2627115017215,17.3159470879662));
#80312=CARTESIAN_POINT('',(0.,33.2627115017215,17.3159470879662));
#80313=CARTESIAN_POINT('Origin',(0.,33.2627115017215,17.3159470879662));
#80314=CARTESIAN_POINT('',(22.,33.2627115017215,17.3159470879662));
#80315=CARTESIAN_POINT('Origin',(22.,36.0526339333865,16.681708856921));
#80316=CARTESIAN_POINT('Origin',(0.,36.0526339333865,16.681708856921));
#80317=CARTESIAN_POINT('Origin',(11.,0.,0.));
#80318=CARTESIAN_POINT('Origin',(0.,35.764258829506,11.2768697064435));
#80319=CARTESIAN_POINT('',(0.,35.764258829506,11.2768697064435));
#80320=CARTESIAN_POINT('Origin',(0.,35.764258829506,11.2768697064435));
#80321=CARTESIAN_POINT('',(22.,35.764258829506,11.2768697064435));
#80322=CARTESIAN_POINT('Origin',(22.,38.4016617574847,10.1678020331627));
#80323=CARTESIAN_POINT('Origin',(0.,38.4016617574847,10.1678020331627));
#80324=CARTESIAN_POINT('Origin',(19.,0.,0.));
#80325=CARTESIAN_POINT('',(19.,-34.,-4.163799117101E-15));
#80326=CARTESIAN_POINT('',(19.,-4.163799117101E-15,34.));
#80327=CARTESIAN_POINT('Origin',(19.,0.,0.));
#80328=CARTESIAN_POINT('',(18.,-4.04133443718627E-15,33.));
#80329=CARTESIAN_POINT('Origin',(19.,-4.04133443718627E-15,33.));
#80330=CARTESIAN_POINT('Origin',(18.,0.,0.));
#80331=CARTESIAN_POINT('Origin',(19.,0.,0.));
#80332=CARTESIAN_POINT('Origin',(18.,24.,0.));
#80333=CARTESIAN_POINT('',(18.,-3.06161699786838E-15,25.));
#80334=CARTESIAN_POINT('Origin',(18.,0.,0.));
#80335=CARTESIAN_POINT('Origin',(20.,0.,0.));
#80336=CARTESIAN_POINT('',(22.,-34.,-4.163799117101E-15));
#80337=CARTESIAN_POINT('Origin',(22.,0.,0.));
#80338=CARTESIAN_POINT('',(20.,-34.,-4.163799117101E-15));
#80339=CARTESIAN_POINT('Origin',(3.,0.,0.));
#80340=CARTESIAN_POINT('',(4.,-4.04133443718627E-15,33.));
#80341=CARTESIAN_POINT('Origin',(4.,0.,0.));
#80342=CARTESIAN_POINT('',(3.,-4.163799117101E-15,34.));
#80343=CARTESIAN_POINT('Origin',(3.,-4.04133443718627E-15,33.));
#80344=CARTESIAN_POINT('',(3.,-34.,-4.163799117101E-15));
#80345=CARTESIAN_POINT('Origin',(3.,0.,0.));
#80346=CARTESIAN_POINT('Origin',(3.,0.,0.));
#80347=CARTESIAN_POINT('Origin',(4.,34.,0.));
#80348=CARTESIAN_POINT('',(4.,-3.06161699786838E-15,25.));
#80349=CARTESIAN_POINT('Origin',(4.,0.,0.));
#80350=CARTESIAN_POINT('Origin',(2.,0.,0.));
#80351=CARTESIAN_POINT('',(2.,-34.,-4.163799117101E-15));
#80352=CARTESIAN_POINT('Origin',(19.,0.,0.));
#80353=CARTESIAN_POINT('',(19.,-2.93915231795365E-15,24.));
#80354=CARTESIAN_POINT('Origin',(19.,-3.06161699786838E-15,25.));
#80355=CARTESIAN_POINT('',(19.,-24.,-2.93915231795365E-15));
#80356=CARTESIAN_POINT('Origin',(19.,0.,0.));
#80357=CARTESIAN_POINT('Origin',(19.,0.,0.));
#80358=CARTESIAN_POINT('Origin',(20.,0.,0.));
#80359=CARTESIAN_POINT('',(22.,-24.,-2.93915231795365E-15));
#80360=CARTESIAN_POINT('Origin',(22.,0.,0.));
#80361=CARTESIAN_POINT('',(20.,-24.,-2.93915231795365E-15));
#80362=CARTESIAN_POINT('Origin',(3.,0.,0.));
#80363=CARTESIAN_POINT('',(3.,-24.,-2.93915231795365E-15));
#80364=CARTESIAN_POINT('',(3.,-2.93915231795365E-15,24.));
#80365=CARTESIAN_POINT('Origin',(3.,0.,0.));
#80366=CARTESIAN_POINT('Origin',(3.,-3.06161699786838E-15,25.));
#80367=CARTESIAN_POINT('Origin',(3.,0.,0.));
#80368=CARTESIAN_POINT('Origin',(2.,0.,0.));
#80369=CARTESIAN_POINT('',(0.,-24.,-2.93915231795365E-15));
#80370=CARTESIAN_POINT('',(2.,-24.,-2.93915231795365E-15));
#80371=CARTESIAN_POINT('Origin',(0.,0.,0.));
#80372=CARTESIAN_POINT('Origin',(11.,0.,0.));
#80373=CARTESIAN_POINT('',(21.2,-15.01,-1.83819484552018E-15));
#80374=CARTESIAN_POINT('Origin',(21.2,0.,0.));
#80375=CARTESIAN_POINT('',(0.800000000000001,-15.01,-1.83819484552018E-15));
#80376=CARTESIAN_POINT('',(11.,-15.01,-1.83819484552018E-15));
#80377=CARTESIAN_POINT('Origin',(0.800000000000001,0.,0.));
#80378=CARTESIAN_POINT('Origin',(0.4,0.,0.));
#80379=CARTESIAN_POINT('',(-4.85722573273506E-16,-15.81,-1.93616658945197E-15));
#80380=CARTESIAN_POINT('',(0.4,-15.41,-1.88718071748607E-15));
#80381=CARTESIAN_POINT('Origin',(0.,0.,0.));
#80382=CARTESIAN_POINT('Origin',(0.,24.,0.));
#80383=CARTESIAN_POINT('Origin',(22.,34.,0.));
#80384=CARTESIAN_POINT('Origin',(22.,15.81,0.));
#80385=CARTESIAN_POINT('',(22.,-15.81,-1.93616658945197E-15));
#80386=CARTESIAN_POINT('Origin',(22.,0.,0.));
#80387=CARTESIAN_POINT('Origin',(21.6,0.,0.));
#80388=CARTESIAN_POINT('',(21.6,-15.41,-1.88718071748607E-15));
#80389=CARTESIAN_POINT('',(0.,0.,0.));
#80390=CARTESIAN_POINT('Origin',(11.85,-24.7487373415292,-24.7487373415292));
#80391=CARTESIAN_POINT('',(12.,-24.7487373415292,-21.4487373415292));
#80392=CARTESIAN_POINT('Origin',(12.,-24.7487373415292,-24.7487373415292));
#80393=CARTESIAN_POINT('',(11.7,-24.7487373415292,-21.7487373415292));
#80394=CARTESIAN_POINT('',(11.85,-24.7487373415292,-21.5987373415292));
#80395=CARTESIAN_POINT('Origin',(11.7,-24.7487373415292,-24.7487373415292));
#80396=CARTESIAN_POINT('Origin',(12.,20.,0.));
#80397=CARTESIAN_POINT('',(12.,-47.,-5.75583995599256E-15));
#80398=CARTESIAN_POINT('Origin',(12.,0.,0.));
#80399=CARTESIAN_POINT('',(12.,24.7487373415292,28.0487373415292));
#80400=CARTESIAN_POINT('Origin',(12.,24.7487373415292,24.7487373415292));
#80401=CARTESIAN_POINT('',(12.,-35.,5.50000000000001));
#80402=CARTESIAN_POINT('Origin',(12.,-35.,4.28626379701574E-15));
#80403=CARTESIAN_POINT('',(12.,2.81668763803891E-15,40.5));
#80404=CARTESIAN_POINT('Origin',(12.,2.14313189850787E-15,35.));
#80405=CARTESIAN_POINT('',(12.,35.,5.5));
#80406=CARTESIAN_POINT('Origin',(12.,35.,0.));
#80407=CARTESIAN_POINT('',(12.,-5.75583995599256E-15,-29.5));
#80408=CARTESIAN_POINT('Origin',(12.,-6.4293956955236E-15,-35.));
#80409=CARTESIAN_POINT('',(12.,-2.63299061816681E-15,21.5));
#80410=CARTESIAN_POINT('Origin',(12.,0.,0.));
#80411=CARTESIAN_POINT('Origin',(-0.5,-24.7487373415292,-24.7487373415292));
#80412=CARTESIAN_POINT('',(0.,-24.7487373415292,-21.7487373415292));
#80413=CARTESIAN_POINT('Origin',(0.,-24.7487373415292,-24.7487373415292));
#80414=CARTESIAN_POINT('',(-0.5,-24.7487373415292,-21.7487373415292));
#80415=CARTESIAN_POINT('Origin',(11.85,24.7487373415292,24.7487373415292));
#80416=CARTESIAN_POINT('',(11.7,24.7487373415292,27.7487373415292));
#80417=CARTESIAN_POINT('',(11.85,24.7487373415292,27.8987373415292));
#80418=CARTESIAN_POINT('Origin',(11.7,24.7487373415292,24.7487373415292));
#80419=CARTESIAN_POINT('Origin',(-0.5,24.7487373415292,24.7487373415292));
#80420=CARTESIAN_POINT('',(0.,24.7487373415292,27.7487373415292));
#80421=CARTESIAN_POINT('Origin',(0.,24.7487373415292,24.7487373415292));
#80422=CARTESIAN_POINT('',(-0.5,24.7487373415292,27.7487373415292));
#80423=CARTESIAN_POINT('Origin',(-0.5,35.,0.));
#80424=CARTESIAN_POINT('',(0.,35.,3.3));
#80425=CARTESIAN_POINT('Origin',(0.,35.,0.));
#80426=CARTESIAN_POINT('',(5.5,35.,3.3));
#80427=CARTESIAN_POINT('',(-0.5,35.,3.3));
#80428=CARTESIAN_POINT('Origin',(5.5,35.,0.));
#80429=CARTESIAN_POINT('Origin',(-0.5,2.14313189850787E-15,35.));
#80430=CARTESIAN_POINT('',(0.,1.73899845478924E-15,38.3));
#80431=CARTESIAN_POINT('Origin',(0.,2.14313189850787E-15,35.));
#80432=CARTESIAN_POINT('',(5.5,2.54726534222649E-15,38.3));
#80433=CARTESIAN_POINT('',(-0.5,1.73899845478924E-15,38.3));
#80434=CARTESIAN_POINT('Origin',(5.5,2.14313189850787E-15,35.));
#80435=CARTESIAN_POINT('Origin',(-0.5,-35.,4.28626379701574E-15));
#80436=CARTESIAN_POINT('',(0.,-35.,3.3));
#80437=CARTESIAN_POINT('Origin',(0.,-35.,4.28626379701574E-15));
#80438=CARTESIAN_POINT('',(5.5,-35.,3.3));
#80439=CARTESIAN_POINT('',(-0.5,-35.,3.3));
#80440=CARTESIAN_POINT('Origin',(5.5,-35.,4.28626379701574E-15));
#80441=CARTESIAN_POINT('Origin',(-0.5,-6.4293956955236E-15,-35.));
#80442=CARTESIAN_POINT('',(0.,-6.83352913924223E-15,-31.7));
#80443=CARTESIAN_POINT('Origin',(0.,-6.4293956955236E-15,-35.));
#80444=CARTESIAN_POINT('',(5.5,-6.02526225180498E-15,-31.7));
#80445=CARTESIAN_POINT('',(-0.5,-6.83352913924223E-15,-31.7));
#80446=CARTESIAN_POINT('Origin',(5.5,-6.4293956955236E-15,-35.));
#80447=CARTESIAN_POINT('Origin',(5.5,-35.,4.28626379701574E-15));
#80448=CARTESIAN_POINT('',(5.5,-35.,5.50000000000001));
#80449=CARTESIAN_POINT('Origin',(5.5,-35.,4.28626379701574E-15));
#80450=CARTESIAN_POINT('',(5.5,-35.,5.50000000000001));
#80451=CARTESIAN_POINT('Origin',(5.5,-35.,4.44089209850063E-15));
#80452=CARTESIAN_POINT('Origin',(5.5,2.14313189850787E-15,35.));
#80453=CARTESIAN_POINT('',(5.5,1.46957615897682E-15,40.5));
#80454=CARTESIAN_POINT('Origin',(5.5,2.14313189850787E-15,35.));
#80455=CARTESIAN_POINT('',(5.5,1.46957615897682E-15,40.5));
#80456=CARTESIAN_POINT('Origin',(5.5,2.22044604925031E-15,35.));
#80457=CARTESIAN_POINT('Origin',(5.5,35.,0.));
#80458=CARTESIAN_POINT('',(5.5,35.,5.5));
#80459=CARTESIAN_POINT('Origin',(5.5,35.,0.));
#80460=CARTESIAN_POINT('',(5.5,35.,5.5));
#80461=CARTESIAN_POINT('Origin',(5.5,35.,0.));
#80462=CARTESIAN_POINT('Origin',(5.5,-6.4293956955236E-15,-35.));
#80463=CARTESIAN_POINT('',(5.5,-7.10295143505465E-15,-29.5));
#80464=CARTESIAN_POINT('Origin',(5.5,-6.4293956955236E-15,-35.));
#80465=CARTESIAN_POINT('',(5.5,-7.10295143505465E-15,-29.5));
#80466=CARTESIAN_POINT('Origin',(5.5,-6.66133814775094E-15,-35.));
#80467=CARTESIAN_POINT('Origin',(18.4828269369554,0.,0.));
#80468=CARTESIAN_POINT('',(16.9656538739108,0.,0.));
#80469=CARTESIAN_POINT('',(20.,-5.05,-6.18446633569413E-16));
#80470=CARTESIAN_POINT('',(18.4828269369554,-2.525,-3.09223316784707E-16));
#80471=CARTESIAN_POINT('Origin',(20.,0.,0.));
#80472=CARTESIAN_POINT('Origin',(29.75,0.,0.));
#80473=CARTESIAN_POINT('',(39.5,-5.05,-6.18446633569413E-16));
#80474=CARTESIAN_POINT('',(29.75,-5.05,-6.18446633569413E-16));
#80475=CARTESIAN_POINT('Origin',(39.5,0.,0.));
#80476=CARTESIAN_POINT('Origin',(39.8,0.,0.));
#80477=CARTESIAN_POINT('',(40.,-5.55,6.79678973526781E-16));
#80478=CARTESIAN_POINT('',(39.8,-5.35,-6.55186037543834E-16));
#80479=CARTESIAN_POINT('Origin',(40.,0.,0.));
#80480=CARTESIAN_POINT('Origin',(13.5,0.,0.));
#80481=CARTESIAN_POINT('',(13.5,-2.44929359829471E-15,20.));
#80482=CARTESIAN_POINT('Origin',(13.5,-2.63299061816681E-15,21.5));
#80483=CARTESIAN_POINT('',(13.5,-20.,-2.44929359829471E-15));
#80484=CARTESIAN_POINT('Origin',(13.5,0.,0.));
#80485=CARTESIAN_POINT('Origin',(13.5,0.,0.));
#80486=CARTESIAN_POINT('Origin',(15.25,0.,0.));
#80487=CARTESIAN_POINT('',(18.5,-20.,-2.44929359829471E-15));
#80488=CARTESIAN_POINT('Origin',(18.5,0.,0.));
#80489=CARTESIAN_POINT('',(15.25,-20.,-2.44929359829471E-15));
#80490=CARTESIAN_POINT('Origin',(-4.,19.5,0.));
#80491=CARTESIAN_POINT('',(-4.,-19.5,-2.38806125833734E-15));
#80492=CARTESIAN_POINT('Origin',(-4.,0.,0.));
#80493=CARTESIAN_POINT('Origin',(-3.75,0.,0.));
#80494=CARTESIAN_POINT('',(-3.5,-20.,-2.44929359829471E-15));
#80495=CARTESIAN_POINT('Origin',(-3.5,0.,0.));
#80496=CARTESIAN_POINT('',(-3.75,-19.75,-2.41867742831602E-15));
#80497=CARTESIAN_POINT('Origin',(-1.75,0.,0.));
#80498=CARTESIAN_POINT('',(0.,-20.,-2.44929359829471E-15));
#80499=CARTESIAN_POINT('Origin',(0.,0.,0.));
#80500=CARTESIAN_POINT('',(-1.75,-20.,-2.44929359829471E-15));
#80501=CARTESIAN_POINT('Origin',(0.,47.,0.));
#80502=CARTESIAN_POINT('',(-2.35922392732846E-15,-47.,-5.75583995599256E-15));
#80503=CARTESIAN_POINT('Origin',(0.,0.,0.));
#80504=CARTESIAN_POINT('Origin',(0.499999999999998,0.,0.));
#80505=CARTESIAN_POINT('',(1.,-48.,-5.8783046359073E-15));
#80506=CARTESIAN_POINT('Origin',(1.,0.,0.));
#80507=CARTESIAN_POINT('',(0.499999999999998,-47.5,-5.81707229594993E-15));
#80508=CARTESIAN_POINT('Origin',(6.,0.,0.));
#80509=CARTESIAN_POINT('',(11.,-48.,-5.8783046359073E-15));
#80510=CARTESIAN_POINT('Origin',(11.,0.,0.));
#80511=CARTESIAN_POINT('',(6.,-48.,-5.8783046359073E-15));
#80512=CARTESIAN_POINT('Origin',(11.5,0.,0.));
#80513=CARTESIAN_POINT('',(11.5,-47.5,-5.81707229594993E-15));
#80514=CARTESIAN_POINT('Origin',(18.5,14.995,0.));
#80515=CARTESIAN_POINT('',(18.5,-14.995,-1.83635787532146E-15));
#80516=CARTESIAN_POINT('Origin',(18.5,0.,0.));
#80517=CARTESIAN_POINT('Origin',(28.75,0.,0.));
#80518=CARTESIAN_POINT('',(39.,-14.995,-1.83635787532146E-15));
#80519=CARTESIAN_POINT('Origin',(39.,0.,0.));
#80520=CARTESIAN_POINT('',(28.75,-14.995,-1.83635787532146E-15));
#80521=CARTESIAN_POINT('Origin',(39.5,0.,0.));
#80522=CARTESIAN_POINT('',(40.,-13.995,-1.71389319540672E-15));
#80523=CARTESIAN_POINT('Origin',(40.,0.,0.));
#80524=CARTESIAN_POINT('',(39.5,-14.495,-1.77512553536409E-15));
#80525=CARTESIAN_POINT('Origin',(40.,0.,0.));
#80526=CARTESIAN_POINT('',(0.,0.,0.));
#80527=CARTESIAN_POINT('Origin',(28.9568224176764,-54.2987720370293,-0.6));
#80528=CARTESIAN_POINT('',(28.9568224176764,-54.2987720370293,-0.6));
#80529=CARTESIAN_POINT('',(31.0441293939948,-54.2987720370293,-0.6));
#80530=CARTESIAN_POINT('',(14.4784112088382,-54.2987720370293,-0.6));
#80531=CARTESIAN_POINT('',(28.9568224176764,-54.2987720370293,-0.9));
#80532=CARTESIAN_POINT('',(28.9568224176764,-54.2987720370293,-0.6));
#80533=CARTESIAN_POINT('',(31.0441293939948,-54.2987720370293,-0.9));
#80534=CARTESIAN_POINT('',(28.9568224176764,-54.2987720370293,-0.9));
#80535=CARTESIAN_POINT('',(31.0441293939948,-54.2987720370293,-0.6));
#80536=CARTESIAN_POINT('Origin',(28.9568224176764,-53.1414733529091,-0.6));
#80537=CARTESIAN_POINT('',(28.9568224176764,-53.1414733529091,-0.6));
#80538=CARTESIAN_POINT('',(28.9568224176764,-53.0707366764545,-0.6));
#80539=CARTESIAN_POINT('',(28.9568224176764,-53.1414733529091,-0.9));
#80540=CARTESIAN_POINT('',(28.9568224176764,-53.1414733529091,-0.6));
#80541=CARTESIAN_POINT('',(28.9568224176764,-53.1414733529091,-0.9));
#80542=CARTESIAN_POINT('Origin',(30.8377161249518,-53.1414733529091,-0.6));
#80543=CARTESIAN_POINT('',(30.8377161249518,-53.1414733529091,-0.6));
#80544=CARTESIAN_POINT('',(15.4188580624759,-53.1414733529091,-0.6));
#80545=CARTESIAN_POINT('',(30.8377161249518,-53.1414733529091,-0.9));
#80546=CARTESIAN_POINT('',(30.8377161249518,-53.1414733529091,-0.6));
#80547=CARTESIAN_POINT('',(30.8377161249518,-53.1414733529091,-0.9));
#80548=CARTESIAN_POINT('Origin',(30.8377161249518,-52.7425650954247,-0.6));
#80549=CARTESIAN_POINT('',(30.8377161249518,-52.7425650954247,-0.6));
#80550=CARTESIAN_POINT('',(30.8377161249518,-52.8712825477123,-0.6));
#80551=CARTESIAN_POINT('',(30.8377161249518,-52.7425650954247,-0.9));
#80552=CARTESIAN_POINT('',(30.8377161249518,-52.7425650954247,-0.6));
#80553=CARTESIAN_POINT('',(30.8377161249518,-52.7425650954247,-0.9));
#80554=CARTESIAN_POINT('Origin',(28.9568224176764,-52.7425650954247,-0.6));
#80555=CARTESIAN_POINT('',(28.9568224176764,-52.7425650954247,-0.6));
#80556=CARTESIAN_POINT('',(14.4784112088382,-52.7425650954247,-0.6));
#80557=CARTESIAN_POINT('',(28.9568224176764,-52.7425650954247,-0.9));
#80558=CARTESIAN_POINT('',(28.9568224176764,-52.7425650954247,-0.6));
#80559=CARTESIAN_POINT('',(28.9568224176764,-52.7425650954247,-0.9));
#80560=CARTESIAN_POINT('Origin',(28.9568224176764,-51.7012278437614,-0.6));
#80561=CARTESIAN_POINT('',(28.9568224176764,-51.7012278437614,-0.6));
#80562=CARTESIAN_POINT('',(28.9568224176764,-52.3506139218807,-0.6));
#80563=CARTESIAN_POINT('',(28.9568224176764,-51.7012278437614,-0.9));
#80564=CARTESIAN_POINT('',(28.9568224176764,-51.7012278437614,-0.6));
#80565=CARTESIAN_POINT('',(28.9568224176764,-51.7012278437614,-0.9));
#80566=CARTESIAN_POINT('Origin',(30.9652796015143,-51.7012278437614,-0.6));
#80567=CARTESIAN_POINT('',(30.9652796015143,-51.7012278437614,-0.6));
#80568=CARTESIAN_POINT('',(15.4826398007572,-51.7012278437614,-0.6));
#80569=CARTESIAN_POINT('',(30.9652796015143,-51.7012278437614,-0.9));
#80570=CARTESIAN_POINT('',(30.9652796015143,-51.7012278437614,-0.6));
#80571=CARTESIAN_POINT('',(30.9652796015143,-51.7012278437614,-0.9));
#80572=CARTESIAN_POINT('Origin',(30.9652796015143,-51.3000003695488,-0.6));
#80573=CARTESIAN_POINT('',(30.9652796015143,-51.3000003695488,-0.6));
#80574=CARTESIAN_POINT('',(30.9652796015143,-52.1500001847744,-0.6));
#80575=CARTESIAN_POINT('',(30.9652796015143,-51.3000003695488,-0.9));
#80576=CARTESIAN_POINT('',(30.9652796015143,-51.3000003695488,-0.6));
#80577=CARTESIAN_POINT('',(30.9652796015143,-51.3000003695488,-0.9));
#80578=CARTESIAN_POINT('Origin',(28.5068884119391,-51.3000003695488,-0.6));
#80579=CARTESIAN_POINT('',(28.5068884119391,-51.3000003695488,-0.6));
#80580=CARTESIAN_POINT('',(14.2534442059696,-51.3000003695488,-0.6));
#80581=CARTESIAN_POINT('',(28.5068884119391,-51.3000003695488,-0.9));
#80582=CARTESIAN_POINT('',(28.5068884119391,-51.3000003695488,-0.6));
#80583=CARTESIAN_POINT('',(28.5068884119391,-51.3000003695488,-0.9));
#80584=CARTESIAN_POINT('Origin',(28.5068884119391,-54.7000001072884,-0.6));
#80585=CARTESIAN_POINT('',(28.5068884119391,-54.7000001072884,-0.6));
#80586=CARTESIAN_POINT('',(28.5068884119391,-53.8500000536442,-0.6));
#80587=CARTESIAN_POINT('',(28.5068884119391,-54.7000001072884,-0.9));
#80588=CARTESIAN_POINT('',(28.5068884119391,-54.7000001072884,-0.6));
#80589=CARTESIAN_POINT('',(28.5068884119391,-54.7000001072884,-0.9));
#80590=CARTESIAN_POINT('Origin',(31.0441293939948,-54.7000001072884,-0.6));
#80591=CARTESIAN_POINT('',(31.0441293939948,-54.7000001072884,-0.6));
#80592=CARTESIAN_POINT('',(15.5220646969974,-54.7000001072884,-0.6));
#80593=CARTESIAN_POINT('',(31.0441293939948,-54.7000001072884,-0.9));
#80594=CARTESIAN_POINT('',(31.0441293939948,-54.7000001072884,-0.6));
#80595=CARTESIAN_POINT('',(31.0441293939948,-54.7000001072884,-0.9));
#80596=CARTESIAN_POINT('Origin',(31.0441293939948,-54.2987720370293,-0.6));
#80597=CARTESIAN_POINT('',(31.0441293939948,-53.6493860185146,-0.6));
#80598=CARTESIAN_POINT('',(31.0441293939948,-54.2987720370293,-0.9));
#80599=CARTESIAN_POINT('Origin',(29.775508902967,-53.0000002384186,-0.9));
#80600=CARTESIAN_POINT('Origin',(23.8243475183845,-51.3000003695488,-0.6));
#80601=CARTESIAN_POINT('',(23.8243475183845,-51.3000003695488,-0.6));
#80602=CARTESIAN_POINT('',(24.2742815241218,-51.3000003695488,-0.6));
#80603=CARTESIAN_POINT('',(11.9121737591922,-51.3000003695488,-0.6));
#80604=CARTESIAN_POINT('',(23.8243475183845,-51.3000003695488,-0.9));
#80605=CARTESIAN_POINT('',(23.8243475183845,-51.3000003695488,-0.6));
#80606=CARTESIAN_POINT('',(24.2742815241218,-51.3000003695488,-0.9));
#80607=CARTESIAN_POINT('',(23.8243475183845,-51.3000003695488,-0.9));
#80608=CARTESIAN_POINT('',(24.2742815241218,-51.3000003695488,-0.6));
#80609=CARTESIAN_POINT('Origin',(23.8243475183845,-54.7000001072884,-0.6));
#80610=CARTESIAN_POINT('',(23.8243475183845,-54.7000001072884,-0.6));
#80611=CARTESIAN_POINT('',(23.8243475183845,-53.8500000536442,-0.6));
#80612=CARTESIAN_POINT('',(23.8243475183845,-54.7000001072884,-0.9));
#80613=CARTESIAN_POINT('',(23.8243475183845,-54.7000001072884,-0.6));
#80614=CARTESIAN_POINT('',(23.8243475183845,-54.7000001072884,-0.9));
#80615=CARTESIAN_POINT('Origin',(24.2742815241218,-54.7000001072884,-0.6));
#80616=CARTESIAN_POINT('',(24.2742815241218,-54.7000001072884,-0.6));
#80617=CARTESIAN_POINT('',(12.1371407620609,-54.7000001072884,-0.6));
#80618=CARTESIAN_POINT('',(24.2742815241218,-54.7000001072884,-0.9));
#80619=CARTESIAN_POINT('',(24.2742815241218,-54.7000001072884,-0.6));
#80620=CARTESIAN_POINT('',(24.2742815241218,-54.7000001072884,-0.9));
#80621=CARTESIAN_POINT('Origin',(24.2742815241218,-51.3000003695488,-0.6));
#80622=CARTESIAN_POINT('',(24.2742815241218,-52.1500001847744,-0.6));
#80623=CARTESIAN_POINT('',(24.2742815241218,-51.3000003695488,-0.9));
#80624=CARTESIAN_POINT('Origin',(24.0493145212531,-53.0000002384186,-0.9));
#80625=CARTESIAN_POINT('Ctrl Pts',(19.2345800623298,-54.7579811215401,-0.6));
#80626=CARTESIAN_POINT('Ctrl Pts',(19.2345800623298,-54.7579811215401,-0.9));
#80627=CARTESIAN_POINT('Ctrl Pts',(18.773049376905,-54.7579811215401,-0.6));
#80628=CARTESIAN_POINT('Ctrl Pts',(18.773049376905,-54.7579811215401,-0.9));
#80629=CARTESIAN_POINT('Ctrl Pts',(18.4611120447516,-54.623465359211,-0.6));
#80630=CARTESIAN_POINT('Ctrl Pts',(18.4611120447516,-54.623465359211,-0.9));
#80631=CARTESIAN_POINT('',(19.2345800623298,-54.7579811215401,-0.6));
#80632=CARTESIAN_POINT('',(18.4611120447516,-54.623465359211,-0.6));
#80633=CARTESIAN_POINT('Ctrl Pts',(19.2345800623298,-54.7579811215401,-0.6));
#80634=CARTESIAN_POINT('Ctrl Pts',(18.773049376905,-54.7579811215401,-0.6));
#80635=CARTESIAN_POINT('Ctrl Pts',(18.4611120447516,-54.623465359211,-0.6));
#80636=CARTESIAN_POINT('',(19.2345800623298,-54.7579811215401,-0.9));
#80637=CARTESIAN_POINT('',(19.2345800623298,-54.7579811215401,-0.6));
#80638=CARTESIAN_POINT('',(18.4611120447516,-54.623465359211,-0.9));
#80639=CARTESIAN_POINT('Ctrl Pts',(19.2345800623298,-54.7579811215401,-0.9));
#80640=CARTESIAN_POINT('Ctrl Pts',(18.773049376905,-54.7579811215401,-0.9));
#80641=CARTESIAN_POINT('Ctrl Pts',(18.4611120447516,-54.623465359211,-0.9));
#80642=CARTESIAN_POINT('',(18.4611120447516,-54.623465359211,-0.6));
#80643=CARTESIAN_POINT('Ctrl Pts',(19.889763854444,-54.6246246695518,-0.6));
#80644=CARTESIAN_POINT('Ctrl Pts',(19.889763854444,-54.6246246695518,-0.9));
#80645=CARTESIAN_POINT('Ctrl Pts',(19.5987024530768,-54.7579811215401,-0.6));
#80646=CARTESIAN_POINT('Ctrl Pts',(19.5987024530768,-54.7579811215401,-0.9));
#80647=CARTESIAN_POINT('Ctrl Pts',(19.2345800623298,-54.7579811215401,-0.6));
#80648=CARTESIAN_POINT('Ctrl Pts',(19.2345800623298,-54.7579811215401,-0.9));
#80649=CARTESIAN_POINT('',(19.889763854444,-54.6246246695518,-0.6));
#80650=CARTESIAN_POINT('Ctrl Pts',(19.889763854444,-54.6246246695518,-0.6));
#80651=CARTESIAN_POINT('Ctrl Pts',(19.5987024530768,-54.7579811215401,-0.6));
#80652=CARTESIAN_POINT('Ctrl Pts',(19.2345800623298,-54.7579811215401,-0.6));
#80653=CARTESIAN_POINT('',(19.889763854444,-54.6246246695518,-0.9));
#80654=CARTESIAN_POINT('',(19.889763854444,-54.6246246695518,-0.6));
#80655=CARTESIAN_POINT('Ctrl Pts',(19.889763854444,-54.6246246695518,-0.9));
#80656=CARTESIAN_POINT('Ctrl Pts',(19.5987024530768,-54.7579811215401,-0.9));
#80657=CARTESIAN_POINT('Ctrl Pts',(19.2345800623298,-54.7579811215401,-0.9));
#80658=CARTESIAN_POINT('Ctrl Pts',(20.3362169489264,-54.2512277960777,-0.6));
#80659=CARTESIAN_POINT('Ctrl Pts',(20.3362169489264,-54.2512277960777,-0.9));
#80660=CARTESIAN_POINT('Ctrl Pts',(20.1808347925544,-54.4912688136101,-0.6));
#80661=CARTESIAN_POINT('Ctrl Pts',(20.1808347925544,-54.4912688136101,-0.9));
#80662=CARTESIAN_POINT('Ctrl Pts',(19.889763854444,-54.6246246695518,-0.6));
#80663=CARTESIAN_POINT('Ctrl Pts',(19.889763854444,-54.6246246695518,-0.9));
#80664=CARTESIAN_POINT('',(20.3362169489264,-54.2512277960777,-0.6));
#80665=CARTESIAN_POINT('Ctrl Pts',(20.3362169489264,-54.2512277960777,-0.6));
#80666=CARTESIAN_POINT('Ctrl Pts',(20.1808347925544,-54.4912688136101,-0.6));
#80667=CARTESIAN_POINT('Ctrl Pts',(19.889763854444,-54.6246246695518,-0.6));
#80668=CARTESIAN_POINT('',(20.3362169489264,-54.2512277960777,-0.9));
#80669=CARTESIAN_POINT('',(20.3362169489264,-54.2512277960777,-0.6));
#80670=CARTESIAN_POINT('Ctrl Pts',(20.3362169489264,-54.2512277960777,-0.9));
#80671=CARTESIAN_POINT('Ctrl Pts',(20.1808347925544,-54.4912688136101,-0.9));
#80672=CARTESIAN_POINT('Ctrl Pts',(19.889763854444,-54.6246246695518,-0.9));
#80673=CARTESIAN_POINT('Ctrl Pts',(20.4916086420417,-53.7398366332054,-0.6));
#80674=CARTESIAN_POINT('Ctrl Pts',(20.4916086420417,-53.7398366332054,-0.9));
#80675=CARTESIAN_POINT('Ctrl Pts',(20.4916086420417,-54.0111867785454,-0.6));
#80676=CARTESIAN_POINT('Ctrl Pts',(20.4916086420417,-54.0111867785454,-0.9));
#80677=CARTESIAN_POINT('Ctrl Pts',(20.3362169489264,-54.2512277960777,-0.6));
#80678=CARTESIAN_POINT('Ctrl Pts',(20.3362169489264,-54.2512277960777,-0.9));
#80679=CARTESIAN_POINT('',(20.4916086420417,-53.7398366332054,-0.6));
#80680=CARTESIAN_POINT('Ctrl Pts',(20.4916086420417,-53.7398366332054,-0.6));
#80681=CARTESIAN_POINT('Ctrl Pts',(20.4916086420417,-54.0111867785454,-0.6));
#80682=CARTESIAN_POINT('Ctrl Pts',(20.3362169489264,-54.2512277960777,-0.6));
#80683=CARTESIAN_POINT('',(20.4916086420417,-53.7398366332054,-0.9));
#80684=CARTESIAN_POINT('',(20.4916086420417,-53.7398366332054,-0.6));
#80685=CARTESIAN_POINT('Ctrl Pts',(20.4916086420417,-53.7398366332054,-0.9));
#80686=CARTESIAN_POINT('Ctrl Pts',(20.4916086420417,-54.0111867785454,-0.9));
#80687=CARTESIAN_POINT('Ctrl Pts',(20.3362169489264,-54.2512277960777,-0.9));
#80688=CARTESIAN_POINT('Ctrl Pts',(20.3501310572028,-53.2562760710716,-0.6));
#80689=CARTESIAN_POINT('Ctrl Pts',(20.3501310572028,-53.2562760710716,-0.9));
#80690=CARTESIAN_POINT('Ctrl Pts',(20.4916086420417,-53.4661666750908,-0.6));
#80691=CARTESIAN_POINT('Ctrl Pts',(20.4916086420417,-53.4661666750908,-0.9));
#80692=CARTESIAN_POINT('Ctrl Pts',(20.4916086420417,-53.7398366332054,-0.6));
#80693=CARTESIAN_POINT('Ctrl Pts',(20.4916086420417,-53.7398366332054,-0.9));
#80694=CARTESIAN_POINT('',(20.3501310572028,-53.2562760710716,-0.6));
#80695=CARTESIAN_POINT('Ctrl Pts',(20.3501310572028,-53.2562760710716,-0.6));
#80696=CARTESIAN_POINT('Ctrl Pts',(20.4916086420417,-53.4661666750908,-0.6));
#80697=CARTESIAN_POINT('Ctrl Pts',(20.4916086420417,-53.7398366332054,-0.6));
#80698=CARTESIAN_POINT('',(20.3501310572028,-53.2562760710716,-0.9));
#80699=CARTESIAN_POINT('',(20.3501310572028,-53.2562760710716,-0.6));
#80700=CARTESIAN_POINT('Ctrl Pts',(20.3501310572028,-53.2562760710716,-0.9));
#80701=CARTESIAN_POINT('Ctrl Pts',(20.4916086420417,-53.4661666750908,-0.9));
#80702=CARTESIAN_POINT('Ctrl Pts',(20.4916086420417,-53.7398366332054,-0.9));
#80703=CARTESIAN_POINT('Ctrl Pts',(19.9118032678962,-52.9095498919487,-0.6));
#80704=CARTESIAN_POINT('Ctrl Pts',(19.9118032678962,-52.9095498919487,-0.9));
#80705=CARTESIAN_POINT('Ctrl Pts',(20.2086630091071,-53.046384871006,-0.6));
#80706=CARTESIAN_POINT('Ctrl Pts',(20.2086630091071,-53.046384871006,-0.9));
#80707=CARTESIAN_POINT('Ctrl Pts',(20.3501310572028,-53.2562760710716,-0.6));
#80708=CARTESIAN_POINT('Ctrl Pts',(20.3501310572028,-53.2562760710716,-0.9));
#80709=CARTESIAN_POINT('',(19.9118032678962,-52.9095498919487,-0.6));
#80710=CARTESIAN_POINT('Ctrl Pts',(19.9118032678962,-52.9095498919487,-0.6));
#80711=CARTESIAN_POINT('Ctrl Pts',(20.2086630091071,-53.046384871006,-0.6));
#80712=CARTESIAN_POINT('Ctrl Pts',(20.3501310572028,-53.2562760710716,-0.6));
#80713=CARTESIAN_POINT('',(19.9118032678962,-52.9095498919487,-0.9));
#80714=CARTESIAN_POINT('',(19.9118032678962,-52.9095498919487,-0.6));
#80715=CARTESIAN_POINT('Ctrl Pts',(19.9118032678962,-52.9095498919487,-0.9));
#80716=CARTESIAN_POINT('Ctrl Pts',(20.2086630091071,-53.046384871006,-0.9));
#80717=CARTESIAN_POINT('Ctrl Pts',(20.3501310572028,-53.2562760710716,-0.9));
#80718=CARTESIAN_POINT('Ctrl Pts',(19.1592111811042,-52.6927010416985,-0.6));
#80719=CARTESIAN_POINT('Ctrl Pts',(19.1592111811042,-52.6927010416985,-0.9));
#80720=CARTESIAN_POINT('Ctrl Pts',(19.7077074274421,-52.8167806267738,-0.6));
#80721=CARTESIAN_POINT('Ctrl Pts',(19.7077074274421,-52.8167806267738,-0.9));
#80722=CARTESIAN_POINT('Ctrl Pts',(19.9118032678962,-52.9095498919487,-0.6));
#80723=CARTESIAN_POINT('Ctrl Pts',(19.9118032678962,-52.9095498919487,-0.9));
#80724=CARTESIAN_POINT('',(19.1592111811042,-52.6927010416985,-0.6));
#80725=CARTESIAN_POINT('Ctrl Pts',(19.1592111811042,-52.6927010416985,-0.6));
#80726=CARTESIAN_POINT('Ctrl Pts',(19.7077074274421,-52.8167806267738,-0.6));
#80727=CARTESIAN_POINT('Ctrl Pts',(19.9118032678962,-52.9095498919487,-0.6));
#80728=CARTESIAN_POINT('',(19.1592111811042,-52.6927010416985,-0.9));
#80729=CARTESIAN_POINT('',(19.1592111811042,-52.6927010416985,-0.6));
#80730=CARTESIAN_POINT('Ctrl Pts',(19.1592111811042,-52.6927010416985,-0.9));
#80731=CARTESIAN_POINT('Ctrl Pts',(19.7077074274421,-52.8167806267738,-0.9));
#80732=CARTESIAN_POINT('Ctrl Pts',(19.9118032678962,-52.9095498919487,-0.9));
#80733=CARTESIAN_POINT('Ctrl Pts',(18.4808340296149,-52.4503414034843,-0.6));
#80734=CARTESIAN_POINT('Ctrl Pts',(18.4808340296149,-52.4503414034843,-0.9));
#80735=CARTESIAN_POINT('Ctrl Pts',(18.6107053980231,-52.5686220526695,-0.6));
#80736=CARTESIAN_POINT('Ctrl Pts',(18.6107053980231,-52.5686220526695,-0.9));
#80737=CARTESIAN_POINT('Ctrl Pts',(19.1592111811042,-52.6927010416985,-0.6));
#80738=CARTESIAN_POINT('Ctrl Pts',(19.1592111811042,-52.6927010416985,-0.9));
#80739=CARTESIAN_POINT('',(18.4808340296149,-52.4503414034843,-0.6));
#80740=CARTESIAN_POINT('Ctrl Pts',(18.4808340296149,-52.4503414034843,-0.6));
#80741=CARTESIAN_POINT('Ctrl Pts',(18.6107053980231,-52.5686220526695,-0.6));
#80742=CARTESIAN_POINT('Ctrl Pts',(19.1592111811042,-52.6927010416985,-0.6));
#80743=CARTESIAN_POINT('',(18.4808340296149,-52.4503414034843,-0.9));
#80744=CARTESIAN_POINT('',(18.4808340296149,-52.4503414034843,-0.6));
#80745=CARTESIAN_POINT('Ctrl Pts',(18.4808340296149,-52.4503414034843,-0.9));
#80746=CARTESIAN_POINT('Ctrl Pts',(18.6107053980231,-52.5686220526695,-0.9));
#80747=CARTESIAN_POINT('Ctrl Pts',(19.1592111811042,-52.6927010416985,-0.9));
#80748=CARTESIAN_POINT('Ctrl Pts',(18.3486356958747,-52.1488408446312,-0.6));
#80749=CARTESIAN_POINT('Ctrl Pts',(18.3486356958747,-52.1488408446312,-0.9));
#80750=CARTESIAN_POINT('Ctrl Pts',(18.3486356958747,-52.3320601582527,-0.6));
#80751=CARTESIAN_POINT('Ctrl Pts',(18.3486356958747,-52.3320601582527,-0.9));
#80752=CARTESIAN_POINT('Ctrl Pts',(18.4808340296149,-52.4503414034843,-0.6));
#80753=CARTESIAN_POINT('Ctrl Pts',(18.4808340296149,-52.4503414034843,-0.9));
#80754=CARTESIAN_POINT('',(18.3486356958747,-52.1488408446312,-0.6));
#80755=CARTESIAN_POINT('Ctrl Pts',(18.3486356958747,-52.1488408446312,-0.6));
#80756=CARTESIAN_POINT('Ctrl Pts',(18.3486356958747,-52.3320601582527,-0.6));
#80757=CARTESIAN_POINT('Ctrl Pts',(18.4808340296149,-52.4503414034843,-0.6));
#80758=CARTESIAN_POINT('',(18.3486356958747,-52.1488408446312,-0.9));
#80759=CARTESIAN_POINT('',(18.3486356958747,-52.1488408446312,-0.6));
#80760=CARTESIAN_POINT('Ctrl Pts',(18.3486356958747,-52.1488408446312,-0.9));
#80761=CARTESIAN_POINT('Ctrl Pts',(18.3486356958747,-52.3320601582527,-0.9));
#80762=CARTESIAN_POINT('Ctrl Pts',(18.4808340296149,-52.4503414034843,-0.9));
#80763=CARTESIAN_POINT('Ctrl Pts',(18.5353365167975,-51.788199365139,-0.6));
#80764=CARTESIAN_POINT('Ctrl Pts',(18.5353365167975,-51.788199365139,-0.9));
#80765=CARTESIAN_POINT('Ctrl Pts',(18.3486356958747,-51.9377903342247,-0.6));
#80766=CARTESIAN_POINT('Ctrl Pts',(18.3486356958747,-51.9377903342247,-0.9));
#80767=CARTESIAN_POINT('Ctrl Pts',(18.3486356958747,-52.1488408446312,-0.6));
#80768=CARTESIAN_POINT('Ctrl Pts',(18.3486356958747,-52.1488408446312,-0.9));
#80769=CARTESIAN_POINT('',(18.5353365167975,-51.788199365139,-0.6));
#80770=CARTESIAN_POINT('Ctrl Pts',(18.5353365167975,-51.788199365139,-0.6));
#80771=CARTESIAN_POINT('Ctrl Pts',(18.3486356958747,-51.9377903342247,-0.6));
#80772=CARTESIAN_POINT('Ctrl Pts',(18.3486356958747,-52.1488408446312,-0.6));
#80773=CARTESIAN_POINT('',(18.5353365167975,-51.788199365139,-0.9));
#80774=CARTESIAN_POINT('',(18.5353365167975,-51.788199365139,-0.6));
#80775=CARTESIAN_POINT('Ctrl Pts',(18.5353365167975,-51.788199365139,-0.9));
#80776=CARTESIAN_POINT('Ctrl Pts',(18.3486356958747,-51.9377903342247,-0.9));
#80777=CARTESIAN_POINT('Ctrl Pts',(18.3486356958747,-52.1488408446312,-0.9));
#80778=CARTESIAN_POINT('Ctrl Pts',(19.1302194818854,-51.6386083960533,-0.6));
#80779=CARTESIAN_POINT('Ctrl Pts',(19.1302194818854,-51.6386083960533,-0.9));
#80780=CARTESIAN_POINT('Ctrl Pts',(18.7220278009772,-51.6386083960533,-0.6));
#80781=CARTESIAN_POINT('Ctrl Pts',(18.7220278009772,-51.6386083960533,-0.9));
#80782=CARTESIAN_POINT('Ctrl Pts',(18.5353365167975,-51.788199365139,-0.6));
#80783=CARTESIAN_POINT('Ctrl Pts',(18.5353365167975,-51.788199365139,-0.9));
#80784=CARTESIAN_POINT('',(19.1302194818854,-51.6386083960533,-0.6));
#80785=CARTESIAN_POINT('Ctrl Pts',(19.1302194818854,-51.6386083960533,-0.6));
#80786=CARTESIAN_POINT('Ctrl Pts',(18.7220278009772,-51.6386083960533,-0.6));
#80787=CARTESIAN_POINT('Ctrl Pts',(18.5353365167975,-51.788199365139,-0.6));
#80788=CARTESIAN_POINT('',(19.1302194818854,-51.6386083960533,-0.9));
#80789=CARTESIAN_POINT('',(19.1302194818854,-51.6386083960533,-0.6));
#80790=CARTESIAN_POINT('Ctrl Pts',(19.1302194818854,-51.6386083960533,-0.9));
#80791=CARTESIAN_POINT('Ctrl Pts',(18.7220278009772,-51.6386083960533,-0.9));
#80792=CARTESIAN_POINT('Ctrl Pts',(18.5353365167975,-51.788199365139,-0.9));
#80793=CARTESIAN_POINT('Ctrl Pts',(19.7227850183845,-51.8032745718956,-0.6));
#80794=CARTESIAN_POINT('Ctrl Pts',(19.7227850183845,-51.8032745718956,-0.9));
#80795=CARTESIAN_POINT('Ctrl Pts',(19.5221700891852,-51.6386083960533,-0.6));
#80796=CARTESIAN_POINT('Ctrl Pts',(19.5221700891852,-51.6386083960533,-0.9));
#80797=CARTESIAN_POINT('Ctrl Pts',(19.1302194818854,-51.6386083960533,-0.6));
#80798=CARTESIAN_POINT('Ctrl Pts',(19.1302194818854,-51.6386083960533,-0.9));
#80799=CARTESIAN_POINT('',(19.7227850183845,-51.8032745718956,-0.6));
#80800=CARTESIAN_POINT('Ctrl Pts',(19.7227850183845,-51.8032745718956,-0.6));
#80801=CARTESIAN_POINT('Ctrl Pts',(19.5221700891852,-51.6386083960533,-0.6));
#80802=CARTESIAN_POINT('Ctrl Pts',(19.1302194818854,-51.6386083960533,-0.6));
#80803=CARTESIAN_POINT('',(19.7227850183845,-51.8032745718956,-0.9));
#80804=CARTESIAN_POINT('',(19.7227850183845,-51.8032745718956,-0.6));
#80805=CARTESIAN_POINT('Ctrl Pts',(19.7227850183845,-51.8032745718956,-0.9));
#80806=CARTESIAN_POINT('Ctrl Pts',(19.5221700891852,-51.6386083960533,-0.9));
#80807=CARTESIAN_POINT('Ctrl Pts',(19.1302194818854,-51.6386083960533,-0.9));
#80808=CARTESIAN_POINT('Ctrl Pts',(19.958180449903,-52.2903136610985,-0.6));
#80809=CARTESIAN_POINT('Ctrl Pts',(19.958180449903,-52.2903136610985,-0.9));
#80810=CARTESIAN_POINT('Ctrl Pts',(19.9233904108405,-51.9679401516914,-0.6));
#80811=CARTESIAN_POINT('Ctrl Pts',(19.9233904108405,-51.9679401516914,-0.9));
#80812=CARTESIAN_POINT('Ctrl Pts',(19.7227850183845,-51.8032745718956,-0.6));
#80813=CARTESIAN_POINT('Ctrl Pts',(19.7227850183845,-51.8032745718956,-0.9));
#80814=CARTESIAN_POINT('',(19.958180449903,-52.2903136610985,-0.6));
#80815=CARTESIAN_POINT('Ctrl Pts',(19.958180449903,-52.2903136610985,-0.6));
#80816=CARTESIAN_POINT('Ctrl Pts',(19.9233904108405,-51.9679401516914,-0.6));
#80817=CARTESIAN_POINT('Ctrl Pts',(19.7227850183845,-51.8032745718956,-0.6));
#80818=CARTESIAN_POINT('',(19.958180449903,-52.2903136610985,-0.9));
#80819=CARTESIAN_POINT('',(19.958180449903,-52.2903136610985,-0.6));
#80820=CARTESIAN_POINT('Ctrl Pts',(19.958180449903,-52.2903136610985,-0.9));
#80821=CARTESIAN_POINT('Ctrl Pts',(19.9233904108405,-51.9679401516914,-0.9));
#80822=CARTESIAN_POINT('Ctrl Pts',(19.7227850183845,-51.8032745718956,-0.9));
#80823=CARTESIAN_POINT('Origin',(20.3895654901862,-52.2578446269035,-0.6));
#80824=CARTESIAN_POINT('',(20.3895654901862,-52.2578446269035,-0.6));
#80825=CARTESIAN_POINT('',(10.2244394493007,-53.022942611759,-0.6));
#80826=CARTESIAN_POINT('',(20.3895654901862,-52.2578446269035,-0.9));
#80827=CARTESIAN_POINT('',(20.3895654901862,-52.2578446269035,-0.6));
#80828=CARTESIAN_POINT('',(20.3895654901862,-52.2578446269035,-0.9));
#80829=CARTESIAN_POINT('Ctrl Pts',(20.2225771173835,-51.7221013903618,-0.6));
#80830=CARTESIAN_POINT('Ctrl Pts',(20.2225771173835,-51.7221013903618,-0.9));
#80831=CARTESIAN_POINT('Ctrl Pts',(20.3779688104987,-51.9586632847786,-0.6));
#80832=CARTESIAN_POINT('Ctrl Pts',(20.3779688104987,-51.9586632847786,-0.9));
#80833=CARTESIAN_POINT('Ctrl Pts',(20.3895654901862,-52.2578446269035,-0.6));
#80834=CARTESIAN_POINT('Ctrl Pts',(20.3895654901862,-52.2578446269035,-0.9));
#80835=CARTESIAN_POINT('',(20.2225771173835,-51.7221013903618,-0.6));
#80836=CARTESIAN_POINT('Ctrl Pts',(20.2225771173835,-51.7221013903618,-0.6));
#80837=CARTESIAN_POINT('Ctrl Pts',(20.3779688104987,-51.9586632847786,-0.6));
#80838=CARTESIAN_POINT('Ctrl Pts',(20.3895654901862,-52.2578446269035,-0.6));
#80839=CARTESIAN_POINT('',(20.2225771173835,-51.7221013903618,-0.9));
#80840=CARTESIAN_POINT('',(20.2225771173835,-51.7221013903618,-0.6));
#80841=CARTESIAN_POINT('Ctrl Pts',(20.2225771173835,-51.7221013903618,-0.9));
#80842=CARTESIAN_POINT('Ctrl Pts',(20.3779688104987,-51.9586632847786,-0.9));
#80843=CARTESIAN_POINT('Ctrl Pts',(20.3895654901862,-52.2578446269035,-0.9));
#80844=CARTESIAN_POINT('Ctrl Pts',(19.7784414514899,-51.3637797236443,-0.6));
#80845=CARTESIAN_POINT('Ctrl Pts',(19.7784414514899,-51.3637797236443,-0.9));
#80846=CARTESIAN_POINT('Ctrl Pts',(20.0671854242682,-51.4855388998985,-0.6));
#80847=CARTESIAN_POINT('Ctrl Pts',(20.0671854242682,-51.4855388998985,-0.9));
#80848=CARTESIAN_POINT('Ctrl Pts',(20.2225771173835,-51.7221013903618,-0.6));
#80849=CARTESIAN_POINT('Ctrl Pts',(20.2225771173835,-51.7221013903618,-0.9));
#80850=CARTESIAN_POINT('',(19.7784414514899,-51.3637797236443,-0.6));
#80851=CARTESIAN_POINT('Ctrl Pts',(19.7784414514899,-51.3637797236443,-0.6));
#80852=CARTESIAN_POINT('Ctrl Pts',(20.0671854242682,-51.4855388998985,-0.6));
#80853=CARTESIAN_POINT('Ctrl Pts',(20.2225771173835,-51.7221013903618,-0.6));
#80854=CARTESIAN_POINT('',(19.7784414514899,-51.3637797236443,-0.9));
#80855=CARTESIAN_POINT('',(19.7784414514899,-51.3637797236443,-0.6));
#80856=CARTESIAN_POINT('Ctrl Pts',(19.7784414514899,-51.3637797236443,-0.9));
#80857=CARTESIAN_POINT('Ctrl Pts',(20.0671854242682,-51.4855388998985,-0.9));
#80858=CARTESIAN_POINT('Ctrl Pts',(20.2225771173835,-51.7221013903618,-0.9));
#80859=CARTESIAN_POINT('Ctrl Pts',(19.1116609796882,-51.2420193552971,-0.6));
#80860=CARTESIAN_POINT('Ctrl Pts',(19.1116609796882,-51.2420193552971,-0.9));
#80861=CARTESIAN_POINT('Ctrl Pts',(19.4896974787116,-51.2420193552971,-0.6));
#80862=CARTESIAN_POINT('Ctrl Pts',(19.4896974787116,-51.2420193552971,-0.9));
#80863=CARTESIAN_POINT('Ctrl Pts',(19.7784414514899,-51.3637797236443,-0.6));
#80864=CARTESIAN_POINT('Ctrl Pts',(19.7784414514899,-51.3637797236443,-0.9));
#80865=CARTESIAN_POINT('',(19.1116609796882,-51.2420193552971,-0.6));
#80866=CARTESIAN_POINT('Ctrl Pts',(19.1116609796882,-51.2420193552971,-0.6));
#80867=CARTESIAN_POINT('Ctrl Pts',(19.4896974787116,-51.2420193552971,-0.6));
#80868=CARTESIAN_POINT('Ctrl Pts',(19.7784414514899,-51.3637797236443,-0.6));
#80869=CARTESIAN_POINT('',(19.1116609796882,-51.2420193552971,-0.9));
#80870=CARTESIAN_POINT('',(19.1116609796882,-51.2420193552971,-0.6));
#80871=CARTESIAN_POINT('Ctrl Pts',(19.1116609796882,-51.2420193552971,-0.9));
#80872=CARTESIAN_POINT('Ctrl Pts',(19.4896974787116,-51.2420193552971,-0.9));
#80873=CARTESIAN_POINT('Ctrl Pts',(19.7784414514899,-51.3637797236443,-0.9));
#80874=CARTESIAN_POINT('Ctrl Pts',(18.4877863153815,-51.3579813838005,-0.6));
#80875=CARTESIAN_POINT('Ctrl Pts',(18.4877863153815,-51.3579813838005,-0.9));
#80876=CARTESIAN_POINT('Ctrl Pts',(18.7684145197272,-51.2420193552971,-0.6));
#80877=CARTESIAN_POINT('Ctrl Pts',(18.7684145197272,-51.2420193552971,-0.9));
#80878=CARTESIAN_POINT('Ctrl Pts',(19.1116609796882,-51.2420193552971,-0.6));
#80879=CARTESIAN_POINT('Ctrl Pts',(19.1116609796882,-51.2420193552971,-0.9));
#80880=CARTESIAN_POINT('',(18.4877863153815,-51.3579813838005,-0.6));
#80881=CARTESIAN_POINT('Ctrl Pts',(18.4877863153815,-51.3579813838005,-0.6));
#80882=CARTESIAN_POINT('Ctrl Pts',(18.7684145197272,-51.2420193552971,-0.6));
#80883=CARTESIAN_POINT('Ctrl Pts',(19.1116609796882,-51.2420193552971,-0.6));
#80884=CARTESIAN_POINT('',(18.4877863153815,-51.3579813838005,-0.9));
#80885=CARTESIAN_POINT('',(18.4877863153815,-51.3579813838005,-0.6));
#80886=CARTESIAN_POINT('Ctrl Pts',(18.4877863153815,-51.3579813838005,-0.9));
#80887=CARTESIAN_POINT('Ctrl Pts',(18.7684145197272,-51.2420193552971,-0.9));
#80888=CARTESIAN_POINT('Ctrl Pts',(19.1116609796882,-51.2420193552971,-0.9));
#80889=CARTESIAN_POINT('Ctrl Pts',(18.0610456690192,-51.6977493166924,-0.6));
#80890=CARTESIAN_POINT('Ctrl Pts',(18.0610456690192,-51.6977493166924,-0.9));
#80891=CARTESIAN_POINT('Ctrl Pts',(18.2071581110358,-51.4739434123039,-0.6));
#80892=CARTESIAN_POINT('Ctrl Pts',(18.2071581110358,-51.4739434123039,-0.9));
#80893=CARTESIAN_POINT('Ctrl Pts',(18.4877863153815,-51.3579813838005,-0.6));
#80894=CARTESIAN_POINT('Ctrl Pts',(18.4877863153815,-51.3579813838005,-0.9));
#80895=CARTESIAN_POINT('',(18.0610456690192,-51.6977493166924,-0.6));
#80896=CARTESIAN_POINT('Ctrl Pts',(18.0610456690192,-51.6977493166924,-0.6));
#80897=CARTESIAN_POINT('Ctrl Pts',(18.2071581110358,-51.4739434123039,-0.6));
#80898=CARTESIAN_POINT('Ctrl Pts',(18.4877863153815,-51.3579813838005,-0.6));
#80899=CARTESIAN_POINT('',(18.0610456690192,-51.6977493166924,-0.9));
#80900=CARTESIAN_POINT('',(18.0610456690192,-51.6977493166924,-0.6));
#80901=CARTESIAN_POINT('Ctrl Pts',(18.0610456690192,-51.6977493166924,-0.9));
#80902=CARTESIAN_POINT('Ctrl Pts',(18.2071581110358,-51.4739434123039,-0.9));
#80903=CARTESIAN_POINT('Ctrl Pts',(18.4877863153815,-51.3579813838005,-0.9));
#80904=CARTESIAN_POINT('Ctrl Pts',(17.9149332270026,-52.1789906620979,-0.6));
#80905=CARTESIAN_POINT('Ctrl Pts',(17.9149332270026,-52.1789906620979,-0.9));
#80906=CARTESIAN_POINT('Ctrl Pts',(17.9149332270026,-51.9215552210808,-0.6));
#80907=CARTESIAN_POINT('Ctrl Pts',(17.9149332270026,-51.9215552210808,-0.9));
#80908=CARTESIAN_POINT('Ctrl Pts',(18.0610456690192,-51.6977493166924,-0.6));
#80909=CARTESIAN_POINT('Ctrl Pts',(18.0610456690192,-51.6977493166924,-0.9));
#80910=CARTESIAN_POINT('',(17.9149332270026,-52.1789906620979,-0.6));
#80911=CARTESIAN_POINT('Ctrl Pts',(17.9149332270026,-52.1789906620979,-0.6));
#80912=CARTESIAN_POINT('Ctrl Pts',(17.9149332270026,-51.9215552210808,-0.6));
#80913=CARTESIAN_POINT('Ctrl Pts',(18.0610456690192,-51.6977493166924,-0.6));
#80914=CARTESIAN_POINT('',(17.9149332270026,-52.1789906620979,-0.9));
#80915=CARTESIAN_POINT('',(17.9149332270026,-52.1789906620979,-0.6));
#80916=CARTESIAN_POINT('Ctrl Pts',(17.9149332270026,-52.1789906620979,-0.9));
#80917=CARTESIAN_POINT('Ctrl Pts',(17.9149332270026,-51.9215552210808,-0.9));
#80918=CARTESIAN_POINT('Ctrl Pts',(18.0610456690192,-51.6977493166924,-0.9));
#80919=CARTESIAN_POINT('Ctrl Pts',(18.0343809351325,-52.6022509932518,-0.6));
#80920=CARTESIAN_POINT('Ctrl Pts',(18.0343809351325,-52.6022509932518,-0.9));
#80921=CARTESIAN_POINT('Ctrl Pts',(17.9149332270026,-52.4132333397865,-0.6));
#80922=CARTESIAN_POINT('Ctrl Pts',(17.9149332270026,-52.4132333397865,-0.9));
#80923=CARTESIAN_POINT('Ctrl Pts',(17.9149332270026,-52.1789906620979,-0.6));
#80924=CARTESIAN_POINT('Ctrl Pts',(17.9149332270026,-52.1789906620979,-0.9));
#80925=CARTESIAN_POINT('',(18.0343809351325,-52.6022509932518,-0.6));
#80926=CARTESIAN_POINT('Ctrl Pts',(18.0343809351325,-52.6022509932518,-0.6));
#80927=CARTESIAN_POINT('Ctrl Pts',(17.9149332270026,-52.4132333397865,-0.6));
#80928=CARTESIAN_POINT('Ctrl Pts',(17.9149332270026,-52.1789906620979,-0.6));
#80929=CARTESIAN_POINT('',(18.0343809351325,-52.6022509932518,-0.9));
#80930=CARTESIAN_POINT('',(18.0343809351325,-52.6022509932518,-0.6));
#80931=CARTESIAN_POINT('Ctrl Pts',(18.0343809351325,-52.6022509932518,-0.9));
#80932=CARTESIAN_POINT('Ctrl Pts',(17.9149332270026,-52.4132333397865,-0.9));
#80933=CARTESIAN_POINT('Ctrl Pts',(17.9149332270026,-52.1789906620979,-0.9));
#80934=CARTESIAN_POINT('Ctrl Pts',(18.3973398432136,-52.9188267588615,-0.6));
#80935=CARTESIAN_POINT('Ctrl Pts',(18.3973398432136,-52.9188267588615,-0.9));
#80936=CARTESIAN_POINT('Ctrl Pts',(18.1538191065192,-52.7912692427635,-0.6));
#80937=CARTESIAN_POINT('Ctrl Pts',(18.1538191065192,-52.7912692427635,-0.9));
#80938=CARTESIAN_POINT('Ctrl Pts',(18.0343809351325,-52.6022509932518,-0.6));
#80939=CARTESIAN_POINT('Ctrl Pts',(18.0343809351325,-52.6022509932518,-0.9));
#80940=CARTESIAN_POINT('',(18.3973398432136,-52.9188267588615,-0.6));
#80941=CARTESIAN_POINT('Ctrl Pts',(18.3973398432136,-52.9188267588615,-0.6));
#80942=CARTESIAN_POINT('Ctrl Pts',(18.1538191065192,-52.7912692427635,-0.6));
#80943=CARTESIAN_POINT('Ctrl Pts',(18.0343809351325,-52.6022509932518,-0.6));
#80944=CARTESIAN_POINT('',(18.3973398432136,-52.9188267588615,-0.9));
#80945=CARTESIAN_POINT('',(18.3973398432136,-52.9188267588615,-0.6));
#80946=CARTESIAN_POINT('Ctrl Pts',(18.3973398432136,-52.9188267588615,-0.9));
#80947=CARTESIAN_POINT('Ctrl Pts',(18.1538191065192,-52.7912692427635,-0.9));
#80948=CARTESIAN_POINT('Ctrl Pts',(18.0343809351325,-52.6022509932518,-0.9));
#80949=CARTESIAN_POINT('Ctrl Pts',(19.0536775812507,-53.1310371756554,-0.6));
#80950=CARTESIAN_POINT('Ctrl Pts',(19.0536775812507,-53.1310371756554,-0.9));
#80951=CARTESIAN_POINT('Ctrl Pts',(18.5851946100593,-53.018553674221,-0.6));
#80952=CARTESIAN_POINT('Ctrl Pts',(18.5851946100593,-53.018553674221,-0.9));
#80953=CARTESIAN_POINT('Ctrl Pts',(18.3973398432136,-52.9188267588615,-0.6));
#80954=CARTESIAN_POINT('Ctrl Pts',(18.3973398432136,-52.9188267588615,-0.9));
#80955=CARTESIAN_POINT('',(19.0536775812507,-53.1310371756554,-0.6));
#80956=CARTESIAN_POINT('Ctrl Pts',(19.0536775812507,-53.1310371756554,-0.6));
#80957=CARTESIAN_POINT('Ctrl Pts',(18.5851946100593,-53.018553674221,-0.6));
#80958=CARTESIAN_POINT('Ctrl Pts',(18.3973398432136,-52.9188267588615,-0.6));
#80959=CARTESIAN_POINT('',(19.0536775812507,-53.1310371756554,-0.9));
#80960=CARTESIAN_POINT('',(19.0536775812507,-53.1310371756554,-0.6));
#80961=CARTESIAN_POINT('Ctrl Pts',(19.0536775812507,-53.1310371756554,-0.9));
#80962=CARTESIAN_POINT('Ctrl Pts',(18.5851946100593,-53.018553674221,-0.9));
#80963=CARTESIAN_POINT('Ctrl Pts',(18.3973398432136,-52.9188267588615,-0.9));
#80964=CARTESIAN_POINT('Ctrl Pts',(19.6590032801032,-53.2968620657921,-0.6));
#80965=CARTESIAN_POINT('Ctrl Pts',(19.6590032801032,-53.2968620657921,-0.9));
#80966=CARTESIAN_POINT('Ctrl Pts',(19.5221700891852,-53.2435200810432,-0.6));
#80967=CARTESIAN_POINT('Ctrl Pts',(19.5221700891852,-53.2435200810432,-0.9));
#80968=CARTESIAN_POINT('Ctrl Pts',(19.0536775812507,-53.1310371756554,-0.6));
#80969=CARTESIAN_POINT('Ctrl Pts',(19.0536775812507,-53.1310371756554,-0.9));
#80970=CARTESIAN_POINT('',(19.6590032801032,-53.2968620657921,-0.6));
#80971=CARTESIAN_POINT('Ctrl Pts',(19.6590032801032,-53.2968620657921,-0.6));
#80972=CARTESIAN_POINT('Ctrl Pts',(19.5221700891852,-53.2435200810432,-0.6));
#80973=CARTESIAN_POINT('Ctrl Pts',(19.0536775812507,-53.1310371756554,-0.6));
#80974=CARTESIAN_POINT('',(19.6590032801032,-53.2968620657921,-0.9));
#80975=CARTESIAN_POINT('',(19.6590032801032,-53.2968620657921,-0.6));
#80976=CARTESIAN_POINT('Ctrl Pts',(19.6590032801032,-53.2968620657921,-0.9));
#80977=CARTESIAN_POINT('Ctrl Pts',(19.5221700891852,-53.2435200810432,-0.9));
#80978=CARTESIAN_POINT('Ctrl Pts',(19.0536775812507,-53.1310371756554,-0.9));
#80979=CARTESIAN_POINT('Ctrl Pts',(19.9651422724128,-53.4974763989449,-0.6));
#80980=CARTESIAN_POINT('Ctrl Pts',(19.9651422724128,-53.4974763989449,-0.9));
#80981=CARTESIAN_POINT('Ctrl Pts',(19.8723688349128,-53.3780352473259,-0.6));
#80982=CARTESIAN_POINT('Ctrl Pts',(19.8723688349128,-53.3780352473259,-0.9));
#80983=CARTESIAN_POINT('Ctrl Pts',(19.6590032801032,-53.2968620657921,-0.6));
#80984=CARTESIAN_POINT('Ctrl Pts',(19.6590032801032,-53.2968620657921,-0.9));
#80985=CARTESIAN_POINT('',(19.9651422724128,-53.4974763989449,-0.6));
#80986=CARTESIAN_POINT('Ctrl Pts',(19.9651422724128,-53.4974763989449,-0.6));
#80987=CARTESIAN_POINT('Ctrl Pts',(19.8723688349128,-53.3780352473259,-0.6));
#80988=CARTESIAN_POINT('Ctrl Pts',(19.6590032801032,-53.2968620657921,-0.6));
#80989=CARTESIAN_POINT('',(19.9651422724128,-53.4974763989449,-0.9));
#80990=CARTESIAN_POINT('',(19.9651422724128,-53.4974763989449,-0.6));
#80991=CARTESIAN_POINT('Ctrl Pts',(19.9651422724128,-53.4974763989449,-0.9));
#80992=CARTESIAN_POINT('Ctrl Pts',(19.8723688349128,-53.3780352473259,-0.9));
#80993=CARTESIAN_POINT('Ctrl Pts',(19.6590032801032,-53.2968620657921,-0.9));
#80994=CARTESIAN_POINT('Ctrl Pts',(20.0579061731696,-53.7769441008568,-0.6));
#80995=CARTESIAN_POINT('Ctrl Pts',(20.0579061731696,-53.7769441008568,-0.9));
#80996=CARTESIAN_POINT('Ctrl Pts',(20.0579061731696,-53.6169169545174,-0.6));
#80997=CARTESIAN_POINT('Ctrl Pts',(20.0579061731696,-53.6169169545174,-0.9));
#80998=CARTESIAN_POINT('Ctrl Pts',(19.9651422724128,-53.4974763989449,-0.6));
#80999=CARTESIAN_POINT('Ctrl Pts',(19.9651422724128,-53.4974763989449,-0.9));
#81000=CARTESIAN_POINT('',(20.0579061731696,-53.7769441008568,-0.6));
#81001=CARTESIAN_POINT('Ctrl Pts',(20.0579061731696,-53.7769441008568,-0.6));
#81002=CARTESIAN_POINT('Ctrl Pts',(20.0579061731696,-53.6169169545174,-0.6));
#81003=CARTESIAN_POINT('Ctrl Pts',(19.9651422724128,-53.4974763989449,-0.6));
#81004=CARTESIAN_POINT('',(20.0579061731696,-53.7769441008568,-0.9));
#81005=CARTESIAN_POINT('',(20.0579061731696,-53.7769441008568,-0.6));
#81006=CARTESIAN_POINT('Ctrl Pts',(20.0579061731696,-53.7769441008568,-0.9));
#81007=CARTESIAN_POINT('Ctrl Pts',(20.0579061731696,-53.6169169545174,-0.9));
#81008=CARTESIAN_POINT('Ctrl Pts',(19.9651422724128,-53.4974763989449,-0.9));
#81009=CARTESIAN_POINT('Ctrl Pts',(19.9616613611579,-54.0680084824562,-0.6));
#81010=CARTESIAN_POINT('Ctrl Pts',(19.9616613611579,-54.0680084824562,-0.9));
#81011=CARTESIAN_POINT('Ctrl Pts',(20.0579061731696,-53.934652030468,-0.6));
#81012=CARTESIAN_POINT('Ctrl Pts',(20.0579061731696,-53.934652030468,-0.9));
#81013=CARTESIAN_POINT('Ctrl Pts',(20.0579061731696,-53.7769441008568,-0.6));
#81014=CARTESIAN_POINT('Ctrl Pts',(20.0579061731696,-53.7769441008568,-0.9));
#81015=CARTESIAN_POINT('',(19.9616613611579,-54.0680084824562,-0.6));
#81016=CARTESIAN_POINT('Ctrl Pts',(19.9616613611579,-54.0680084824562,-0.6));
#81017=CARTESIAN_POINT('Ctrl Pts',(20.0579061731696,-53.934652030468,-0.6));
#81018=CARTESIAN_POINT('Ctrl Pts',(20.0579061731696,-53.7769441008568,-0.6));
#81019=CARTESIAN_POINT('',(19.9616613611579,-54.0680084824562,-0.9));
#81020=CARTESIAN_POINT('',(19.9616613611579,-54.0680084824562,-0.6));
#81021=CARTESIAN_POINT('Ctrl Pts',(19.9616613611579,-54.0680084824562,-0.9));
#81022=CARTESIAN_POINT('Ctrl Pts',(20.0579061731696,-53.934652030468,-0.9));
#81023=CARTESIAN_POINT('Ctrl Pts',(20.0579061731696,-53.7769441008568,-0.9));
#81024=CARTESIAN_POINT('Ctrl Pts',(19.6682825312018,-54.2778990864754,-0.6));
#81025=CARTESIAN_POINT('Ctrl Pts',(19.6682825312018,-54.2778990864754,-0.9));
#81026=CARTESIAN_POINT('Ctrl Pts',(19.8654165491462,-54.201364338398,-0.6));
#81027=CARTESIAN_POINT('Ctrl Pts',(19.8654165491462,-54.201364338398,-0.9));
#81028=CARTESIAN_POINT('Ctrl Pts',(19.9616613611579,-54.0680084824562,-0.6));
#81029=CARTESIAN_POINT('Ctrl Pts',(19.9616613611579,-54.0680084824562,-0.9));
#81030=CARTESIAN_POINT('',(19.6682825312018,-54.2778990864754,-0.6));
#81031=CARTESIAN_POINT('Ctrl Pts',(19.6682825312018,-54.2778990864754,-0.6));
#81032=CARTESIAN_POINT('Ctrl Pts',(19.8654165491462,-54.201364338398,-0.6));
#81033=CARTESIAN_POINT('Ctrl Pts',(19.9616613611579,-54.0680084824562,-0.6));
#81034=CARTESIAN_POINT('',(19.6682825312018,-54.2778990864754,-0.9));
#81035=CARTESIAN_POINT('',(19.6682825312018,-54.2778990864754,-0.6));
#81036=CARTESIAN_POINT('Ctrl Pts',(19.6682825312018,-54.2778990864754,-0.9));
#81037=CARTESIAN_POINT('Ctrl Pts',(19.8654165491462,-54.201364338398,-0.9));
#81038=CARTESIAN_POINT('Ctrl Pts',(19.9616613611579,-54.0680084824562,-0.9));
#81039=CARTESIAN_POINT('Ctrl Pts',(19.2137041315436,-54.3544338345528,-0.6));
#81040=CARTESIAN_POINT('Ctrl Pts',(19.2137041315436,-54.3544338345528,-0.9));
#81041=CARTESIAN_POINT('Ctrl Pts',(19.4711485132575,-54.3544338345528,-0.6));
#81042=CARTESIAN_POINT('Ctrl Pts',(19.4711485132575,-54.3544338345528,-0.9));
#81043=CARTESIAN_POINT('Ctrl Pts',(19.6682825312018,-54.2778990864754,-0.6));
#81044=CARTESIAN_POINT('Ctrl Pts',(19.6682825312018,-54.2778990864754,-0.9));
#81045=CARTESIAN_POINT('',(19.2137041315436,-54.3544338345528,-0.6));
#81046=CARTESIAN_POINT('Ctrl Pts',(19.2137041315436,-54.3544338345528,-0.6));
#81047=CARTESIAN_POINT('Ctrl Pts',(19.4711485132575,-54.3544338345528,-0.6));
#81048=CARTESIAN_POINT('Ctrl Pts',(19.6682825312018,-54.2778990864754,-0.6));
#81049=CARTESIAN_POINT('',(19.2137041315436,-54.3544338345528,-0.9));
#81050=CARTESIAN_POINT('',(19.2137041315436,-54.3544338345528,-0.6));
#81051=CARTESIAN_POINT('Ctrl Pts',(19.2137041315436,-54.3544338345528,-0.9));
#81052=CARTESIAN_POINT('Ctrl Pts',(19.4711485132575,-54.3544338345528,-0.9));
#81053=CARTESIAN_POINT('Ctrl Pts',(19.6682825312018,-54.2778990864754,-0.9));
#81054=CARTESIAN_POINT('Ctrl Pts',(18.6918821558356,-54.2535470128059,-0.6));
#81055=CARTESIAN_POINT('Ctrl Pts',(18.6918821558356,-54.2535470128059,-0.9));
#81056=CARTESIAN_POINT('Ctrl Pts',(18.9238062128425,-54.3544338345528,-0.6));
#81057=CARTESIAN_POINT('Ctrl Pts',(18.9238062128425,-54.3544338345528,-0.9));
#81058=CARTESIAN_POINT('Ctrl Pts',(19.2137041315436,-54.3544338345528,-0.6));
#81059=CARTESIAN_POINT('Ctrl Pts',(19.2137041315436,-54.3544338345528,-0.9));
#81060=CARTESIAN_POINT('',(18.6918821558356,-54.2535470128059,-0.6));
#81061=CARTESIAN_POINT('Ctrl Pts',(18.6918821558356,-54.2535470128059,-0.6));
#81062=CARTESIAN_POINT('Ctrl Pts',(18.9238062128425,-54.3544338345528,-0.6));
#81063=CARTESIAN_POINT('Ctrl Pts',(19.2137041315436,-54.3544338345528,-0.6));
#81064=CARTESIAN_POINT('',(18.6918821558356,-54.2535470128059,-0.9));
#81065=CARTESIAN_POINT('',(18.6918821558356,-54.2535470128059,-0.6));
#81066=CARTESIAN_POINT('Ctrl Pts',(18.6918821558356,-54.2535470128059,-0.9));
#81067=CARTESIAN_POINT('Ctrl Pts',(18.9238062128425,-54.3544338345528,-0.9));
#81068=CARTESIAN_POINT('Ctrl Pts',(19.2137041315436,-54.3544338345528,-0.9));
#81069=CARTESIAN_POINT('Ctrl Pts',(18.3497896417975,-53.9891545176506,-0.6));
#81070=CARTESIAN_POINT('Ctrl Pts',(18.3497896417975,-53.9891545176506,-0.9));
#81071=CARTESIAN_POINT('Ctrl Pts',(18.4599580988288,-54.1526601910591,-0.6));
#81072=CARTESIAN_POINT('Ctrl Pts',(18.4599580988288,-54.1526601910591,-0.9));
#81073=CARTESIAN_POINT('Ctrl Pts',(18.6918821558356,-54.2535470128059,-0.6));
#81074=CARTESIAN_POINT('Ctrl Pts',(18.6918821558356,-54.2535470128059,-0.9));
#81075=CARTESIAN_POINT('',(18.3497896417975,-53.9891545176506,-0.6));
#81076=CARTESIAN_POINT('Ctrl Pts',(18.3497896417975,-53.9891545176506,-0.6));
#81077=CARTESIAN_POINT('Ctrl Pts',(18.4599580988288,-54.1526601910591,-0.6));
#81078=CARTESIAN_POINT('Ctrl Pts',(18.6918821558356,-54.2535470128059,-0.6));
#81079=CARTESIAN_POINT('',(18.3497896417975,-53.9891545176506,-0.9));
#81080=CARTESIAN_POINT('',(18.3497896417975,-53.9891545176506,-0.6));
#81081=CARTESIAN_POINT('Ctrl Pts',(18.3497896417975,-53.9891545176506,-0.9));
#81082=CARTESIAN_POINT('Ctrl Pts',(18.4599580988288,-54.1526601910591,-0.9));
#81083=CARTESIAN_POINT('Ctrl Pts',(18.6918821558356,-54.2535470128059,-0.9));
#81084=CARTESIAN_POINT('Ctrl Pts',(18.2094755396247,-53.5705320239067,-0.6));
#81085=CARTESIAN_POINT('Ctrl Pts',(18.2094755396247,-53.5705320239067,-0.9));
#81086=CARTESIAN_POINT('Ctrl Pts',(18.2396307215095,-53.8256482481956,-0.6));
#81087=CARTESIAN_POINT('Ctrl Pts',(18.2396307215095,-53.8256482481956,-0.9));
#81088=CARTESIAN_POINT('Ctrl Pts',(18.3497896417975,-53.9891545176506,-0.6));
#81089=CARTESIAN_POINT('Ctrl Pts',(18.3497896417975,-53.9891545176506,-0.9));
#81090=CARTESIAN_POINT('',(18.2094755396247,-53.5705320239067,-0.6));
#81091=CARTESIAN_POINT('Ctrl Pts',(18.2094755396247,-53.5705320239067,-0.6));
#81092=CARTESIAN_POINT('Ctrl Pts',(18.2396307215095,-53.8256482481956,-0.6));
#81093=CARTESIAN_POINT('Ctrl Pts',(18.3497896417975,-53.9891545176506,-0.6));
#81094=CARTESIAN_POINT('',(18.2094755396247,-53.5705320239067,-0.9));
#81095=CARTESIAN_POINT('',(18.2094755396247,-53.5705320239067,-0.6));
#81096=CARTESIAN_POINT('Ctrl Pts',(18.2094755396247,-53.5705320239067,-0.9));
#81097=CARTESIAN_POINT('Ctrl Pts',(18.2396307215095,-53.8256482481956,-0.9));
#81098=CARTESIAN_POINT('Ctrl Pts',(18.3497896417975,-53.9891545176506,-0.9));
#81099=CARTESIAN_POINT('Origin',(17.7850618585944,-53.6076400876045,-0.6));
#81100=CARTESIAN_POINT('',(17.7850618585944,-53.6076400876045,-0.6));
#81101=CARTESIAN_POINT('',(8.98635809002947,-54.3769434218173,-0.6));
#81102=CARTESIAN_POINT('',(17.7850618585944,-53.6076400876045,-0.9));
#81103=CARTESIAN_POINT('',(17.7850618585944,-53.6076400876045,-0.6));
#81104=CARTESIAN_POINT('',(17.7850618585944,-53.6076400876045,-0.9));
#81105=CARTESIAN_POINT('Ctrl Pts',(17.9717626795173,-54.2187587618828,-0.6));
#81106=CARTESIAN_POINT('Ctrl Pts',(17.9717626795173,-54.2187587618828,-0.9));
#81107=CARTESIAN_POINT('Ctrl Pts',(17.7943411096931,-53.9485673308372,-0.6));
#81108=CARTESIAN_POINT('Ctrl Pts',(17.7943411096931,-53.9485673308372,-0.9));
#81109=CARTESIAN_POINT('Ctrl Pts',(17.7850618585944,-53.6076400876045,-0.6));
#81110=CARTESIAN_POINT('Ctrl Pts',(17.7850618585944,-53.6076400876045,-0.9));
#81111=CARTESIAN_POINT('',(17.9717626795173,-54.2187587618828,-0.6));
#81112=CARTESIAN_POINT('Ctrl Pts',(17.9717626795173,-54.2187587618828,-0.6));
#81113=CARTESIAN_POINT('Ctrl Pts',(17.7943411096931,-53.9485673308372,-0.6));
#81114=CARTESIAN_POINT('Ctrl Pts',(17.7850618585944,-53.6076400876045,-0.6));
#81115=CARTESIAN_POINT('',(17.9717626795173,-54.2187587618828,-0.9));
#81116=CARTESIAN_POINT('',(17.9717626795173,-54.2187587618828,-0.6));
#81117=CARTESIAN_POINT('Ctrl Pts',(17.9717626795173,-54.2187587618828,-0.9));
#81118=CARTESIAN_POINT('Ctrl Pts',(17.7943411096931,-53.9485673308372,-0.9));
#81119=CARTESIAN_POINT('Ctrl Pts',(17.7850618585944,-53.6076400876045,-0.9));
#81120=CARTESIAN_POINT('Ctrl Pts',(18.4611120447516,-54.623465359211,-0.6));
#81121=CARTESIAN_POINT('Ctrl Pts',(18.4611120447516,-54.623465359211,-0.9));
#81122=CARTESIAN_POINT('Ctrl Pts',(18.1491842493415,-54.4889495968819,-0.6));
#81123=CARTESIAN_POINT('Ctrl Pts',(18.1491842493415,-54.4889495968819,-0.9));
#81124=CARTESIAN_POINT('Ctrl Pts',(17.9717626795173,-54.2187587618828,-0.6));
#81125=CARTESIAN_POINT('Ctrl Pts',(17.9717626795173,-54.2187587618828,-0.9));
#81126=CARTESIAN_POINT('Ctrl Pts',(18.4611120447516,-54.623465359211,-0.6));
#81127=CARTESIAN_POINT('Ctrl Pts',(18.1491842493415,-54.4889495968819,-0.6));
#81128=CARTESIAN_POINT('Ctrl Pts',(17.9717626795173,-54.2187587618828,-0.6));
#81129=CARTESIAN_POINT('Ctrl Pts',(18.4611120447516,-54.623465359211,-0.9));
#81130=CARTESIAN_POINT('Ctrl Pts',(18.1491842493415,-54.4889495968819,-0.9));
#81131=CARTESIAN_POINT('Ctrl Pts',(17.9717626795173,-54.2187587618828,-0.9));
#81132=CARTESIAN_POINT('Origin',(19.1383352503181,-53.0000002384186,-0.9));
#81133=CARTESIAN_POINT('Ctrl Pts',(10.8737364038825,-54.212960422039,-0.6));
#81134=CARTESIAN_POINT('Ctrl Pts',(10.8737364038825,-54.212960422039,-0.9));
#81135=CARTESIAN_POINT('Ctrl Pts',(11.1404504999518,-54.3729875683784,-0.6));
#81136=CARTESIAN_POINT('Ctrl Pts',(11.1404504999518,-54.3729875683784,-0.9));
#81137=CARTESIAN_POINT('Ctrl Pts',(11.4512243494391,-54.3729875683784,-0.6));
#81138=CARTESIAN_POINT('Ctrl Pts',(11.4512243494391,-54.3729875683784,-0.9));
#81139=CARTESIAN_POINT('',(10.8737364038825,-54.212960422039,-0.6));
#81140=CARTESIAN_POINT('',(11.4512243494391,-54.3729875683784,-0.6));
#81141=CARTESIAN_POINT('Ctrl Pts',(10.8737364038825,-54.212960422039,-0.6));
#81142=CARTESIAN_POINT('Ctrl Pts',(11.1404504999518,-54.3729875683784,-0.6));
#81143=CARTESIAN_POINT('Ctrl Pts',(11.4512243494391,-54.3729875683784,-0.6));
#81144=CARTESIAN_POINT('',(10.8737364038825,-54.212960422039,-0.9));
#81145=CARTESIAN_POINT('',(10.8737364038825,-54.212960422039,-0.6));
#81146=CARTESIAN_POINT('',(11.4512243494391,-54.3729875683784,-0.9));
#81147=CARTESIAN_POINT('Ctrl Pts',(10.8737364038825,-54.212960422039,-0.9));
#81148=CARTESIAN_POINT('Ctrl Pts',(11.1404504999518,-54.3729875683784,-0.9));
#81149=CARTESIAN_POINT('Ctrl Pts',(11.4512243494391,-54.3729875683784,-0.9));
#81150=CARTESIAN_POINT('',(11.4512243494391,-54.3729875683784,-0.6));
#81151=CARTESIAN_POINT('Ctrl Pts',(10.4806223139167,-53.7293998599052,-0.6));
#81152=CARTESIAN_POINT('Ctrl Pts',(10.4806223139167,-53.7293998599052,-0.9));
#81153=CARTESIAN_POINT('Ctrl Pts',(10.6070223078132,-54.0529332756996,-0.6));
#81154=CARTESIAN_POINT('Ctrl Pts',(10.6070223078132,-54.0529332756996,-0.9));
#81155=CARTESIAN_POINT('Ctrl Pts',(10.8737364038825,-54.212960422039,-0.6));
#81156=CARTESIAN_POINT('Ctrl Pts',(10.8737364038825,-54.212960422039,-0.9));
#81157=CARTESIAN_POINT('',(10.4806223139167,-53.7293998599052,-0.6));
#81158=CARTESIAN_POINT('Ctrl Pts',(10.4806223139167,-53.7293998599052,-0.6));
#81159=CARTESIAN_POINT('Ctrl Pts',(10.6070223078132,-54.0529332756996,-0.6));
#81160=CARTESIAN_POINT('Ctrl Pts',(10.8737364038825,-54.212960422039,-0.6));
#81161=CARTESIAN_POINT('',(10.4806223139167,-53.7293998599052,-0.9));
#81162=CARTESIAN_POINT('',(10.4806223139167,-53.7293998599052,-0.6));
#81163=CARTESIAN_POINT('Ctrl Pts',(10.4806223139167,-53.7293998599052,-0.9));
#81164=CARTESIAN_POINT('Ctrl Pts',(10.6070223078132,-54.0529332756996,-0.9));
#81165=CARTESIAN_POINT('Ctrl Pts',(10.8737364038825,-54.212960422039,-0.9));
#81166=CARTESIAN_POINT('Ctrl Pts',(10.3542318567634,-52.9721693396568,-0.6));
#81167=CARTESIAN_POINT('Ctrl Pts',(10.3542318567634,-52.9721693396568,-0.9));
#81168=CARTESIAN_POINT('Ctrl Pts',(10.3542318567634,-53.4058664441109,-0.6));
#81169=CARTESIAN_POINT('Ctrl Pts',(10.3542318567634,-53.4058664441109,-0.9));
#81170=CARTESIAN_POINT('Ctrl Pts',(10.4806223139167,-53.7293998599052,-0.6));
#81171=CARTESIAN_POINT('Ctrl Pts',(10.4806223139167,-53.7293998599052,-0.9));
#81172=CARTESIAN_POINT('',(10.3542318567634,-52.9721693396568,-0.6));
#81173=CARTESIAN_POINT('Ctrl Pts',(10.3542318567634,-52.9721693396568,-0.6));
#81174=CARTESIAN_POINT('Ctrl Pts',(10.3542318567634,-53.4058664441109,-0.6));
#81175=CARTESIAN_POINT('Ctrl Pts',(10.4806223139167,-53.7293998599052,-0.6));
#81176=CARTESIAN_POINT('',(10.3542318567634,-52.9721693396568,-0.9));
#81177=CARTESIAN_POINT('',(10.3542318567634,-52.9721693396568,-0.6));
#81178=CARTESIAN_POINT('Ctrl Pts',(10.3542318567634,-52.9721693396568,-0.9));
#81179=CARTESIAN_POINT('Ctrl Pts',(10.3542318567634,-53.4058664441109,-0.9));
#81180=CARTESIAN_POINT('Ctrl Pts',(10.4806223139167,-53.7293998599052,-0.9));
#81181=CARTESIAN_POINT('Ctrl Pts',(10.4609098657966,-52.3193041682243,-0.6));
#81182=CARTESIAN_POINT('Ctrl Pts',(10.4609098657966,-52.3193041682243,-0.9));
#81183=CARTESIAN_POINT('Ctrl Pts',(10.3542318567634,-52.6358799338341,-0.6));
#81184=CARTESIAN_POINT('Ctrl Pts',(10.3542318567634,-52.6358799338341,-0.9));
#81185=CARTESIAN_POINT('Ctrl Pts',(10.3542318567634,-52.9721693396568,-0.6));
#81186=CARTESIAN_POINT('Ctrl Pts',(10.3542318567634,-52.9721693396568,-0.9));
#81187=CARTESIAN_POINT('',(10.4609098657966,-52.3193041682243,-0.6));
#81188=CARTESIAN_POINT('Ctrl Pts',(10.4609098657966,-52.3193041682243,-0.6));
#81189=CARTESIAN_POINT('Ctrl Pts',(10.3542318567634,-52.6358799338341,-0.6));
#81190=CARTESIAN_POINT('Ctrl Pts',(10.3542318567634,-52.9721693396568,-0.6));
#81191=CARTESIAN_POINT('',(10.4609098657966,-52.3193041682243,-0.9));
#81192=CARTESIAN_POINT('',(10.4609098657966,-52.3193041682243,-0.6));
#81193=CARTESIAN_POINT('Ctrl Pts',(10.4609098657966,-52.3193041682243,-0.9));
#81194=CARTESIAN_POINT('Ctrl Pts',(10.3542318567634,-52.6358799338341,-0.9));
#81195=CARTESIAN_POINT('Ctrl Pts',(10.3542318567634,-52.9721693396568,-0.9));
#81196=CARTESIAN_POINT('Ctrl Pts',(10.8308305963874,-51.8148706555367,-0.6));
#81197=CARTESIAN_POINT('Ctrl Pts',(10.8308305963874,-51.8148706555367,-0.9));
#81198=CARTESIAN_POINT('Ctrl Pts',(10.5675974115729,-52.0027284026146,-0.6));
#81199=CARTESIAN_POINT('Ctrl Pts',(10.5675974115729,-52.0027284026146,-0.9));
#81200=CARTESIAN_POINT('Ctrl Pts',(10.4609098657966,-52.3193041682243,-0.6));
#81201=CARTESIAN_POINT('Ctrl Pts',(10.4609098657966,-52.3193041682243,-0.9));
#81202=CARTESIAN_POINT('',(10.8308305963874,-51.8148706555367,-0.6));
#81203=CARTESIAN_POINT('Ctrl Pts',(10.8308305963874,-51.8148706555367,-0.6));
#81204=CARTESIAN_POINT('Ctrl Pts',(10.5675974115729,-52.0027284026146,-0.6));
#81205=CARTESIAN_POINT('Ctrl Pts',(10.4609098657966,-52.3193041682243,-0.6));
#81206=CARTESIAN_POINT('',(10.8308305963874,-51.8148706555367,-0.9));
#81207=CARTESIAN_POINT('',(10.8308305963874,-51.8148706555367,-0.6));
#81208=CARTESIAN_POINT('Ctrl Pts',(10.8308305963874,-51.8148706555367,-0.9));
#81209=CARTESIAN_POINT('Ctrl Pts',(10.5675974115729,-52.0027284026146,-0.9));
#81210=CARTESIAN_POINT('Ctrl Pts',(10.4609098657966,-52.3193041682243,-0.9));
#81211=CARTESIAN_POINT('Ctrl Pts',(11.4860143885016,-51.6270129084587,-0.6));
#81212=CARTESIAN_POINT('Ctrl Pts',(11.4860143885016,-51.6270129084587,-0.9));
#81213=CARTESIAN_POINT('Ctrl Pts',(11.0940637812018,-51.6270129084587,-0.6));
#81214=CARTESIAN_POINT('Ctrl Pts',(11.0940637812018,-51.6270129084587,-0.9));
#81215=CARTESIAN_POINT('Ctrl Pts',(10.8308305963874,-51.8148706555367,-0.6));
#81216=CARTESIAN_POINT('Ctrl Pts',(10.8308305963874,-51.8148706555367,-0.9));
#81217=CARTESIAN_POINT('',(11.4860143885016,-51.6270129084587,-0.6));
#81218=CARTESIAN_POINT('Ctrl Pts',(11.4860143885016,-51.6270129084587,-0.6));
#81219=CARTESIAN_POINT('Ctrl Pts',(11.0940637812018,-51.6270129084587,-0.6));
#81220=CARTESIAN_POINT('Ctrl Pts',(10.8308305963874,-51.8148706555367,-0.6));
#81221=CARTESIAN_POINT('',(11.4860143885016,-51.6270129084587,-0.9));
#81222=CARTESIAN_POINT('',(11.4860143885016,-51.6270129084587,-0.6));
#81223=CARTESIAN_POINT('Ctrl Pts',(11.4860143885016,-51.6270129084587,-0.9));
#81224=CARTESIAN_POINT('Ctrl Pts',(11.0940637812018,-51.6270129084587,-0.9));
#81225=CARTESIAN_POINT('Ctrl Pts',(10.8308305963874,-51.8148706555367,-0.9));
#81226=CARTESIAN_POINT('Ctrl Pts',(12.0519056543708,-51.796316921711,-0.6));
#81227=CARTESIAN_POINT('Ctrl Pts',(12.0519056543708,-51.796316921711,-0.9));
#81228=CARTESIAN_POINT('Ctrl Pts',(11.8269434198737,-51.6270129084587,-0.6));
#81229=CARTESIAN_POINT('Ctrl Pts',(11.8269434198737,-51.6270129084587,-0.9));
#81230=CARTESIAN_POINT('Ctrl Pts',(11.4860143885016,-51.6270129084587,-0.6));
#81231=CARTESIAN_POINT('Ctrl Pts',(11.4860143885016,-51.6270129084587,-0.9));
#81232=CARTESIAN_POINT('',(12.0519056543708,-51.796316921711,-0.6));
#81233=CARTESIAN_POINT('Ctrl Pts',(12.0519056543708,-51.796316921711,-0.6));
#81234=CARTESIAN_POINT('Ctrl Pts',(11.8269434198737,-51.6270129084587,-0.6));
#81235=CARTESIAN_POINT('Ctrl Pts',(11.4860143885016,-51.6270129084587,-0.6));
#81236=CARTESIAN_POINT('',(12.0519056543708,-51.796316921711,-0.9));
#81237=CARTESIAN_POINT('',(12.0519056543708,-51.796316921711,-0.6));
#81238=CARTESIAN_POINT('Ctrl Pts',(12.0519056543708,-51.796316921711,-0.9));
#81239=CARTESIAN_POINT('Ctrl Pts',(11.8269434198737,-51.6270129084587,-0.9));
#81240=CARTESIAN_POINT('Ctrl Pts',(11.4860143885016,-51.6270129084587,-0.9));
#81241=CARTESIAN_POINT('Ctrl Pts',(12.3951521143317,-52.3366985917091,-0.6));
#81242=CARTESIAN_POINT('Ctrl Pts',(12.3951521143317,-52.3366985917091,-0.9));
#81243=CARTESIAN_POINT('Ctrl Pts',(12.276877425611,-51.9656209349632,-0.6));
#81244=CARTESIAN_POINT('Ctrl Pts',(12.276877425611,-51.9656209349632,-0.9));
#81245=CARTESIAN_POINT('Ctrl Pts',(12.0519056543708,-51.796316921711,-0.6));
#81246=CARTESIAN_POINT('Ctrl Pts',(12.0519056543708,-51.796316921711,-0.9));
#81247=CARTESIAN_POINT('',(12.3951521143317,-52.3366985917091,-0.6));
#81248=CARTESIAN_POINT('Ctrl Pts',(12.3951521143317,-52.3366985917091,-0.6));
#81249=CARTESIAN_POINT('Ctrl Pts',(12.276877425611,-51.9656209349632,-0.6));
#81250=CARTESIAN_POINT('Ctrl Pts',(12.0519056543708,-51.796316921711,-0.6));
#81251=CARTESIAN_POINT('',(12.3951521143317,-52.3366985917091,-0.9));
#81252=CARTESIAN_POINT('',(12.3951521143317,-52.3366985917091,-0.6));
#81253=CARTESIAN_POINT('Ctrl Pts',(12.3951521143317,-52.3366985917091,-0.9));
#81254=CARTESIAN_POINT('Ctrl Pts',(12.276877425611,-51.9656209349632,-0.9));
#81255=CARTESIAN_POINT('Ctrl Pts',(12.0519056543708,-51.796316921711,-0.9));
#81256=CARTESIAN_POINT('Origin',(12.8381338343024,-52.2323332428932,-0.6));
#81257=CARTESIAN_POINT('',(12.8381338343024,-52.2323332428932,-0.6));
#81258=CARTESIAN_POINT('',(6.67095317451304,-53.685305073903,-0.6));
#81259=CARTESIAN_POINT('',(12.8381338343024,-52.2323332428932,-0.9));
#81260=CARTESIAN_POINT('',(12.8381338343024,-52.2323332428932,-0.6));
#81261=CARTESIAN_POINT('',(12.8381338343024,-52.2323332428932,-0.9));
#81262=CARTESIAN_POINT('Ctrl Pts',(12.3534097895026,-51.5017740130424,-0.6));
#81263=CARTESIAN_POINT('Ctrl Pts',(12.3534097895026,-51.5017740130424,-0.9));
#81264=CARTESIAN_POINT('Ctrl Pts',(12.7012911066413,-51.7615286707878,-0.6));
#81265=CARTESIAN_POINT('Ctrl Pts',(12.7012911066413,-51.7615286707878,-0.9));
#81266=CARTESIAN_POINT('Ctrl Pts',(12.8381338343024,-52.2323332428932,-0.6));
#81267=CARTESIAN_POINT('Ctrl Pts',(12.8381338343024,-52.2323332428932,-0.9));
#81268=CARTESIAN_POINT('',(12.3534097895026,-51.5017740130424,-0.6));
#81269=CARTESIAN_POINT('Ctrl Pts',(12.3534097895026,-51.5017740130424,-0.6));
#81270=CARTESIAN_POINT('Ctrl Pts',(12.7012911066413,-51.7615286707878,-0.6));
#81271=CARTESIAN_POINT('Ctrl Pts',(12.8381338343024,-52.2323332428932,-0.6));
#81272=CARTESIAN_POINT('',(12.3534097895026,-51.5017740130424,-0.9));
#81273=CARTESIAN_POINT('',(12.3534097895026,-51.5017740130424,-0.6));
#81274=CARTESIAN_POINT('Ctrl Pts',(12.3534097895026,-51.5017740130424,-0.9));
#81275=CARTESIAN_POINT('Ctrl Pts',(12.7012911066413,-51.7615286707878,-0.9));
#81276=CARTESIAN_POINT('Ctrl Pts',(12.8381338343024,-52.2323332428932,-0.9));
#81277=CARTESIAN_POINT('Ctrl Pts',(11.4952936396003,-51.2420193552971,-0.6));
#81278=CARTESIAN_POINT('Ctrl Pts',(11.4952936396003,-51.2420193552971,-0.9));
#81279=CARTESIAN_POINT('Ctrl Pts',(12.0055284723639,-51.2420193552971,-0.6));
#81280=CARTESIAN_POINT('Ctrl Pts',(12.0055284723639,-51.2420193552971,-0.9));
#81281=CARTESIAN_POINT('Ctrl Pts',(12.3534097895026,-51.5017740130424,-0.6));
#81282=CARTESIAN_POINT('Ctrl Pts',(12.3534097895026,-51.5017740130424,-0.9));
#81283=CARTESIAN_POINT('',(11.4952936396003,-51.2420193552971,-0.6));
#81284=CARTESIAN_POINT('Ctrl Pts',(11.4952936396003,-51.2420193552971,-0.6));
#81285=CARTESIAN_POINT('Ctrl Pts',(12.0055284723639,-51.2420193552971,-0.6));
#81286=CARTESIAN_POINT('Ctrl Pts',(12.3534097895026,-51.5017740130424,-0.6));
#81287=CARTESIAN_POINT('',(11.4952936396003,-51.2420193552971,-0.9));
#81288=CARTESIAN_POINT('',(11.4952936396003,-51.2420193552971,-0.6));
#81289=CARTESIAN_POINT('Ctrl Pts',(11.4952936396003,-51.2420193552971,-0.9));
#81290=CARTESIAN_POINT('Ctrl Pts',(12.0055284723639,-51.2420193552971,-0.9));
#81291=CARTESIAN_POINT('Ctrl Pts',(12.3534097895026,-51.5017740130424,-0.9));
#81292=CARTESIAN_POINT('Ctrl Pts',(10.6708040460944,-51.4472715258598,-0.6));
#81293=CARTESIAN_POINT('Ctrl Pts',(10.6708040460944,-51.4472715258598,-0.9));
#81294=CARTESIAN_POINT('Ctrl Pts',(11.045359633863,-51.2420193552971,-0.6));
#81295=CARTESIAN_POINT('Ctrl Pts',(11.045359633863,-51.2420193552971,-0.9));
#81296=CARTESIAN_POINT('Ctrl Pts',(11.4952936396003,-51.2420193552971,-0.6));
#81297=CARTESIAN_POINT('Ctrl Pts',(11.4952936396003,-51.2420193552971,-0.9));
#81298=CARTESIAN_POINT('',(10.6708040460944,-51.4472715258598,-0.6));
#81299=CARTESIAN_POINT('Ctrl Pts',(10.6708040460944,-51.4472715258598,-0.6));
#81300=CARTESIAN_POINT('Ctrl Pts',(11.045359633863,-51.2420193552971,-0.6));
#81301=CARTESIAN_POINT('Ctrl Pts',(11.4952936396003,-51.2420193552971,-0.6));
#81302=CARTESIAN_POINT('',(10.6708040460944,-51.4472715258598,-0.9));
#81303=CARTESIAN_POINT('',(10.6708040460944,-51.4472715258598,-0.6));
#81304=CARTESIAN_POINT('Ctrl Pts',(10.6708040460944,-51.4472715258598,-0.9));
#81305=CARTESIAN_POINT('Ctrl Pts',(11.045359633863,-51.2420193552971,-0.9));
#81306=CARTESIAN_POINT('Ctrl Pts',(11.4952936396003,-51.2420193552971,-0.9));
#81307=CARTESIAN_POINT('Ctrl Pts',(10.0933161005378,-52.0479540228844,-0.6));
#81308=CARTESIAN_POINT('Ctrl Pts',(10.0933161005378,-52.0479540228844,-0.9));
#81309=CARTESIAN_POINT('Ctrl Pts',(10.2962484583259,-51.652524292469,-0.6));
#81310=CARTESIAN_POINT('Ctrl Pts',(10.2962484583259,-51.652524292469,-0.9));
#81311=CARTESIAN_POINT('Ctrl Pts',(10.6708040460944,-51.4472715258598,-0.6));
#81312=CARTESIAN_POINT('Ctrl Pts',(10.6708040460944,-51.4472715258598,-0.9));
#81313=CARTESIAN_POINT('',(10.0933161005378,-52.0479540228844,-0.6));
#81314=CARTESIAN_POINT('Ctrl Pts',(10.0933161005378,-52.0479540228844,-0.6));
#81315=CARTESIAN_POINT('Ctrl Pts',(10.2962484583259,-51.652524292469,-0.6));
#81316=CARTESIAN_POINT('Ctrl Pts',(10.6708040460944,-51.4472715258598,-0.6));
#81317=CARTESIAN_POINT('',(10.0933161005378,-52.0479540228844,-0.9));
#81318=CARTESIAN_POINT('',(10.0933161005378,-52.0479540228844,-0.6));
#81319=CARTESIAN_POINT('Ctrl Pts',(10.0933161005378,-52.0479540228844,-0.9));
#81320=CARTESIAN_POINT('Ctrl Pts',(10.2962484583259,-51.652524292469,-0.9));
#81321=CARTESIAN_POINT('Ctrl Pts',(10.6708040460944,-51.4472715258598,-0.9));
#81322=CARTESIAN_POINT('Ctrl Pts',(9.89038374274969,-52.974488556385,-0.6));
#81323=CARTESIAN_POINT('Ctrl Pts',(9.89038374274969,-52.974488556385,-0.9));
#81324=CARTESIAN_POINT('Ctrl Pts',(9.89038374274969,-52.4433831572533,-0.6));
#81325=CARTESIAN_POINT('Ctrl Pts',(9.89038374274969,-52.4433831572533,-0.9));
#81326=CARTESIAN_POINT('Ctrl Pts',(10.0933161005378,-52.0479540228844,-0.6));
#81327=CARTESIAN_POINT('Ctrl Pts',(10.0933161005378,-52.0479540228844,-0.9));
#81328=CARTESIAN_POINT('',(9.89038374274969,-52.974488556385,-0.6));
#81329=CARTESIAN_POINT('Ctrl Pts',(9.89038374274969,-52.974488556385,-0.6));
#81330=CARTESIAN_POINT('Ctrl Pts',(9.89038374274969,-52.4433831572533,-0.6));
#81331=CARTESIAN_POINT('Ctrl Pts',(10.0933161005378,-52.0479540228844,-0.6));
#81332=CARTESIAN_POINT('',(9.89038374274969,-52.974488556385,-0.9));
#81333=CARTESIAN_POINT('',(9.89038374274969,-52.974488556385,-0.6));
#81334=CARTESIAN_POINT('Ctrl Pts',(9.89038374274969,-52.974488556385,-0.9));
#81335=CARTESIAN_POINT('Ctrl Pts',(9.89038374274969,-52.4433831572533,-0.9));
#81336=CARTESIAN_POINT('Ctrl Pts',(10.0933161005378,-52.0479540228844,-0.9));
#81337=CARTESIAN_POINT('Ctrl Pts',(10.0701227411628,-53.8859484791756,-0.6));
#81338=CARTESIAN_POINT('Ctrl Pts',(10.0701227411628,-53.8859484791756,-0.9));
#81339=CARTESIAN_POINT('Ctrl Pts',(9.89038374274969,-53.4615282416344,-0.6));
#81340=CARTESIAN_POINT('Ctrl Pts',(9.89038374274969,-53.4615282416344,-0.9));
#81341=CARTESIAN_POINT('Ctrl Pts',(9.89038374274969,-52.974488556385,-0.6));
#81342=CARTESIAN_POINT('Ctrl Pts',(9.89038374274969,-52.974488556385,-0.9));
#81343=CARTESIAN_POINT('',(10.0701227411628,-53.8859484791756,-0.6));
#81344=CARTESIAN_POINT('Ctrl Pts',(10.0701227411628,-53.8859484791756,-0.6));
#81345=CARTESIAN_POINT('Ctrl Pts',(9.89038374274969,-53.4615282416344,-0.6));
#81346=CARTESIAN_POINT('Ctrl Pts',(9.89038374274969,-52.974488556385,-0.6));
#81347=CARTESIAN_POINT('',(10.0701227411628,-53.8859484791756,-0.9));
#81348=CARTESIAN_POINT('',(10.0701227411628,-53.8859484791756,-0.6));
#81349=CARTESIAN_POINT('Ctrl Pts',(10.0701227411628,-53.8859484791756,-0.9));
#81350=CARTESIAN_POINT('Ctrl Pts',(9.89038374274969,-53.4615282416344,-0.9));
#81351=CARTESIAN_POINT('Ctrl Pts',(9.89038374274969,-52.974488556385,-0.9));
#81352=CARTESIAN_POINT('Ctrl Pts',(10.5942716822028,-54.5341746211052,-0.6));
#81353=CARTESIAN_POINT('Ctrl Pts',(10.5942716822028,-54.5341746211052,-0.9));
#81354=CARTESIAN_POINT('Ctrl Pts',(10.2498617395759,-54.3103687167168,-0.6));
#81355=CARTESIAN_POINT('Ctrl Pts',(10.2498617395759,-54.3103687167168,-0.9));
#81356=CARTESIAN_POINT('Ctrl Pts',(10.0701227411628,-53.8859484791756,-0.6));
#81357=CARTESIAN_POINT('Ctrl Pts',(10.0701227411628,-53.8859484791756,-0.9));
#81358=CARTESIAN_POINT('',(10.5942716822028,-54.5341746211052,-0.6));
#81359=CARTESIAN_POINT('Ctrl Pts',(10.5942716822028,-54.5341746211052,-0.6));
#81360=CARTESIAN_POINT('Ctrl Pts',(10.2498617395759,-54.3103687167168,-0.6));
#81361=CARTESIAN_POINT('Ctrl Pts',(10.0701227411628,-53.8859484791756,-0.6));
#81362=CARTESIAN_POINT('',(10.5942716822028,-54.5341746211052,-0.9));
#81363=CARTESIAN_POINT('',(10.5942716822028,-54.5341746211052,-0.6));
#81364=CARTESIAN_POINT('Ctrl Pts',(10.5942716822028,-54.5341746211052,-0.9));
#81365=CARTESIAN_POINT('Ctrl Pts',(10.2498617395759,-54.3103687167168,-0.9));
#81366=CARTESIAN_POINT('Ctrl Pts',(10.0701227411628,-53.8859484791756,-0.9));
#81367=CARTESIAN_POINT('Ctrl Pts',(11.4883318170905,-54.7579811215401,-0.6));
#81368=CARTESIAN_POINT('Ctrl Pts',(11.4883318170905,-54.7579811215401,-0.9));
#81369=CARTESIAN_POINT('Ctrl Pts',(10.9386720880866,-54.7579811215401,-0.6));
#81370=CARTESIAN_POINT('Ctrl Pts',(10.9386720880866,-54.7579811215401,-0.9));
#81371=CARTESIAN_POINT('Ctrl Pts',(10.5942716822028,-54.5341746211052,-0.6));
#81372=CARTESIAN_POINT('Ctrl Pts',(10.5942716822028,-54.5341746211052,-0.9));
#81373=CARTESIAN_POINT('',(11.4883318170905,-54.7579811215401,-0.6));
#81374=CARTESIAN_POINT('Ctrl Pts',(11.4883318170905,-54.7579811215401,-0.6));
#81375=CARTESIAN_POINT('Ctrl Pts',(10.9386720880866,-54.7579811215401,-0.6));
#81376=CARTESIAN_POINT('Ctrl Pts',(10.5942716822028,-54.5341746211052,-0.6));
#81377=CARTESIAN_POINT('',(11.4883318170905,-54.7579811215401,-0.9));
#81378=CARTESIAN_POINT('',(11.4883318170905,-54.7579811215401,-0.6));
#81379=CARTESIAN_POINT('Ctrl Pts',(11.4883318170905,-54.7579811215401,-0.9));
#81380=CARTESIAN_POINT('Ctrl Pts',(10.9386720880866,-54.7579811215401,-0.9));
#81381=CARTESIAN_POINT('Ctrl Pts',(10.5942716822028,-54.5341746211052,-0.9));
#81382=CARTESIAN_POINT('Ctrl Pts',(12.3870363458991,-54.4669167399406,-0.6));
#81383=CARTESIAN_POINT('Ctrl Pts',(12.3870363458991,-54.4669167399406,-0.9));
#81384=CARTESIAN_POINT('Ctrl Pts',(12.0194425806403,-54.7579811215401,-0.6));
#81385=CARTESIAN_POINT('Ctrl Pts',(12.0194425806403,-54.7579811215401,-0.9));
#81386=CARTESIAN_POINT('Ctrl Pts',(11.4883318170905,-54.7579811215401,-0.6));
#81387=CARTESIAN_POINT('Ctrl Pts',(11.4883318170905,-54.7579811215401,-0.9));
#81388=CARTESIAN_POINT('',(12.3870363458991,-54.4669167399406,-0.6));
#81389=CARTESIAN_POINT('Ctrl Pts',(12.3870363458991,-54.4669167399406,-0.6));
#81390=CARTESIAN_POINT('Ctrl Pts',(12.0194425806403,-54.7579811215401,-0.6));
#81391=CARTESIAN_POINT('Ctrl Pts',(11.4883318170905,-54.7579811215401,-0.6));
#81392=CARTESIAN_POINT('',(12.3870363458991,-54.4669167399406,-0.9));
#81393=CARTESIAN_POINT('',(12.3870363458991,-54.4669167399406,-0.6));
#81394=CARTESIAN_POINT('Ctrl Pts',(12.3870363458991,-54.4669167399406,-0.9));
#81395=CARTESIAN_POINT('Ctrl Pts',(12.0194425806403,-54.7579811215401,-0.9));
#81396=CARTESIAN_POINT('Ctrl Pts',(11.4883318170905,-54.7579811215401,-0.9));
#81397=CARTESIAN_POINT('Ctrl Pts',(12.8961076959968,-53.6215553879738,-0.6));
#81398=CARTESIAN_POINT('Ctrl Pts',(12.8961076959968,-53.6215553879738,-0.9));
#81399=CARTESIAN_POINT('Ctrl Pts',(12.7546396479011,-54.1758529543877,-0.6));
#81400=CARTESIAN_POINT('Ctrl Pts',(12.7546396479011,-54.1758529543877,-0.9));
#81401=CARTESIAN_POINT('Ctrl Pts',(12.3870363458991,-54.4669167399406,-0.6));
#81402=CARTESIAN_POINT('Ctrl Pts',(12.3870363458991,-54.4669167399406,-0.9));
#81403=CARTESIAN_POINT('',(12.8961076959968,-53.6215553879738,-0.6));
#81404=CARTESIAN_POINT('Ctrl Pts',(12.8961076959968,-53.6215553879738,-0.6));
#81405=CARTESIAN_POINT('Ctrl Pts',(12.7546396479011,-54.1758529543877,-0.6));
#81406=CARTESIAN_POINT('Ctrl Pts',(12.3870363458991,-54.4669167399406,-0.6));
#81407=CARTESIAN_POINT('',(12.8961076959968,-53.6215553879738,-0.9));
#81408=CARTESIAN_POINT('',(12.8961076959968,-53.6215553879738,-0.6));
#81409=CARTESIAN_POINT('Ctrl Pts',(12.8961076959968,-53.6215553879738,-0.9));
#81410=CARTESIAN_POINT('Ctrl Pts',(12.7546396479011,-54.1758529543877,-0.9));
#81411=CARTESIAN_POINT('Ctrl Pts',(12.3870363458991,-54.4669167399406,-0.9));
#81412=CARTESIAN_POINT('Origin',(12.4461832270026,-53.5079125761986,-0.6));
#81413=CARTESIAN_POINT('',(12.4461832270026,-53.5079125761986,-0.6));
#81414=CARTESIAN_POINT('',(6.53600250299025,-52.0151074458665,-0.6));
#81415=CARTESIAN_POINT('',(12.4461832270026,-53.5079125761986,-0.9));
#81416=CARTESIAN_POINT('',(12.4461832270026,-53.5079125761986,-0.6));
#81417=CARTESIAN_POINT('',(12.4461832270026,-53.5079125761986,-0.9));
#81418=CARTESIAN_POINT('Ctrl Pts',(12.0913400873542,-54.1549794077873,-0.6));
#81419=CARTESIAN_POINT('Ctrl Pts',(12.0913400873542,-54.1549794077873,-0.9));
#81420=CARTESIAN_POINT('Ctrl Pts',(12.3534097895026,-53.9369718432426,-0.6));
#81421=CARTESIAN_POINT('Ctrl Pts',(12.3534097895026,-53.9369718432426,-0.9));
#81422=CARTESIAN_POINT('Ctrl Pts',(12.4461832270026,-53.5079125761986,-0.6));
#81423=CARTESIAN_POINT('Ctrl Pts',(12.4461832270026,-53.5079125761986,-0.9));
#81424=CARTESIAN_POINT('',(12.0913400873542,-54.1549794077873,-0.6));
#81425=CARTESIAN_POINT('Ctrl Pts',(12.0913400873542,-54.1549794077873,-0.6));
#81426=CARTESIAN_POINT('Ctrl Pts',(12.3534097895026,-53.9369718432426,-0.6));
#81427=CARTESIAN_POINT('Ctrl Pts',(12.4461832270026,-53.5079125761986,-0.6));
#81428=CARTESIAN_POINT('',(12.0913400873542,-54.1549794077873,-0.9));
#81429=CARTESIAN_POINT('',(12.0913400873542,-54.1549794077873,-0.6));
#81430=CARTESIAN_POINT('Ctrl Pts',(12.0913400873542,-54.1549794077873,-0.9));
#81431=CARTESIAN_POINT('Ctrl Pts',(12.3534097895026,-53.9369718432426,-0.9));
#81432=CARTESIAN_POINT('Ctrl Pts',(12.4461832270026,-53.5079125761986,-0.9));
#81433=CARTESIAN_POINT('Ctrl Pts',(11.4512243494391,-54.3729875683784,-0.6));
#81434=CARTESIAN_POINT('Ctrl Pts',(11.4512243494391,-54.3729875683784,-0.9));
#81435=CARTESIAN_POINT('Ctrl Pts',(11.8292608484626,-54.3729875683784,-0.6));
#81436=CARTESIAN_POINT('Ctrl Pts',(11.8292608484626,-54.3729875683784,-0.9));
#81437=CARTESIAN_POINT('Ctrl Pts',(12.0913400873542,-54.1549794077873,-0.6));
#81438=CARTESIAN_POINT('Ctrl Pts',(12.0913400873542,-54.1549794077873,-0.9));
#81439=CARTESIAN_POINT('Ctrl Pts',(11.4512243494391,-54.3729875683784,-0.6));
#81440=CARTESIAN_POINT('Ctrl Pts',(11.8292608484626,-54.3729875683784,-0.6));
#81441=CARTESIAN_POINT('Ctrl Pts',(12.0913400873542,-54.1549794077873,-0.6));
#81442=CARTESIAN_POINT('Ctrl Pts',(11.4512243494391,-54.3729875683784,-0.9));
#81443=CARTESIAN_POINT('Ctrl Pts',(11.8292608484626,-54.3729875683784,-0.9));
#81444=CARTESIAN_POINT('Ctrl Pts',(12.0913400873542,-54.1549794077873,-0.9));
#81445=CARTESIAN_POINT('Origin',(11.3932457193732,-53.0000002384186,-0.9));
#81446=CARTESIAN_POINT('Origin',(4.11548521369696,-54.2987720370293,-0.6));
#81447=CARTESIAN_POINT('',(4.11548521369696,-54.2987720370293,-0.6));
#81448=CARTESIAN_POINT('',(5.78997518867254,-54.2987720370293,-0.6));
#81449=CARTESIAN_POINT('',(2.05774260684848,-54.2987720370293,-0.6));
#81450=CARTESIAN_POINT('',(4.11548521369696,-54.2987720370293,-0.9));
#81451=CARTESIAN_POINT('',(4.11548521369696,-54.2987720370293,-0.6));
#81452=CARTESIAN_POINT('',(5.78997518867254,-54.2987720370293,-0.9));
#81453=CARTESIAN_POINT('',(4.11548521369696,-54.2987720370293,-0.9));
#81454=CARTESIAN_POINT('',(5.78997518867254,-54.2987720370293,-0.6));
#81455=CARTESIAN_POINT('Origin',(4.11548521369696,-51.3000003695488,-0.6));
#81456=CARTESIAN_POINT('',(4.11548521369696,-51.3000003695488,-0.6));
#81457=CARTESIAN_POINT('',(4.11548521369696,-52.1500001847744,-0.6));
#81458=CARTESIAN_POINT('',(4.11548521369696,-51.3000003695488,-0.9));
#81459=CARTESIAN_POINT('',(4.11548521369696,-51.3000003695488,-0.6));
#81460=CARTESIAN_POINT('',(4.11548521369696,-51.3000003695488,-0.9));
#81461=CARTESIAN_POINT('Origin',(3.66555359214544,-51.3000003695488,-0.6));
#81462=CARTESIAN_POINT('',(3.66555359214544,-51.3000003695488,-0.6));
#81463=CARTESIAN_POINT('',(1.83277679607272,-51.3000003695488,-0.6));
#81464=CARTESIAN_POINT('',(3.66555359214544,-51.3000003695488,-0.9));
#81465=CARTESIAN_POINT('',(3.66555359214544,-51.3000003695488,-0.6));
#81466=CARTESIAN_POINT('',(3.66555359214544,-51.3000003695488,-0.9));
#81467=CARTESIAN_POINT('Origin',(3.66555359214544,-54.7000001072884,-0.6));
#81468=CARTESIAN_POINT('',(3.66555359214544,-54.7000001072884,-0.6));
#81469=CARTESIAN_POINT('',(3.66555359214544,-53.8500000536442,-0.6));
#81470=CARTESIAN_POINT('',(3.66555359214544,-54.7000001072884,-0.9));
#81471=CARTESIAN_POINT('',(3.66555359214544,-54.7000001072884,-0.6));
#81472=CARTESIAN_POINT('',(3.66555359214544,-54.7000001072884,-0.9));
#81473=CARTESIAN_POINT('Origin',(5.78997518867254,-54.7000001072884,-0.6));
#81474=CARTESIAN_POINT('',(5.78997518867254,-54.7000001072884,-0.6));
#81475=CARTESIAN_POINT('',(2.89498759433627,-54.7000001072884,-0.6));
#81476=CARTESIAN_POINT('',(5.78997518867254,-54.7000001072884,-0.9));
#81477=CARTESIAN_POINT('',(5.78997518867254,-54.7000001072884,-0.6));
#81478=CARTESIAN_POINT('',(5.78997518867254,-54.7000001072884,-0.9));
#81479=CARTESIAN_POINT('Origin',(5.78997518867254,-54.2987720370293,-0.6));
#81480=CARTESIAN_POINT('',(5.78997518867254,-53.6493860185146,-0.6));
#81481=CARTESIAN_POINT('',(5.78997518867254,-54.2987720370293,-0.9));
#81482=CARTESIAN_POINT('Origin',(4.72776439040899,-53.0000002384186,-0.9));
#81483=CARTESIAN_POINT('Origin',(-31.9741490855813,-51.7012278437614,-0.6));
#81484=CARTESIAN_POINT('',(-31.9741490855813,-51.7012278437614,-0.6));
#81485=CARTESIAN_POINT('',(-33.0989785864949,-51.7012278437614,-0.6));
#81486=CARTESIAN_POINT('',(-15.9870745427907,-51.7012278437614,-0.6));
#81487=CARTESIAN_POINT('',(-31.9741490855813,-51.7012278437614,-0.9));
#81488=CARTESIAN_POINT('',(-31.9741490855813,-51.7012278437614,-0.6));
#81489=CARTESIAN_POINT('',(-33.0989785864949,-51.7012278437614,-0.9));
#81490=CARTESIAN_POINT('',(-31.9741490855813,-51.7012278437614,-0.9));
#81491=CARTESIAN_POINT('',(-33.0989785864949,-51.7012278437614,-0.6));
#81492=CARTESIAN_POINT('Origin',(-31.9741490855813,-51.3000003695488,-0.6));
#81493=CARTESIAN_POINT('',(-31.9741490855813,-51.3000003695488,-0.6));
#81494=CARTESIAN_POINT('',(-31.9741490855813,-52.1500001847744,-0.6));
#81495=CARTESIAN_POINT('',(-31.9741490855813,-51.3000003695488,-0.9));
#81496=CARTESIAN_POINT('',(-31.9741490855813,-51.3000003695488,-0.6));
#81497=CARTESIAN_POINT('',(-31.9741490855813,-51.3000003695488,-0.9));
#81498=CARTESIAN_POINT('Origin',(-34.6691012382507,-51.3000003695488,-0.6));
#81499=CARTESIAN_POINT('',(-34.6691012382507,-51.3000003695488,-0.6));
#81500=CARTESIAN_POINT('',(-17.3345506191254,-51.3000003695488,-0.6));
#81501=CARTESIAN_POINT('',(-34.6691012382507,-51.3000003695488,-0.9));
#81502=CARTESIAN_POINT('',(-34.6691012382507,-51.3000003695488,-0.6));
#81503=CARTESIAN_POINT('',(-34.6691012382507,-51.3000003695488,-0.9));
#81504=CARTESIAN_POINT('Origin',(-34.6691012382507,-51.7012278437614,-0.6));
#81505=CARTESIAN_POINT('',(-34.6691012382507,-51.7012278437614,-0.6));
#81506=CARTESIAN_POINT('',(-34.6691012382507,-52.3506139218807,-0.6));
#81507=CARTESIAN_POINT('',(-34.6691012382507,-51.7012278437614,-0.9));
#81508=CARTESIAN_POINT('',(-34.6691012382507,-51.7012278437614,-0.6));
#81509=CARTESIAN_POINT('',(-34.6691012382507,-51.7012278437614,-0.9));
#81510=CARTESIAN_POINT('Origin',(-33.5489102080464,-51.7012278437614,-0.6));
#81511=CARTESIAN_POINT('',(-33.5489102080464,-51.7012278437614,-0.6));
#81512=CARTESIAN_POINT('',(-16.7744551040232,-51.7012278437614,-0.6));
#81513=CARTESIAN_POINT('',(-33.5489102080464,-51.7012278437614,-0.9));
#81514=CARTESIAN_POINT('',(-33.5489102080464,-51.7012278437614,-0.6));
#81515=CARTESIAN_POINT('',(-33.5489102080464,-51.7012278437614,-0.9));
#81516=CARTESIAN_POINT('Origin',(-33.5489102080464,-54.7000001072884,-0.6));
#81517=CARTESIAN_POINT('',(-33.5489102080464,-54.7000001072884,-0.6));
#81518=CARTESIAN_POINT('',(-33.5489102080464,-53.8500000536442,-0.6));
#81519=CARTESIAN_POINT('',(-33.5489102080464,-54.7000001072884,-0.9));
#81520=CARTESIAN_POINT('',(-33.5489102080464,-54.7000001072884,-0.6));
#81521=CARTESIAN_POINT('',(-33.5489102080464,-54.7000001072884,-0.9));
#81522=CARTESIAN_POINT('Origin',(-33.0989785864949,-54.7000001072884,-0.6));
#81523=CARTESIAN_POINT('',(-33.0989785864949,-54.7000001072884,-0.6));
#81524=CARTESIAN_POINT('',(-16.5494892932475,-54.7000001072884,-0.6));
#81525=CARTESIAN_POINT('',(-33.0989785864949,-54.7000001072884,-0.9));
#81526=CARTESIAN_POINT('',(-33.0989785864949,-54.7000001072884,-0.6));
#81527=CARTESIAN_POINT('',(-33.0989785864949,-54.7000001072884,-0.9));
#81528=CARTESIAN_POINT('Origin',(-33.0989785864949,-51.7012278437614,-0.6));
#81529=CARTESIAN_POINT('',(-33.0989785864949,-52.3506139218807,-0.6));
#81530=CARTESIAN_POINT('',(-33.0989785864949,-51.7012278437614,-0.9));
#81531=CARTESIAN_POINT('Origin',(-33.321625161916,-53.0000002384186,-0.9));
#81532=CARTESIAN_POINT('Ctrl Pts',(-3.18315122276545,-54.3521146178246,
-0.6));
#81533=CARTESIAN_POINT('Ctrl Pts',(-3.18315122276545,-54.3521146178246,
-0.9));
#81534=CARTESIAN_POINT('Ctrl Pts',(-2.68683526664972,-54.3521146178246,
-0.6));
#81535=CARTESIAN_POINT('Ctrl Pts',(-2.68683526664972,-54.3521146178246,
-0.9));
#81536=CARTESIAN_POINT('Ctrl Pts',(-2.47578475624323,-54.1271488070488,
-0.6));
#81537=CARTESIAN_POINT('Ctrl Pts',(-2.47578475624323,-54.1271488070488,
-0.9));
#81538=CARTESIAN_POINT('',(-3.18315122276545,-54.3521146178246,-0.6));
#81539=CARTESIAN_POINT('',(-2.47578475624323,-54.1271488070488,-0.6));
#81540=CARTESIAN_POINT('Ctrl Pts',(-3.18315122276545,-54.3521146178246,
-0.6));
#81541=CARTESIAN_POINT('Ctrl Pts',(-2.68683526664972,-54.3521146178246,
-0.6));
#81542=CARTESIAN_POINT('Ctrl Pts',(-2.47578475624323,-54.1271488070488,
-0.6));
#81543=CARTESIAN_POINT('',(-3.18315122276545,-54.3521146178246,-0.9));
#81544=CARTESIAN_POINT('',(-3.18315122276545,-54.3521146178246,-0.6));
#81545=CARTESIAN_POINT('',(-2.47578475624323,-54.1271488070488,-0.9));
#81546=CARTESIAN_POINT('Ctrl Pts',(-3.18315122276545,-54.3521146178246,
-0.9));
#81547=CARTESIAN_POINT('Ctrl Pts',(-2.68683526664972,-54.3521146178246,
-0.9));
#81548=CARTESIAN_POINT('Ctrl Pts',(-2.47578475624323,-54.1271488070488,
-0.9));
#81549=CARTESIAN_POINT('',(-2.47578475624323,-54.1271488070488,-0.6));
#81550=CARTESIAN_POINT('Ctrl Pts',(-3.67367122322321,-54.2384724020958,
-0.6));
#81551=CARTESIAN_POINT('Ctrl Pts',(-3.67367122322321,-54.2384724020958,
-0.9));
#81552=CARTESIAN_POINT('Ctrl Pts',(-3.47305629402399,-54.3521146178246,
-0.6));
#81553=CARTESIAN_POINT('Ctrl Pts',(-3.47305629402399,-54.3521146178246,
-0.9));
#81554=CARTESIAN_POINT('Ctrl Pts',(-3.18315122276545,-54.3521146178246,
-0.6));
#81555=CARTESIAN_POINT('Ctrl Pts',(-3.18315122276545,-54.3521146178246,
-0.9));
#81556=CARTESIAN_POINT('',(-3.67367122322321,-54.2384724020958,-0.6));
#81557=CARTESIAN_POINT('Ctrl Pts',(-3.67367122322321,-54.2384724020958,
-0.6));
#81558=CARTESIAN_POINT('Ctrl Pts',(-3.47305629402399,-54.3521146178246,
-0.6));
#81559=CARTESIAN_POINT('Ctrl Pts',(-3.18315122276545,-54.3521146178246,
-0.6));
#81560=CARTESIAN_POINT('',(-3.67367122322321,-54.2384724020958,-0.9));
#81561=CARTESIAN_POINT('',(-3.67367122322321,-54.2384724020958,-0.6));
#81562=CARTESIAN_POINT('Ctrl Pts',(-3.67367122322321,-54.2384724020958,
-0.9));
#81563=CARTESIAN_POINT('Ctrl Pts',(-3.47305629402399,-54.3521146178246,
-0.9));
#81564=CARTESIAN_POINT('Ctrl Pts',(-3.18315122276545,-54.3521146178246,
-0.9));
#81565=CARTESIAN_POINT('Ctrl Pts',(-3.95661685615778,-53.914938390255,-0.6));
#81566=CARTESIAN_POINT('Ctrl Pts',(-3.95661685615778,-53.914938390255,-0.9));
#81567=CARTESIAN_POINT('Ctrl Pts',(-3.87428376823664,-54.1248295903206,
-0.6));
#81568=CARTESIAN_POINT('Ctrl Pts',(-3.87428376823664,-54.1248295903206,
-0.9));
#81569=CARTESIAN_POINT('Ctrl Pts',(-3.67367122322321,-54.2384724020958,
-0.6));
#81570=CARTESIAN_POINT('Ctrl Pts',(-3.67367122322321,-54.2384724020958,
-0.9));
#81571=CARTESIAN_POINT('',(-3.95661685615778,-53.914938390255,-0.6));
#81572=CARTESIAN_POINT('Ctrl Pts',(-3.95661685615778,-53.914938390255,-0.6));
#81573=CARTESIAN_POINT('Ctrl Pts',(-3.87428376823664,-54.1248295903206,
-0.6));
#81574=CARTESIAN_POINT('Ctrl Pts',(-3.67367122322321,-54.2384724020958,
-0.6));
#81575=CARTESIAN_POINT('',(-3.95661685615778,-53.914938390255,-0.9));
#81576=CARTESIAN_POINT('',(-3.95661685615778,-53.914938390255,-0.6));
#81577=CARTESIAN_POINT('Ctrl Pts',(-3.95661685615778,-53.914938390255,-0.9));
#81578=CARTESIAN_POINT('Ctrl Pts',(-3.87428376823664,-54.1248295903206,
-0.9));
#81579=CARTESIAN_POINT('Ctrl Pts',(-3.67367122322321,-54.2384724020958,
-0.9));
#81580=CARTESIAN_POINT('Ctrl Pts',(-4.03894994407892,-53.2620738148689,
-0.6));
#81581=CARTESIAN_POINT('Ctrl Pts',(-4.03894994407892,-53.2620738148689,
-0.9));
#81582=CARTESIAN_POINT('Ctrl Pts',(-4.03894994407892,-53.7050477862358,
-0.6));
#81583=CARTESIAN_POINT('Ctrl Pts',(-4.03894994407892,-53.7050477862358,
-0.9));
#81584=CARTESIAN_POINT('Ctrl Pts',(-3.95661685615778,-53.914938390255,-0.6));
#81585=CARTESIAN_POINT('Ctrl Pts',(-3.95661685615778,-53.914938390255,-0.9));
#81586=CARTESIAN_POINT('',(-4.03894994407892,-53.2620738148689,-0.6));
#81587=CARTESIAN_POINT('Ctrl Pts',(-4.03894994407892,-53.2620738148689,
-0.6));
#81588=CARTESIAN_POINT('Ctrl Pts',(-4.03894994407892,-53.7050477862358,
-0.6));
#81589=CARTESIAN_POINT('Ctrl Pts',(-3.95661685615778,-53.914938390255,-0.6));
#81590=CARTESIAN_POINT('',(-4.03894994407892,-53.2620738148689,-0.9));
#81591=CARTESIAN_POINT('',(-4.03894994407892,-53.2620738148689,-0.6));
#81592=CARTESIAN_POINT('Ctrl Pts',(-4.03894994407892,-53.2620738148689,
-0.9));
#81593=CARTESIAN_POINT('Ctrl Pts',(-4.03894994407892,-53.7050477862358,
-0.9));
#81594=CARTESIAN_POINT('Ctrl Pts',(-3.95661685615778,-53.914938390255,-0.9));
#81595=CARTESIAN_POINT('Origin',(-4.03894994407892,-51.3000003695488,-0.6));
#81596=CARTESIAN_POINT('',(-4.03894994407892,-51.3000003695488,-0.6));
#81597=CARTESIAN_POINT('',(-4.03894994407892,-52.1500001847744,-0.6));
#81598=CARTESIAN_POINT('',(-4.03894994407892,-51.3000003695488,-0.9));
#81599=CARTESIAN_POINT('',(-4.03894994407892,-51.3000003695488,-0.6));
#81600=CARTESIAN_POINT('',(-4.03894994407892,-51.3000003695488,-0.9));
#81601=CARTESIAN_POINT('Origin',(-4.48888156563044,-51.3000003695488,-0.6));
#81602=CARTESIAN_POINT('',(-4.48888156563044,-51.3000003695488,-0.6));
#81603=CARTESIAN_POINT('',(-2.24444078281522,-51.3000003695488,-0.6));
#81604=CARTESIAN_POINT('',(-4.48888156563044,-51.3000003695488,-0.9));
#81605=CARTESIAN_POINT('',(-4.48888156563044,-51.3000003695488,-0.6));
#81606=CARTESIAN_POINT('',(-4.48888156563044,-51.3000003695488,-0.9));
#81607=CARTESIAN_POINT('Origin',(-4.48888156563044,-53.2643930315971,-0.6));
#81608=CARTESIAN_POINT('',(-4.48888156563044,-53.2643930315971,-0.6));
#81609=CARTESIAN_POINT('',(-4.48888156563044,-53.1321965157986,-0.6));
#81610=CARTESIAN_POINT('',(-4.48888156563044,-53.2643930315971,-0.9));
#81611=CARTESIAN_POINT('',(-4.48888156563044,-53.2643930315971,-0.6));
#81612=CARTESIAN_POINT('',(-4.48888156563044,-53.2643930315971,-0.9));
#81613=CARTESIAN_POINT('Ctrl Pts',(-4.35900542885065,-54.1167120337486,
-0.6));
#81614=CARTESIAN_POINT('Ctrl Pts',(-4.35900542885065,-54.1167120337486,
-0.9));
#81615=CARTESIAN_POINT('Ctrl Pts',(-4.48888156563044,-53.8047747015953,
-0.6));
#81616=CARTESIAN_POINT('Ctrl Pts',(-4.48888156563044,-53.8047747015953,
-0.9));
#81617=CARTESIAN_POINT('Ctrl Pts',(-4.48888156563044,-53.2643930315971,
-0.6));
#81618=CARTESIAN_POINT('Ctrl Pts',(-4.48888156563044,-53.2643930315971,
-0.9));
#81619=CARTESIAN_POINT('',(-4.35900542885065,-54.1167120337486,-0.6));
#81620=CARTESIAN_POINT('Ctrl Pts',(-4.35900542885065,-54.1167120337486,
-0.6));
#81621=CARTESIAN_POINT('Ctrl Pts',(-4.48888156563044,-53.8047747015953,
-0.6));
#81622=CARTESIAN_POINT('Ctrl Pts',(-4.48888156563044,-53.2643930315971,
-0.6));
#81623=CARTESIAN_POINT('',(-4.35900542885065,-54.1167120337486,-0.9));
#81624=CARTESIAN_POINT('',(-4.35900542885065,-54.1167120337486,-0.6));
#81625=CARTESIAN_POINT('Ctrl Pts',(-4.35900542885065,-54.1167120337486,
-0.9));
#81626=CARTESIAN_POINT('Ctrl Pts',(-4.48888156563044,-53.8047747015953,
-0.9));
#81627=CARTESIAN_POINT('Ctrl Pts',(-4.48888156563044,-53.2643930315971,
-0.9));
#81628=CARTESIAN_POINT('Ctrl Pts',(-3.92530772835016,-54.5933155417442,
-0.6));
#81629=CARTESIAN_POINT('Ctrl Pts',(-3.92530772835016,-54.5933155417442,
-0.9));
#81630=CARTESIAN_POINT('Ctrl Pts',(-4.22912690788507,-54.4286493659019,
-0.6));
#81631=CARTESIAN_POINT('Ctrl Pts',(-4.22912690788507,-54.4286493659019,
-0.9));
#81632=CARTESIAN_POINT('Ctrl Pts',(-4.35900542885065,-54.1167120337486,
-0.6));
#81633=CARTESIAN_POINT('Ctrl Pts',(-4.35900542885065,-54.1167120337486,
-0.9));
#81634=CARTESIAN_POINT('',(-3.92530772835016,-54.5933155417442,-0.6));
#81635=CARTESIAN_POINT('Ctrl Pts',(-3.92530772835016,-54.5933155417442,
-0.6));
#81636=CARTESIAN_POINT('Ctrl Pts',(-4.22912690788507,-54.4286493659019,
-0.6));
#81637=CARTESIAN_POINT('Ctrl Pts',(-4.35900542885065,-54.1167120337486,
-0.6));
#81638=CARTESIAN_POINT('',(-3.92530772835016,-54.5933155417442,-0.9));
#81639=CARTESIAN_POINT('',(-3.92530772835016,-54.5933155417442,-0.6));
#81640=CARTESIAN_POINT('Ctrl Pts',(-3.92530772835016,-54.5933155417442,
-0.9));
#81641=CARTESIAN_POINT('Ctrl Pts',(-4.22912690788507,-54.4286493659019,
-0.9));
#81642=CARTESIAN_POINT('Ctrl Pts',(-4.35900542885065,-54.1167120337486,
-0.9));
#81643=CARTESIAN_POINT('Ctrl Pts',(-3.14372394233942,-54.7579811215401,
-0.6));
#81644=CARTESIAN_POINT('Ctrl Pts',(-3.14372394233942,-54.7579811215401,
-0.9));
#81645=CARTESIAN_POINT('Ctrl Pts',(-3.62148616462946,-54.7579811215401,
-0.6));
#81646=CARTESIAN_POINT('Ctrl Pts',(-3.62148616462946,-54.7579811215401,
-0.9));
#81647=CARTESIAN_POINT('Ctrl Pts',(-3.92530772835016,-54.5933155417442,
-0.6));
#81648=CARTESIAN_POINT('Ctrl Pts',(-3.92530772835016,-54.5933155417442,
-0.9));
#81649=CARTESIAN_POINT('',(-3.14372394233942,-54.7579811215401,-0.6));
#81650=CARTESIAN_POINT('Ctrl Pts',(-3.14372394233942,-54.7579811215401,
-0.6));
#81651=CARTESIAN_POINT('Ctrl Pts',(-3.62148616462946,-54.7579811215401,
-0.6));
#81652=CARTESIAN_POINT('Ctrl Pts',(-3.92530772835016,-54.5933155417442,
-0.6));
#81653=CARTESIAN_POINT('',(-3.14372394233942,-54.7579811215401,-0.9));
#81654=CARTESIAN_POINT('',(-3.14372394233942,-54.7579811215401,-0.6));
#81655=CARTESIAN_POINT('Ctrl Pts',(-3.14372394233942,-54.7579811215401,
-0.9));
#81656=CARTESIAN_POINT('Ctrl Pts',(-3.62148616462946,-54.7579811215401,
-0.9));
#81657=CARTESIAN_POINT('Ctrl Pts',(-3.92530772835016,-54.5933155417442,
-0.9));
#81658=CARTESIAN_POINT('Ctrl Pts',(-2.34938714653254,-54.5689634680748,
-0.6));
#81659=CARTESIAN_POINT('Ctrl Pts',(-2.34938714653254,-54.5689634680748,
-0.9));
#81660=CARTESIAN_POINT('Ctrl Pts',(-2.65204761177301,-54.7579811215401,
-0.6));
#81661=CARTESIAN_POINT('Ctrl Pts',(-2.65204761177301,-54.7579811215401,
-0.9));
#81662=CARTESIAN_POINT('Ctrl Pts',(-3.14372394233942,-54.7579811215401,
-0.6));
#81663=CARTESIAN_POINT('Ctrl Pts',(-3.14372394233942,-54.7579811215401,
-0.9));
#81664=CARTESIAN_POINT('',(-2.34938714653254,-54.5689634680748,-0.6));
#81665=CARTESIAN_POINT('Ctrl Pts',(-2.34938714653254,-54.5689634680748,
-0.6));
#81666=CARTESIAN_POINT('Ctrl Pts',(-2.65204761177301,-54.7579811215401,
-0.6));
#81667=CARTESIAN_POINT('Ctrl Pts',(-3.14372394233942,-54.7579811215401,
-0.6));
#81668=CARTESIAN_POINT('',(-2.34938714653254,-54.5689634680748,-0.9));
#81669=CARTESIAN_POINT('',(-2.34938714653254,-54.5689634680748,-0.6));
#81670=CARTESIAN_POINT('Ctrl Pts',(-2.34938714653254,-54.5689634680748,
-0.9));
#81671=CARTESIAN_POINT('Ctrl Pts',(-2.65204761177301,-54.7579811215401,
-0.9));
#81672=CARTESIAN_POINT('Ctrl Pts',(-3.14372394233942,-54.7579811215401,
-0.9));
#81673=CARTESIAN_POINT('Ctrl Pts',(-1.93076465278864,-54.0784446597099,
-0.6));
#81674=CARTESIAN_POINT('Ctrl Pts',(-1.93076465278864,-54.0784446597099,
-0.9));
#81675=CARTESIAN_POINT('Ctrl Pts',(-2.04672668129206,-54.3799452185631,
-0.6));
#81676=CARTESIAN_POINT('Ctrl Pts',(-2.04672668129206,-54.3799452185631,
-0.9));
#81677=CARTESIAN_POINT('Ctrl Pts',(-2.34938714653254,-54.5689634680748,
-0.6));
#81678=CARTESIAN_POINT('Ctrl Pts',(-2.34938714653254,-54.5689634680748,
-0.9));
#81679=CARTESIAN_POINT('',(-1.93076465278864,-54.0784446597099,-0.6));
#81680=CARTESIAN_POINT('Ctrl Pts',(-1.93076465278864,-54.0784446597099,
-0.6));
#81681=CARTESIAN_POINT('Ctrl Pts',(-2.04672668129206,-54.3799452185631,
-0.6));
#81682=CARTESIAN_POINT('Ctrl Pts',(-2.34938714653254,-54.5689634680748,
-0.6));
#81683=CARTESIAN_POINT('',(-1.93076465278864,-54.0784446597099,-0.9));
#81684=CARTESIAN_POINT('',(-1.93076465278864,-54.0784446597099,-0.6));
#81685=CARTESIAN_POINT('Ctrl Pts',(-1.93076465278864,-54.0784446597099,
-0.9));
#81686=CARTESIAN_POINT('Ctrl Pts',(-2.04672668129206,-54.3799452185631,
-0.9));
#81687=CARTESIAN_POINT('Ctrl Pts',(-2.34938714653254,-54.5689634680748,
-0.9));
#81688=CARTESIAN_POINT('Ctrl Pts',(-1.81480262428522,-53.2643930315971,
-0.6));
#81689=CARTESIAN_POINT('Ctrl Pts',(-1.81480262428522,-53.2643930315971,
-0.9));
#81690=CARTESIAN_POINT('Ctrl Pts',(-1.81480262428522,-53.7769441008568,
-0.6));
#81691=CARTESIAN_POINT('Ctrl Pts',(-1.81480262428522,-53.7769441008568,
-0.9));
#81692=CARTESIAN_POINT('Ctrl Pts',(-1.93076465278864,-54.0784446597099,
-0.6));
#81693=CARTESIAN_POINT('Ctrl Pts',(-1.93076465278864,-54.0784446597099,
-0.9));
#81694=CARTESIAN_POINT('',(-1.81480262428522,-53.2643930315971,-0.6));
#81695=CARTESIAN_POINT('Ctrl Pts',(-1.81480262428522,-53.2643930315971,
-0.6));
#81696=CARTESIAN_POINT('Ctrl Pts',(-1.81480262428522,-53.7769441008568,
-0.6));
#81697=CARTESIAN_POINT('Ctrl Pts',(-1.93076465278864,-54.0784446597099,
-0.6));
#81698=CARTESIAN_POINT('',(-1.81480262428522,-53.2643930315971,-0.9));
#81699=CARTESIAN_POINT('',(-1.81480262428522,-53.2643930315971,-0.6));
#81700=CARTESIAN_POINT('Ctrl Pts',(-1.81480262428522,-53.2643930315971,
-0.9));
#81701=CARTESIAN_POINT('Ctrl Pts',(-1.81480262428522,-53.7769441008568,
-0.9));
#81702=CARTESIAN_POINT('Ctrl Pts',(-1.93076465278864,-54.0784446597099,
-0.9));
#81703=CARTESIAN_POINT('Origin',(-1.81480262428522,-51.3000003695488,-0.6));
#81704=CARTESIAN_POINT('',(-1.81480262428522,-51.3000003695488,-0.6));
#81705=CARTESIAN_POINT('',(-1.81480262428522,-52.1500001847744,-0.6));
#81706=CARTESIAN_POINT('',(-1.81480262428522,-51.3000003695488,-0.9));
#81707=CARTESIAN_POINT('',(-1.81480262428522,-51.3000003695488,-0.6));
#81708=CARTESIAN_POINT('',(-1.81480262428522,-51.3000003695488,-0.9));
#81709=CARTESIAN_POINT('Origin',(-2.26473424583673,-51.3000003695488,-0.6));
#81710=CARTESIAN_POINT('',(-2.26473424583673,-51.3000003695488,-0.6));
#81711=CARTESIAN_POINT('',(-1.13236712291837,-51.3000003695488,-0.6));
#81712=CARTESIAN_POINT('',(-2.26473424583673,-51.3000003695488,-0.9));
#81713=CARTESIAN_POINT('',(-2.26473424583673,-51.3000003695488,-0.6));
#81714=CARTESIAN_POINT('',(-2.26473424583673,-51.3000003695488,-0.9));
#81715=CARTESIAN_POINT('Origin',(-2.26473424583673,-53.2620738148689,-0.6));
#81716=CARTESIAN_POINT('',(-2.26473424583673,-53.2620738148689,-0.6));
#81717=CARTESIAN_POINT('',(-2.26473424583673,-53.1310369074345,-0.6));
#81718=CARTESIAN_POINT('',(-2.26473424583673,-53.2620738148689,-0.9));
#81719=CARTESIAN_POINT('',(-2.26473424583673,-53.2620738148689,-0.6));
#81720=CARTESIAN_POINT('',(-2.26473424583673,-53.2620738148689,-0.9));
#81721=CARTESIAN_POINT('Ctrl Pts',(-2.47578475624323,-54.1271488070488,
-0.6));
#81722=CARTESIAN_POINT('Ctrl Pts',(-2.47578475624323,-54.1271488070488,
-0.9));
#81723=CARTESIAN_POINT('Ctrl Pts',(-2.26473424583673,-53.902182996273,-0.6));
#81724=CARTESIAN_POINT('Ctrl Pts',(-2.26473424583673,-53.902182996273,-0.9));
#81725=CARTESIAN_POINT('Ctrl Pts',(-2.26473424583673,-53.2620738148689,
-0.6));
#81726=CARTESIAN_POINT('Ctrl Pts',(-2.26473424583673,-53.2620738148689,
-0.9));
#81727=CARTESIAN_POINT('Ctrl Pts',(-2.47578475624323,-54.1271488070488,
-0.6));
#81728=CARTESIAN_POINT('Ctrl Pts',(-2.26473424583673,-53.902182996273,-0.6));
#81729=CARTESIAN_POINT('Ctrl Pts',(-2.26473424583673,-53.2620738148689,
-0.6));
#81730=CARTESIAN_POINT('Ctrl Pts',(-2.47578475624323,-54.1271488070488,
-0.9));
#81731=CARTESIAN_POINT('Ctrl Pts',(-2.26473424583673,-53.902182996273,-0.9));
#81732=CARTESIAN_POINT('Ctrl Pts',(-2.26473424583673,-53.2620738148689,
-0.9));
#81733=CARTESIAN_POINT('Origin',(-3.15184209495783,-53.0289907455444,-0.9));
#81734=CARTESIAN_POINT('Origin',(-10.6418142095208,-53.190177500248,-0.6));
#81735=CARTESIAN_POINT('',(-10.6418142095208,-53.190177500248,-0.6));
#81736=CARTESIAN_POINT('',(-11.1636433377862,-53.190177500248,-0.6));
#81737=CARTESIAN_POINT('',(-5.32090710476041,-53.190177500248,-0.6));
#81738=CARTESIAN_POINT('',(-10.6418142095208,-53.190177500248,-0.9));
#81739=CARTESIAN_POINT('',(-10.6418142095208,-53.190177500248,-0.6));
#81740=CARTESIAN_POINT('',(-11.1636433377862,-53.190177500248,-0.9));
#81741=CARTESIAN_POINT('',(-10.6418142095208,-53.190177500248,-0.9));
#81742=CARTESIAN_POINT('',(-11.1636433377862,-53.190177500248,-0.6));
#81743=CARTESIAN_POINT('Ctrl Pts',(-10.3913364186883,-53.2064120173454,
-0.6));
#81744=CARTESIAN_POINT('Ctrl Pts',(-10.3913364186883,-53.2064120173454,
-0.9));
#81745=CARTESIAN_POINT('Ctrl Pts',(-10.4678711667657,-53.190177500248,-0.6));
#81746=CARTESIAN_POINT('Ctrl Pts',(-10.4678711667657,-53.190177500248,-0.9));
#81747=CARTESIAN_POINT('Ctrl Pts',(-10.6418142095208,-53.190177500248,-0.6));
#81748=CARTESIAN_POINT('Ctrl Pts',(-10.6418142095208,-53.190177500248,-0.9));
#81749=CARTESIAN_POINT('',(-10.3913364186883,-53.2064120173454,-0.6));
#81750=CARTESIAN_POINT('Ctrl Pts',(-10.3913364186883,-53.2064120173454,
-0.6));
#81751=CARTESIAN_POINT('Ctrl Pts',(-10.4678711667657,-53.190177500248,-0.6));
#81752=CARTESIAN_POINT('Ctrl Pts',(-10.6418142095208,-53.190177500248,-0.6));
#81753=CARTESIAN_POINT('',(-10.3913364186883,-53.2064120173454,-0.9));
#81754=CARTESIAN_POINT('',(-10.3913364186883,-53.2064120173454,-0.6));
#81755=CARTESIAN_POINT('Ctrl Pts',(-10.3913364186883,-53.2064120173454,
-0.9));
#81756=CARTESIAN_POINT('Ctrl Pts',(-10.4678711667657,-53.190177500248,-0.9));
#81757=CARTESIAN_POINT('Ctrl Pts',(-10.6418142095208,-53.190177500248,-0.9));
#81758=CARTESIAN_POINT('Ctrl Pts',(-10.1860842481256,-53.2968620657921,
-0.6));
#81759=CARTESIAN_POINT('Ctrl Pts',(-10.1860842481256,-53.2968620657921,
-0.9));
#81760=CARTESIAN_POINT('Ctrl Pts',(-10.2869710698724,-53.2319239974022,
-0.6));
#81761=CARTESIAN_POINT('Ctrl Pts',(-10.2869710698724,-53.2319239974022,
-0.9));
#81762=CARTESIAN_POINT('Ctrl Pts',(-10.3913364186883,-53.2064120173454,
-0.6));
#81763=CARTESIAN_POINT('Ctrl Pts',(-10.3913364186883,-53.2064120173454,
-0.9));
#81764=CARTESIAN_POINT('',(-10.1860842481256,-53.2968620657921,-0.6));
#81765=CARTESIAN_POINT('Ctrl Pts',(-10.1860842481256,-53.2968620657921,
-0.6));
#81766=CARTESIAN_POINT('Ctrl Pts',(-10.2869710698724,-53.2319239974022,
-0.6));
#81767=CARTESIAN_POINT('Ctrl Pts',(-10.3913364186883,-53.2064120173454,
-0.6));
#81768=CARTESIAN_POINT('',(-10.1860842481256,-53.2968620657921,-0.9));
#81769=CARTESIAN_POINT('',(-10.1860842481256,-53.2968620657921,-0.6));
#81770=CARTESIAN_POINT('Ctrl Pts',(-10.1860842481256,-53.2968620657921,
-0.9));
#81771=CARTESIAN_POINT('Ctrl Pts',(-10.2869710698724,-53.2319239974022,
-0.9));
#81772=CARTESIAN_POINT('Ctrl Pts',(-10.3913364186883,-53.2064120173454,
-0.9));
#81773=CARTESIAN_POINT('Ctrl Pts',(-9.9576411023736,-53.5241476893425,-0.6));
#81774=CARTESIAN_POINT('Ctrl Pts',(-9.9576411023736,-53.5241476893425,-0.9));
#81775=CARTESIAN_POINT('Ctrl Pts',(-10.0851974263787,-53.3618007302284,
-0.6));
#81776=CARTESIAN_POINT('Ctrl Pts',(-10.0851974263787,-53.3618007302284,
-0.9));
#81777=CARTESIAN_POINT('Ctrl Pts',(-10.1860842481256,-53.2968620657921,
-0.6));
#81778=CARTESIAN_POINT('Ctrl Pts',(-10.1860842481256,-53.2968620657921,
-0.9));
#81779=CARTESIAN_POINT('',(-9.9576411023736,-53.5241476893425,-0.6));
#81780=CARTESIAN_POINT('Ctrl Pts',(-9.9576411023736,-53.5241476893425,-0.6));
#81781=CARTESIAN_POINT('Ctrl Pts',(-10.0851974263787,-53.3618007302284,
-0.6));
#81782=CARTESIAN_POINT('Ctrl Pts',(-10.1860842481256,-53.2968620657921,
-0.6));
#81783=CARTESIAN_POINT('',(-9.9576411023736,-53.5241476893425,-0.9));
#81784=CARTESIAN_POINT('',(-9.9576411023736,-53.5241476893425,-0.6));
#81785=CARTESIAN_POINT('Ctrl Pts',(-9.9576411023736,-53.5241476893425,-0.9));
#81786=CARTESIAN_POINT('Ctrl Pts',(-10.0851974263787,-53.3618007302284,
-0.9));
#81787=CARTESIAN_POINT('Ctrl Pts',(-10.1860842481256,-53.2968620657921,
-0.9));
#81788=CARTESIAN_POINT('Ctrl Pts',(-9.63294837623835,-53.9926330447197,
-0.6));
#81789=CARTESIAN_POINT('Ctrl Pts',(-9.63294837623835,-53.9926330447197,
-0.9));
#81790=CARTESIAN_POINT('Ctrl Pts',(-9.83008239418268,-53.6864940524101,
-0.6));
#81791=CARTESIAN_POINT('Ctrl Pts',(-9.83008239418268,-53.6864940524101,
-0.9));
#81792=CARTESIAN_POINT('Ctrl Pts',(-9.9576411023736,-53.5241476893425,-0.6));
#81793=CARTESIAN_POINT('Ctrl Pts',(-9.9576411023736,-53.5241476893425,-0.9));
#81794=CARTESIAN_POINT('',(-9.63294837623835,-53.9926330447197,-0.6));
#81795=CARTESIAN_POINT('Ctrl Pts',(-9.63294837623835,-53.9926330447197,
-0.6));
#81796=CARTESIAN_POINT('Ctrl Pts',(-9.83008239418268,-53.6864940524101,
-0.6));
#81797=CARTESIAN_POINT('Ctrl Pts',(-9.9576411023736,-53.5241476893425,-0.6));
#81798=CARTESIAN_POINT('',(-9.63294837623835,-53.9926330447197,-0.9));
#81799=CARTESIAN_POINT('',(-9.63294837623835,-53.9926330447197,-0.6));
#81800=CARTESIAN_POINT('Ctrl Pts',(-9.63294837623835,-53.9926330447197,
-0.9));
#81801=CARTESIAN_POINT('Ctrl Pts',(-9.83008239418268,-53.6864940524101,
-0.9));
#81802=CARTESIAN_POINT('Ctrl Pts',(-9.9576411023736,-53.5241476893425,-0.9));
#81803=CARTESIAN_POINT('Origin',(-9.18301437050104,-54.7000001072884,-0.6));
#81804=CARTESIAN_POINT('',(-9.18301437050104,-54.7000001072884,-0.6));
#81805=CARTESIAN_POINT('',(-8.24537770178333,-56.174112505218,-0.6));
#81806=CARTESIAN_POINT('',(-9.18301437050104,-54.7000001072884,-0.9));
#81807=CARTESIAN_POINT('',(-9.18301437050104,-54.7000001072884,-0.6));
#81808=CARTESIAN_POINT('',(-9.18301437050104,-54.7000001072884,-0.9));
#81809=CARTESIAN_POINT('Origin',(-8.6171231046319,-54.7000001072884,-0.6));
#81810=CARTESIAN_POINT('',(-8.6171231046319,-54.7000001072884,-0.6));
#81811=CARTESIAN_POINT('',(-4.30856155231595,-54.7000001072884,-0.6));
#81812=CARTESIAN_POINT('',(-8.6171231046319,-54.7000001072884,-0.9));
#81813=CARTESIAN_POINT('',(-8.6171231046319,-54.7000001072884,-0.6));
#81814=CARTESIAN_POINT('',(-8.6171231046319,-54.7000001072884,-0.9));
#81815=CARTESIAN_POINT('Origin',(-9.2085275426507,-53.7746248841286,-0.6));
#81816=CARTESIAN_POINT('',(-9.2085275426507,-53.7746248841286,-0.6));
#81817=CARTESIAN_POINT('',(-8.0490517968636,-55.5888657961523,-0.6));
#81818=CARTESIAN_POINT('',(-9.2085275426507,-53.7746248841286,-0.9));
#81819=CARTESIAN_POINT('',(-9.2085275426507,-53.7746248841286,-0.6));
#81820=CARTESIAN_POINT('',(-9.2085275426507,-53.7746248841286,-0.9));
#81821=CARTESIAN_POINT('Ctrl Pts',(-9.58192441612482,-53.3223740458488,
-0.6));
#81822=CARTESIAN_POINT('Ctrl Pts',(-9.58192441612482,-53.3223740458488,
-0.9));
#81823=CARTESIAN_POINT('Ctrl Pts',(-9.38478801399469,-53.5032741427422,
-0.6));
#81824=CARTESIAN_POINT('Ctrl Pts',(-9.38478801399469,-53.5032741427422,
-0.9));
#81825=CARTESIAN_POINT('Ctrl Pts',(-9.2085275426507,-53.7746248841286,-0.6));
#81826=CARTESIAN_POINT('Ctrl Pts',(-9.2085275426507,-53.7746248841286,-0.9));
#81827=CARTESIAN_POINT('',(-9.58192441612482,-53.3223740458488,-0.6));
#81828=CARTESIAN_POINT('Ctrl Pts',(-9.58192441612482,-53.3223740458488,
-0.6));
#81829=CARTESIAN_POINT('Ctrl Pts',(-9.38478801399469,-53.5032741427422,
-0.6));
#81830=CARTESIAN_POINT('Ctrl Pts',(-9.2085275426507,-53.7746248841286,-0.6));
#81831=CARTESIAN_POINT('',(-9.58192441612482,-53.3223740458488,-0.9));
#81832=CARTESIAN_POINT('',(-9.58192441612482,-53.3223740458488,-0.6));
#81833=CARTESIAN_POINT('Ctrl Pts',(-9.58192441612482,-53.3223740458488,
-0.9));
#81834=CARTESIAN_POINT('Ctrl Pts',(-9.38478801399469,-53.5032741427422,
-0.9));
#81835=CARTESIAN_POINT('Ctrl Pts',(-9.2085275426507,-53.7746248841286,-0.9));
#81836=CARTESIAN_POINT('Ctrl Pts',(-9.85327575355768,-53.1530694365501,
-0.6));
#81837=CARTESIAN_POINT('Ctrl Pts',(-9.85327575355768,-53.1530694365501,
-0.9));
#81838=CARTESIAN_POINT('Ctrl Pts',(-9.67469308525324,-53.2388810515404,
-0.6));
#81839=CARTESIAN_POINT('Ctrl Pts',(-9.67469308525324,-53.2388810515404,
-0.9));
#81840=CARTESIAN_POINT('Ctrl Pts',(-9.58192441612482,-53.3223740458488,
-0.6));
#81841=CARTESIAN_POINT('Ctrl Pts',(-9.58192441612482,-53.3223740458488,
-0.9));
#81842=CARTESIAN_POINT('',(-9.85327575355768,-53.1530694365501,-0.6));
#81843=CARTESIAN_POINT('Ctrl Pts',(-9.85327575355768,-53.1530694365501,
-0.6));
#81844=CARTESIAN_POINT('Ctrl Pts',(-9.67469308525324,-53.2388810515404,
-0.6));
#81845=CARTESIAN_POINT('Ctrl Pts',(-9.58192441612482,-53.3223740458488,
-0.6));
#81846=CARTESIAN_POINT('',(-9.85327575355768,-53.1530694365501,-0.9));
#81847=CARTESIAN_POINT('',(-9.85327575355768,-53.1530694365501,-0.6));
#81848=CARTESIAN_POINT('Ctrl Pts',(-9.85327575355768,-53.1530694365501,
-0.9));
#81849=CARTESIAN_POINT('Ctrl Pts',(-9.67469308525324,-53.2388810515404,
-0.9));
#81850=CARTESIAN_POINT('Ctrl Pts',(-9.58192441612482,-53.3223740458488,
-0.9));
#81851=CARTESIAN_POINT('Ctrl Pts',(-9.12967298179865,-52.8376535773277,
-0.6));
#81852=CARTESIAN_POINT('Ctrl Pts',(-9.12967298179865,-52.8376535773277,
-0.9));
#81853=CARTESIAN_POINT('Ctrl Pts',(-9.36391685158014,-53.0858115553856,
-0.6));
#81854=CARTESIAN_POINT('Ctrl Pts',(-9.36391685158014,-53.0858115553856,
-0.9));
#81855=CARTESIAN_POINT('Ctrl Pts',(-9.85327575355768,-53.1530694365501,
-0.6));
#81856=CARTESIAN_POINT('Ctrl Pts',(-9.85327575355768,-53.1530694365501,
-0.9));
#81857=CARTESIAN_POINT('',(-9.12967298179865,-52.8376535773277,-0.6));
#81858=CARTESIAN_POINT('Ctrl Pts',(-9.12967298179865,-52.8376535773277,
-0.6));
#81859=CARTESIAN_POINT('Ctrl Pts',(-9.36391685158014,-53.0858115553856,
-0.6));
#81860=CARTESIAN_POINT('Ctrl Pts',(-9.85327575355768,-53.1530694365501,
-0.6));
#81861=CARTESIAN_POINT('',(-9.12967298179865,-52.8376535773277,-0.9));
#81862=CARTESIAN_POINT('',(-9.12967298179865,-52.8376535773277,-0.6));
#81863=CARTESIAN_POINT('Ctrl Pts',(-9.12967298179865,-52.8376535773277,
-0.9));
#81864=CARTESIAN_POINT('Ctrl Pts',(-9.36391685158014,-53.0858115553856,
-0.9));
#81865=CARTESIAN_POINT('Ctrl Pts',(-9.85327575355768,-53.1530694365501,
-0.9));
#81866=CARTESIAN_POINT('Ctrl Pts',(-8.89542911201715,-52.2276942133904,
-0.6));
#81867=CARTESIAN_POINT('Ctrl Pts',(-8.89542911201715,-52.2276942133904,
-0.9));
#81868=CARTESIAN_POINT('Ctrl Pts',(-8.89542911201715,-52.5894955992699,
-0.6));
#81869=CARTESIAN_POINT('Ctrl Pts',(-8.89542911201715,-52.5894955992699,
-0.9));
#81870=CARTESIAN_POINT('Ctrl Pts',(-9.12967298179865,-52.8376535773277,
-0.6));
#81871=CARTESIAN_POINT('Ctrl Pts',(-9.12967298179865,-52.8376535773277,
-0.9));
#81872=CARTESIAN_POINT('',(-8.89542911201715,-52.2276942133904,-0.6));
#81873=CARTESIAN_POINT('Ctrl Pts',(-8.89542911201715,-52.2276942133904,
-0.6));
#81874=CARTESIAN_POINT('Ctrl Pts',(-8.89542911201715,-52.5894955992699,
-0.6));
#81875=CARTESIAN_POINT('Ctrl Pts',(-9.12967298179865,-52.8376535773277,
-0.6));
#81876=CARTESIAN_POINT('',(-8.89542911201715,-52.2276942133904,-0.9));
#81877=CARTESIAN_POINT('',(-8.89542911201715,-52.2276942133904,-0.6));
#81878=CARTESIAN_POINT('Ctrl Pts',(-8.89542911201715,-52.2276942133904,
-0.9));
#81879=CARTESIAN_POINT('Ctrl Pts',(-8.89542911201715,-52.5894955992699,
-0.9));
#81880=CARTESIAN_POINT('Ctrl Pts',(-9.12967298179865,-52.8376535773277,
-0.9));
#81881=CARTESIAN_POINT('Ctrl Pts',(-9.03690431267023,-51.7151431441307,
-0.6));
#81882=CARTESIAN_POINT('Ctrl Pts',(-9.03690431267023,-51.7151431441307,
-0.9));
#81883=CARTESIAN_POINT('Ctrl Pts',(-8.89542911201715,-51.9470672011375,
-0.6));
#81884=CARTESIAN_POINT('Ctrl Pts',(-8.89542911201715,-51.9470672011375,
-0.9));
#81885=CARTESIAN_POINT('Ctrl Pts',(-8.89542911201715,-52.2276942133904,
-0.6));
#81886=CARTESIAN_POINT('Ctrl Pts',(-8.89542911201715,-52.2276942133904,
-0.9));
#81887=CARTESIAN_POINT('',(-9.03690431267023,-51.7151431441307,-0.6));
#81888=CARTESIAN_POINT('Ctrl Pts',(-9.03690431267023,-51.7151431441307,
-0.6));
#81889=CARTESIAN_POINT('Ctrl Pts',(-8.89542911201715,-51.9470672011375,
-0.6));
#81890=CARTESIAN_POINT('Ctrl Pts',(-8.89542911201715,-52.2276942133904,
-0.6));
#81891=CARTESIAN_POINT('',(-9.03690431267023,-51.7151431441307,-0.9));
#81892=CARTESIAN_POINT('',(-9.03690431267023,-51.7151431441307,-0.6));
#81893=CARTESIAN_POINT('Ctrl Pts',(-9.03690431267023,-51.7151431441307,
-0.9));
#81894=CARTESIAN_POINT('Ctrl Pts',(-8.89542911201715,-51.9470672011375,
-0.9));
#81895=CARTESIAN_POINT('Ctrl Pts',(-8.89542911201715,-52.2276942133904,
-0.9));
#81896=CARTESIAN_POINT('Ctrl Pts',(-9.41493842750788,-51.3916097283363,
-0.6));
#81897=CARTESIAN_POINT('Ctrl Pts',(-9.41493842750788,-51.3916097283363,
-0.9));
#81898=CARTESIAN_POINT('Ctrl Pts',(-9.17837712913752,-51.4832196831703,
-0.6));
#81899=CARTESIAN_POINT('Ctrl Pts',(-9.17837712913752,-51.4832196831703,
-0.9));
#81900=CARTESIAN_POINT('Ctrl Pts',(-9.03690431267023,-51.7151431441307,
-0.6));
#81901=CARTESIAN_POINT('Ctrl Pts',(-9.03690431267023,-51.7151431441307,
-0.9));
#81902=CARTESIAN_POINT('',(-9.41493842750788,-51.3916097283363,-0.6));
#81903=CARTESIAN_POINT('Ctrl Pts',(-9.41493842750788,-51.3916097283363,
-0.6));
#81904=CARTESIAN_POINT('Ctrl Pts',(-9.17837712913752,-51.4832196831703,
-0.6));
#81905=CARTESIAN_POINT('Ctrl Pts',(-9.03690431267023,-51.7151431441307,
-0.6));
#81906=CARTESIAN_POINT('',(-9.41493842750788,-51.3916097283363,-0.9));
#81907=CARTESIAN_POINT('',(-9.41493842750788,-51.3916097283363,-0.6));
#81908=CARTESIAN_POINT('Ctrl Pts',(-9.41493842750788,-51.3916097283363,
-0.9));
#81909=CARTESIAN_POINT('Ctrl Pts',(-9.17837712913752,-51.4832196831703,
-0.9));
#81910=CARTESIAN_POINT('Ctrl Pts',(-9.03690431267023,-51.7151431441307,
-0.9));
#81911=CARTESIAN_POINT('Ctrl Pts',(-10.1060709729791,-51.3000003695488,
-0.6));
#81912=CARTESIAN_POINT('Ctrl Pts',(-10.1060709729791,-51.3000003695488,
-0.9));
#81913=CARTESIAN_POINT('Ctrl Pts',(-9.65150211006403,-51.3000003695488,
-0.6));
#81914=CARTESIAN_POINT('Ctrl Pts',(-9.65150211006403,-51.3000003695488,
-0.9));
#81915=CARTESIAN_POINT('Ctrl Pts',(-9.41493842750788,-51.3916097283363,
-0.6));
#81916=CARTESIAN_POINT('Ctrl Pts',(-9.41493842750788,-51.3916097283363,
-0.9));
#81917=CARTESIAN_POINT('',(-10.1060709729791,-51.3000003695488,-0.6));
#81918=CARTESIAN_POINT('Ctrl Pts',(-10.1060709729791,-51.3000003695488,
-0.6));
#81919=CARTESIAN_POINT('Ctrl Pts',(-9.65150211006403,-51.3000003695488,
-0.6));
#81920=CARTESIAN_POINT('Ctrl Pts',(-9.41493842750788,-51.3916097283363,
-0.6));
#81921=CARTESIAN_POINT('',(-10.1060709729791,-51.3000003695488,-0.9));
#81922=CARTESIAN_POINT('',(-10.1060709729791,-51.3000003695488,-0.6));
#81923=CARTESIAN_POINT('Ctrl Pts',(-10.1060709729791,-51.3000003695488,
-0.9));
#81924=CARTESIAN_POINT('Ctrl Pts',(-9.65150211006403,-51.3000003695488,
-0.9));
#81925=CARTESIAN_POINT('Ctrl Pts',(-9.41493842750788,-51.3916097283363,
-0.9));
#81926=CARTESIAN_POINT('Origin',(-11.6135749593377,-51.3000003695488,-0.6));
#81927=CARTESIAN_POINT('',(-11.6135749593377,-51.3000003695488,-0.6));
#81928=CARTESIAN_POINT('',(-5.80678747966886,-51.3000003695488,-0.6));
#81929=CARTESIAN_POINT('',(-11.6135749593377,-51.3000003695488,-0.9));
#81930=CARTESIAN_POINT('',(-11.6135749593377,-51.3000003695488,-0.6));
#81931=CARTESIAN_POINT('',(-11.6135749593377,-51.3000003695488,-0.9));
#81932=CARTESIAN_POINT('Origin',(-11.6135749593377,-54.7000001072884,-0.6));
#81933=CARTESIAN_POINT('',(-11.6135749593377,-54.7000001072884,-0.6));
#81934=CARTESIAN_POINT('',(-11.6135749593377,-53.8500000536442,-0.6));
#81935=CARTESIAN_POINT('',(-11.6135749593377,-54.7000001072884,-0.9));
#81936=CARTESIAN_POINT('',(-11.6135749593377,-54.7000001072884,-0.6));
#81937=CARTESIAN_POINT('',(-11.6135749593377,-54.7000001072884,-0.9));
#81938=CARTESIAN_POINT('Origin',(-11.1636433377862,-54.7000001072884,-0.6));
#81939=CARTESIAN_POINT('',(-11.1636433377862,-54.7000001072884,-0.6));
#81940=CARTESIAN_POINT('',(-5.5818216688931,-54.7000001072884,-0.6));
#81941=CARTESIAN_POINT('',(-11.1636433377862,-54.7000001072884,-0.9));
#81942=CARTESIAN_POINT('',(-11.1636433377862,-54.7000001072884,-0.6));
#81943=CARTESIAN_POINT('',(-11.1636433377862,-54.7000001072884,-0.9));
#81944=CARTESIAN_POINT('Origin',(-11.1636433377862,-53.190177500248,-0.6));
#81945=CARTESIAN_POINT('',(-11.1636433377862,-53.095088750124,-0.6));
#81946=CARTESIAN_POINT('',(-11.1636433377862,-53.190177500248,-0.9));
#81947=CARTESIAN_POINT('Origin',(-10.1153490319848,-53.0000002384186,-0.9));
#81948=CARTESIAN_POINT('Origin',(-15.6907925382257,-51.7012278437614,-0.6));
#81949=CARTESIAN_POINT('',(-15.6907925382257,-51.7012278437614,-0.6));
#81950=CARTESIAN_POINT('',(-16.8156227841973,-51.7012278437614,-0.6));
#81951=CARTESIAN_POINT('',(-7.84539626911283,-51.7012278437614,-0.6));
#81952=CARTESIAN_POINT('',(-15.6907925382257,-51.7012278437614,-0.9));
#81953=CARTESIAN_POINT('',(-15.6907925382257,-51.7012278437614,-0.6));
#81954=CARTESIAN_POINT('',(-16.8156227841973,-51.7012278437614,-0.9));
#81955=CARTESIAN_POINT('',(-15.6907925382257,-51.7012278437614,-0.9));
#81956=CARTESIAN_POINT('',(-16.8156227841973,-51.7012278437614,-0.6));
#81957=CARTESIAN_POINT('Origin',(-15.6907925382257,-51.3000003695488,-0.6));
#81958=CARTESIAN_POINT('',(-15.6907925382257,-51.3000003695488,-0.6));
#81959=CARTESIAN_POINT('',(-15.6907925382257,-52.1500001847744,-0.6));
#81960=CARTESIAN_POINT('',(-15.6907925382257,-51.3000003695488,-0.9));
#81961=CARTESIAN_POINT('',(-15.6907925382257,-51.3000003695488,-0.6));
#81962=CARTESIAN_POINT('',(-15.6907925382257,-51.3000003695488,-0.9));
#81963=CARTESIAN_POINT('Origin',(-18.3857450261712,-51.3000003695488,-0.6));
#81964=CARTESIAN_POINT('',(-18.3857450261712,-51.3000003695488,-0.6));
#81965=CARTESIAN_POINT('',(-9.1928725130856,-51.3000003695488,-0.6));
#81966=CARTESIAN_POINT('',(-18.3857450261712,-51.3000003695488,-0.9));
#81967=CARTESIAN_POINT('',(-18.3857450261712,-51.3000003695488,-0.6));
#81968=CARTESIAN_POINT('',(-18.3857450261712,-51.3000003695488,-0.9));
#81969=CARTESIAN_POINT('Origin',(-18.3857450261712,-51.7012278437614,-0.6));
#81970=CARTESIAN_POINT('',(-18.3857450261712,-51.7012278437614,-0.6));
#81971=CARTESIAN_POINT('',(-18.3857450261712,-52.3506139218807,-0.6));
#81972=CARTESIAN_POINT('',(-18.3857450261712,-51.7012278437614,-0.9));
#81973=CARTESIAN_POINT('',(-18.3857450261712,-51.7012278437614,-0.6));
#81974=CARTESIAN_POINT('',(-18.3857450261712,-51.7012278437614,-0.9));
#81975=CARTESIAN_POINT('Origin',(-17.2655544057488,-51.7012278437614,-0.6));
#81976=CARTESIAN_POINT('',(-17.2655544057488,-51.7012278437614,-0.6));
#81977=CARTESIAN_POINT('',(-8.63277720287442,-51.7012278437614,-0.6));
#81978=CARTESIAN_POINT('',(-17.2655544057488,-51.7012278437614,-0.9));
#81979=CARTESIAN_POINT('',(-17.2655544057488,-51.7012278437614,-0.6));
#81980=CARTESIAN_POINT('',(-17.2655544057488,-51.7012278437614,-0.9));
#81981=CARTESIAN_POINT('Origin',(-17.2655544057488,-54.7000001072884,-0.6));
#81982=CARTESIAN_POINT('',(-17.2655544057488,-54.7000001072884,-0.6));
#81983=CARTESIAN_POINT('',(-17.2655544057488,-53.8500000536442,-0.6));
#81984=CARTESIAN_POINT('',(-17.2655544057488,-54.7000001072884,-0.9));
#81985=CARTESIAN_POINT('',(-17.2655544057488,-54.7000001072884,-0.6));
#81986=CARTESIAN_POINT('',(-17.2655544057488,-54.7000001072884,-0.9));
#81987=CARTESIAN_POINT('Origin',(-16.8156227841973,-54.7000001072884,-0.6));
#81988=CARTESIAN_POINT('',(-16.8156227841973,-54.7000001072884,-0.6));
#81989=CARTESIAN_POINT('',(-8.40781139209867,-54.7000001072884,-0.6));
#81990=CARTESIAN_POINT('',(-16.8156227841973,-54.7000001072884,-0.9));
#81991=CARTESIAN_POINT('',(-16.8156227841973,-54.7000001072884,-0.6));
#81992=CARTESIAN_POINT('',(-16.8156227841973,-54.7000001072884,-0.9));
#81993=CARTESIAN_POINT('Origin',(-16.8156227841973,-51.7012278437614,-0.6));
#81994=CARTESIAN_POINT('',(-16.8156227841973,-52.3506139218807,-0.6));
#81995=CARTESIAN_POINT('',(-16.8156227841973,-51.7012278437614,-0.9));
#81996=CARTESIAN_POINT('Origin',(-17.0382687821984,-53.0000002384186,-0.9));
#81997=CARTESIAN_POINT('Ctrl Pts',(-23.8846537843347,-51.7406551241875,
-0.6));
#81998=CARTESIAN_POINT('Ctrl Pts',(-23.8846537843347,-51.7406551241875,
-0.9));
#81999=CARTESIAN_POINT('Ctrl Pts',(-23.6225793138146,-51.5064118504524,
-0.6));
#82000=CARTESIAN_POINT('Ctrl Pts',(-23.6225793138146,-51.5064118504524,
-0.9));
#82001=CARTESIAN_POINT('Ctrl Pts',(-23.5135755315423,-51.2860844731331,
-0.6));
#82002=CARTESIAN_POINT('Ctrl Pts',(-23.5135755315423,-51.2860844731331,
-0.9));
#82003=CARTESIAN_POINT('',(-23.8846537843347,-51.7406551241875,-0.6));
#82004=CARTESIAN_POINT('',(-23.5135755315423,-51.2860844731331,-0.6));
#82005=CARTESIAN_POINT('Ctrl Pts',(-23.8846537843347,-51.7406551241875,
-0.6));
#82006=CARTESIAN_POINT('Ctrl Pts',(-23.6225793138146,-51.5064118504524,
-0.6));
#82007=CARTESIAN_POINT('Ctrl Pts',(-23.5135755315423,-51.2860844731331,
-0.6));
#82008=CARTESIAN_POINT('',(-23.8846537843347,-51.7406551241875,-0.9));
#82009=CARTESIAN_POINT('',(-23.8846537843347,-51.7406551241875,-0.6));
#82010=CARTESIAN_POINT('',(-23.5135755315423,-51.2860844731331,-0.9));
#82011=CARTESIAN_POINT('Ctrl Pts',(-23.8846537843347,-51.7406551241875,
-0.9));
#82012=CARTESIAN_POINT('Ctrl Pts',(-23.6225793138146,-51.5064118504524,
-0.9));
#82013=CARTESIAN_POINT('Ctrl Pts',(-23.5135755315423,-51.2860844731331,
-0.9));
#82014=CARTESIAN_POINT('',(-23.5135755315423,-51.2860844731331,-0.6));
#82015=CARTESIAN_POINT('Ctrl Pts',(-24.4969317689538,-52.1395633816719,
-0.6));
#82016=CARTESIAN_POINT('Ctrl Pts',(-24.4969317689538,-52.1395633816719,
-0.9));
#82017=CARTESIAN_POINT('Ctrl Pts',(-24.1467270627618,-51.9748978018761,
-0.6));
#82018=CARTESIAN_POINT('Ctrl Pts',(-24.1467270627618,-51.9748978018761,
-0.9));
#82019=CARTESIAN_POINT('Ctrl Pts',(-23.8846537843347,-51.7406551241875,
-0.6));
#82020=CARTESIAN_POINT('Ctrl Pts',(-23.8846537843347,-51.7406551241875,
-0.9));
#82021=CARTESIAN_POINT('',(-24.4969317689538,-52.1395633816719,-0.6));
#82022=CARTESIAN_POINT('Ctrl Pts',(-24.4969317689538,-52.1395633816719,
-0.6));
#82023=CARTESIAN_POINT('Ctrl Pts',(-24.1467270627618,-51.9748978018761,
-0.6));
#82024=CARTESIAN_POINT('Ctrl Pts',(-23.8846537843347,-51.7406551241875,
-0.6));
#82025=CARTESIAN_POINT('',(-24.4969317689538,-52.1395633816719,-0.9));
#82026=CARTESIAN_POINT('',(-24.4969317689538,-52.1395633816719,-0.6));
#82027=CARTESIAN_POINT('Ctrl Pts',(-24.4969317689538,-52.1395633816719,
-0.9));
#82028=CARTESIAN_POINT('Ctrl Pts',(-24.1467270627618,-51.9748978018761,
-0.9));
#82029=CARTESIAN_POINT('Ctrl Pts',(-23.8846537843347,-51.7406551241875,
-0.9));
#82030=CARTESIAN_POINT('Origin',(-24.4969317689538,-52.5431100726128,-0.6));
#82031=CARTESIAN_POINT('',(-24.4969317689538,-52.5431100726128,-0.6));
#82032=CARTESIAN_POINT('',(-24.4969317689538,-52.7715550363062,-0.6));
#82033=CARTESIAN_POINT('',(-24.4969317689538,-52.5431100726128,-0.9));
#82034=CARTESIAN_POINT('',(-24.4969317689538,-52.5431100726128,-0.6));
#82035=CARTESIAN_POINT('',(-24.4969317689538,-52.5431100726128,-0.9));
#82036=CARTESIAN_POINT('Ctrl Pts',(-24.0574369207025,-52.3274211287498,
-0.6));
#82037=CARTESIAN_POINT('Ctrl Pts',(-24.0574369207025,-52.3274211287498,
-0.9));
#82038=CARTESIAN_POINT('Ctrl Pts',(-24.3021163716912,-52.4712137579918,
-0.6));
#82039=CARTESIAN_POINT('Ctrl Pts',(-24.3021163716912,-52.4712137579918,
-0.9));
#82040=CARTESIAN_POINT('Ctrl Pts',(-24.4969317689538,-52.5431100726128,
-0.6));
#82041=CARTESIAN_POINT('Ctrl Pts',(-24.4969317689538,-52.5431100726128,
-0.9));
#82042=CARTESIAN_POINT('',(-24.0574369207025,-52.3274211287498,-0.6));
#82043=CARTESIAN_POINT('Ctrl Pts',(-24.0574369207025,-52.3274211287498,
-0.6));
#82044=CARTESIAN_POINT('Ctrl Pts',(-24.3021163716912,-52.4712137579918,
-0.6));
#82045=CARTESIAN_POINT('Ctrl Pts',(-24.4969317689538,-52.5431100726128,
-0.6));
#82046=CARTESIAN_POINT('',(-24.0574369207025,-52.3274211287498,-0.9));
#82047=CARTESIAN_POINT('',(-24.0574369207025,-52.3274211287498,-0.6));
#82048=CARTESIAN_POINT('Ctrl Pts',(-24.0574369207025,-52.3274211287498,
-0.9));
#82049=CARTESIAN_POINT('Ctrl Pts',(-24.3021163716912,-52.4712137579918,
-0.9));
#82050=CARTESIAN_POINT('Ctrl Pts',(-24.4969317689538,-52.5431100726128,
-0.9));
#82051=CARTESIAN_POINT('Ctrl Pts',(-23.6620065942407,-52.039835870266,-0.6));
#82052=CARTESIAN_POINT('Ctrl Pts',(-23.6620065942407,-52.039835870266,-0.9));
#82053=CARTESIAN_POINT('Ctrl Pts',(-23.8127574697137,-52.1836284995079,
-0.6));
#82054=CARTESIAN_POINT('Ctrl Pts',(-23.8127574697137,-52.1836284995079,
-0.9));
#82055=CARTESIAN_POINT('Ctrl Pts',(-24.0574369207025,-52.3274211287498,
-0.6));
#82056=CARTESIAN_POINT('Ctrl Pts',(-24.0574369207025,-52.3274211287498,
-0.9));
#82057=CARTESIAN_POINT('',(-23.6620065942407,-52.039835870266,-0.6));
#82058=CARTESIAN_POINT('Ctrl Pts',(-23.6620065942407,-52.039835870266,-0.6));
#82059=CARTESIAN_POINT('Ctrl Pts',(-23.8127574697137,-52.1836284995079,
-0.6));
#82060=CARTESIAN_POINT('Ctrl Pts',(-24.0574369207025,-52.3274211287498,
-0.6));
#82061=CARTESIAN_POINT('',(-23.6620065942407,-52.039835870266,-0.9));
#82062=CARTESIAN_POINT('',(-23.6620065942407,-52.039835870266,-0.6));
#82063=CARTESIAN_POINT('Ctrl Pts',(-23.6620065942407,-52.039835870266,-0.9));
#82064=CARTESIAN_POINT('Ctrl Pts',(-23.8127574697137,-52.1836284995079,
-0.9));
#82065=CARTESIAN_POINT('Ctrl Pts',(-24.0574369207025,-52.3274211287498,
-0.9));
#82066=CARTESIAN_POINT('Origin',(-23.6620065942407,-54.7000001072884,-0.6));
#82067=CARTESIAN_POINT('',(-23.6620065942407,-54.7000001072884,-0.6));
#82068=CARTESIAN_POINT('',(-23.6620065942407,-53.8500000536442,-0.6));
#82069=CARTESIAN_POINT('',(-23.6620065942407,-54.7000001072884,-0.9));
#82070=CARTESIAN_POINT('',(-23.6620065942407,-54.7000001072884,-0.6));
#82071=CARTESIAN_POINT('',(-23.6620065942407,-54.7000001072884,-0.9));
#82072=CARTESIAN_POINT('Origin',(-23.2445440068841,-54.7000001072884,-0.6));
#82073=CARTESIAN_POINT('',(-23.2445440068841,-54.7000001072884,-0.6));
#82074=CARTESIAN_POINT('',(-11.622272003442,-54.7000001072884,-0.6));
#82075=CARTESIAN_POINT('',(-23.2445440068841,-54.7000001072884,-0.9));
#82076=CARTESIAN_POINT('',(-23.2445440068841,-54.7000001072884,-0.6));
#82077=CARTESIAN_POINT('',(-23.2445440068841,-54.7000001072884,-0.9));
#82078=CARTESIAN_POINT('Origin',(-23.2445440068841,-51.2860844731331,-0.6));
#82079=CARTESIAN_POINT('',(-23.2445440068841,-51.2860844731331,-0.6));
#82080=CARTESIAN_POINT('',(-23.2445440068841,-52.1430422365665,-0.6));
#82081=CARTESIAN_POINT('',(-23.2445440068841,-51.2860844731331,-0.9));
#82082=CARTESIAN_POINT('',(-23.2445440068841,-51.2860844731331,-0.6));
#82083=CARTESIAN_POINT('',(-23.2445440068841,-51.2860844731331,-0.9));
#82084=CARTESIAN_POINT('Origin',(-23.5135755315423,-51.2860844731331,-0.6));
#82085=CARTESIAN_POINT('',(-11.7567877657712,-51.2860844731331,-0.6));
#82086=CARTESIAN_POINT('',(-23.5135755315423,-51.2860844731331,-0.9));
#82087=CARTESIAN_POINT('Origin',(-23.8707378879189,-52.9930422902107,-0.9));
#82088=CARTESIAN_POINT('Ctrl Pts',(-27.3136434331536,-54.5573667883873,
-0.6));
#82089=CARTESIAN_POINT('Ctrl Pts',(-27.3136434331536,-54.5573667883873,
-0.9));
#82090=CARTESIAN_POINT('Ctrl Pts',(-27.5583228841424,-54.7579811215401,
-0.6));
#82091=CARTESIAN_POINT('Ctrl Pts',(-27.5583228841424,-54.7579811215401,
-0.9));
#82092=CARTESIAN_POINT('Ctrl Pts',(-27.9317197576165,-54.7579811215401,
-0.6));
#82093=CARTESIAN_POINT('Ctrl Pts',(-27.9317197576165,-54.7579811215401,
-0.9));
#82094=CARTESIAN_POINT('',(-27.3136434331536,-54.5573667883873,-0.6));
#82095=CARTESIAN_POINT('',(-27.9317197576165,-54.7579811215401,-0.6));
#82096=CARTESIAN_POINT('Ctrl Pts',(-27.3136434331536,-54.5573667883873,
-0.6));
#82097=CARTESIAN_POINT('Ctrl Pts',(-27.5583228841424,-54.7579811215401,
-0.6));
#82098=CARTESIAN_POINT('Ctrl Pts',(-27.9317197576165,-54.7579811215401,
-0.6));
#82099=CARTESIAN_POINT('',(-27.3136434331536,-54.5573667883873,-0.9));
#82100=CARTESIAN_POINT('',(-27.3136434331536,-54.5573667883873,-0.6));
#82101=CARTESIAN_POINT('',(-27.9317197576165,-54.7579811215401,-0.9));
#82102=CARTESIAN_POINT('Ctrl Pts',(-27.3136434331536,-54.5573667883873,
-0.9));
#82103=CARTESIAN_POINT('Ctrl Pts',(-27.5583228841424,-54.7579811215401,
-0.9));
#82104=CARTESIAN_POINT('Ctrl Pts',(-27.9317197576165,-54.7579811215401,
-0.9));
#82105=CARTESIAN_POINT('',(-27.9317197576165,-54.7579811215401,-0.6));
#82106=CARTESIAN_POINT('Ctrl Pts',(-26.9460448995233,-53.9891545176506,
-0.6));
#82107=CARTESIAN_POINT('Ctrl Pts',(-26.9460448995233,-53.9891545176506,
-0.9));
#82108=CARTESIAN_POINT('Ctrl Pts',(-27.0689639821649,-54.356753051281,-0.6));
#82109=CARTESIAN_POINT('Ctrl Pts',(-27.0689639821649,-54.356753051281,-0.9));
#82110=CARTESIAN_POINT('Ctrl Pts',(-27.3136434331536,-54.5573667883873,
-0.6));
#82111=CARTESIAN_POINT('Ctrl Pts',(-27.3136434331536,-54.5573667883873,
-0.9));
#82112=CARTESIAN_POINT('',(-26.9460448995233,-53.9891545176506,-0.6));
#82113=CARTESIAN_POINT('Ctrl Pts',(-26.9460448995233,-53.9891545176506,
-0.6));
#82114=CARTESIAN_POINT('Ctrl Pts',(-27.0689639821649,-54.356753051281,-0.6));
#82115=CARTESIAN_POINT('Ctrl Pts',(-27.3136434331536,-54.5573667883873,
-0.6));
#82116=CARTESIAN_POINT('',(-26.9460448995233,-53.9891545176506,-0.9));
#82117=CARTESIAN_POINT('',(-26.9460448995233,-53.9891545176506,-0.6));
#82118=CARTESIAN_POINT('Ctrl Pts',(-26.9460448995233,-53.9891545176506,
-0.9));
#82119=CARTESIAN_POINT('Ctrl Pts',(-27.0689639821649,-54.356753051281,-0.9));
#82120=CARTESIAN_POINT('Ctrl Pts',(-27.3136434331536,-54.5573667883873,
-0.9));
#82121=CARTESIAN_POINT('Ctrl Pts',(-26.8231252208352,-53.0231921076775,
-0.6));
#82122=CARTESIAN_POINT('Ctrl Pts',(-26.8231252208352,-53.0231921076775,
-0.9));
#82123=CARTESIAN_POINT('Ctrl Pts',(-26.8231252208352,-53.6215553879738,
-0.6));
#82124=CARTESIAN_POINT('Ctrl Pts',(-26.8231252208352,-53.6215553879738,
-0.9));
#82125=CARTESIAN_POINT('Ctrl Pts',(-26.9460448995233,-53.9891545176506,
-0.6));
#82126=CARTESIAN_POINT('Ctrl Pts',(-26.9460448995233,-53.9891545176506,
-0.9));
#82127=CARTESIAN_POINT('',(-26.8231252208352,-53.0231921076775,-0.6));
#82128=CARTESIAN_POINT('Ctrl Pts',(-26.8231252208352,-53.0231921076775,
-0.6));
#82129=CARTESIAN_POINT('Ctrl Pts',(-26.8231252208352,-53.6215553879738,
-0.6));
#82130=CARTESIAN_POINT('Ctrl Pts',(-26.9460448995233,-53.9891545176506,
-0.6));
#82131=CARTESIAN_POINT('',(-26.8231252208352,-53.0231921076775,-0.9));
#82132=CARTESIAN_POINT('',(-26.8231252208352,-53.0231921076775,-0.6));
#82133=CARTESIAN_POINT('Ctrl Pts',(-26.8231252208352,-53.0231921076775,
-0.9));
#82134=CARTESIAN_POINT('Ctrl Pts',(-26.8231252208352,-53.6215553879738,
-0.9));
#82135=CARTESIAN_POINT('Ctrl Pts',(-26.9460448995233,-53.9891545176506,
-0.9));
#82136=CARTESIAN_POINT('Ctrl Pts',(-26.8996599689126,-52.2195772528648,
-0.6));
#82137=CARTESIAN_POINT('Ctrl Pts',(-26.8996599689126,-52.2195772528648,
-0.9));
#82138=CARTESIAN_POINT('Ctrl Pts',(-26.8231252208352,-52.5175992846489,
-0.6));
#82139=CARTESIAN_POINT('Ctrl Pts',(-26.8231252208352,-52.5175992846489,
-0.9));
#82140=CARTESIAN_POINT('Ctrl Pts',(-26.8231252208352,-53.0231921076775,
-0.6));
#82141=CARTESIAN_POINT('Ctrl Pts',(-26.8231252208352,-53.0231921076775,
-0.9));
#82142=CARTESIAN_POINT('',(-26.8996599689126,-52.2195772528648,-0.6));
#82143=CARTESIAN_POINT('Ctrl Pts',(-26.8996599689126,-52.2195772528648,
-0.6));
#82144=CARTESIAN_POINT('Ctrl Pts',(-26.8231252208352,-52.5175992846489,
-0.6));
#82145=CARTESIAN_POINT('Ctrl Pts',(-26.8231252208352,-53.0231921076775,
-0.6));
#82146=CARTESIAN_POINT('',(-26.8996599689126,-52.2195772528648,-0.9));
#82147=CARTESIAN_POINT('',(-26.8996599689126,-52.2195772528648,-0.6));
#82148=CARTESIAN_POINT('Ctrl Pts',(-26.8996599689126,-52.2195772528648,
-0.9));
#82149=CARTESIAN_POINT('Ctrl Pts',(-26.8231252208352,-52.5175992846489,
-0.9));
#82150=CARTESIAN_POINT('Ctrl Pts',(-26.8231252208352,-53.0231921076775,
-0.9));
#82151=CARTESIAN_POINT('Ctrl Pts',(-27.1107104793191,-51.7139838337898,
-0.6));
#82152=CARTESIAN_POINT('Ctrl Pts',(-27.1107104793191,-51.7139838337898,
-0.9));
#82153=CARTESIAN_POINT('Ctrl Pts',(-26.97619471699,-51.9215552210808,-0.6));
#82154=CARTESIAN_POINT('Ctrl Pts',(-26.97619471699,-51.9215552210808,-0.9));
#82155=CARTESIAN_POINT('Ctrl Pts',(-26.8996599689126,-52.2195772528648,
-0.6));
#82156=CARTESIAN_POINT('Ctrl Pts',(-26.8996599689126,-52.2195772528648,
-0.9));
#82157=CARTESIAN_POINT('',(-27.1107104793191,-51.7139838337898,-0.6));
#82158=CARTESIAN_POINT('Ctrl Pts',(-27.1107104793191,-51.7139838337898,
-0.6));
#82159=CARTESIAN_POINT('Ctrl Pts',(-26.97619471699,-51.9215552210808,-0.6));
#82160=CARTESIAN_POINT('Ctrl Pts',(-26.8996599689126,-52.2195772528648,
-0.6));
#82161=CARTESIAN_POINT('',(-27.1107104793191,-51.7139838337898,-0.9));
#82162=CARTESIAN_POINT('',(-27.1107104793191,-51.7139838337898,-0.6));
#82163=CARTESIAN_POINT('Ctrl Pts',(-27.1107104793191,-51.7139838337898,
-0.9));
#82164=CARTESIAN_POINT('Ctrl Pts',(-26.97619471699,-51.9215552210808,-0.9));
#82165=CARTESIAN_POINT('Ctrl Pts',(-26.8996599689126,-52.2195772528648,
-0.9));
#82166=CARTESIAN_POINT('Ctrl Pts',(-27.4516383185983,-51.3962487578392,
-0.6));
#82167=CARTESIAN_POINT('Ctrl Pts',(-27.4516383185983,-51.3962487578392,
-0.9));
#82168=CARTESIAN_POINT('Ctrl Pts',(-27.2452262416482,-51.5064124464989,
-0.6));
#82169=CARTESIAN_POINT('Ctrl Pts',(-27.2452262416482,-51.5064124464989,
-0.9));
#82170=CARTESIAN_POINT('Ctrl Pts',(-27.1107104793191,-51.7139838337898,
-0.6));
#82171=CARTESIAN_POINT('Ctrl Pts',(-27.1107104793191,-51.7139838337898,
-0.9));
#82172=CARTESIAN_POINT('',(-27.4516383185983,-51.3962487578392,-0.6));
#82173=CARTESIAN_POINT('Ctrl Pts',(-27.4516383185983,-51.3962487578392,
-0.6));
#82174=CARTESIAN_POINT('Ctrl Pts',(-27.2452262416482,-51.5064124464989,
-0.6));
#82175=CARTESIAN_POINT('Ctrl Pts',(-27.1107104793191,-51.7139838337898,
-0.6));
#82176=CARTESIAN_POINT('',(-27.4516383185983,-51.3962487578392,-0.9));
#82177=CARTESIAN_POINT('',(-27.4516383185983,-51.3962487578392,-0.6));
#82178=CARTESIAN_POINT('Ctrl Pts',(-27.4516383185983,-51.3962487578392,
-0.9));
#82179=CARTESIAN_POINT('Ctrl Pts',(-27.2452262416482,-51.5064124464989,
-0.9));
#82180=CARTESIAN_POINT('Ctrl Pts',(-27.1107104793191,-51.7139838337898,
-0.9));
#82181=CARTESIAN_POINT('Ctrl Pts',(-27.9317197576165,-51.2860850691795,
-0.6));
#82182=CARTESIAN_POINT('Ctrl Pts',(-27.9317197576165,-51.2860850691795,
-0.9));
#82183=CARTESIAN_POINT('Ctrl Pts',(-27.6580503955483,-51.2860850691795,
-0.6));
#82184=CARTESIAN_POINT('Ctrl Pts',(-27.6580503955483,-51.2860850691795,
-0.9));
#82185=CARTESIAN_POINT('Ctrl Pts',(-27.4516383185983,-51.3962487578392,
-0.6));
#82186=CARTESIAN_POINT('Ctrl Pts',(-27.4516383185983,-51.3962487578392,
-0.9));
#82187=CARTESIAN_POINT('',(-27.9317197576165,-51.2860850691795,-0.6));
#82188=CARTESIAN_POINT('Ctrl Pts',(-27.9317197576165,-51.2860850691795,
-0.6));
#82189=CARTESIAN_POINT('Ctrl Pts',(-27.6580503955483,-51.2860850691795,
-0.6));
#82190=CARTESIAN_POINT('Ctrl Pts',(-27.4516383185983,-51.3962487578392,
-0.6));
#82191=CARTESIAN_POINT('',(-27.9317197576165,-51.2860850691795,-0.9));
#82192=CARTESIAN_POINT('',(-27.9317197576165,-51.2860850691795,-0.6));
#82193=CARTESIAN_POINT('Ctrl Pts',(-27.9317197576165,-51.2860850691795,
-0.9));
#82194=CARTESIAN_POINT('Ctrl Pts',(-27.6580503955483,-51.2860850691795,
-0.9));
#82195=CARTESIAN_POINT('Ctrl Pts',(-27.4516383185983,-51.3962487578392,
-0.9));
#82196=CARTESIAN_POINT('Ctrl Pts',(-28.5474774613976,-51.4855388998985,
-0.6));
#82197=CARTESIAN_POINT('Ctrl Pts',(-28.5474774613976,-51.4855388998985,
-0.9));
#82198=CARTESIAN_POINT('Ctrl Pts',(-28.3027980104089,-51.2860850691795,
-0.6));
#82199=CARTESIAN_POINT('Ctrl Pts',(-28.3027980104089,-51.2860850691795,
-0.9));
#82200=CARTESIAN_POINT('Ctrl Pts',(-27.9317197576165,-51.2860850691795,
-0.6));
#82201=CARTESIAN_POINT('Ctrl Pts',(-27.9317197576165,-51.2860850691795,
-0.9));
#82202=CARTESIAN_POINT('',(-28.5474774613976,-51.4855388998985,-0.6));
#82203=CARTESIAN_POINT('Ctrl Pts',(-28.5474774613976,-51.4855388998985,
-0.6));
#82204=CARTESIAN_POINT('Ctrl Pts',(-28.3027980104089,-51.2860850691795,
-0.6));
#82205=CARTESIAN_POINT('Ctrl Pts',(-27.9317197576165,-51.2860850691795,
-0.6));
#82206=CARTESIAN_POINT('',(-28.5474774613976,-51.4855388998985,-0.9));
#82207=CARTESIAN_POINT('',(-28.5474774613976,-51.4855388998985,-0.6));
#82208=CARTESIAN_POINT('Ctrl Pts',(-28.5474774613976,-51.4855388998985,
-0.9));
#82209=CARTESIAN_POINT('Ctrl Pts',(-28.3027980104089,-51.2860850691795,
-0.9));
#82210=CARTESIAN_POINT('Ctrl Pts',(-27.9317197576165,-51.2860850691795,
-0.9));
#82211=CARTESIAN_POINT('Ctrl Pts',(-28.9162359014153,-52.0525924563408,
-0.6));
#82212=CARTESIAN_POINT('Ctrl Pts',(-28.9162359014153,-52.0525924563408,
-0.9));
#82213=CARTESIAN_POINT('Ctrl Pts',(-28.7921569123864,-51.684993326664,-0.6));
#82214=CARTESIAN_POINT('Ctrl Pts',(-28.7921569123864,-51.684993326664,-0.9));
#82215=CARTESIAN_POINT('Ctrl Pts',(-28.5474774613976,-51.4855388998985,
-0.6));
#82216=CARTESIAN_POINT('Ctrl Pts',(-28.5474774613976,-51.4855388998985,
-0.9));
#82217=CARTESIAN_POINT('',(-28.9162359014153,-52.0525924563408,-0.6));
#82218=CARTESIAN_POINT('Ctrl Pts',(-28.9162359014153,-52.0525924563408,
-0.6));
#82219=CARTESIAN_POINT('Ctrl Pts',(-28.7921569123864,-51.684993326664,-0.6));
#82220=CARTESIAN_POINT('Ctrl Pts',(-28.5474774613976,-51.4855388998985,
-0.6));
#82221=CARTESIAN_POINT('',(-28.9162359014153,-52.0525924563408,-0.9));
#82222=CARTESIAN_POINT('',(-28.9162359014153,-52.0525924563408,-0.6));
#82223=CARTESIAN_POINT('Ctrl Pts',(-28.9162359014153,-52.0525924563408,
-0.9));
#82224=CARTESIAN_POINT('Ctrl Pts',(-28.7921569123864,-51.684993326664,-0.9));
#82225=CARTESIAN_POINT('Ctrl Pts',(-28.5474774613976,-51.4855388998985,
-0.9));
#82226=CARTESIAN_POINT('Ctrl Pts',(-29.0403148904443,-53.0231921076775,
-0.6));
#82227=CARTESIAN_POINT('Ctrl Pts',(-29.0403148904443,-53.0231921076775,
-0.9));
#82228=CARTESIAN_POINT('Ctrl Pts',(-29.0403148904443,-52.4201909899712,
-0.6));
#82229=CARTESIAN_POINT('Ctrl Pts',(-29.0403148904443,-52.4201909899712,
-0.9));
#82230=CARTESIAN_POINT('Ctrl Pts',(-28.9162359014153,-52.0525924563408,
-0.6));
#82231=CARTESIAN_POINT('Ctrl Pts',(-28.9162359014153,-52.0525924563408,
-0.9));
#82232=CARTESIAN_POINT('',(-29.0403148904443,-53.0231921076775,-0.6));
#82233=CARTESIAN_POINT('Ctrl Pts',(-29.0403148904443,-53.0231921076775,
-0.6));
#82234=CARTESIAN_POINT('Ctrl Pts',(-29.0403148904443,-52.4201909899712,
-0.6));
#82235=CARTESIAN_POINT('Ctrl Pts',(-28.9162359014153,-52.0525924563408,
-0.6));
#82236=CARTESIAN_POINT('',(-29.0403148904443,-53.0231921076775,-0.9));
#82237=CARTESIAN_POINT('',(-29.0403148904443,-53.0231921076775,-0.6));
#82238=CARTESIAN_POINT('Ctrl Pts',(-29.0403148904443,-53.0231921076775,
-0.9));
#82239=CARTESIAN_POINT('Ctrl Pts',(-29.0403148904443,-52.4201909899712,
-0.9));
#82240=CARTESIAN_POINT('Ctrl Pts',(-28.9162359014153,-52.0525924563408,
-0.9));
#82241=CARTESIAN_POINT('Ctrl Pts',(-28.7040254846215,-54.4054571986198,
-0.6));
#82242=CARTESIAN_POINT('Ctrl Pts',(-28.7040254846215,-54.4054571986198,
-0.9));
#82243=CARTESIAN_POINT('Ctrl Pts',(-29.0403148904443,-53.9810369610786,
-0.6));
#82244=CARTESIAN_POINT('Ctrl Pts',(-29.0403148904443,-53.9810369610786,
-0.9));
#82245=CARTESIAN_POINT('Ctrl Pts',(-29.0403148904443,-53.0231921076775,
-0.6));
#82246=CARTESIAN_POINT('Ctrl Pts',(-29.0403148904443,-53.0231921076775,
-0.9));
#82247=CARTESIAN_POINT('',(-28.7040254846215,-54.4054571986198,-0.6));
#82248=CARTESIAN_POINT('Ctrl Pts',(-28.7040254846215,-54.4054571986198,
-0.6));
#82249=CARTESIAN_POINT('Ctrl Pts',(-29.0403148904443,-53.9810369610786,
-0.6));
#82250=CARTESIAN_POINT('Ctrl Pts',(-29.0403148904443,-53.0231921076775,
-0.6));
#82251=CARTESIAN_POINT('',(-28.7040254846215,-54.4054571986198,-0.9));
#82252=CARTESIAN_POINT('',(-28.7040254846215,-54.4054571986198,-0.6));
#82253=CARTESIAN_POINT('Ctrl Pts',(-28.7040254846215,-54.4054571986198,
-0.9));
#82254=CARTESIAN_POINT('Ctrl Pts',(-29.0403148904443,-53.9810369610786,
-0.9));
#82255=CARTESIAN_POINT('Ctrl Pts',(-29.0403148904443,-53.0231921076775,
-0.9));
#82256=CARTESIAN_POINT('Ctrl Pts',(-27.9317197576165,-54.7579811215401,
-0.6));
#82257=CARTESIAN_POINT('Ctrl Pts',(-27.9317197576165,-54.7579811215401,
-0.9));
#82258=CARTESIAN_POINT('Ctrl Pts',(-28.4233978763223,-54.7579811215401,
-0.6));
#82259=CARTESIAN_POINT('Ctrl Pts',(-28.4233978763223,-54.7579811215401,
-0.9));
#82260=CARTESIAN_POINT('Ctrl Pts',(-28.7040254846215,-54.4054571986198,
-0.6));
#82261=CARTESIAN_POINT('Ctrl Pts',(-28.7040254846215,-54.4054571986198,
-0.9));
#82262=CARTESIAN_POINT('Ctrl Pts',(-27.9317197576165,-54.7579811215401,
-0.6));
#82263=CARTESIAN_POINT('Ctrl Pts',(-28.4233978763223,-54.7579811215401,
-0.6));
#82264=CARTESIAN_POINT('Ctrl Pts',(-28.7040254846215,-54.4054571986198,
-0.6));
#82265=CARTESIAN_POINT('Ctrl Pts',(-27.9317197576165,-54.7579811215401,
-0.9));
#82266=CARTESIAN_POINT('Ctrl Pts',(-28.4233978763223,-54.7579811215401,
-0.9));
#82267=CARTESIAN_POINT('Ctrl Pts',(-28.7040254846215,-54.4054571986198,
-0.9));
#82268=CARTESIAN_POINT('Origin',(-27.9317200556397,-53.0220330953598,-0.9));
#82269=CARTESIAN_POINT('Ctrl Pts',(-30.7495922222733,-51.7406551241875,
-0.6));
#82270=CARTESIAN_POINT('Ctrl Pts',(-30.7495922222733,-51.7406551241875,
-0.9));
#82271=CARTESIAN_POINT('Ctrl Pts',(-30.487518645823,-51.5064118504524,-0.6));
#82272=CARTESIAN_POINT('Ctrl Pts',(-30.487518645823,-51.5064118504524,-0.9));
#82273=CARTESIAN_POINT('Ctrl Pts',(-30.3785142675042,-51.2860844731331,
-0.6));
#82274=CARTESIAN_POINT('Ctrl Pts',(-30.3785142675042,-51.2860844731331,
-0.9));
#82275=CARTESIAN_POINT('',(-30.7495922222733,-51.7406551241875,-0.6));
#82276=CARTESIAN_POINT('',(-30.3785142675042,-51.2860844731331,-0.6));
#82277=CARTESIAN_POINT('Ctrl Pts',(-30.7495922222733,-51.7406551241875,
-0.6));
#82278=CARTESIAN_POINT('Ctrl Pts',(-30.487518645823,-51.5064118504524,-0.6));
#82279=CARTESIAN_POINT('Ctrl Pts',(-30.3785142675042,-51.2860844731331,
-0.6));
#82280=CARTESIAN_POINT('',(-30.7495922222733,-51.7406551241875,-0.9));
#82281=CARTESIAN_POINT('',(-30.7495922222733,-51.7406551241875,-0.6));
#82282=CARTESIAN_POINT('',(-30.3785142675042,-51.2860844731331,-0.9));
#82283=CARTESIAN_POINT('Ctrl Pts',(-30.7495922222733,-51.7406551241875,
-0.9));
#82284=CARTESIAN_POINT('Ctrl Pts',(-30.487518645823,-51.5064118504524,-0.9));
#82285=CARTESIAN_POINT('Ctrl Pts',(-30.3785142675042,-51.2860844731331,
-0.9));
#82286=CARTESIAN_POINT('',(-30.3785142675042,-51.2860844731331,-0.6));
#82287=CARTESIAN_POINT('Ctrl Pts',(-31.3618705049157,-52.1395633816719,
-0.6));
#82288=CARTESIAN_POINT('Ctrl Pts',(-31.3618705049157,-52.1395633816719,
-0.9));
#82289=CARTESIAN_POINT('Ctrl Pts',(-31.0116657987237,-51.9748978018761,
-0.6));
#82290=CARTESIAN_POINT('Ctrl Pts',(-31.0116657987237,-51.9748978018761,
-0.9));
#82291=CARTESIAN_POINT('Ctrl Pts',(-30.7495922222733,-51.7406551241875,
-0.6));
#82292=CARTESIAN_POINT('Ctrl Pts',(-30.7495922222733,-51.7406551241875,
-0.9));
#82293=CARTESIAN_POINT('',(-31.3618705049157,-52.1395633816719,-0.6));
#82294=CARTESIAN_POINT('Ctrl Pts',(-31.3618705049157,-52.1395633816719,
-0.6));
#82295=CARTESIAN_POINT('Ctrl Pts',(-31.0116657987237,-51.9748978018761,
-0.6));
#82296=CARTESIAN_POINT('Ctrl Pts',(-30.7495922222733,-51.7406551241875,
-0.6));
#82297=CARTESIAN_POINT('',(-31.3618705049157,-52.1395633816719,-0.9));
#82298=CARTESIAN_POINT('',(-31.3618705049157,-52.1395633816719,-0.6));
#82299=CARTESIAN_POINT('Ctrl Pts',(-31.3618705049157,-52.1395633816719,
-0.9));
#82300=CARTESIAN_POINT('Ctrl Pts',(-31.0116657987237,-51.9748978018761,
-0.9));
#82301=CARTESIAN_POINT('Ctrl Pts',(-30.7495922222733,-51.7406551241875,
-0.9));
#82302=CARTESIAN_POINT('Origin',(-31.3618705049157,-52.5431100726128,-0.6));
#82303=CARTESIAN_POINT('',(-31.3618705049157,-52.5431100726128,-0.6));
#82304=CARTESIAN_POINT('',(-31.3618705049157,-52.7715550363064,-0.6));
#82305=CARTESIAN_POINT('',(-31.3618705049157,-52.5431100726128,-0.9));
#82306=CARTESIAN_POINT('',(-31.3618705049157,-52.5431100726128,-0.6));
#82307=CARTESIAN_POINT('',(-31.3618705049157,-52.5431100726128,-0.9));
#82308=CARTESIAN_POINT('Ctrl Pts',(-30.9223753586411,-52.3274211287498,
-0.6));
#82309=CARTESIAN_POINT('Ctrl Pts',(-30.9223753586411,-52.3274211287498,
-0.9));
#82310=CARTESIAN_POINT('Ctrl Pts',(-31.1670548096299,-52.4712137579918,
-0.6));
#82311=CARTESIAN_POINT('Ctrl Pts',(-31.1670548096299,-52.4712137579918,
-0.9));
#82312=CARTESIAN_POINT('Ctrl Pts',(-31.3618705049157,-52.5431100726128,
-0.6));
#82313=CARTESIAN_POINT('Ctrl Pts',(-31.3618705049157,-52.5431100726128,
-0.9));
#82314=CARTESIAN_POINT('',(-30.9223753586411,-52.3274211287498,-0.6));
#82315=CARTESIAN_POINT('Ctrl Pts',(-30.9223753586411,-52.3274211287498,
-0.6));
#82316=CARTESIAN_POINT('Ctrl Pts',(-31.1670548096299,-52.4712137579918,
-0.6));
#82317=CARTESIAN_POINT('Ctrl Pts',(-31.3618705049157,-52.5431100726128,
-0.6));
#82318=CARTESIAN_POINT('',(-30.9223753586411,-52.3274211287498,-0.9));
#82319=CARTESIAN_POINT('',(-30.9223753586411,-52.3274211287498,-0.6));
#82320=CARTESIAN_POINT('Ctrl Pts',(-30.9223753586411,-52.3274211287498,
-0.9));
#82321=CARTESIAN_POINT('Ctrl Pts',(-31.1670548096299,-52.4712137579918,
-0.9));
#82322=CARTESIAN_POINT('Ctrl Pts',(-31.3618705049157,-52.5431100726128,
-0.9));
#82323=CARTESIAN_POINT('Ctrl Pts',(-30.5269453302026,-52.039835870266,-0.6));
#82324=CARTESIAN_POINT('Ctrl Pts',(-30.5269453302026,-52.039835870266,-0.9));
#82325=CARTESIAN_POINT('Ctrl Pts',(-30.6776959076524,-52.1836284995079,
-0.6));
#82326=CARTESIAN_POINT('Ctrl Pts',(-30.6776959076524,-52.1836284995079,
-0.9));
#82327=CARTESIAN_POINT('Ctrl Pts',(-30.9223753586411,-52.3274211287498,
-0.6));
#82328=CARTESIAN_POINT('Ctrl Pts',(-30.9223753586411,-52.3274211287498,
-0.9));
#82329=CARTESIAN_POINT('',(-30.5269453302026,-52.039835870266,-0.6));
#82330=CARTESIAN_POINT('Ctrl Pts',(-30.5269453302026,-52.039835870266,-0.6));
#82331=CARTESIAN_POINT('Ctrl Pts',(-30.6776959076524,-52.1836284995079,
-0.6));
#82332=CARTESIAN_POINT('Ctrl Pts',(-30.9223753586411,-52.3274211287498,
-0.6));
#82333=CARTESIAN_POINT('',(-30.5269453302026,-52.039835870266,-0.9));
#82334=CARTESIAN_POINT('',(-30.5269453302026,-52.039835870266,-0.6));
#82335=CARTESIAN_POINT('Ctrl Pts',(-30.5269453302026,-52.039835870266,-0.9));
#82336=CARTESIAN_POINT('Ctrl Pts',(-30.6776959076524,-52.1836284995079,
-0.9));
#82337=CARTESIAN_POINT('Ctrl Pts',(-30.9223753586411,-52.3274211287498,
-0.9));
#82338=CARTESIAN_POINT('Origin',(-30.5269453302026,-54.7000001072884,-0.6));
#82339=CARTESIAN_POINT('',(-30.5269453302026,-54.7000001072884,-0.6));
#82340=CARTESIAN_POINT('',(-30.5269453302026,-53.8500000536442,-0.6));
#82341=CARTESIAN_POINT('',(-30.5269453302026,-54.7000001072884,-0.9));
#82342=CARTESIAN_POINT('',(-30.5269453302026,-54.7000001072884,-0.6));
#82343=CARTESIAN_POINT('',(-30.5269453302026,-54.7000001072884,-0.9));
#82344=CARTESIAN_POINT('Origin',(-30.109482742846,-54.7000001072884,-0.6));
#82345=CARTESIAN_POINT('',(-30.109482742846,-54.7000001072884,-0.6));
#82346=CARTESIAN_POINT('',(-15.054741371423,-54.7000001072884,-0.6));
#82347=CARTESIAN_POINT('',(-30.109482742846,-54.7000001072884,-0.9));
#82348=CARTESIAN_POINT('',(-30.109482742846,-54.7000001072884,-0.6));
#82349=CARTESIAN_POINT('',(-30.109482742846,-54.7000001072884,-0.9));
#82350=CARTESIAN_POINT('Origin',(-30.109482742846,-51.2860844731331,-0.6));
#82351=CARTESIAN_POINT('',(-30.109482742846,-51.2860844731331,-0.6));
#82352=CARTESIAN_POINT('',(-30.109482742846,-52.1430422365665,-0.6));
#82353=CARTESIAN_POINT('',(-30.109482742846,-51.2860844731331,-0.9));
#82354=CARTESIAN_POINT('',(-30.109482742846,-51.2860844731331,-0.6));
#82355=CARTESIAN_POINT('',(-30.109482742846,-51.2860844731331,-0.9));
#82356=CARTESIAN_POINT('Origin',(-30.3785142675042,-51.2860844731331,-0.6));
#82357=CARTESIAN_POINT('',(-15.1892571337521,-51.2860844731331,-0.6));
#82358=CARTESIAN_POINT('',(-30.3785142675042,-51.2860844731331,-0.9));
#82359=CARTESIAN_POINT('Origin',(-30.7356766238809,-52.9930422902107,-0.9));
#82360=CARTESIAN_POINT('Origin',(-26.4450899139047,-53.2597545981407,-0.6));
#82361=CARTESIAN_POINT('',(-26.4450899139047,-53.2597545981407,-0.6));
#82362=CARTESIAN_POINT('',(-25.1625523343682,-53.2597545981407,-0.6));
#82363=CARTESIAN_POINT('',(-13.2225449569523,-53.2597545981407,-0.6));
#82364=CARTESIAN_POINT('',(-26.4450899139047,-53.2597545981407,-0.9));
#82365=CARTESIAN_POINT('',(-26.4450899139047,-53.2597545981407,-0.6));
#82366=CARTESIAN_POINT('',(-25.1625523343682,-53.2597545981407,-0.9));
#82367=CARTESIAN_POINT('',(-26.4450899139047,-53.2597545981407,-0.9));
#82368=CARTESIAN_POINT('',(-25.1625523343682,-53.2597545981407,-0.6));
#82369=CARTESIAN_POINT('Origin',(-26.4450899139047,-53.6795364022255,-0.6));
#82370=CARTESIAN_POINT('',(-26.4450899139047,-53.6795364022255,-0.6));
#82371=CARTESIAN_POINT('',(-26.4450899139047,-53.3397682011127,-0.6));
#82372=CARTESIAN_POINT('',(-26.4450899139047,-53.6795364022255,-0.9));
#82373=CARTESIAN_POINT('',(-26.4450899139047,-53.6795364022255,-0.6));
#82374=CARTESIAN_POINT('',(-26.4450899139047,-53.6795364022255,-0.9));
#82375=CARTESIAN_POINT('Origin',(-25.1625523343682,-53.6795364022255,-0.6));
#82376=CARTESIAN_POINT('',(-25.1625523343682,-53.6795364022255,-0.6));
#82377=CARTESIAN_POINT('',(-12.5812761671841,-53.6795364022255,-0.6));
#82378=CARTESIAN_POINT('',(-25.1625523343682,-53.6795364022255,-0.9));
#82379=CARTESIAN_POINT('',(-25.1625523343682,-53.6795364022255,-0.6));
#82380=CARTESIAN_POINT('',(-25.1625523343682,-53.6795364022255,-0.9));
#82381=CARTESIAN_POINT('Origin',(-25.1625523343682,-53.2597545981407,-0.6));
#82382=CARTESIAN_POINT('',(-25.1625523343682,-53.1298772990704,-0.6));
#82383=CARTESIAN_POINT('',(-25.1625523343682,-53.2597545981407,-0.9));
#82384=CARTESIAN_POINT('Origin',(-25.8038211241364,-53.4696455001831,-0.9));
#82385=CARTESIAN_POINT('Ctrl Pts',(-20.1901099458337,-54.3451569676399,
-0.6));
#82386=CARTESIAN_POINT('Ctrl Pts',(-20.1901099458337,-54.3451569676399,
-0.9));
#82387=CARTESIAN_POINT('Ctrl Pts',(-20.5171224847436,-54.7579811215401,
-0.6));
#82388=CARTESIAN_POINT('Ctrl Pts',(-20.5171224847436,-54.7579811215401,
-0.9));
#82389=CARTESIAN_POINT('Ctrl Pts',(-21.0830161347985,-54.7579811215401,
-0.6));
#82390=CARTESIAN_POINT('Ctrl Pts',(-21.0830161347985,-54.7579811215401,
-0.9));
#82391=CARTESIAN_POINT('',(-20.1901099458337,-54.3451569676399,-0.6));
#82392=CARTESIAN_POINT('',(-21.0830161347985,-54.7579811215401,-0.6));
#82393=CARTESIAN_POINT('Ctrl Pts',(-20.1901099458337,-54.3451569676399,
-0.6));
#82394=CARTESIAN_POINT('Ctrl Pts',(-20.5171224847436,-54.7579811215401,
-0.6));
#82395=CARTESIAN_POINT('Ctrl Pts',(-21.0830161347985,-54.7579811215401,
-0.6));
#82396=CARTESIAN_POINT('',(-20.1901099458337,-54.3451569676399,-0.9));
#82397=CARTESIAN_POINT('',(-20.1901099458337,-54.3451569676399,-0.6));
#82398=CARTESIAN_POINT('',(-21.0830161347985,-54.7579811215401,-0.9));
#82399=CARTESIAN_POINT('Ctrl Pts',(-20.1901099458337,-54.3451569676399,
-0.9));
#82400=CARTESIAN_POINT('Ctrl Pts',(-20.5171224847436,-54.7579811215401,
-0.9));
#82401=CARTESIAN_POINT('Ctrl Pts',(-21.0830161347985,-54.7579811215401,
-0.9));
#82402=CARTESIAN_POINT('',(-21.0830161347985,-54.7579811215401,-0.6));
#82403=CARTESIAN_POINT('Ctrl Pts',(-19.9210784211755,-53.5473398566246,
-0.6));
#82404=CARTESIAN_POINT('Ctrl Pts',(-19.9210784211755,-53.5473398566246,
-0.9));
#82405=CARTESIAN_POINT('Ctrl Pts',(-19.9210784211755,-54.0088675618172,
-0.6));
#82406=CARTESIAN_POINT('Ctrl Pts',(-19.9210784211755,-54.0088675618172,
-0.9));
#82407=CARTESIAN_POINT('Ctrl Pts',(-20.1901099458337,-54.3451569676399,
-0.6));
#82408=CARTESIAN_POINT('Ctrl Pts',(-20.1901099458337,-54.3451569676399,
-0.9));
#82409=CARTESIAN_POINT('',(-19.9210784211755,-53.5473398566246,-0.6));
#82410=CARTESIAN_POINT('Ctrl Pts',(-19.9210784211755,-53.5473398566246,
-0.6));
#82411=CARTESIAN_POINT('Ctrl Pts',(-19.9210784211755,-54.0088675618172,
-0.6));
#82412=CARTESIAN_POINT('Ctrl Pts',(-20.1901099458337,-54.3451569676399,
-0.6));
#82413=CARTESIAN_POINT('',(-19.9210784211755,-53.5473398566246,-0.9));
#82414=CARTESIAN_POINT('',(-19.9210784211755,-53.5473398566246,-0.6));
#82415=CARTESIAN_POINT('Ctrl Pts',(-19.9210784211755,-53.5473398566246,
-0.9));
#82416=CARTESIAN_POINT('Ctrl Pts',(-19.9210784211755,-54.0088675618172,
-0.9));
#82417=CARTESIAN_POINT('Ctrl Pts',(-20.1901099458337,-54.3451569676399,
-0.9));
#82418=CARTESIAN_POINT('Ctrl Pts',(-20.2272174134851,-52.7541605830193,
-0.6));
#82419=CARTESIAN_POINT('Ctrl Pts',(-20.2272174134851,-52.7541605830193,
-0.9));
#82420=CARTESIAN_POINT('Ctrl Pts',(-19.9210784211755,-53.0626193881035,
-0.6));
#82421=CARTESIAN_POINT('Ctrl Pts',(-19.9210784211755,-53.0626193881035,
-0.9));
#82422=CARTESIAN_POINT('Ctrl Pts',(-19.9210784211755,-53.5473398566246,
-0.6));
#82423=CARTESIAN_POINT('Ctrl Pts',(-19.9210784211755,-53.5473398566246,
-0.9));
#82424=CARTESIAN_POINT('',(-20.2272174134851,-52.7541605830193,-0.6));
#82425=CARTESIAN_POINT('Ctrl Pts',(-20.2272174134851,-52.7541605830193,
-0.6));
#82426=CARTESIAN_POINT('Ctrl Pts',(-19.9210784211755,-53.0626193881035,
-0.6));
#82427=CARTESIAN_POINT('Ctrl Pts',(-19.9210784211755,-53.5473398566246,
-0.6));
#82428=CARTESIAN_POINT('',(-20.2272174134851,-52.7541605830193,-0.9));
#82429=CARTESIAN_POINT('',(-20.2272174134851,-52.7541605830193,-0.6));
#82430=CARTESIAN_POINT('Ctrl Pts',(-20.2272174134851,-52.7541605830193,
-0.9));
#82431=CARTESIAN_POINT('Ctrl Pts',(-19.9210784211755,-53.0626193881035,
-0.9));
#82432=CARTESIAN_POINT('Ctrl Pts',(-19.9210784211755,-53.5473398566246,
-0.9));
#82433=CARTESIAN_POINT('Ctrl Pts',(-20.9786507859826,-52.4457023739815,
-0.6));
#82434=CARTESIAN_POINT('Ctrl Pts',(-20.9786507859826,-52.4457023739815,
-0.9));
#82435=CARTESIAN_POINT('Ctrl Pts',(-20.5333575978875,-52.4457023739815,
-0.6));
#82436=CARTESIAN_POINT('Ctrl Pts',(-20.5333575978875,-52.4457023739815,
-0.9));
#82437=CARTESIAN_POINT('Ctrl Pts',(-20.2272174134851,-52.7541605830193,
-0.6));
#82438=CARTESIAN_POINT('Ctrl Pts',(-20.2272174134851,-52.7541605830193,
-0.9));
#82439=CARTESIAN_POINT('',(-20.9786507859826,-52.4457023739815,-0.6));
#82440=CARTESIAN_POINT('Ctrl Pts',(-20.9786507859826,-52.4457023739815,
-0.6));
#82441=CARTESIAN_POINT('Ctrl Pts',(-20.5333575978875,-52.4457023739815,
-0.6));
#82442=CARTESIAN_POINT('Ctrl Pts',(-20.2272174134851,-52.7541605830193,
-0.6));
#82443=CARTESIAN_POINT('',(-20.9786507859826,-52.4457023739815,-0.9));
#82444=CARTESIAN_POINT('',(-20.9786507859826,-52.4457023739815,-0.6));
#82445=CARTESIAN_POINT('Ctrl Pts',(-20.9786507859826,-52.4457023739815,
-0.9));
#82446=CARTESIAN_POINT('Ctrl Pts',(-20.5333575978875,-52.4457023739815,
-0.9));
#82447=CARTESIAN_POINT('Ctrl Pts',(-20.2272174134851,-52.7541605830193,
-0.9));
#82448=CARTESIAN_POINT('Ctrl Pts',(-21.6210791841149,-52.6590721011162,
-0.6));
#82449=CARTESIAN_POINT('Ctrl Pts',(-21.6210791841149,-52.6590721011162,
-0.9));
#82450=CARTESIAN_POINT('Ctrl Pts',(-21.3149389997125,-52.4457023739815,
-0.6));
#82451=CARTESIAN_POINT('Ctrl Pts',(-21.3149389997125,-52.4457023739815,
-0.9));
#82452=CARTESIAN_POINT('Ctrl Pts',(-20.9786507859826,-52.4457023739815,
-0.6));
#82453=CARTESIAN_POINT('Ctrl Pts',(-20.9786507859826,-52.4457023739815,
-0.9));
#82454=CARTESIAN_POINT('',(-21.6210791841149,-52.6590721011162,-0.6));
#82455=CARTESIAN_POINT('Ctrl Pts',(-21.6210791841149,-52.6590721011162,
-0.6));
#82456=CARTESIAN_POINT('Ctrl Pts',(-21.3149389997125,-52.4457023739815,
-0.6));
#82457=CARTESIAN_POINT('Ctrl Pts',(-20.9786507859826,-52.4457023739815,
-0.6));
#82458=CARTESIAN_POINT('',(-21.6210791841149,-52.6590721011162,-0.9));
#82459=CARTESIAN_POINT('',(-21.6210791841149,-52.6590721011162,-0.6));
#82460=CARTESIAN_POINT('Ctrl Pts',(-21.6210791841149,-52.6590721011162,
-0.9));
#82461=CARTESIAN_POINT('Ctrl Pts',(-21.3149389997125,-52.4457023739815,
-0.9));
#82462=CARTESIAN_POINT('Ctrl Pts',(-20.9786507859826,-52.4457023739815,
-0.9));
#82463=CARTESIAN_POINT('Origin',(-21.437859274447,-51.7452935576439,-0.6));
#82464=CARTESIAN_POINT('',(-21.437859274447,-51.7452935576439,-0.6));
#82465=CARTESIAN_POINT('',(-21.1445044486643,-50.2822356077188,-0.6));
#82466=CARTESIAN_POINT('',(-21.437859274447,-51.7452935576439,-0.9));
#82467=CARTESIAN_POINT('',(-21.437859274447,-51.7452935576439,-0.6));
#82468=CARTESIAN_POINT('',(-21.437859274447,-51.7452935576439,-0.9));
#82469=CARTESIAN_POINT('Origin',(-20.0811061635613,-51.7452935576439,-0.6));
#82470=CARTESIAN_POINT('',(-20.0811061635613,-51.7452935576439,-0.6));
#82471=CARTESIAN_POINT('',(-10.0405530817807,-51.7452935576439,-0.6));
#82472=CARTESIAN_POINT('',(-20.0811061635613,-51.7452935576439,-0.9));
#82473=CARTESIAN_POINT('',(-20.0811061635613,-51.7452935576439,-0.6));
#82474=CARTESIAN_POINT('',(-20.0811061635613,-51.7452935576439,-0.9));
#82475=CARTESIAN_POINT('Origin',(-20.0811061635613,-51.346384704113,-0.6));
#82476=CARTESIAN_POINT('',(-20.0811061635613,-51.346384704113,-0.6));
#82477=CARTESIAN_POINT('',(-20.0811061635613,-52.1731923520565,-0.6));
#82478=CARTESIAN_POINT('',(-20.0811061635613,-51.346384704113,-0.9));
#82479=CARTESIAN_POINT('',(-20.0811061635613,-51.346384704113,-0.6));
#82480=CARTESIAN_POINT('',(-20.0811061635613,-51.346384704113,-0.9));
#82481=CARTESIAN_POINT('Origin',(-21.7718288674951,-51.346384704113,-0.6));
#82482=CARTESIAN_POINT('',(-21.7718288674951,-51.346384704113,-0.6));
#82483=CARTESIAN_POINT('',(-10.8859144337475,-51.346384704113,-0.6));
#82484=CARTESIAN_POINT('',(-21.7718288674951,-51.346384704113,-0.9));
#82485=CARTESIAN_POINT('',(-21.7718288674951,-51.346384704113,-0.6));
#82486=CARTESIAN_POINT('',(-21.7718288674951,-51.346384704113,-0.9));
#82487=CARTESIAN_POINT('Origin',(-22.1011600270867,-53.0927692055702,-0.6));
#82488=CARTESIAN_POINT('',(-22.1011600270867,-53.0927692055702,-0.6));
#82489=CARTESIAN_POINT('',(-21.7132280182382,-51.0356348344644,-0.6));
#82490=CARTESIAN_POINT('',(-22.1011600270867,-53.0927692055702,-0.9));
#82491=CARTESIAN_POINT('',(-22.1011600270867,-53.0927692055702,-0.6));
#82492=CARTESIAN_POINT('',(-22.1011600270867,-53.0927692055702,-0.9));
#82493=CARTESIAN_POINT('Origin',(-21.7092094197869,-53.1437925696373,-0.6));
#82494=CARTESIAN_POINT('',(-21.7092094197869,-53.1437925696373,-0.6));
#82495=CARTESIAN_POINT('',(-11.0446884509171,-54.5320790676332,-0.6));
#82496=CARTESIAN_POINT('',(-21.7092094197869,-53.1437925696373,-0.9));
#82497=CARTESIAN_POINT('',(-21.7092094197869,-53.1437925696373,-0.6));
#82498=CARTESIAN_POINT('',(-21.7092094197869,-53.1437925696373,-0.9));
#82499=CARTESIAN_POINT('Ctrl Pts',(-21.454093195498,-52.9060707688332,-0.6));
#82500=CARTESIAN_POINT('Ctrl Pts',(-21.454093195498,-52.9060707688332,-0.9));
#82501=CARTESIAN_POINT('Ctrl Pts',(-21.6164407506585,-52.9976807236671,
-0.6));
#82502=CARTESIAN_POINT('Ctrl Pts',(-21.6164407506585,-52.9976807236671,
-0.9));
#82503=CARTESIAN_POINT('Ctrl Pts',(-21.7092094197869,-53.1437925696373,
-0.6));
#82504=CARTESIAN_POINT('Ctrl Pts',(-21.7092094197869,-53.1437925696373,
-0.9));
#82505=CARTESIAN_POINT('',(-21.454093195498,-52.9060707688332,-0.6));
#82506=CARTESIAN_POINT('Ctrl Pts',(-21.454093195498,-52.9060707688332,-0.6));
#82507=CARTESIAN_POINT('Ctrl Pts',(-21.6164407506585,-52.9976807236671,
-0.6));
#82508=CARTESIAN_POINT('Ctrl Pts',(-21.7092094197869,-53.1437925696373,
-0.6));
#82509=CARTESIAN_POINT('',(-21.454093195498,-52.9060707688332,-0.9));
#82510=CARTESIAN_POINT('',(-21.454093195498,-52.9060707688332,-0.6));
#82511=CARTESIAN_POINT('Ctrl Pts',(-21.454093195498,-52.9060707688332,-0.9));
#82512=CARTESIAN_POINT('Ctrl Pts',(-21.6164407506585,-52.9976807236671,
-0.9));
#82513=CARTESIAN_POINT('Ctrl Pts',(-21.7092094197869,-53.1437925696373,
-0.9));
#82514=CARTESIAN_POINT('Ctrl Pts',(-21.0899731889367,-52.8144608139992,
-0.6));
#82515=CARTESIAN_POINT('Ctrl Pts',(-21.0899731889367,-52.8144608139992,
-0.9));
#82516=CARTESIAN_POINT('Ctrl Pts',(-21.2917468324304,-52.8144608139992,
-0.6));
#82517=CARTESIAN_POINT('Ctrl Pts',(-21.2917468324304,-52.8144608139992,
-0.9));
#82518=CARTESIAN_POINT('Ctrl Pts',(-21.454093195498,-52.9060707688332,-0.6));
#82519=CARTESIAN_POINT('Ctrl Pts',(-21.454093195498,-52.9060707688332,-0.9));
#82520=CARTESIAN_POINT('',(-21.0899731889367,-52.8144608139992,-0.6));
#82521=CARTESIAN_POINT('Ctrl Pts',(-21.0899731889367,-52.8144608139992,
-0.6));
#82522=CARTESIAN_POINT('Ctrl Pts',(-21.2917468324304,-52.8144608139992,
-0.6));
#82523=CARTESIAN_POINT('Ctrl Pts',(-21.454093195498,-52.9060707688332,-0.6));
#82524=CARTESIAN_POINT('',(-21.0899731889367,-52.8144608139992,-0.9));
#82525=CARTESIAN_POINT('',(-21.0899731889367,-52.8144608139992,-0.6));
#82526=CARTESIAN_POINT('Ctrl Pts',(-21.0899731889367,-52.8144608139992,
-0.9));
#82527=CARTESIAN_POINT('Ctrl Pts',(-21.2917468324304,-52.8144608139992,
-0.9));
#82528=CARTESIAN_POINT('Ctrl Pts',(-21.454093195498,-52.9060707688332,-0.9));
#82529=CARTESIAN_POINT('Ctrl Pts',(-20.5646667256951,-53.0208728909492,
-0.6));
#82530=CARTESIAN_POINT('Ctrl Pts',(-20.5646667256951,-53.0208728909492,
-0.9));
#82531=CARTESIAN_POINT('Ctrl Pts',(-20.7652804628015,-52.8144608139992,
-0.6));
#82532=CARTESIAN_POINT('Ctrl Pts',(-20.7652804628015,-52.8144608139992,
-0.9));
#82533=CARTESIAN_POINT('Ctrl Pts',(-21.0899731889367,-52.8144608139992,
-0.6));
#82534=CARTESIAN_POINT('Ctrl Pts',(-21.0899731889367,-52.8144608139992,
-0.9));
#82535=CARTESIAN_POINT('',(-20.5646667256951,-53.0208728909492,-0.6));
#82536=CARTESIAN_POINT('Ctrl Pts',(-20.5646667256951,-53.0208728909492,
-0.6));
#82537=CARTESIAN_POINT('Ctrl Pts',(-20.7652804628015,-52.8144608139992,
-0.6));
#82538=CARTESIAN_POINT('Ctrl Pts',(-21.0899731889367,-52.8144608139992,
-0.6));
#82539=CARTESIAN_POINT('',(-20.5646667256951,-53.0208728909492,-0.9));
#82540=CARTESIAN_POINT('',(-20.5646667256951,-53.0208728909492,-0.6));
#82541=CARTESIAN_POINT('Ctrl Pts',(-20.5646667256951,-53.0208728909492,
-0.9));
#82542=CARTESIAN_POINT('Ctrl Pts',(-20.7652804628015,-52.8144608139992,
-0.9));
#82543=CARTESIAN_POINT('Ctrl Pts',(-21.0899731889367,-52.8144608139992,
-0.9));
#82544=CARTESIAN_POINT('Ctrl Pts',(-20.3640529885888,-53.584447324276,-0.6));
#82545=CARTESIAN_POINT('Ctrl Pts',(-20.3640529885888,-53.584447324276,-0.9));
#82546=CARTESIAN_POINT('Ctrl Pts',(-20.3640529885888,-53.2272849678993,
-0.6));
#82547=CARTESIAN_POINT('Ctrl Pts',(-20.3640529885888,-53.2272849678993,
-0.9));
#82548=CARTESIAN_POINT('Ctrl Pts',(-20.5646667256951,-53.0208728909492,
-0.6));
#82549=CARTESIAN_POINT('Ctrl Pts',(-20.5646667256951,-53.0208728909492,
-0.9));
#82550=CARTESIAN_POINT('',(-20.3640529885888,-53.584447324276,-0.6));
#82551=CARTESIAN_POINT('Ctrl Pts',(-20.3640529885888,-53.584447324276,-0.6));
#82552=CARTESIAN_POINT('Ctrl Pts',(-20.3640529885888,-53.2272849678993,
-0.6));
#82553=CARTESIAN_POINT('Ctrl Pts',(-20.5646667256951,-53.0208728909492,
-0.6));
#82554=CARTESIAN_POINT('',(-20.3640529885888,-53.584447324276,-0.9));
#82555=CARTESIAN_POINT('',(-20.3640529885888,-53.584447324276,-0.6));
#82556=CARTESIAN_POINT('Ctrl Pts',(-20.3640529885888,-53.584447324276,-0.9));
#82557=CARTESIAN_POINT('Ctrl Pts',(-20.3640529885888,-53.2272849678993,
-0.9));
#82558=CARTESIAN_POINT('Ctrl Pts',(-20.5646667256951,-53.0208728909492,
-0.9));
#82559=CARTESIAN_POINT('Ctrl Pts',(-20.5727836862206,-54.1874490380287,
-0.6));
#82560=CARTESIAN_POINT('Ctrl Pts',(-20.5727836862206,-54.1874490380287,
-0.9));
#82561=CARTESIAN_POINT('Ctrl Pts',(-20.3640529885888,-53.9601640105247,
-0.6));
#82562=CARTESIAN_POINT('Ctrl Pts',(-20.3640529885888,-53.9601640105247,
-0.9));
#82563=CARTESIAN_POINT('Ctrl Pts',(-20.3640529885888,-53.584447324276,-0.6));
#82564=CARTESIAN_POINT('Ctrl Pts',(-20.3640529885888,-53.584447324276,-0.9));
#82565=CARTESIAN_POINT('',(-20.5727836862206,-54.1874490380287,-0.6));
#82566=CARTESIAN_POINT('Ctrl Pts',(-20.5727836862206,-54.1874490380287,
-0.6));
#82567=CARTESIAN_POINT('Ctrl Pts',(-20.3640529885888,-53.9601640105247,
-0.6));
#82568=CARTESIAN_POINT('Ctrl Pts',(-20.3640529885888,-53.584447324276,-0.6));
#82569=CARTESIAN_POINT('',(-20.5727836862206,-54.1874490380287,-0.9));
#82570=CARTESIAN_POINT('',(-20.5727836862206,-54.1874490380287,-0.6));
#82571=CARTESIAN_POINT('Ctrl Pts',(-20.5727836862206,-54.1874490380287,
-0.9));
#82572=CARTESIAN_POINT('Ctrl Pts',(-20.3640529885888,-53.9601640105247,
-0.9));
#82573=CARTESIAN_POINT('Ctrl Pts',(-20.3640529885888,-53.584447324276,-0.9));
#82574=CARTESIAN_POINT('Ctrl Pts',(-21.0830161347985,-54.4147340655327,
-0.6));
#82575=CARTESIAN_POINT('Ctrl Pts',(-21.0830161347985,-54.4147340655327,
-0.9));
#82576=CARTESIAN_POINT('Ctrl Pts',(-20.7815155759454,-54.4147340655327,
-0.6));
#82577=CARTESIAN_POINT('Ctrl Pts',(-20.7815155759454,-54.4147340655327,
-0.9));
#82578=CARTESIAN_POINT('Ctrl Pts',(-20.5727836862206,-54.1874490380287,
-0.6));
#82579=CARTESIAN_POINT('Ctrl Pts',(-20.5727836862206,-54.1874490380287,
-0.9));
#82580=CARTESIAN_POINT('',(-21.0830161347985,-54.4147340655327,-0.6));
#82581=CARTESIAN_POINT('Ctrl Pts',(-21.0830161347985,-54.4147340655327,
-0.6));
#82582=CARTESIAN_POINT('Ctrl Pts',(-20.7815155759454,-54.4147340655327,
-0.6));
#82583=CARTESIAN_POINT('Ctrl Pts',(-20.5727836862206,-54.1874490380287,
-0.6));
#82584=CARTESIAN_POINT('',(-21.0830161347985,-54.4147340655327,-0.9));
#82585=CARTESIAN_POINT('',(-21.0830161347985,-54.4147340655327,-0.6));
#82586=CARTESIAN_POINT('Ctrl Pts',(-21.0830161347985,-54.4147340655327,
-0.9));
#82587=CARTESIAN_POINT('Ctrl Pts',(-20.7815155759454,-54.4147340655327,
-0.9));
#82588=CARTESIAN_POINT('Ctrl Pts',(-20.5727836862206,-54.1874490380287,
-0.9));
#82589=CARTESIAN_POINT('Ctrl Pts',(-21.5109154954553,-54.2535470128059,
-0.6));
#82590=CARTESIAN_POINT('Ctrl Pts',(-21.5109154954553,-54.2535470128059,
-0.9));
#82591=CARTESIAN_POINT('Ctrl Pts',(-21.333493925631,-54.4147340655327,-0.6));
#82592=CARTESIAN_POINT('Ctrl Pts',(-21.333493925631,-54.4147340655327,-0.9));
#82593=CARTESIAN_POINT('Ctrl Pts',(-21.0830161347985,-54.4147340655327,
-0.6));
#82594=CARTESIAN_POINT('Ctrl Pts',(-21.0830161347985,-54.4147340655327,
-0.9));
#82595=CARTESIAN_POINT('',(-21.5109154954553,-54.2535470128059,-0.6));
#82596=CARTESIAN_POINT('Ctrl Pts',(-21.5109154954553,-54.2535470128059,
-0.6));
#82597=CARTESIAN_POINT('Ctrl Pts',(-21.333493925631,-54.4147340655327,-0.6));
#82598=CARTESIAN_POINT('Ctrl Pts',(-21.0830161347985,-54.4147340655327,
-0.6));
#82599=CARTESIAN_POINT('',(-21.5109154954553,-54.2535470128059,-0.9));
#82600=CARTESIAN_POINT('',(-21.5109154954553,-54.2535470128059,-0.6));
#82601=CARTESIAN_POINT('Ctrl Pts',(-21.5109154954553,-54.2535470128059,
-0.9));
#82602=CARTESIAN_POINT('Ctrl Pts',(-21.333493925631,-54.4147340655327,-0.9));
#82603=CARTESIAN_POINT('Ctrl Pts',(-21.0830161347985,-54.4147340655327,
-0.9));
#82604=CARTESIAN_POINT('Ctrl Pts',(-21.7370400205255,-53.7723056674004,
-0.6));
#82605=CARTESIAN_POINT('Ctrl Pts',(-21.7370400205255,-53.7723056674004,
-0.9));
#82606=CARTESIAN_POINT('Ctrl Pts',(-21.6883370652795,-54.0923599600792,
-0.6));
#82607=CARTESIAN_POINT('Ctrl Pts',(-21.6883370652795,-54.0923599600792,
-0.9));
#82608=CARTESIAN_POINT('Ctrl Pts',(-21.5109154954553,-54.2535470128059,
-0.6));
#82609=CARTESIAN_POINT('Ctrl Pts',(-21.5109154954553,-54.2535470128059,
-0.9));
#82610=CARTESIAN_POINT('',(-21.7370400205255,-53.7723056674004,-0.6));
#82611=CARTESIAN_POINT('Ctrl Pts',(-21.7370400205255,-53.7723056674004,
-0.6));
#82612=CARTESIAN_POINT('Ctrl Pts',(-21.6883370652795,-54.0923599600792,
-0.6));
#82613=CARTESIAN_POINT('Ctrl Pts',(-21.5109154954553,-54.2535470128059,
-0.6));
#82614=CARTESIAN_POINT('',(-21.7370400205255,-53.7723056674004,-0.9));
#82615=CARTESIAN_POINT('',(-21.7370400205255,-53.7723056674004,-0.6));
#82616=CARTESIAN_POINT('Ctrl Pts',(-21.7370400205255,-53.7723056674004,
-0.9));
#82617=CARTESIAN_POINT('Ctrl Pts',(-21.6883370652795,-54.0923599600792,
-0.9));
#82618=CARTESIAN_POINT('Ctrl Pts',(-21.5109154954553,-54.2535470128059,
-0.9));
#82619=CARTESIAN_POINT('Origin',(-22.1753761544824,-53.8094131350517,-0.6));
#82620=CARTESIAN_POINT('',(-22.1753761544824,-53.8094131350517,-0.6));
#82621=CARTESIAN_POINT('',(-11.1325660081367,-52.8745809627946,-0.6));
#82622=CARTESIAN_POINT('',(-22.1753761544824,-53.8094131350517,-0.9));
#82623=CARTESIAN_POINT('',(-22.1753761544824,-53.8094131350517,-0.6));
#82624=CARTESIAN_POINT('',(-22.1753761544824,-53.8094131350517,-0.9));
#82625=CARTESIAN_POINT('Ctrl Pts',(-21.8402466550469,-54.4982264637947,
-0.6));
#82626=CARTESIAN_POINT('Ctrl Pts',(-21.8402466550469,-54.4982264637947,
-0.9));
#82627=CARTESIAN_POINT('Ctrl Pts',(-22.1336302533746,-54.2384724020958,
-0.6));
#82628=CARTESIAN_POINT('Ctrl Pts',(-22.1336302533746,-54.2384724020958,
-0.9));
#82629=CARTESIAN_POINT('Ctrl Pts',(-22.1753761544824,-53.8094131350517,
-0.6));
#82630=CARTESIAN_POINT('Ctrl Pts',(-22.1753761544824,-53.8094131350517,
-0.9));
#82631=CARTESIAN_POINT('',(-21.8402466550469,-54.4982264637947,-0.6));
#82632=CARTESIAN_POINT('Ctrl Pts',(-21.8402466550469,-54.4982264637947,
-0.6));
#82633=CARTESIAN_POINT('Ctrl Pts',(-22.1336302533746,-54.2384724020958,
-0.6));
#82634=CARTESIAN_POINT('Ctrl Pts',(-22.1753761544824,-53.8094131350517,
-0.6));
#82635=CARTESIAN_POINT('',(-21.8402466550469,-54.4982264637947,-0.9));
#82636=CARTESIAN_POINT('',(-21.8402466550469,-54.4982264637947,-0.6));
#82637=CARTESIAN_POINT('Ctrl Pts',(-21.8402466550469,-54.4982264637947,
-0.9));
#82638=CARTESIAN_POINT('Ctrl Pts',(-22.1336302533746,-54.2384724020958,
-0.9));
#82639=CARTESIAN_POINT('Ctrl Pts',(-22.1753761544824,-53.8094131350517,
-0.9));
#82640=CARTESIAN_POINT('Ctrl Pts',(-21.0830161347985,-54.7579811215401,
-0.6));
#82641=CARTESIAN_POINT('Ctrl Pts',(-21.0830161347985,-54.7579811215401,
-0.9));
#82642=CARTESIAN_POINT('Ctrl Pts',(-21.5468630567193,-54.7579811215401,
-0.6));
#82643=CARTESIAN_POINT('Ctrl Pts',(-21.5468630567193,-54.7579811215401,
-0.9));
#82644=CARTESIAN_POINT('Ctrl Pts',(-21.8402466550469,-54.4982264637947,
-0.6));
#82645=CARTESIAN_POINT('Ctrl Pts',(-21.8402466550469,-54.4982264637947,
-0.9));
#82646=CARTESIAN_POINT('Ctrl Pts',(-21.0830161347985,-54.7579811215401,
-0.6));
#82647=CARTESIAN_POINT('Ctrl Pts',(-21.5468630567193,-54.7579811215401,
-0.6));
#82648=CARTESIAN_POINT('Ctrl Pts',(-21.8402466550469,-54.4982264637947,
-0.6));
#82649=CARTESIAN_POINT('Ctrl Pts',(-21.0830161347985,-54.7579811215401,
-0.9));
#82650=CARTESIAN_POINT('Ctrl Pts',(-21.5468630567193,-54.7579811215401,
-0.9));
#82651=CARTESIAN_POINT('Ctrl Pts',(-21.8402466550469,-54.4982264637947,
-0.9));
#82652=CARTESIAN_POINT('Origin',(-21.0482272878289,-53.0521829128265,-0.9));
#82653=CARTESIAN_POINT('Ctrl Pts',(-13.8261279836297,-54.7579811215401,
-0.6));
#82654=CARTESIAN_POINT('Ctrl Pts',(-13.8261279836297,-54.7579811215401,
-0.9));
#82655=CARTESIAN_POINT('Ctrl Pts',(-14.3062100186944,-54.7579811215401,
-0.6));
#82656=CARTESIAN_POINT('Ctrl Pts',(-14.3062100186944,-54.7579811215401,
-0.9));
#82657=CARTESIAN_POINT('Ctrl Pts',(-14.684244133532,-54.5260576605797,-0.6));
#82658=CARTESIAN_POINT('Ctrl Pts',(-14.684244133532,-54.5260576605797,-0.9));
#82659=CARTESIAN_POINT('',(-13.8261279836297,-54.7579811215401,-0.6));
#82660=CARTESIAN_POINT('',(-14.684244133532,-54.5260576605797,-0.6));
#82661=CARTESIAN_POINT('Ctrl Pts',(-13.8261279836297,-54.7579811215401,
-0.6));
#82662=CARTESIAN_POINT('Ctrl Pts',(-14.3062100186944,-54.7579811215401,
-0.6));
#82663=CARTESIAN_POINT('Ctrl Pts',(-14.684244133532,-54.5260576605797,-0.6));
#82664=CARTESIAN_POINT('',(-13.8261279836297,-54.7579811215401,-0.9));
#82665=CARTESIAN_POINT('',(-13.8261279836297,-54.7579811215401,-0.6));
#82666=CARTESIAN_POINT('',(-14.684244133532,-54.5260576605797,-0.9));
#82667=CARTESIAN_POINT('Ctrl Pts',(-13.8261279836297,-54.7579811215401,
-0.9));
#82668=CARTESIAN_POINT('Ctrl Pts',(-14.3062100186944,-54.7579811215401,
-0.9));
#82669=CARTESIAN_POINT('Ctrl Pts',(-14.684244133532,-54.5260576605797,-0.9));
#82670=CARTESIAN_POINT('',(-14.684244133532,-54.5260576605797,-0.6));
#82671=CARTESIAN_POINT('Ctrl Pts',(-13.0004796758294,-54.5480899214745,
-0.6));
#82672=CARTESIAN_POINT('Ctrl Pts',(-13.0004796758294,-54.5480899214745,
-0.9));
#82673=CARTESIAN_POINT('Ctrl Pts',(-13.3831534162164,-54.7579811215401,
-0.6));
#82674=CARTESIAN_POINT('Ctrl Pts',(-13.3831534162164,-54.7579811215401,
-0.9));
#82675=CARTESIAN_POINT('Ctrl Pts',(-13.8261279836297,-54.7579811215401,
-0.6));
#82676=CARTESIAN_POINT('Ctrl Pts',(-13.8261279836297,-54.7579811215401,
-0.9));
#82677=CARTESIAN_POINT('',(-13.0004796758294,-54.5480899214745,-0.6));
#82678=CARTESIAN_POINT('Ctrl Pts',(-13.0004796758294,-54.5480899214745,
-0.6));
#82679=CARTESIAN_POINT('Ctrl Pts',(-13.3831534162164,-54.7579811215401,
-0.6));
#82680=CARTESIAN_POINT('Ctrl Pts',(-13.8261279836297,-54.7579811215401,
-0.6));
#82681=CARTESIAN_POINT('',(-13.0004796758294,-54.5480899214745,-0.9));
#82682=CARTESIAN_POINT('',(-13.0004796758294,-54.5480899214745,-0.6));
#82683=CARTESIAN_POINT('Ctrl Pts',(-13.0004796758294,-54.5480899214745,
-0.9));
#82684=CARTESIAN_POINT('Ctrl Pts',(-13.3831534162164,-54.7579811215401,
-0.9));
#82685=CARTESIAN_POINT('Ctrl Pts',(-13.8261279836297,-54.7579811215401,
-0.9));
#82686=CARTESIAN_POINT('Ctrl Pts',(-12.4090728536248,-53.9300135970116,
-0.6));
#82687=CARTESIAN_POINT('Ctrl Pts',(-12.4090728536248,-53.9300135970116,
-0.9));
#82688=CARTESIAN_POINT('Ctrl Pts',(-12.6178059354424,-54.3381993174553,
-0.6));
#82689=CARTESIAN_POINT('Ctrl Pts',(-12.6178059354424,-54.3381993174553,
-0.9));
#82690=CARTESIAN_POINT('Ctrl Pts',(-13.0004796758294,-54.5480899214745,
-0.6));
#82691=CARTESIAN_POINT('Ctrl Pts',(-13.0004796758294,-54.5480899214745,
-0.9));
#82692=CARTESIAN_POINT('',(-12.4090728536248,-53.9300135970116,-0.6));
#82693=CARTESIAN_POINT('Ctrl Pts',(-12.4090728536248,-53.9300135970116,
-0.6));
#82694=CARTESIAN_POINT('Ctrl Pts',(-12.6178059354424,-54.3381993174553,
-0.6));
#82695=CARTESIAN_POINT('Ctrl Pts',(-13.0004796758294,-54.5480899214745,
-0.6));
#82696=CARTESIAN_POINT('',(-12.4090728536248,-53.9300135970116,-0.9));
#82697=CARTESIAN_POINT('',(-12.4090728536248,-53.9300135970116,-0.6));
#82698=CARTESIAN_POINT('Ctrl Pts',(-12.4090728536248,-53.9300135970116,
-0.9));
#82699=CARTESIAN_POINT('Ctrl Pts',(-12.6178059354424,-54.3381993174553,
-0.9));
#82700=CARTESIAN_POINT('Ctrl Pts',(-13.0004796758294,-54.5480899214745,
-0.9));
#82701=CARTESIAN_POINT('Ctrl Pts',(-12.200342155993,-53.0046383738518,-0.6));
#82702=CARTESIAN_POINT('Ctrl Pts',(-12.200342155993,-53.0046383738518,-0.9));
#82703=CARTESIAN_POINT('Ctrl Pts',(-12.200342155993,-53.5218278765678,-0.6));
#82704=CARTESIAN_POINT('Ctrl Pts',(-12.200342155993,-53.5218278765678,-0.9));
#82705=CARTESIAN_POINT('Ctrl Pts',(-12.4090728536248,-53.9300135970116,
-0.6));
#82706=CARTESIAN_POINT('Ctrl Pts',(-12.4090728536248,-53.9300135970116,
-0.9));
#82707=CARTESIAN_POINT('',(-12.200342155993,-53.0046383738518,-0.6));
#82708=CARTESIAN_POINT('Ctrl Pts',(-12.200342155993,-53.0046383738518,-0.6));
#82709=CARTESIAN_POINT('Ctrl Pts',(-12.200342155993,-53.5218278765678,-0.6));
#82710=CARTESIAN_POINT('Ctrl Pts',(-12.4090728536248,-53.9300135970116,
-0.6));
#82711=CARTESIAN_POINT('',(-12.200342155993,-53.0046383738518,-0.9));
#82712=CARTESIAN_POINT('',(-12.200342155993,-53.0046383738518,-0.6));
#82713=CARTESIAN_POINT('Ctrl Pts',(-12.200342155993,-53.0046383738518,-0.9));
#82714=CARTESIAN_POINT('Ctrl Pts',(-12.200342155993,-53.5218278765678,-0.9));
#82715=CARTESIAN_POINT('Ctrl Pts',(-12.4090728536248,-53.9300135970116,
-0.9));
#82716=CARTESIAN_POINT('Ctrl Pts',(-12.3986372724175,-52.0920191407204,
-0.6));
#82717=CARTESIAN_POINT('Ctrl Pts',(-12.3986372724175,-52.0920191407204,
-0.9));
#82718=CARTESIAN_POINT('Ctrl Pts',(-12.200342155993,-52.4944065213203,-0.6));
#82719=CARTESIAN_POINT('Ctrl Pts',(-12.200342155993,-52.4944065213203,-0.9));
#82720=CARTESIAN_POINT('Ctrl Pts',(-12.200342155993,-53.0046383738518,-0.6));
#82721=CARTESIAN_POINT('Ctrl Pts',(-12.200342155993,-53.0046383738518,-0.9));
#82722=CARTESIAN_POINT('',(-12.3986372724175,-52.0920191407204,-0.6));
#82723=CARTESIAN_POINT('Ctrl Pts',(-12.3986372724175,-52.0920191407204,
-0.6));
#82724=CARTESIAN_POINT('Ctrl Pts',(-12.200342155993,-52.4944065213203,-0.6));
#82725=CARTESIAN_POINT('Ctrl Pts',(-12.200342155993,-53.0046383738518,-0.6));
#82726=CARTESIAN_POINT('',(-12.3986372724175,-52.0920191407204,-0.9));
#82727=CARTESIAN_POINT('',(-12.3986372724175,-52.0920191407204,-0.6));
#82728=CARTESIAN_POINT('Ctrl Pts',(-12.3986372724175,-52.0920191407204,
-0.9));
#82729=CARTESIAN_POINT('Ctrl Pts',(-12.200342155993,-52.4944065213203,-0.9));
#82730=CARTESIAN_POINT('Ctrl Pts',(-12.200342155993,-53.0046383738518,-0.9));
#82731=CARTESIAN_POINT('Ctrl Pts',(-12.9749665036798,-51.4646653532982,
-0.6));
#82732=CARTESIAN_POINT('Ctrl Pts',(-12.9749665036798,-51.4646653532982,
-0.9));
#82733=CARTESIAN_POINT('Ctrl Pts',(-12.5969323888421,-51.6896311640739,
-0.6));
#82734=CARTESIAN_POINT('Ctrl Pts',(-12.5969323888421,-51.6896311640739,
-0.9));
#82735=CARTESIAN_POINT('Ctrl Pts',(-12.3986372724175,-52.0920191407204,
-0.6));
#82736=CARTESIAN_POINT('Ctrl Pts',(-12.3986372724175,-52.0920191407204,
-0.9));
#82737=CARTESIAN_POINT('',(-12.9749665036798,-51.4646653532982,-0.6));
#82738=CARTESIAN_POINT('Ctrl Pts',(-12.9749665036798,-51.4646653532982,
-0.6));
#82739=CARTESIAN_POINT('Ctrl Pts',(-12.5969323888421,-51.6896311640739,
-0.6));
#82740=CARTESIAN_POINT('Ctrl Pts',(-12.3986372724175,-52.0920191407204,
-0.6));
#82741=CARTESIAN_POINT('',(-12.9749665036798,-51.4646653532982,-0.9));
#82742=CARTESIAN_POINT('',(-12.9749665036798,-51.4646653532982,-0.6));
#82743=CARTESIAN_POINT('Ctrl Pts',(-12.9749665036798,-51.4646653532982,
-0.9));
#82744=CARTESIAN_POINT('Ctrl Pts',(-12.5969323888421,-51.6896311640739,
-0.9));
#82745=CARTESIAN_POINT('Ctrl Pts',(-12.3986372724175,-52.0920191407204,
-0.9));
#82746=CARTESIAN_POINT('Ctrl Pts',(-13.823808170855,-51.2396995425224,-0.6));
#82747=CARTESIAN_POINT('Ctrl Pts',(-13.823808170855,-51.2396995425224,-0.9));
#82748=CARTESIAN_POINT('Ctrl Pts',(-13.3530030027032,-51.2396995425224,
-0.6));
#82749=CARTESIAN_POINT('Ctrl Pts',(-13.3530030027032,-51.2396995425224,
-0.9));
#82750=CARTESIAN_POINT('Ctrl Pts',(-12.9749665036798,-51.4646653532982,
-0.6));
#82751=CARTESIAN_POINT('Ctrl Pts',(-12.9749665036798,-51.4646653532982,
-0.9));
#82752=CARTESIAN_POINT('',(-13.823808170855,-51.2396995425224,-0.6));
#82753=CARTESIAN_POINT('Ctrl Pts',(-13.823808170855,-51.2396995425224,-0.6));
#82754=CARTESIAN_POINT('Ctrl Pts',(-13.3530030027032,-51.2396995425224,
-0.6));
#82755=CARTESIAN_POINT('Ctrl Pts',(-12.9749665036798,-51.4646653532982,
-0.6));
#82756=CARTESIAN_POINT('',(-13.823808170855,-51.2396995425224,-0.9));
#82757=CARTESIAN_POINT('',(-13.823808170855,-51.2396995425224,-0.6));
#82758=CARTESIAN_POINT('Ctrl Pts',(-13.823808170855,-51.2396995425224,-0.9));
#82759=CARTESIAN_POINT('Ctrl Pts',(-13.3530030027032,-51.2396995425224,
-0.9));
#82760=CARTESIAN_POINT('Ctrl Pts',(-12.9749665036798,-51.4646653532982,
-0.9));
#82761=CARTESIAN_POINT('Ctrl Pts',(-14.9973401799798,-51.7186216711998,
-0.6));
#82762=CARTESIAN_POINT('Ctrl Pts',(-14.9973401799798,-51.7186216711998,
-0.9));
#82763=CARTESIAN_POINT('Ctrl Pts',(-14.5427713170648,-51.2396995425224,
-0.6));
#82764=CARTESIAN_POINT('Ctrl Pts',(-14.5427713170648,-51.2396995425224,
-0.9));
#82765=CARTESIAN_POINT('Ctrl Pts',(-13.823808170855,-51.2396995425224,-0.6));
#82766=CARTESIAN_POINT('Ctrl Pts',(-13.823808170855,-51.2396995425224,-0.9));
#82767=CARTESIAN_POINT('',(-14.9973401799798,-51.7186216711998,-0.6));
#82768=CARTESIAN_POINT('Ctrl Pts',(-14.9973401799798,-51.7186216711998,
-0.6));
#82769=CARTESIAN_POINT('Ctrl Pts',(-14.5427713170648,-51.2396995425224,
-0.6));
#82770=CARTESIAN_POINT('Ctrl Pts',(-13.823808170855,-51.2396995425224,-0.6));
#82771=CARTESIAN_POINT('',(-14.9973401799798,-51.7186216711998,-0.9));
#82772=CARTESIAN_POINT('',(-14.9973401799798,-51.7186216711998,-0.6));
#82773=CARTESIAN_POINT('Ctrl Pts',(-14.9973401799798,-51.7186216711998,
-0.9));
#82774=CARTESIAN_POINT('Ctrl Pts',(-14.5427713170648,-51.2396995425224,
-0.9));
#82775=CARTESIAN_POINT('Ctrl Pts',(-13.823808170855,-51.2396995425224,-0.9));
#82776=CARTESIAN_POINT('Ctrl Pts',(-15.4519114270806,-53.0440656542778,
-0.6));
#82777=CARTESIAN_POINT('Ctrl Pts',(-15.4519114270806,-53.0440656542778,
-0.9));
#82778=CARTESIAN_POINT('Ctrl Pts',(-15.4519114270806,-52.1975443959236,
-0.6));
#82779=CARTESIAN_POINT('Ctrl Pts',(-15.4519114270806,-52.1975443959236,
-0.9));
#82780=CARTESIAN_POINT('Ctrl Pts',(-14.9973401799798,-51.7186216711998,
-0.6));
#82781=CARTESIAN_POINT('Ctrl Pts',(-14.9973401799798,-51.7186216711998,
-0.9));
#82782=CARTESIAN_POINT('',(-15.4519114270806,-53.0440656542778,-0.6));
#82783=CARTESIAN_POINT('Ctrl Pts',(-15.4519114270806,-53.0440656542778,
-0.6));
#82784=CARTESIAN_POINT('Ctrl Pts',(-15.4519114270806,-52.1975443959236,
-0.6));
#82785=CARTESIAN_POINT('Ctrl Pts',(-14.9973401799798,-51.7186216711998,
-0.6));
#82786=CARTESIAN_POINT('',(-15.4519114270806,-53.0440656542778,-0.9));
#82787=CARTESIAN_POINT('',(-15.4519114270806,-53.0440656542778,-0.6));
#82788=CARTESIAN_POINT('Ctrl Pts',(-15.4519114270806,-53.0440656542778,
-0.9));
#82789=CARTESIAN_POINT('Ctrl Pts',(-15.4519114270806,-52.1975443959236,
-0.9));
#82790=CARTESIAN_POINT('Ctrl Pts',(-14.9973401799798,-51.7186216711998,
-0.9));
#82791=CARTESIAN_POINT('Ctrl Pts',(-15.2570960298181,-53.8929061293602,
-0.6));
#82792=CARTESIAN_POINT('Ctrl Pts',(-15.2570960298181,-53.8929061293602,
-0.9));
#82793=CARTESIAN_POINT('Ctrl Pts',(-15.4519114270806,-53.4916780591011,
-0.6));
#82794=CARTESIAN_POINT('Ctrl Pts',(-15.4519114270806,-53.4916780591011,
-0.9));
#82795=CARTESIAN_POINT('Ctrl Pts',(-15.4519114270806,-53.0440656542778,
-0.6));
#82796=CARTESIAN_POINT('Ctrl Pts',(-15.4519114270806,-53.0440656542778,
-0.9));
#82797=CARTESIAN_POINT('',(-15.2570960298181,-53.8929061293602,-0.6));
#82798=CARTESIAN_POINT('Ctrl Pts',(-15.2570960298181,-53.8929061293602,
-0.6));
#82799=CARTESIAN_POINT('Ctrl Pts',(-15.4519114270806,-53.4916780591011,
-0.6));
#82800=CARTESIAN_POINT('Ctrl Pts',(-15.4519114270806,-53.0440656542778,
-0.6));
#82801=CARTESIAN_POINT('',(-15.2570960298181,-53.8929061293602,-0.9));
#82802=CARTESIAN_POINT('',(-15.2570960298181,-53.8929061293602,-0.6));
#82803=CARTESIAN_POINT('Ctrl Pts',(-15.2570960298181,-53.8929061293602,
-0.9));
#82804=CARTESIAN_POINT('Ctrl Pts',(-15.4519114270806,-53.4916780591011,
-0.9));
#82805=CARTESIAN_POINT('Ctrl Pts',(-15.4519114270806,-53.0440656542778,
-0.9));
#82806=CARTESIAN_POINT('Ctrl Pts',(-14.684244133532,-54.5260576605797,-0.6));
#82807=CARTESIAN_POINT('Ctrl Pts',(-14.684244133532,-54.5260576605797,-0.9));
#82808=CARTESIAN_POINT('Ctrl Pts',(-15.0622806325555,-54.2941336035728,
-0.6));
#82809=CARTESIAN_POINT('Ctrl Pts',(-15.0622806325555,-54.2941336035728,
-0.9));
#82810=CARTESIAN_POINT('Ctrl Pts',(-15.2570960298181,-53.8929061293602,
-0.6));
#82811=CARTESIAN_POINT('Ctrl Pts',(-15.2570960298181,-53.8929061293602,
-0.9));
#82812=CARTESIAN_POINT('Ctrl Pts',(-14.684244133532,-54.5260576605797,-0.6));
#82813=CARTESIAN_POINT('Ctrl Pts',(-15.0622806325555,-54.2941336035728,
-0.6));
#82814=CARTESIAN_POINT('Ctrl Pts',(-15.2570960298181,-53.8929061293602,
-0.6));
#82815=CARTESIAN_POINT('Ctrl Pts',(-14.684244133532,-54.5260576605797,-0.9));
#82816=CARTESIAN_POINT('Ctrl Pts',(-15.0622806325555,-54.2941336035728,
-0.9));
#82817=CARTESIAN_POINT('Ctrl Pts',(-15.2570960298181,-53.8929061293602,
-0.9));
#82818=CARTESIAN_POINT('Origin',(-13.8261267915368,-52.9988403320313,-0.9));
#82819=CARTESIAN_POINT('Ctrl Pts',(-5.29945466667414,-52.0896999239922,
-0.6));
#82820=CARTESIAN_POINT('Ctrl Pts',(-5.29945466667414,-52.0896999239922,
-0.9));
#82821=CARTESIAN_POINT('Ctrl Pts',(-5.10115955024958,-52.4920873045921,
-0.6));
#82822=CARTESIAN_POINT('Ctrl Pts',(-5.10115955024958,-52.4920873045921,
-0.9));
#82823=CARTESIAN_POINT('Ctrl Pts',(-5.10115955024958,-52.9976807236671,
-0.6));
#82824=CARTESIAN_POINT('Ctrl Pts',(-5.10115955024958,-52.9976807236671,
-0.9));
#82825=CARTESIAN_POINT('',(-5.29945466667414,-52.0896999239922,-0.6));
#82826=CARTESIAN_POINT('',(-5.10115955024958,-52.9976807236671,-0.6));
#82827=CARTESIAN_POINT('Ctrl Pts',(-5.29945466667414,-52.0896999239922,
-0.6));
#82828=CARTESIAN_POINT('Ctrl Pts',(-5.10115955024958,-52.4920873045921,
-0.6));
#82829=CARTESIAN_POINT('Ctrl Pts',(-5.10115955024958,-52.9976807236671,
-0.6));
#82830=CARTESIAN_POINT('',(-5.29945466667414,-52.0896999239922,-0.9));
#82831=CARTESIAN_POINT('',(-5.29945466667414,-52.0896999239922,-0.6));
#82832=CARTESIAN_POINT('',(-5.10115955024958,-52.9976807236671,-0.9));
#82833=CARTESIAN_POINT('Ctrl Pts',(-5.29945466667414,-52.0896999239922,
-0.9));
#82834=CARTESIAN_POINT('Ctrl Pts',(-5.10115955024958,-52.4920873045921,
-0.9));
#82835=CARTESIAN_POINT('Ctrl Pts',(-5.10115955024958,-52.9976807236671,
-0.9));
#82836=CARTESIAN_POINT('',(-5.10115955024958,-52.9976807236671,-0.6));
#82837=CARTESIAN_POINT('Ctrl Pts',(-5.87578389793634,-51.4635060429573,
-0.6));
#82838=CARTESIAN_POINT('Ctrl Pts',(-5.87578389793634,-51.4635060429573,
-0.9));
#82839=CARTESIAN_POINT('Ctrl Pts',(-5.4977497830987,-51.6873125433922,-0.6));
#82840=CARTESIAN_POINT('Ctrl Pts',(-5.4977497830987,-51.6873125433922,-0.9));
#82841=CARTESIAN_POINT('Ctrl Pts',(-5.29945466667414,-52.0896999239922,
-0.6));
#82842=CARTESIAN_POINT('Ctrl Pts',(-5.29945466667414,-52.0896999239922,
-0.9));
#82843=CARTESIAN_POINT('',(-5.87578389793634,-51.4635060429573,-0.6));
#82844=CARTESIAN_POINT('Ctrl Pts',(-5.87578389793634,-51.4635060429573,
-0.6));
#82845=CARTESIAN_POINT('Ctrl Pts',(-5.4977497830987,-51.6873125433922,-0.6));
#82846=CARTESIAN_POINT('Ctrl Pts',(-5.29945466667414,-52.0896999239922,
-0.6));
#82847=CARTESIAN_POINT('',(-5.87578389793634,-51.4635060429573,-0.9));
#82848=CARTESIAN_POINT('',(-5.87578389793634,-51.4635060429573,-0.6));
#82849=CARTESIAN_POINT('Ctrl Pts',(-5.87578389793634,-51.4635060429573,
-0.9));
#82850=CARTESIAN_POINT('Ctrl Pts',(-5.4977497830987,-51.6873125433922,-0.9));
#82851=CARTESIAN_POINT('Ctrl Pts',(-5.29945466667414,-52.0896999239922,
-0.9));
#82852=CARTESIAN_POINT('Ctrl Pts',(-6.72462556511164,-51.2396995425224,
-0.6));
#82853=CARTESIAN_POINT('Ctrl Pts',(-6.72462556511164,-51.2396995425224,
-0.9));
#82854=CARTESIAN_POINT('Ctrl Pts',(-6.25382039695978,-51.2396995425224,
-0.6));
#82855=CARTESIAN_POINT('Ctrl Pts',(-6.25382039695978,-51.2396995425224,
-0.9));
#82856=CARTESIAN_POINT('Ctrl Pts',(-5.87578389793634,-51.4635060429573,
-0.6));
#82857=CARTESIAN_POINT('Ctrl Pts',(-5.87578389793634,-51.4635060429573,
-0.9));
#82858=CARTESIAN_POINT('',(-6.72462556511164,-51.2396995425224,-0.6));
#82859=CARTESIAN_POINT('Ctrl Pts',(-6.72462556511164,-51.2396995425224,
-0.6));
#82860=CARTESIAN_POINT('Ctrl Pts',(-6.25382039695978,-51.2396995425224,
-0.6));
#82861=CARTESIAN_POINT('Ctrl Pts',(-5.87578389793634,-51.4635060429573,
-0.6));
#82862=CARTESIAN_POINT('',(-6.72462556511164,-51.2396995425224,-0.9));
#82863=CARTESIAN_POINT('',(-6.72462556511164,-51.2396995425224,-0.6));
#82864=CARTESIAN_POINT('Ctrl Pts',(-6.72462556511164,-51.2396995425224,
-0.9));
#82865=CARTESIAN_POINT('Ctrl Pts',(-6.25382039695978,-51.2396995425224,
-0.9));
#82866=CARTESIAN_POINT('Ctrl Pts',(-5.87578389793634,-51.4635060429573,
-0.9));
#82867=CARTESIAN_POINT('Ctrl Pts',(-7.56766650825739,-51.4553884863853,
-0.6));
#82868=CARTESIAN_POINT('Ctrl Pts',(-7.56766650825739,-51.4553884863853,
-0.9));
#82869=CARTESIAN_POINT('Ctrl Pts',(-7.19079110771418,-51.2396995425224,
-0.6));
#82870=CARTESIAN_POINT('Ctrl Pts',(-7.19079110771418,-51.2396995425224,
-0.9));
#82871=CARTESIAN_POINT('Ctrl Pts',(-6.72462556511164,-51.2396995425224,
-0.6));
#82872=CARTESIAN_POINT('Ctrl Pts',(-6.72462556511164,-51.2396995425224,
-0.9));
#82873=CARTESIAN_POINT('',(-7.56766650825739,-51.4553884863853,-0.6));
#82874=CARTESIAN_POINT('Ctrl Pts',(-7.56766650825739,-51.4553884863853,
-0.6));
#82875=CARTESIAN_POINT('Ctrl Pts',(-7.19079110771418,-51.2396995425224,
-0.6));
#82876=CARTESIAN_POINT('Ctrl Pts',(-6.72462556511164,-51.2396995425224,
-0.6));
#82877=CARTESIAN_POINT('',(-7.56766650825739,-51.4553884863853,-0.9));
#82878=CARTESIAN_POINT('',(-7.56766650825739,-51.4553884863853,-0.6));
#82879=CARTESIAN_POINT('Ctrl Pts',(-7.56766650825739,-51.4553884863853,
-0.9));
#82880=CARTESIAN_POINT('Ctrl Pts',(-7.19079110771418,-51.2396995425224,
-0.9));
#82881=CARTESIAN_POINT('Ctrl Pts',(-6.72462556511164,-51.2396995425224,
-0.9));
#82882=CARTESIAN_POINT('Ctrl Pts',(-8.14863536506891,-52.0839015841484,
-0.6));
#82883=CARTESIAN_POINT('Ctrl Pts',(-8.14863536506891,-52.0839015841484,
-0.9));
#82884=CARTESIAN_POINT('Ctrl Pts',(-7.94454429298639,-51.6710774302483,
-0.6));
#82885=CARTESIAN_POINT('Ctrl Pts',(-7.94454429298639,-51.6710774302483,
-0.9));
#82886=CARTESIAN_POINT('Ctrl Pts',(-7.56766650825739,-51.4553884863853,
-0.6));
#82887=CARTESIAN_POINT('Ctrl Pts',(-7.56766650825739,-51.4553884863853,
-0.9));
#82888=CARTESIAN_POINT('',(-8.14863536506891,-52.0839015841484,-0.6));
#82889=CARTESIAN_POINT('Ctrl Pts',(-8.14863536506891,-52.0839015841484,
-0.6));
#82890=CARTESIAN_POINT('Ctrl Pts',(-7.94454429298639,-51.6710774302483,
-0.6));
#82891=CARTESIAN_POINT('Ctrl Pts',(-7.56766650825739,-51.4553884863853,
-0.6));
#82892=CARTESIAN_POINT('',(-8.14863536506891,-52.0839015841484,-0.9));
#82893=CARTESIAN_POINT('',(-8.14863536506891,-52.0839015841484,-0.6));
#82894=CARTESIAN_POINT('Ctrl Pts',(-8.14863536506891,-52.0839015841484,
-0.9));
#82895=CARTESIAN_POINT('Ctrl Pts',(-7.94454429298639,-51.6710774302483,
-0.9));
#82896=CARTESIAN_POINT('Ctrl Pts',(-7.56766650825739,-51.4553884863853,
-0.9));
#82897=CARTESIAN_POINT('Ctrl Pts',(-8.35272882133722,-52.9999999403954,
-0.6));
#82898=CARTESIAN_POINT('Ctrl Pts',(-8.35272882133722,-52.9999999403954,
-0.9));
#82899=CARTESIAN_POINT('Ctrl Pts',(-8.35272882133722,-52.4967257380486,
-0.6));
#82900=CARTESIAN_POINT('Ctrl Pts',(-8.35272882133722,-52.4967257380486,
-0.9));
#82901=CARTESIAN_POINT('Ctrl Pts',(-8.14863536506891,-52.0839015841484,
-0.6));
#82902=CARTESIAN_POINT('Ctrl Pts',(-8.14863536506891,-52.0839015841484,
-0.9));
#82903=CARTESIAN_POINT('',(-8.35272882133722,-52.9999999403954,-0.6));
#82904=CARTESIAN_POINT('Ctrl Pts',(-8.35272882133722,-52.9999999403954,
-0.6));
#82905=CARTESIAN_POINT('Ctrl Pts',(-8.35272882133722,-52.4967257380486,
-0.6));
#82906=CARTESIAN_POINT('Ctrl Pts',(-8.14863536506891,-52.0839015841484,
-0.6));
#82907=CARTESIAN_POINT('',(-8.35272882133722,-52.9999999403954,-0.9));
#82908=CARTESIAN_POINT('',(-8.35272882133722,-52.9999999403954,-0.6));
#82909=CARTESIAN_POINT('Ctrl Pts',(-8.35272882133722,-52.9999999403954,
-0.9));
#82910=CARTESIAN_POINT('Ctrl Pts',(-8.35272882133722,-52.4967257380486,
-0.9));
#82911=CARTESIAN_POINT('Ctrl Pts',(-8.14863536506891,-52.0839015841484,
-0.9));
#82912=CARTESIAN_POINT('Ctrl Pts',(-8.14979646354914,-53.9091406464577,
-0.6));
#82913=CARTESIAN_POINT('Ctrl Pts',(-8.14979646354914,-53.9091406464577,
-0.9));
#82914=CARTESIAN_POINT('Ctrl Pts',(-8.35272882133722,-53.5055933594704,
-0.6));
#82915=CARTESIAN_POINT('Ctrl Pts',(-8.35272882133722,-53.5055933594704,
-0.9));
#82916=CARTESIAN_POINT('Ctrl Pts',(-8.35272882133722,-52.9999999403954,
-0.6));
#82917=CARTESIAN_POINT('Ctrl Pts',(-8.35272882133722,-52.9999999403954,
-0.9));
#82918=CARTESIAN_POINT('',(-8.14979646354914,-53.9091406464577,-0.6));
#82919=CARTESIAN_POINT('Ctrl Pts',(-8.14979646354914,-53.9091406464577,
-0.6));
#82920=CARTESIAN_POINT('Ctrl Pts',(-8.35272882133722,-53.5055933594704,
-0.6));
#82921=CARTESIAN_POINT('Ctrl Pts',(-8.35272882133722,-52.9999999403954,
-0.6));
#82922=CARTESIAN_POINT('',(-8.14979646354914,-53.9091406464577,-0.9));
#82923=CARTESIAN_POINT('',(-8.14979646354914,-53.9091406464577,-0.6));
#82924=CARTESIAN_POINT('Ctrl Pts',(-8.14979646354914,-53.9091406464577,
-0.9));
#82925=CARTESIAN_POINT('Ctrl Pts',(-8.35272882133722,-53.5055933594704,
-0.9));
#82926=CARTESIAN_POINT('Ctrl Pts',(-8.35272882133722,-52.9999999403954,
-0.9));
#82927=CARTESIAN_POINT('Ctrl Pts',(-7.57114741951227,-54.5353345274925,
-0.6));
#82928=CARTESIAN_POINT('Ctrl Pts',(-7.57114741951227,-54.5353345274925,
-0.9));
#82929=CARTESIAN_POINT('Ctrl Pts',(-7.94686172157526,-54.312687933445,-0.6));
#82930=CARTESIAN_POINT('Ctrl Pts',(-7.94686172157526,-54.312687933445,-0.9));
#82931=CARTESIAN_POINT('Ctrl Pts',(-8.14979646354914,-53.9091406464577,
-0.6));
#82932=CARTESIAN_POINT('Ctrl Pts',(-8.14979646354914,-53.9091406464577,
-0.9));
#82933=CARTESIAN_POINT('',(-7.57114741951227,-54.5353345274925,-0.6));
#82934=CARTESIAN_POINT('Ctrl Pts',(-7.57114741951227,-54.5353345274925,
-0.6));
#82935=CARTESIAN_POINT('Ctrl Pts',(-7.94686172157526,-54.312687933445,-0.6));
#82936=CARTESIAN_POINT('Ctrl Pts',(-8.14979646354914,-53.9091406464577,
-0.6));
#82937=CARTESIAN_POINT('',(-7.57114741951227,-54.5353345274925,-0.9));
#82938=CARTESIAN_POINT('',(-7.57114741951227,-54.5353345274925,-0.6));
#82939=CARTESIAN_POINT('Ctrl Pts',(-7.57114741951227,-54.5353345274925,
-0.9));
#82940=CARTESIAN_POINT('Ctrl Pts',(-7.94686172157526,-54.312687933445,-0.9));
#82941=CARTESIAN_POINT('Ctrl Pts',(-8.14979646354914,-53.9091406464577,
-0.9));
#82942=CARTESIAN_POINT('Ctrl Pts',(-6.73390243202448,-54.7579811215401,
-0.6));
#82943=CARTESIAN_POINT('Ctrl Pts',(-6.73390243202448,-54.7579811215401,
-0.9));
#82944=CARTESIAN_POINT('Ctrl Pts',(-7.19543073326349,-54.7579811215401,
-0.6));
#82945=CARTESIAN_POINT('Ctrl Pts',(-7.19543073326349,-54.7579811215401,
-0.9));
#82946=CARTESIAN_POINT('Ctrl Pts',(-7.57114741951227,-54.5353345274925,
-0.6));
#82947=CARTESIAN_POINT('Ctrl Pts',(-7.57114741951227,-54.5353345274925,
-0.9));
#82948=CARTESIAN_POINT('',(-6.73390243202448,-54.7579811215401,-0.6));
#82949=CARTESIAN_POINT('Ctrl Pts',(-6.73390243202448,-54.7579811215401,
-0.6));
#82950=CARTESIAN_POINT('Ctrl Pts',(-7.19543073326349,-54.7579811215401,
-0.6));
#82951=CARTESIAN_POINT('Ctrl Pts',(-7.57114741951227,-54.5353345274925,
-0.6));
#82952=CARTESIAN_POINT('',(-6.73390243202448,-54.7579811215401,-0.9));
#82953=CARTESIAN_POINT('',(-6.73390243202448,-54.7579811215401,-0.6));
#82954=CARTESIAN_POINT('Ctrl Pts',(-6.73390243202448,-54.7579811215401,
-0.9));
#82955=CARTESIAN_POINT('Ctrl Pts',(-7.19543073326349,-54.7579811215401,
-0.9));
#82956=CARTESIAN_POINT('Ctrl Pts',(-7.57114741951227,-54.5353345274925,
-0.9));
#82957=CARTESIAN_POINT('Ctrl Pts',(-5.89897725731134,-54.5469306111336,
-0.6));
#82958=CARTESIAN_POINT('Ctrl Pts',(-5.89897725731134,-54.5469306111336,
-0.9));
#82959=CARTESIAN_POINT('Ctrl Pts',(-6.27701137214899,-54.7579811215401,
-0.6));
#82960=CARTESIAN_POINT('Ctrl Pts',(-6.27701137214899,-54.7579811215401,
-0.9));
#82961=CARTESIAN_POINT('Ctrl Pts',(-6.73390243202448,-54.7579811215401,
-0.6));
#82962=CARTESIAN_POINT('Ctrl Pts',(-6.73390243202448,-54.7579811215401,
-0.9));
#82963=CARTESIAN_POINT('',(-5.89897725731134,-54.5469306111336,-0.6));
#82964=CARTESIAN_POINT('Ctrl Pts',(-5.89897725731134,-54.5469306111336,
-0.6));
#82965=CARTESIAN_POINT('Ctrl Pts',(-6.27701137214899,-54.7579811215401,
-0.6));
#82966=CARTESIAN_POINT('Ctrl Pts',(-6.73390243202448,-54.7579811215401,
-0.6));
#82967=CARTESIAN_POINT('',(-5.89897725731134,-54.5469306111336,-0.9));
#82968=CARTESIAN_POINT('',(-5.89897725731134,-54.5469306111336,-0.6));
#82969=CARTESIAN_POINT('Ctrl Pts',(-5.89897725731134,-54.5469306111336,
-0.9));
#82970=CARTESIAN_POINT('Ctrl Pts',(-6.27701137214899,-54.7579811215401,
-0.9));
#82971=CARTESIAN_POINT('Ctrl Pts',(-6.73390243202448,-54.7579811215401,
-0.9));
#82972=CARTESIAN_POINT('Ctrl Pts',(-5.16841743141413,-54.9643931984901,
-0.6));
#82973=CARTESIAN_POINT('Ctrl Pts',(-5.16841743141413,-54.9643931984901,
-0.9));
#82974=CARTESIAN_POINT('Ctrl Pts',(-5.53485725075006,-54.8321966528893,
-0.6));
#82975=CARTESIAN_POINT('Ctrl Pts',(-5.53485725075006,-54.8321966528893,
-0.9));
#82976=CARTESIAN_POINT('Ctrl Pts',(-5.89897725731134,-54.5469306111336,
-0.6));
#82977=CARTESIAN_POINT('Ctrl Pts',(-5.89897725731134,-54.5469306111336,
-0.9));
#82978=CARTESIAN_POINT('',(-5.16841743141413,-54.9643931984901,-0.6));
#82979=CARTESIAN_POINT('Ctrl Pts',(-5.16841743141413,-54.9643931984901,
-0.6));
#82980=CARTESIAN_POINT('Ctrl Pts',(-5.53485725075006,-54.8321966528893,
-0.6));
#82981=CARTESIAN_POINT('Ctrl Pts',(-5.89897725731134,-54.5469306111336,
-0.6));
#82982=CARTESIAN_POINT('',(-5.16841743141413,-54.9643931984901,-0.9));
#82983=CARTESIAN_POINT('',(-5.16841743141413,-54.9643931984901,-0.6));
#82984=CARTESIAN_POINT('Ctrl Pts',(-5.16841743141413,-54.9643931984901,
-0.9));
#82985=CARTESIAN_POINT('Ctrl Pts',(-5.53485725075006,-54.8321966528893,
-0.9));
#82986=CARTESIAN_POINT('Ctrl Pts',(-5.89897725731134,-54.5469306111336,
-0.9));
#82987=CARTESIAN_POINT('Origin',(-5.03622148185968,-54.6512959599495,-0.6));
#82988=CARTESIAN_POINT('',(-5.03622148185968,-54.6512959599495,-0.6));
#82989=CARTESIAN_POINT('',(-4.359374539743,-53.0482293818458,-0.6));
#82990=CARTESIAN_POINT('',(-5.03622148185968,-54.6512959599495,-0.9));
#82991=CARTESIAN_POINT('',(-5.03622148185968,-54.6512959599495,-0.6));
#82992=CARTESIAN_POINT('',(-5.03622148185968,-54.6512959599495,-0.9));
#82993=CARTESIAN_POINT('Ctrl Pts',(-5.61371181160212,-54.3358801007271,
-0.6));
#82994=CARTESIAN_POINT('Ctrl Pts',(-5.61371181160212,-54.3358801007271,
-0.9));
#82995=CARTESIAN_POINT('Ctrl Pts',(-5.30061338096857,-54.55156904459,-0.6));
#82996=CARTESIAN_POINT('Ctrl Pts',(-5.30061338096857,-54.55156904459,-0.9));
#82997=CARTESIAN_POINT('Ctrl Pts',(-5.03622148185968,-54.6512959599495,
-0.6));
#82998=CARTESIAN_POINT('Ctrl Pts',(-5.03622148185968,-54.6512959599495,
-0.9));
#82999=CARTESIAN_POINT('',(-5.61371181160212,-54.3358801007271,-0.6));
#83000=CARTESIAN_POINT('Ctrl Pts',(-5.61371181160212,-54.3358801007271,
-0.6));
#83001=CARTESIAN_POINT('Ctrl Pts',(-5.30061338096857,-54.55156904459,-0.6));
#83002=CARTESIAN_POINT('Ctrl Pts',(-5.03622148185968,-54.6512959599495,
-0.6));
#83003=CARTESIAN_POINT('',(-5.61371181160212,-54.3358801007271,-0.9));
#83004=CARTESIAN_POINT('',(-5.61371181160212,-54.3358801007271,-0.6));
#83005=CARTESIAN_POINT('Ctrl Pts',(-5.61371181160212,-54.3358801007271,
-0.9));
#83006=CARTESIAN_POINT('Ctrl Pts',(-5.30061338096857,-54.55156904459,-0.9));
#83007=CARTESIAN_POINT('Ctrl Pts',(-5.03622148185968,-54.6512959599495,
-0.9));
#83008=CARTESIAN_POINT('Ctrl Pts',(-5.22871825844049,-53.7525920271873,
-0.6));
#83009=CARTESIAN_POINT('Ctrl Pts',(-5.22871825844049,-53.7525920271873,
-0.9));
#83010=CARTESIAN_POINT('Ctrl Pts',(-5.35627696663141,-54.0877215266228,
-0.6));
#83011=CARTESIAN_POINT('Ctrl Pts',(-5.35627696663141,-54.0877215266228,
-0.9));
#83012=CARTESIAN_POINT('Ctrl Pts',(-5.61371181160212,-54.3358801007271,
-0.6));
#83013=CARTESIAN_POINT('Ctrl Pts',(-5.61371181160212,-54.3358801007271,
-0.9));
#83014=CARTESIAN_POINT('',(-5.22871825844049,-53.7525920271873,-0.6));
#83015=CARTESIAN_POINT('Ctrl Pts',(-5.22871825844049,-53.7525920271873,
-0.6));
#83016=CARTESIAN_POINT('Ctrl Pts',(-5.35627696663141,-54.0877215266228,
-0.6));
#83017=CARTESIAN_POINT('Ctrl Pts',(-5.61371181160212,-54.3358801007271,
-0.6));
#83018=CARTESIAN_POINT('',(-5.22871825844049,-53.7525920271873,-0.9));
#83019=CARTESIAN_POINT('',(-5.22871825844049,-53.7525920271873,-0.6));
#83020=CARTESIAN_POINT('Ctrl Pts',(-5.22871825844049,-53.7525920271873,
-0.9));
#83021=CARTESIAN_POINT('Ctrl Pts',(-5.35627696663141,-54.0877215266228,
-0.9));
#83022=CARTESIAN_POINT('Ctrl Pts',(-5.61371181160212,-54.3358801007271,
-0.9));
#83023=CARTESIAN_POINT('Ctrl Pts',(-5.10115955024958,-52.9976807236671,
-0.6));
#83024=CARTESIAN_POINT('Ctrl Pts',(-5.10115955024958,-52.9976807236671,
-0.9));
#83025=CARTESIAN_POINT('Ctrl Pts',(-5.10115955024958,-53.4174625277519,
-0.6));
#83026=CARTESIAN_POINT('Ctrl Pts',(-5.10115955024958,-53.4174625277519,
-0.9));
#83027=CARTESIAN_POINT('Ctrl Pts',(-5.22871825844049,-53.7525920271873,
-0.6));
#83028=CARTESIAN_POINT('Ctrl Pts',(-5.22871825844049,-53.7525920271873,
-0.9));
#83029=CARTESIAN_POINT('Ctrl Pts',(-5.10115955024958,-52.9976807236671,
-0.6));
#83030=CARTESIAN_POINT('Ctrl Pts',(-5.10115955024958,-53.4174625277519,
-0.6));
#83031=CARTESIAN_POINT('Ctrl Pts',(-5.22871825844049,-53.7525920271873,
-0.6));
#83032=CARTESIAN_POINT('Ctrl Pts',(-5.10115955024958,-52.9976807236671,
-0.9));
#83033=CARTESIAN_POINT('Ctrl Pts',(-5.10115955024958,-53.4174625277519,
-0.9));
#83034=CARTESIAN_POINT('Ctrl Pts',(-5.22871825844049,-53.7525920271873,
-0.9));
#83035=CARTESIAN_POINT('Origin',(-6.69447515159845,-53.1020463705063,-0.9));
#83036=CARTESIAN_POINT('Origin',(-0.606480576097965,-54.2987720370293,-0.6));
#83037=CARTESIAN_POINT('',(-0.606480576097965,-54.2987720370293,-0.6));
#83038=CARTESIAN_POINT('',(1.48083116859198,-54.2987720370293,-0.6));
#83039=CARTESIAN_POINT('',(-0.303240288048983,-54.2987720370293,-0.6));
#83040=CARTESIAN_POINT('',(-0.606480576097965,-54.2987720370293,-0.9));
#83041=CARTESIAN_POINT('',(-0.606480576097965,-54.2987720370293,-0.6));
#83042=CARTESIAN_POINT('',(1.48083116859198,-54.2987720370293,-0.9));
#83043=CARTESIAN_POINT('',(-0.606480576097965,-54.2987720370293,-0.9));
#83044=CARTESIAN_POINT('',(1.48083116859198,-54.2987720370293,-0.6));
#83045=CARTESIAN_POINT('Origin',(-0.606480576097965,-53.1414733529091,-0.6));
#83046=CARTESIAN_POINT('',(-0.606480576097965,-53.1414733529091,-0.6));
#83047=CARTESIAN_POINT('',(-0.606480576097965,-53.0707366764545,-0.6));
#83048=CARTESIAN_POINT('',(-0.606480576097965,-53.1414733529091,-0.9));
#83049=CARTESIAN_POINT('',(-0.606480576097965,-53.1414733529091,-0.6));
#83050=CARTESIAN_POINT('',(-0.606480576097965,-53.1414733529091,-0.9));
#83051=CARTESIAN_POINT('Origin',(1.2744202837348,-53.1414733529091,-0.6));
#83052=CARTESIAN_POINT('',(1.2744202837348,-53.1414733529091,-0.6));
#83053=CARTESIAN_POINT('',(0.637210141867399,-53.1414733529091,-0.6));
#83054=CARTESIAN_POINT('',(1.2744202837348,-53.1414733529091,-0.9));
#83055=CARTESIAN_POINT('',(1.2744202837348,-53.1414733529091,-0.6));
#83056=CARTESIAN_POINT('',(1.2744202837348,-53.1414733529091,-0.9));
#83057=CARTESIAN_POINT('Origin',(1.2744202837348,-52.7425650954247,-0.6));
#83058=CARTESIAN_POINT('',(1.2744202837348,-52.7425650954247,-0.6));
#83059=CARTESIAN_POINT('',(1.2744202837348,-52.8712825477123,-0.6));
#83060=CARTESIAN_POINT('',(1.2744202837348,-52.7425650954247,-0.9));
#83061=CARTESIAN_POINT('',(1.2744202837348,-52.7425650954247,-0.6));
#83062=CARTESIAN_POINT('',(1.2744202837348,-52.7425650954247,-0.9));
#83063=CARTESIAN_POINT('Origin',(-0.606480576097965,-52.7425650954247,-0.6));
#83064=CARTESIAN_POINT('',(-0.606480576097965,-52.7425650954247,-0.6));
#83065=CARTESIAN_POINT('',(-0.303240288048983,-52.7425650954247,-0.6));
#83066=CARTESIAN_POINT('',(-0.606480576097965,-52.7425650954247,-0.9));
#83067=CARTESIAN_POINT('',(-0.606480576097965,-52.7425650954247,-0.6));
#83068=CARTESIAN_POINT('',(-0.606480576097965,-52.7425650954247,-0.9));
#83069=CARTESIAN_POINT('Origin',(-0.606480576097965,-51.7012278437614,-0.6));
#83070=CARTESIAN_POINT('',(-0.606480576097965,-51.7012278437614,-0.6));
#83071=CARTESIAN_POINT('',(-0.606480576097965,-52.3506139218807,-0.6));
#83072=CARTESIAN_POINT('',(-0.606480576097965,-51.7012278437614,-0.9));
#83073=CARTESIAN_POINT('',(-0.606480576097965,-51.7012278437614,-0.6));
#83074=CARTESIAN_POINT('',(-0.606480576097965,-51.7012278437614,-0.9));
#83075=CARTESIAN_POINT('Origin',(1.40197899192572,-51.7012278437614,-0.6));
#83076=CARTESIAN_POINT('',(1.40197899192572,-51.7012278437614,-0.6));
#83077=CARTESIAN_POINT('',(0.700989495962858,-51.7012278437614,-0.6));
#83078=CARTESIAN_POINT('',(1.40197899192572,-51.7012278437614,-0.9));
#83079=CARTESIAN_POINT('',(1.40197899192572,-51.7012278437614,-0.6));
#83080=CARTESIAN_POINT('',(1.40197899192572,-51.7012278437614,-0.9));
#83081=CARTESIAN_POINT('Origin',(1.40197899192572,-51.3000003695488,-0.6));
#83082=CARTESIAN_POINT('',(1.40197899192572,-51.3000003695488,-0.6));
#83083=CARTESIAN_POINT('',(1.40197899192572,-52.1500001847744,-0.6));
#83084=CARTESIAN_POINT('',(1.40197899192572,-51.3000003695488,-0.9));
#83085=CARTESIAN_POINT('',(1.40197899192572,-51.3000003695488,-0.6));
#83086=CARTESIAN_POINT('',(1.40197899192572,-51.3000003695488,-0.9));
#83087=CARTESIAN_POINT('Origin',(-1.05641219764948,-51.3000003695488,-0.6));
#83088=CARTESIAN_POINT('',(-1.05641219764948,-51.3000003695488,-0.6));
#83089=CARTESIAN_POINT('',(-0.528206098824739,-51.3000003695488,-0.6));
#83090=CARTESIAN_POINT('',(-1.05641219764948,-51.3000003695488,-0.9));
#83091=CARTESIAN_POINT('',(-1.05641219764948,-51.3000003695488,-0.6));
#83092=CARTESIAN_POINT('',(-1.05641219764948,-51.3000003695488,-0.9));
#83093=CARTESIAN_POINT('Origin',(-1.05641219764948,-54.7000001072884,-0.6));
#83094=CARTESIAN_POINT('',(-1.05641219764948,-54.7000001072884,-0.6));
#83095=CARTESIAN_POINT('',(-1.05641219764948,-53.8500000536442,-0.6));
#83096=CARTESIAN_POINT('',(-1.05641219764948,-54.7000001072884,-0.9));
#83097=CARTESIAN_POINT('',(-1.05641219764948,-54.7000001072884,-0.6));
#83098=CARTESIAN_POINT('',(-1.05641219764948,-54.7000001072884,-0.9));
#83099=CARTESIAN_POINT('Origin',(1.48083116859198,-54.7000001072884,-0.6));
#83100=CARTESIAN_POINT('',(1.48083116859198,-54.7000001072884,-0.6));
#83101=CARTESIAN_POINT('',(0.740415584295988,-54.7000001072884,-0.6));
#83102=CARTESIAN_POINT('',(1.48083116859198,-54.7000001072884,-0.9));
#83103=CARTESIAN_POINT('',(1.48083116859198,-54.7000001072884,-0.6));
#83104=CARTESIAN_POINT('',(1.48083116859198,-54.7000001072884,-0.9));
#83105=CARTESIAN_POINT('Origin',(1.48083116859198,-54.2987720370293,-0.6));
#83106=CARTESIAN_POINT('',(1.48083116859198,-53.6493860185146,-0.6));
#83107=CARTESIAN_POINT('',(1.48083116859198,-54.2987720370293,-0.9));
#83108=CARTESIAN_POINT('Origin',(0.212209485471249,-53.0000002384186,-0.9));
#83109=CARTESIAN_POINT('Origin',(1.88669826835394,-53.2597545981407,-0.6));
#83110=CARTESIAN_POINT('',(1.88669826835394,-53.2597545981407,-0.6));
#83111=CARTESIAN_POINT('',(3.16923525184393,-53.2597545981407,-0.6));
#83112=CARTESIAN_POINT('',(0.94334913417697,-53.2597545981407,-0.6));
#83113=CARTESIAN_POINT('',(1.88669826835394,-53.2597545981407,-0.9));
#83114=CARTESIAN_POINT('',(1.88669826835394,-53.2597545981407,-0.6));
#83115=CARTESIAN_POINT('',(3.16923525184393,-53.2597545981407,-0.9));
#83116=CARTESIAN_POINT('',(1.88669826835394,-53.2597545981407,-0.9));
#83117=CARTESIAN_POINT('',(3.16923525184393,-53.2597545981407,-0.6));
#83118=CARTESIAN_POINT('Origin',(1.88669826835394,-53.6795364022255,-0.6));
#83119=CARTESIAN_POINT('',(1.88669826835394,-53.6795364022255,-0.6));
#83120=CARTESIAN_POINT('',(1.88669826835394,-53.3397682011127,-0.6));
#83121=CARTESIAN_POINT('',(1.88669826835394,-53.6795364022255,-0.9));
#83122=CARTESIAN_POINT('',(1.88669826835394,-53.6795364022255,-0.6));
#83123=CARTESIAN_POINT('',(1.88669826835394,-53.6795364022255,-0.9));
#83124=CARTESIAN_POINT('Origin',(3.16923525184393,-53.6795364022255,-0.6));
#83125=CARTESIAN_POINT('',(3.16923525184393,-53.6795364022255,-0.6));
#83126=CARTESIAN_POINT('',(1.58461762592196,-53.6795364022255,-0.6));
#83127=CARTESIAN_POINT('',(3.16923525184393,-53.6795364022255,-0.9));
#83128=CARTESIAN_POINT('',(3.16923525184393,-53.6795364022255,-0.6));
#83129=CARTESIAN_POINT('',(3.16923525184393,-53.6795364022255,-0.9));
#83130=CARTESIAN_POINT('Origin',(3.16923525184393,-53.2597545981407,-0.6));
#83131=CARTESIAN_POINT('',(3.16923525184393,-53.1298772990704,-0.6));
#83132=CARTESIAN_POINT('',(3.16923525184393,-53.2597545981407,-0.9));
#83133=CARTESIAN_POINT('Origin',(2.52796676009893,-53.4696455001831,-0.9));
#83134=CARTESIAN_POINT('Ctrl Pts',(7.81467344611883,-54.7579811215401,-0.6));
#83135=CARTESIAN_POINT('Ctrl Pts',(7.81467344611883,-54.7579811215401,-0.9));
#83136=CARTESIAN_POINT('Ctrl Pts',(7.33458425849676,-54.7579811215401,-0.6));
#83137=CARTESIAN_POINT('Ctrl Pts',(7.33458425849676,-54.7579811215401,-0.9));
#83138=CARTESIAN_POINT('Ctrl Pts',(6.95654775947332,-54.5260576605797,-0.6));
#83139=CARTESIAN_POINT('Ctrl Pts',(6.95654775947332,-54.5260576605797,-0.9));
#83140=CARTESIAN_POINT('',(7.81467344611883,-54.7579811215401,-0.6));
#83141=CARTESIAN_POINT('',(6.95654775947332,-54.5260576605797,-0.6));
#83142=CARTESIAN_POINT('Ctrl Pts',(7.81467344611883,-54.7579811215401,-0.6));
#83143=CARTESIAN_POINT('Ctrl Pts',(7.33458425849676,-54.7579811215401,-0.6));
#83144=CARTESIAN_POINT('Ctrl Pts',(6.95654775947332,-54.5260576605797,-0.6));
#83145=CARTESIAN_POINT('',(7.81467344611883,-54.7579811215401,-0.9));
#83146=CARTESIAN_POINT('',(7.81467344611883,-54.7579811215401,-0.6));
#83147=CARTESIAN_POINT('',(6.95654775947332,-54.5260576605797,-0.9));
#83148=CARTESIAN_POINT('Ctrl Pts',(7.81467344611883,-54.7579811215401,-0.9));
#83149=CARTESIAN_POINT('Ctrl Pts',(7.33458425849676,-54.7579811215401,-0.9));
#83150=CARTESIAN_POINT('Ctrl Pts',(6.95654775947332,-54.5260576605797,-0.9));
#83151=CARTESIAN_POINT('',(6.95654775947332,-54.5260576605797,-0.6));
#83152=CARTESIAN_POINT('Ctrl Pts',(8.64031698554754,-54.5480899214745,-0.6));
#83153=CARTESIAN_POINT('Ctrl Pts',(8.64031698554754,-54.5480899214745,-0.9));
#83154=CARTESIAN_POINT('Ctrl Pts',(8.25764562934637,-54.7579811215401,-0.6));
#83155=CARTESIAN_POINT('Ctrl Pts',(8.25764562934637,-54.7579811215401,-0.9));
#83156=CARTESIAN_POINT('Ctrl Pts',(7.81467344611883,-54.7579811215401,-0.6));
#83157=CARTESIAN_POINT('Ctrl Pts',(7.81467344611883,-54.7579811215401,-0.9));
#83158=CARTESIAN_POINT('',(8.64031698554754,-54.5480899214745,-0.6));
#83159=CARTESIAN_POINT('Ctrl Pts',(8.64031698554754,-54.5480899214745,-0.6));
#83160=CARTESIAN_POINT('Ctrl Pts',(8.25764562934637,-54.7579811215401,-0.6));
#83161=CARTESIAN_POINT('Ctrl Pts',(7.81467344611883,-54.7579811215401,-0.6));
#83162=CARTESIAN_POINT('',(8.64031698554754,-54.5480899214745,-0.9));
#83163=CARTESIAN_POINT('',(8.64031698554754,-54.5480899214745,-0.6));
#83164=CARTESIAN_POINT('Ctrl Pts',(8.64031698554754,-54.5480899214745,-0.9));
#83165=CARTESIAN_POINT('Ctrl Pts',(8.25764562934637,-54.7579811215401,-0.9));
#83166=CARTESIAN_POINT('Ctrl Pts',(7.81467344611883,-54.7579811215401,-0.9));
#83167=CARTESIAN_POINT('Ctrl Pts',(9.23171903938055,-53.9300135970116,-0.6));
#83168=CARTESIAN_POINT('Ctrl Pts',(9.23171903938055,-53.9300135970116,-0.9));
#83169=CARTESIAN_POINT('Ctrl Pts',(9.02298834174871,-54.3381993174553,-0.6));
#83170=CARTESIAN_POINT('Ctrl Pts',(9.02298834174871,-54.3381993174553,-0.9));
#83171=CARTESIAN_POINT('Ctrl Pts',(8.64031698554754,-54.5480899214745,-0.6));
#83172=CARTESIAN_POINT('Ctrl Pts',(8.64031698554754,-54.5480899214745,-0.9));
#83173=CARTESIAN_POINT('',(9.23171903938055,-53.9300135970116,-0.6));
#83174=CARTESIAN_POINT('Ctrl Pts',(9.23171903938055,-53.9300135970116,-0.6));
#83175=CARTESIAN_POINT('Ctrl Pts',(9.02298834174871,-54.3381993174553,-0.6));
#83176=CARTESIAN_POINT('Ctrl Pts',(8.64031698554754,-54.5480899214745,-0.6));
#83177=CARTESIAN_POINT('',(9.23171903938055,-53.9300135970116,-0.9));
#83178=CARTESIAN_POINT('',(9.23171903938055,-53.9300135970116,-0.6));
#83179=CARTESIAN_POINT('Ctrl Pts',(9.23171903938055,-53.9300135970116,-0.9));
#83180=CARTESIAN_POINT('Ctrl Pts',(9.02298834174871,-54.3381993174553,-0.9));
#83181=CARTESIAN_POINT('Ctrl Pts',(8.64031698554754,-54.5480899214745,-0.9));
#83182=CARTESIAN_POINT('Ctrl Pts',(9.44044973701239,-53.0046383738518,-0.6));
#83183=CARTESIAN_POINT('Ctrl Pts',(9.44044973701239,-53.0046383738518,-0.9));
#83184=CARTESIAN_POINT('Ctrl Pts',(9.44044973701239,-53.5218278765678,-0.6));
#83185=CARTESIAN_POINT('Ctrl Pts',(9.44044973701239,-53.5218278765678,-0.9));
#83186=CARTESIAN_POINT('Ctrl Pts',(9.23171903938055,-53.9300135970116,-0.6));
#83187=CARTESIAN_POINT('Ctrl Pts',(9.23171903938055,-53.9300135970116,-0.9));
#83188=CARTESIAN_POINT('',(9.44044973701239,-53.0046383738518,-0.6));
#83189=CARTESIAN_POINT('Ctrl Pts',(9.44044973701239,-53.0046383738518,-0.6));
#83190=CARTESIAN_POINT('Ctrl Pts',(9.44044973701239,-53.5218278765678,-0.6));
#83191=CARTESIAN_POINT('Ctrl Pts',(9.23171903938055,-53.9300135970116,-0.6));
#83192=CARTESIAN_POINT('',(9.44044973701239,-53.0046383738518,-0.9));
#83193=CARTESIAN_POINT('',(9.44044973701239,-53.0046383738518,-0.6));
#83194=CARTESIAN_POINT('Ctrl Pts',(9.44044973701239,-53.0046383738518,-0.9));
#83195=CARTESIAN_POINT('Ctrl Pts',(9.44044973701239,-53.5218278765678,-0.9));
#83196=CARTESIAN_POINT('Ctrl Pts',(9.23171903938055,-53.9300135970116,-0.9));
#83197=CARTESIAN_POINT('Ctrl Pts',(9.2421617731452,-52.0920191407204,-0.6));
#83198=CARTESIAN_POINT('Ctrl Pts',(9.2421617731452,-52.0920191407204,-0.9));
#83199=CARTESIAN_POINT('Ctrl Pts',(9.44044973701239,-52.4944065213203,-0.6));
#83200=CARTESIAN_POINT('Ctrl Pts',(9.44044973701239,-52.4944065213203,-0.9));
#83201=CARTESIAN_POINT('Ctrl Pts',(9.44044973701239,-53.0046383738518,-0.6));
#83202=CARTESIAN_POINT('Ctrl Pts',(9.44044973701239,-53.0046383738518,-0.9));
#83203=CARTESIAN_POINT('',(9.2421617731452,-52.0920191407204,-0.6));
#83204=CARTESIAN_POINT('Ctrl Pts',(9.2421617731452,-52.0920191407204,-0.6));
#83205=CARTESIAN_POINT('Ctrl Pts',(9.44044973701239,-52.4944065213203,-0.6));
#83206=CARTESIAN_POINT('Ctrl Pts',(9.44044973701239,-53.0046383738518,-0.6));
#83207=CARTESIAN_POINT('',(9.2421617731452,-52.0920191407204,-0.9));
#83208=CARTESIAN_POINT('',(9.2421617731452,-52.0920191407204,-0.6));
#83209=CARTESIAN_POINT('Ctrl Pts',(9.2421617731452,-52.0920191407204,-0.9));
#83210=CARTESIAN_POINT('Ctrl Pts',(9.44044973701239,-52.4944065213203,-0.9));
#83211=CARTESIAN_POINT('Ctrl Pts',(9.44044973701239,-53.0046383738518,-0.9));
#83212=CARTESIAN_POINT('Ctrl Pts',(8.66582777351141,-51.4646653532982,-0.6));
#83213=CARTESIAN_POINT('Ctrl Pts',(8.66582777351141,-51.4646653532982,-0.9));
#83214=CARTESIAN_POINT('Ctrl Pts',(9.04386427253485,-51.6896311640739,-0.6));
#83215=CARTESIAN_POINT('Ctrl Pts',(9.04386427253485,-51.6896311640739,-0.9));
#83216=CARTESIAN_POINT('Ctrl Pts',(9.2421617731452,-52.0920191407204,-0.6));
#83217=CARTESIAN_POINT('Ctrl Pts',(9.2421617731452,-52.0920191407204,-0.9));
#83218=CARTESIAN_POINT('',(8.66582777351141,-51.4646653532982,-0.6));
#83219=CARTESIAN_POINT('Ctrl Pts',(8.66582777351141,-51.4646653532982,-0.6));
#83220=CARTESIAN_POINT('Ctrl Pts',(9.04386427253485,-51.6896311640739,-0.6));
#83221=CARTESIAN_POINT('Ctrl Pts',(9.2421617731452,-52.0920191407204,-0.6));
#83222=CARTESIAN_POINT('',(8.66582777351141,-51.4646653532982,-0.9));
#83223=CARTESIAN_POINT('',(8.66582777351141,-51.4646653532982,-0.6));
#83224=CARTESIAN_POINT('Ctrl Pts',(8.66582777351141,-51.4646653532982,-0.9));
#83225=CARTESIAN_POINT('Ctrl Pts',(9.04386427253485,-51.6896311640739,-0.9));
#83226=CARTESIAN_POINT('Ctrl Pts',(9.2421617731452,-52.0920191407204,-0.9));
#83227=CARTESIAN_POINT('Ctrl Pts',(7.8169908747077,-51.2396995425224,-0.6));
#83228=CARTESIAN_POINT('Ctrl Pts',(7.8169908747077,-51.2396995425224,-0.9));
#83229=CARTESIAN_POINT('Ctrl Pts',(8.28779127448797,-51.2396995425224,-0.6));
#83230=CARTESIAN_POINT('Ctrl Pts',(8.28779127448797,-51.2396995425224,-0.9));
#83231=CARTESIAN_POINT('Ctrl Pts',(8.66582777351141,-51.4646653532982,-0.6));
#83232=CARTESIAN_POINT('Ctrl Pts',(8.66582777351141,-51.4646653532982,-0.9));
#83233=CARTESIAN_POINT('',(7.8169908747077,-51.2396995425224,-0.6));
#83234=CARTESIAN_POINT('Ctrl Pts',(7.8169908747077,-51.2396995425224,-0.6));
#83235=CARTESIAN_POINT('Ctrl Pts',(8.28779127448797,-51.2396995425224,-0.6));
#83236=CARTESIAN_POINT('Ctrl Pts',(8.66582777351141,-51.4646653532982,-0.6));
#83237=CARTESIAN_POINT('',(7.8169908747077,-51.2396995425224,-0.9));
#83238=CARTESIAN_POINT('',(7.8169908747077,-51.2396995425224,-0.6));
#83239=CARTESIAN_POINT('Ctrl Pts',(7.8169908747077,-51.2396995425224,-0.9));
#83240=CARTESIAN_POINT('Ctrl Pts',(8.28779127448797,-51.2396995425224,-0.9));
#83241=CARTESIAN_POINT('Ctrl Pts',(8.66582777351141,-51.4646653532982,-0.9));
#83242=CARTESIAN_POINT('Ctrl Pts',(6.64345648139715,-51.7186216711998,-0.6));
#83243=CARTESIAN_POINT('Ctrl Pts',(6.64345648139715,-51.7186216711998,-0.9));
#83244=CARTESIAN_POINT('Ctrl Pts',(7.09802534431219,-51.2396995425224,-0.6));
#83245=CARTESIAN_POINT('Ctrl Pts',(7.09802534431219,-51.2396995425224,-0.9));
#83246=CARTESIAN_POINT('Ctrl Pts',(7.8169908747077,-51.2396995425224,-0.6));
#83247=CARTESIAN_POINT('Ctrl Pts',(7.8169908747077,-51.2396995425224,-0.9));
#83248=CARTESIAN_POINT('',(6.64345648139715,-51.7186216711998,-0.6));
#83249=CARTESIAN_POINT('Ctrl Pts',(6.64345648139715,-51.7186216711998,-0.6));
#83250=CARTESIAN_POINT('Ctrl Pts',(7.09802534431219,-51.2396995425224,-0.6));
#83251=CARTESIAN_POINT('Ctrl Pts',(7.8169908747077,-51.2396995425224,-0.6));
#83252=CARTESIAN_POINT('',(6.64345648139715,-51.7186216711998,-0.9));
#83253=CARTESIAN_POINT('',(6.64345648139715,-51.7186216711998,-0.6));
#83254=CARTESIAN_POINT('Ctrl Pts',(6.64345648139715,-51.7186216711998,-0.9));
#83255=CARTESIAN_POINT('Ctrl Pts',(7.09802534431219,-51.2396995425224,-0.9));
#83256=CARTESIAN_POINT('Ctrl Pts',(7.8169908747077,-51.2396995425224,-0.9));
#83257=CARTESIAN_POINT('Ctrl Pts',(6.18888761848211,-53.0440656542778,-0.6));
#83258=CARTESIAN_POINT('Ctrl Pts',(6.18888761848211,-53.0440656542778,-0.9));
#83259=CARTESIAN_POINT('Ctrl Pts',(6.18888761848211,-52.1975443959236,-0.6));
#83260=CARTESIAN_POINT('Ctrl Pts',(6.18888761848211,-52.1975443959236,-0.9));
#83261=CARTESIAN_POINT('Ctrl Pts',(6.64345648139715,-51.7186216711998,-0.6));
#83262=CARTESIAN_POINT('Ctrl Pts',(6.64345648139715,-51.7186216711998,-0.9));
#83263=CARTESIAN_POINT('',(6.18888761848211,-53.0440656542778,-0.6));
#83264=CARTESIAN_POINT('Ctrl Pts',(6.18888761848211,-53.0440656542778,-0.6));
#83265=CARTESIAN_POINT('Ctrl Pts',(6.18888761848211,-52.1975443959236,-0.6));
#83266=CARTESIAN_POINT('Ctrl Pts',(6.64345648139715,-51.7186216711998,-0.6));
#83267=CARTESIAN_POINT('',(6.18888761848211,-53.0440656542778,-0.9));
#83268=CARTESIAN_POINT('',(6.18888761848211,-53.0440656542778,-0.6));
#83269=CARTESIAN_POINT('Ctrl Pts',(6.18888761848211,-53.0440656542778,-0.9));
#83270=CARTESIAN_POINT('Ctrl Pts',(6.18888761848211,-52.1975443959236,-0.9));
#83271=CARTESIAN_POINT('Ctrl Pts',(6.64345648139715,-51.7186216711998,-0.9));
#83272=CARTESIAN_POINT('Ctrl Pts',(6.38370420783758,-53.8929061293602,-0.6));
#83273=CARTESIAN_POINT('Ctrl Pts',(6.38370420783758,-53.8929061293602,-0.9));
#83274=CARTESIAN_POINT('Ctrl Pts',(6.18888761848211,-53.4916780591011,-0.6));
#83275=CARTESIAN_POINT('Ctrl Pts',(6.18888761848211,-53.4916780591011,-0.9));
#83276=CARTESIAN_POINT('Ctrl Pts',(6.18888761848211,-53.0440656542778,-0.6));
#83277=CARTESIAN_POINT('Ctrl Pts',(6.18888761848211,-53.0440656542778,-0.9));
#83278=CARTESIAN_POINT('',(6.38370420783758,-53.8929061293602,-0.6));
#83279=CARTESIAN_POINT('Ctrl Pts',(6.38370420783758,-53.8929061293602,-0.6));
#83280=CARTESIAN_POINT('Ctrl Pts',(6.18888761848211,-53.4916780591011,-0.6));
#83281=CARTESIAN_POINT('Ctrl Pts',(6.18888761848211,-53.0440656542778,-0.6));
#83282=CARTESIAN_POINT('',(6.38370420783758,-53.8929061293602,-0.9));
#83283=CARTESIAN_POINT('',(6.38370420783758,-53.8929061293602,-0.6));
#83284=CARTESIAN_POINT('Ctrl Pts',(6.38370420783758,-53.8929061293602,-0.9));
#83285=CARTESIAN_POINT('Ctrl Pts',(6.18888761848211,-53.4916780591011,-0.9));
#83286=CARTESIAN_POINT('Ctrl Pts',(6.18888761848211,-53.0440656542778,-0.9));
#83287=CARTESIAN_POINT('Ctrl Pts',(6.95654775947332,-54.5260576605797,-0.6));
#83288=CARTESIAN_POINT('Ctrl Pts',(6.95654775947332,-54.5260576605797,-0.9));
#83289=CARTESIAN_POINT('Ctrl Pts',(6.57852079719305,-54.2941336035728,-0.6));
#83290=CARTESIAN_POINT('Ctrl Pts',(6.57852079719305,-54.2941336035728,-0.9));
#83291=CARTESIAN_POINT('Ctrl Pts',(6.38370420783758,-53.8929061293602,-0.6));
#83292=CARTESIAN_POINT('Ctrl Pts',(6.38370420783758,-53.8929061293602,-0.9));
#83293=CARTESIAN_POINT('Ctrl Pts',(6.95654775947332,-54.5260576605797,-0.6));
#83294=CARTESIAN_POINT('Ctrl Pts',(6.57852079719305,-54.2941336035728,-0.6));
#83295=CARTESIAN_POINT('Ctrl Pts',(6.38370420783758,-53.8929061293602,-0.6));
#83296=CARTESIAN_POINT('Ctrl Pts',(6.95654775947332,-54.5260576605797,-0.9));
#83297=CARTESIAN_POINT('Ctrl Pts',(6.57852079719305,-54.2941336035728,-0.9));
#83298=CARTESIAN_POINT('Ctrl Pts',(6.38370420783758,-53.8929061293602,-0.9));
#83299=CARTESIAN_POINT('Origin',(7.81466867774725,-52.9988403320313,-0.9));
#83300=CARTESIAN_POINT('Origin',(14.4384088739753,-52.9791269898415,-0.6));
#83301=CARTESIAN_POINT('',(14.4384088739753,-52.9791269898415,-0.6));
#83302=CARTESIAN_POINT('',(13.8817873224616,-53.5218278765678,-0.6));
#83303=CARTESIAN_POINT('',(10.7321883094972,-56.5926579091458,-0.6));
#83304=CARTESIAN_POINT('',(14.4384088739753,-52.9791269898415,-0.9));
#83305=CARTESIAN_POINT('',(14.4384088739753,-52.9791269898415,-0.6));
#83306=CARTESIAN_POINT('',(13.8817873224616,-53.5218278765678,-0.9));
#83307=CARTESIAN_POINT('',(14.4384088739753,-52.9791269898415,-0.9));
#83308=CARTESIAN_POINT('',(13.8817873224616,-53.5218278765678,-0.6));
#83309=CARTESIAN_POINT('Origin',(15.649041198194,-54.7000001072884,-0.6));
#83310=CARTESIAN_POINT('',(15.649041198194,-54.7000001072884,-0.6));
#83311=CARTESIAN_POINT('',(12.6586197719514,-50.4492166618859,-0.6));
#83312=CARTESIAN_POINT('',(15.649041198194,-54.7000001072884,-0.9));
#83313=CARTESIAN_POINT('',(15.649041198194,-54.7000001072884,-0.6));
#83314=CARTESIAN_POINT('',(15.649041198194,-54.7000001072884,-0.9));
#83315=CARTESIAN_POINT('Origin',(16.2427702173591,-54.7000001072884,-0.6));
#83316=CARTESIAN_POINT('',(16.2427702173591,-54.7000001072884,-0.6));
#83317=CARTESIAN_POINT('',(8.12138510867953,-54.7000001072884,-0.6));
#83318=CARTESIAN_POINT('',(16.2427702173591,-54.7000001072884,-0.9));
#83319=CARTESIAN_POINT('',(16.2427702173591,-54.7000001072884,-0.6));
#83320=CARTESIAN_POINT('',(16.2427702173591,-54.7000001072884,-0.9));
#83321=CARTESIAN_POINT('Origin',(14.7538175806403,-52.6776264309883,-0.6));
#83322=CARTESIAN_POINT('',(14.7538175806403,-52.6776264309883,-0.6));
#83323=CARTESIAN_POINT('',(12.2377001613175,-49.2601035965936,-0.6));
#83324=CARTESIAN_POINT('',(14.7538175806403,-52.6776264309883,-0.9));
#83325=CARTESIAN_POINT('',(14.7538175806403,-52.6776264309883,-0.6));
#83326=CARTESIAN_POINT('',(14.7538175806403,-52.6776264309883,-0.9));
#83327=CARTESIAN_POINT('Origin',(16.1801519617438,-51.3000003695488,-0.6));
#83328=CARTESIAN_POINT('',(16.1801519617438,-51.3000003695488,-0.6));
#83329=CARTESIAN_POINT('',(11.569878082483,-55.7528366263105,-0.6));
#83330=CARTESIAN_POINT('',(16.1801519617438,-51.3000003695488,-0.9));
#83331=CARTESIAN_POINT('',(16.1801519617438,-51.3000003695488,-0.6));
#83332=CARTESIAN_POINT('',(16.1801519617438,-51.3000003695488,-0.9));
#83333=CARTESIAN_POINT('Origin',(15.5701914057136,-51.3000003695488,-0.6));
#83334=CARTESIAN_POINT('',(15.5701914057136,-51.3000003695488,-0.6));
#83335=CARTESIAN_POINT('',(7.78509570285678,-51.3000003695488,-0.6));
#83336=CARTESIAN_POINT('',(15.5701914057136,-51.3000003695488,-0.9));
#83337=CARTESIAN_POINT('',(15.5701914057136,-51.3000003695488,-0.6));
#83338=CARTESIAN_POINT('',(15.5701914057136,-51.3000003695488,-0.9));
#83339=CARTESIAN_POINT('Origin',(13.8817873224616,-52.9860846400261,-0.6));
#83340=CARTESIAN_POINT('',(13.8817873224616,-52.9860846400261,-0.6));
#83341=CARTESIAN_POINT('',(10.4030900973563,-56.4600022473006,-0.6));
#83342=CARTESIAN_POINT('',(13.8817873224616,-52.9860846400261,-0.9));
#83343=CARTESIAN_POINT('',(13.8817873224616,-52.9860846400261,-0.6));
#83344=CARTESIAN_POINT('',(13.8817873224616,-52.9860846400261,-0.9));
#83345=CARTESIAN_POINT('Origin',(13.8817873224616,-51.3000003695488,-0.6));
#83346=CARTESIAN_POINT('',(13.8817873224616,-51.3000003695488,-0.6));
#83347=CARTESIAN_POINT('',(13.8817873224616,-52.1500001847744,-0.6));
#83348=CARTESIAN_POINT('',(13.8817873224616,-51.3000003695488,-0.9));
#83349=CARTESIAN_POINT('',(13.8817873224616,-51.3000003695488,-0.6));
#83350=CARTESIAN_POINT('',(13.8817873224616,-51.3000003695488,-0.9));
#83351=CARTESIAN_POINT('Origin',(13.4318533167243,-51.3000003695488,-0.6));
#83352=CARTESIAN_POINT('',(13.4318533167243,-51.3000003695488,-0.6));
#83353=CARTESIAN_POINT('',(6.71592665836215,-51.3000003695488,-0.6));
#83354=CARTESIAN_POINT('',(13.4318533167243,-51.3000003695488,-0.9));
#83355=CARTESIAN_POINT('',(13.4318533167243,-51.3000003695488,-0.6));
#83356=CARTESIAN_POINT('',(13.4318533167243,-51.3000003695488,-0.9));
#83357=CARTESIAN_POINT('Origin',(13.4318533167243,-54.7000001072884,-0.6));
#83358=CARTESIAN_POINT('',(13.4318533167243,-54.7000001072884,-0.6));
#83359=CARTESIAN_POINT('',(13.4318533167243,-53.8500000536442,-0.6));
#83360=CARTESIAN_POINT('',(13.4318533167243,-54.7000001072884,-0.9));
#83361=CARTESIAN_POINT('',(13.4318533167243,-54.7000001072884,-0.6));
#83362=CARTESIAN_POINT('',(13.4318533167243,-54.7000001072884,-0.9));
#83363=CARTESIAN_POINT('Origin',(13.8817873224616,-54.7000001072884,-0.6));
#83364=CARTESIAN_POINT('',(13.8817873224616,-54.7000001072884,-0.6));
#83365=CARTESIAN_POINT('',(6.9408936612308,-54.7000001072884,-0.6));
#83366=CARTESIAN_POINT('',(13.8817873224616,-54.7000001072884,-0.9));
#83367=CARTESIAN_POINT('',(13.8817873224616,-54.7000001072884,-0.6));
#83368=CARTESIAN_POINT('',(13.8817873224616,-54.7000001072884,-0.9));
#83369=CARTESIAN_POINT('Origin',(13.8817873224616,-53.5218278765678,-0.6));
#83370=CARTESIAN_POINT('',(13.8817873224616,-53.2609139382839,-0.6));
#83371=CARTESIAN_POINT('',(13.8817873224616,-53.5218278765678,-0.9));
#83372=CARTESIAN_POINT('Origin',(14.8373117670417,-53.0000002384186,-0.9));
#83373=CARTESIAN_POINT('Origin',(21.5375890955329,-54.2987720370293,-0.6));
#83374=CARTESIAN_POINT('',(21.5375890955329,-54.2987720370293,-0.6));
#83375=CARTESIAN_POINT('',(23.2120695337653,-54.2987720370293,-0.6));
#83376=CARTESIAN_POINT('',(10.7687945477664,-54.2987720370293,-0.6));
#83377=CARTESIAN_POINT('',(21.5375890955329,-54.2987720370293,-0.9));
#83378=CARTESIAN_POINT('',(21.5375890955329,-54.2987720370293,-0.6));
#83379=CARTESIAN_POINT('',(23.2120695337653,-54.2987720370293,-0.9));
#83380=CARTESIAN_POINT('',(21.5375890955329,-54.2987720370293,-0.9));
#83381=CARTESIAN_POINT('',(23.2120695337653,-54.2987720370293,-0.6));
#83382=CARTESIAN_POINT('Origin',(21.5375890955329,-51.3000003695488,-0.6));
#83383=CARTESIAN_POINT('',(21.5375890955329,-51.3000003695488,-0.6));
#83384=CARTESIAN_POINT('',(21.5375890955329,-52.1500001847744,-0.6));
#83385=CARTESIAN_POINT('',(21.5375890955329,-51.3000003695488,-0.9));
#83386=CARTESIAN_POINT('',(21.5375890955329,-51.3000003695488,-0.6));
#83387=CARTESIAN_POINT('',(21.5375890955329,-51.3000003695488,-0.9));
#83388=CARTESIAN_POINT('Origin',(21.0876550897956,-51.3000003695488,-0.6));
#83389=CARTESIAN_POINT('',(21.0876550897956,-51.3000003695488,-0.6));
#83390=CARTESIAN_POINT('',(10.5438275448978,-51.3000003695488,-0.6));
#83391=CARTESIAN_POINT('',(21.0876550897956,-51.3000003695488,-0.9));
#83392=CARTESIAN_POINT('',(21.0876550897956,-51.3000003695488,-0.6));
#83393=CARTESIAN_POINT('',(21.0876550897956,-51.3000003695488,-0.9));
#83394=CARTESIAN_POINT('Origin',(21.0876550897956,-54.7000001072884,-0.6));
#83395=CARTESIAN_POINT('',(21.0876550897956,-54.7000001072884,-0.6));
#83396=CARTESIAN_POINT('',(21.0876550897956,-53.8500000536442,-0.6));
#83397=CARTESIAN_POINT('',(21.0876550897956,-54.7000001072884,-0.9));
#83398=CARTESIAN_POINT('',(21.0876550897956,-54.7000001072884,-0.6));
#83399=CARTESIAN_POINT('',(21.0876550897956,-54.7000001072884,-0.9));
#83400=CARTESIAN_POINT('Origin',(23.2120695337653,-54.7000001072884,-0.6));
#83401=CARTESIAN_POINT('',(23.2120695337653,-54.7000001072884,-0.6));
#83402=CARTESIAN_POINT('',(11.6060347668827,-54.7000001072884,-0.6));
#83403=CARTESIAN_POINT('',(23.2120695337653,-54.7000001072884,-0.9));
#83404=CARTESIAN_POINT('',(23.2120695337653,-54.7000001072884,-0.6));
#83405=CARTESIAN_POINT('',(23.2120695337653,-54.7000001072884,-0.9));
#83406=CARTESIAN_POINT('Origin',(23.2120695337653,-54.2987720370293,-0.6));
#83407=CARTESIAN_POINT('',(23.2120695337653,-53.6493860185146,-0.6));
#83408=CARTESIAN_POINT('',(23.2120695337653,-54.2987720370293,-0.9));
#83409=CARTESIAN_POINT('Origin',(22.1498623117805,-53.0000002384186,-0.9));
#83410=CARTESIAN_POINT('Ctrl Pts',(27.2463884577155,-54.4715551733971,-0.6));
#83411=CARTESIAN_POINT('Ctrl Pts',(27.2463884577155,-54.4715551733971,-0.9));
#83412=CARTESIAN_POINT('Ctrl Pts',(27.0782461389899,-54.5840380787849,-0.6));
#83413=CARTESIAN_POINT('Ctrl Pts',(27.0782461389899,-54.5840380787849,-0.9));
#83414=CARTESIAN_POINT('Ctrl Pts',(26.8405237421393,-54.6420190930367,-0.6));
#83415=CARTESIAN_POINT('Ctrl Pts',(26.8405237421393,-54.6420190930367,-0.9));
#83416=CARTESIAN_POINT('',(27.2463884577155,-54.4715551733971,-0.6));
#83417=CARTESIAN_POINT('',(26.8405237421393,-54.6420190930367,-0.6));
#83418=CARTESIAN_POINT('Ctrl Pts',(27.2463884577155,-54.4715551733971,-0.6));
#83419=CARTESIAN_POINT('Ctrl Pts',(27.0782461389899,-54.5840380787849,-0.6));
#83420=CARTESIAN_POINT('Ctrl Pts',(26.8405237421393,-54.6420190930367,-0.6));
#83421=CARTESIAN_POINT('',(27.2463884577155,-54.4715551733971,-0.9));
#83422=CARTESIAN_POINT('',(27.2463884577155,-54.4715551733971,-0.6));
#83423=CARTESIAN_POINT('',(26.8405237421393,-54.6420190930367,-0.9));
#83424=CARTESIAN_POINT('Ctrl Pts',(27.2463884577155,-54.4715551733971,-0.9));
#83425=CARTESIAN_POINT('Ctrl Pts',(27.0782461389899,-54.5840380787849,-0.9));
#83426=CARTESIAN_POINT('Ctrl Pts',(26.8405237421393,-54.6420190930367,-0.9));
#83427=CARTESIAN_POINT('',(26.8405237421393,-54.6420190930367,-0.6));
#83428=CARTESIAN_POINT('Ctrl Pts',(27.55600836128,-54.1630969643593,-0.6));
#83429=CARTESIAN_POINT('Ctrl Pts',(27.55600836128,-54.1630969643593,-0.9));
#83430=CARTESIAN_POINT('Ctrl Pts',(27.4145307764411,-54.3590722680092,-0.6));
#83431=CARTESIAN_POINT('Ctrl Pts',(27.4145307764411,-54.3590722680092,-0.9));
#83432=CARTESIAN_POINT('Ctrl Pts',(27.2463884577155,-54.4715551733971,-0.6));
#83433=CARTESIAN_POINT('Ctrl Pts',(27.2463884577155,-54.4715551733971,-0.9));
#83434=CARTESIAN_POINT('',(27.55600836128,-54.1630969643593,-0.6));
#83435=CARTESIAN_POINT('Ctrl Pts',(27.55600836128,-54.1630969643593,-0.6));
#83436=CARTESIAN_POINT('Ctrl Pts',(27.4145307764411,-54.3590722680092,-0.6));
#83437=CARTESIAN_POINT('Ctrl Pts',(27.2463884577155,-54.4715551733971,-0.6));
#83438=CARTESIAN_POINT('',(27.55600836128,-54.1630969643593,-0.9));
#83439=CARTESIAN_POINT('',(27.55600836128,-54.1630969643593,-0.6));
#83440=CARTESIAN_POINT('Ctrl Pts',(27.55600836128,-54.1630969643593,-0.9));
#83441=CARTESIAN_POINT('Ctrl Pts',(27.4145307764411,-54.3590722680092,-0.9));
#83442=CARTESIAN_POINT('Ctrl Pts',(27.2463884577155,-54.4715551733971,-0.9));
#83443=CARTESIAN_POINT('Ctrl Pts',(27.7879324182868,-53.6679403185844,-0.6));
#83444=CARTESIAN_POINT('Ctrl Pts',(27.7879324182868,-53.6679403185844,-0.9));
#83445=CARTESIAN_POINT('Ctrl Pts',(27.6974764093757,-53.9671216607094,-0.6));
#83446=CARTESIAN_POINT('Ctrl Pts',(27.6974764093757,-53.9671216607094,-0.9));
#83447=CARTESIAN_POINT('Ctrl Pts',(27.55600836128,-54.1630969643593,-0.6));
#83448=CARTESIAN_POINT('Ctrl Pts',(27.55600836128,-54.1630969643593,-0.9));
#83449=CARTESIAN_POINT('',(27.7879324182868,-53.6679403185844,-0.6));
#83450=CARTESIAN_POINT('Ctrl Pts',(27.7879324182868,-53.6679403185844,-0.6));
#83451=CARTESIAN_POINT('Ctrl Pts',(27.6974764093757,-53.9671216607094,-0.6));
#83452=CARTESIAN_POINT('Ctrl Pts',(27.55600836128,-54.1630969643593,-0.6));
#83453=CARTESIAN_POINT('',(27.7879324182868,-53.6679403185844,-0.9));
#83454=CARTESIAN_POINT('',(27.7879324182868,-53.6679403185844,-0.6));
#83455=CARTESIAN_POINT('Ctrl Pts',(27.7879324182868,-53.6679403185844,-0.9));
#83456=CARTESIAN_POINT('Ctrl Pts',(27.6974764093757,-53.9671216607094,-0.9));
#83457=CARTESIAN_POINT('Ctrl Pts',(27.55600836128,-54.1630969643593,-0.9));
#83458=CARTESIAN_POINT('Ctrl Pts',(27.8783788904548,-52.9814462065697,-0.6));
#83459=CARTESIAN_POINT('Ctrl Pts',(27.8783788904548,-52.9814462065697,-0.9));
#83460=CARTESIAN_POINT('Ctrl Pts',(27.8783788904548,-53.3687583804131,-0.6));
#83461=CARTESIAN_POINT('Ctrl Pts',(27.8783788904548,-53.3687583804131,-0.9));
#83462=CARTESIAN_POINT('Ctrl Pts',(27.7879324182868,-53.6679403185844,-0.6));
#83463=CARTESIAN_POINT('Ctrl Pts',(27.7879324182868,-53.6679403185844,-0.9));
#83464=CARTESIAN_POINT('',(27.8783788904548,-52.9814462065697,-0.6));
#83465=CARTESIAN_POINT('Ctrl Pts',(27.8783788904548,-52.9814462065697,-0.6));
#83466=CARTESIAN_POINT('Ctrl Pts',(27.8783788904548,-53.3687583804131,-0.6));
#83467=CARTESIAN_POINT('Ctrl Pts',(27.7879324182868,-53.6679403185844,-0.6));
#83468=CARTESIAN_POINT('',(27.8783788904548,-52.9814462065697,-0.9));
#83469=CARTESIAN_POINT('',(27.8783788904548,-52.9814462065697,-0.6));
#83470=CARTESIAN_POINT('Ctrl Pts',(27.8783788904548,-52.9814462065697,-0.9));
#83471=CARTESIAN_POINT('Ctrl Pts',(27.8783788904548,-53.3687583804131,-0.9));
#83472=CARTESIAN_POINT('Ctrl Pts',(27.7879324182868,-53.6679403185844,-0.9));
#83473=CARTESIAN_POINT('Ctrl Pts',(27.7450266107917,-52.1731923222542,-0.6));
#83474=CARTESIAN_POINT('Ctrl Pts',(27.7450266107917,-52.1731923222542,-0.9));
#83475=CARTESIAN_POINT('Ctrl Pts',(27.8783788904548,-52.5268761515617,-0.6));
#83476=CARTESIAN_POINT('Ctrl Pts',(27.8783788904548,-52.5268761515617,-0.9));
#83477=CARTESIAN_POINT('Ctrl Pts',(27.8783788904548,-52.9814462065697,-0.6));
#83478=CARTESIAN_POINT('Ctrl Pts',(27.8783788904548,-52.9814462065697,-0.9));
#83479=CARTESIAN_POINT('',(27.7450266107917,-52.1731923222542,-0.6));
#83480=CARTESIAN_POINT('Ctrl Pts',(27.7450266107917,-52.1731923222542,-0.6));
#83481=CARTESIAN_POINT('Ctrl Pts',(27.8783788904548,-52.5268761515617,-0.6));
#83482=CARTESIAN_POINT('Ctrl Pts',(27.8783788904548,-52.9814462065697,-0.6));
#83483=CARTESIAN_POINT('',(27.7450266107917,-52.1731923222542,-0.9));
#83484=CARTESIAN_POINT('',(27.7450266107917,-52.1731923222542,-0.6));
#83485=CARTESIAN_POINT('Ctrl Pts',(27.7450266107917,-52.1731923222542,-0.9));
#83486=CARTESIAN_POINT('Ctrl Pts',(27.8783788904548,-52.5268761515617,-0.9));
#83487=CARTESIAN_POINT('Ctrl Pts',(27.8783788904548,-52.9814462065697,-0.9));
#83488=CARTESIAN_POINT('Ctrl Pts',(27.3426332697272,-51.5922240614891,-0.6));
#83489=CARTESIAN_POINT('Ctrl Pts',(27.3426332697272,-51.5922240614891,-0.9));
#83490=CARTESIAN_POINT('Ctrl Pts',(27.6116647943854,-51.8195084929466,-0.6));
#83491=CARTESIAN_POINT('Ctrl Pts',(27.6116647943854,-51.8195084929466,-0.9));
#83492=CARTESIAN_POINT('Ctrl Pts',(27.7450266107917,-52.1731923222542,-0.6));
#83493=CARTESIAN_POINT('Ctrl Pts',(27.7450266107917,-52.1731923222542,-0.9));
#83494=CARTESIAN_POINT('',(27.3426332697272,-51.5922240614891,-0.6));
#83495=CARTESIAN_POINT('Ctrl Pts',(27.3426332697272,-51.5922240614891,-0.6));
#83496=CARTESIAN_POINT('Ctrl Pts',(27.6116647943854,-51.8195084929466,-0.6));
#83497=CARTESIAN_POINT('Ctrl Pts',(27.7450266107917,-52.1731923222542,-0.6));
#83498=CARTESIAN_POINT('',(27.3426332697272,-51.5922240614891,-0.9));
#83499=CARTESIAN_POINT('',(27.3426332697272,-51.5922240614891,-0.6));
#83500=CARTESIAN_POINT('Ctrl Pts',(27.3426332697272,-51.5922240614891,-0.9));
#83501=CARTESIAN_POINT('Ctrl Pts',(27.6116647943854,-51.8195084929466,-0.9));
#83502=CARTESIAN_POINT('Ctrl Pts',(27.7450266107917,-52.1731923222542,-0.9));
#83503=CARTESIAN_POINT('Ctrl Pts',(26.8439951166511,-51.3487039208412,-0.6));
#83504=CARTESIAN_POINT('Ctrl Pts',(26.8439951166511,-51.3487039208412,-0.9));
#83505=CARTESIAN_POINT('Ctrl Pts',(27.1362200006843,-51.4159618020058,-0.6));
#83506=CARTESIAN_POINT('Ctrl Pts',(27.1362200006843,-51.4159618020058,-0.9));
#83507=CARTESIAN_POINT('Ctrl Pts',(27.3426332697272,-51.5922240614891,-0.6));
#83508=CARTESIAN_POINT('Ctrl Pts',(27.3426332697272,-51.5922240614891,-0.9));
#83509=CARTESIAN_POINT('',(26.8439951166511,-51.3487039208412,-0.6));
#83510=CARTESIAN_POINT('Ctrl Pts',(26.8439951166511,-51.3487039208412,-0.6));
#83511=CARTESIAN_POINT('Ctrl Pts',(27.1362200006843,-51.4159618020058,-0.6));
#83512=CARTESIAN_POINT('Ctrl Pts',(27.3426332697272,-51.5922240614891,-0.6));
#83513=CARTESIAN_POINT('',(26.8439951166511,-51.3487039208412,-0.9));
#83514=CARTESIAN_POINT('',(26.8439951166511,-51.3487039208412,-0.6));
#83515=CARTESIAN_POINT('Ctrl Pts',(26.8439951166511,-51.3487039208412,-0.9));
#83516=CARTESIAN_POINT('Ctrl Pts',(27.1362200006843,-51.4159618020058,-0.9));
#83517=CARTESIAN_POINT('Ctrl Pts',(27.3426332697272,-51.5922240614891,-0.9));
#83518=CARTESIAN_POINT('Ctrl Pts',(26.2386789545417,-51.3000003695488,-0.6));
#83519=CARTESIAN_POINT('Ctrl Pts',(26.2386789545417,-51.3000003695488,-0.9));
#83520=CARTESIAN_POINT('Ctrl Pts',(26.6352644190192,-51.3000003695488,-0.6));
#83521=CARTESIAN_POINT('Ctrl Pts',(26.6352644190192,-51.3000003695488,-0.9));
#83522=CARTESIAN_POINT('Ctrl Pts',(26.8439951166511,-51.3487039208412,-0.6));
#83523=CARTESIAN_POINT('Ctrl Pts',(26.8439951166511,-51.3487039208412,-0.9));
#83524=CARTESIAN_POINT('',(26.2386789545417,-51.3000003695488,-0.6));
#83525=CARTESIAN_POINT('Ctrl Pts',(26.2386789545417,-51.3000003695488,-0.6));
#83526=CARTESIAN_POINT('Ctrl Pts',(26.6352644190192,-51.3000003695488,-0.6));
#83527=CARTESIAN_POINT('Ctrl Pts',(26.8439951166511,-51.3487039208412,-0.6));
#83528=CARTESIAN_POINT('',(26.2386789545417,-51.3000003695488,-0.9));
#83529=CARTESIAN_POINT('',(26.2386789545417,-51.3000003695488,-0.6));
#83530=CARTESIAN_POINT('Ctrl Pts',(26.2386789545417,-51.3000003695488,-0.9));
#83531=CARTESIAN_POINT('Ctrl Pts',(26.6352644190192,-51.3000003695488,-0.9));
#83532=CARTESIAN_POINT('Ctrl Pts',(26.8439951166511,-51.3487039208412,-0.9));
#83533=CARTESIAN_POINT('Origin',(25.06746198982,-51.3000003695488,-0.6));
#83534=CARTESIAN_POINT('',(25.06746198982,-51.3000003695488,-0.6));
#83535=CARTESIAN_POINT('',(12.53373099491,-51.3000003695488,-0.6));
#83536=CARTESIAN_POINT('',(25.06746198982,-51.3000003695488,-0.9));
#83537=CARTESIAN_POINT('',(25.06746198982,-51.3000003695488,-0.6));
#83538=CARTESIAN_POINT('',(25.06746198982,-51.3000003695488,-0.9));
#83539=CARTESIAN_POINT('Origin',(25.06746198982,-54.7000001072884,-0.6));
#83540=CARTESIAN_POINT('',(25.06746198982,-54.7000001072884,-0.6));
#83541=CARTESIAN_POINT('',(25.06746198982,-53.8500000536442,-0.6));
#83542=CARTESIAN_POINT('',(25.06746198982,-54.7000001072884,-0.9));
#83543=CARTESIAN_POINT('',(25.06746198982,-54.7000001072884,-0.6));
#83544=CARTESIAN_POINT('',(25.06746198982,-54.7000001072884,-0.9));
#83545=CARTESIAN_POINT('Origin',(26.2943449243903,-54.7000001072884,-0.6));
#83546=CARTESIAN_POINT('',(26.2943449243903,-54.7000001072884,-0.6));
#83547=CARTESIAN_POINT('',(13.1471724621952,-54.7000001072884,-0.6));
#83548=CARTESIAN_POINT('',(26.2943449243903,-54.7000001072884,-0.9));
#83549=CARTESIAN_POINT('',(26.2943449243903,-54.7000001072884,-0.6));
#83550=CARTESIAN_POINT('',(26.2943449243903,-54.7000001072884,-0.9));
#83551=CARTESIAN_POINT('Ctrl Pts',(26.8405237421393,-54.6420190930367,-0.6));
#83552=CARTESIAN_POINT('Ctrl Pts',(26.8405237421393,-54.6420190930367,-0.9));
#83553=CARTESIAN_POINT('Ctrl Pts',(26.6028013452888,-54.7000001072884,-0.6));
#83554=CARTESIAN_POINT('Ctrl Pts',(26.6028013452888,-54.7000001072884,-0.9));
#83555=CARTESIAN_POINT('Ctrl Pts',(26.2943449243903,-54.7000001072884,-0.6));
#83556=CARTESIAN_POINT('Ctrl Pts',(26.2943449243903,-54.7000001072884,-0.9));
#83557=CARTESIAN_POINT('Ctrl Pts',(26.8405237421393,-54.6420190930367,-0.6));
#83558=CARTESIAN_POINT('Ctrl Pts',(26.6028013452888,-54.7000001072884,-0.6));
#83559=CARTESIAN_POINT('Ctrl Pts',(26.2943449243903,-54.7000001072884,-0.6));
#83560=CARTESIAN_POINT('Ctrl Pts',(26.8405237421393,-54.6420190930367,-0.9));
#83561=CARTESIAN_POINT('Ctrl Pts',(26.6028013452888,-54.7000001072884,-0.9));
#83562=CARTESIAN_POINT('Ctrl Pts',(26.2943449243903,-54.7000001072884,-0.9));
#83563=CARTESIAN_POINT('Origin',(26.4729204401374,-53.0000002384186,-0.9));
#83564=CARTESIAN_POINT('Origin',(32.6444044336677,-53.190177500248,-0.6));
#83565=CARTESIAN_POINT('',(32.6444044336677,-53.190177500248,-0.6));
#83566=CARTESIAN_POINT('',(32.1225824579597,-53.190177500248,-0.6));
#83567=CARTESIAN_POINT('',(16.3222022168338,-53.190177500248,-0.6));
#83568=CARTESIAN_POINT('',(32.6444044336677,-53.190177500248,-0.9));
#83569=CARTESIAN_POINT('',(32.6444044336677,-53.190177500248,-0.6));
#83570=CARTESIAN_POINT('',(32.1225824579597,-53.190177500248,-0.9));
#83571=CARTESIAN_POINT('',(32.6444044336677,-53.190177500248,-0.9));
#83572=CARTESIAN_POINT('',(32.1225824579597,-53.190177500248,-0.6));
#83573=CARTESIAN_POINT('Ctrl Pts',(32.8948869928718,-53.2064120173454,-0.6));
#83574=CARTESIAN_POINT('Ctrl Pts',(32.8948869928718,-53.2064120173454,-0.9));
#83575=CARTESIAN_POINT('Ctrl Pts',(32.818345092237,-53.190177500248,-0.6));
#83576=CARTESIAN_POINT('Ctrl Pts',(32.818345092237,-53.190177500248,-0.9));
#83577=CARTESIAN_POINT('Ctrl Pts',(32.6444044336677,-53.190177500248,-0.6));
#83578=CARTESIAN_POINT('Ctrl Pts',(32.6444044336677,-53.190177500248,-0.9));
#83579=CARTESIAN_POINT('',(32.8948869928718,-53.2064120173454,-0.6));
#83580=CARTESIAN_POINT('Ctrl Pts',(32.8948869928718,-53.2064120173454,-0.6));
#83581=CARTESIAN_POINT('Ctrl Pts',(32.818345092237,-53.190177500248,-0.6));
#83582=CARTESIAN_POINT('Ctrl Pts',(32.6444044336677,-53.190177500248,-0.6));
#83583=CARTESIAN_POINT('',(32.8948869928718,-53.2064120173454,-0.9));
#83584=CARTESIAN_POINT('',(32.8948869928718,-53.2064120173454,-0.6));
#83585=CARTESIAN_POINT('Ctrl Pts',(32.8948869928718,-53.2064120173454,-0.9));
#83586=CARTESIAN_POINT('Ctrl Pts',(32.818345092237,-53.190177500248,-0.9));
#83587=CARTESIAN_POINT('Ctrl Pts',(32.6444044336677,-53.190177500248,-0.9));
#83588=CARTESIAN_POINT('Ctrl Pts',(33.1001367792487,-53.2968620657921,-0.6));
#83589=CARTESIAN_POINT('Ctrl Pts',(33.1001367792487,-53.2968620657921,-0.9));
#83590=CARTESIAN_POINT('Ctrl Pts',(32.9992475733161,-53.2319239974022,-0.6));
#83591=CARTESIAN_POINT('Ctrl Pts',(32.9992475733161,-53.2319239974022,-0.9));
#83592=CARTESIAN_POINT('Ctrl Pts',(32.8948869928718,-53.2064120173454,-0.6));
#83593=CARTESIAN_POINT('Ctrl Pts',(32.8948869928718,-53.2064120173454,-0.9));
#83594=CARTESIAN_POINT('',(33.1001367792487,-53.2968620657921,-0.6));
#83595=CARTESIAN_POINT('Ctrl Pts',(33.1001367792487,-53.2968620657921,-0.6));
#83596=CARTESIAN_POINT('Ctrl Pts',(32.9992475733161,-53.2319239974022,-0.6));
#83597=CARTESIAN_POINT('Ctrl Pts',(32.8948869928718,-53.2064120173454,-0.6));
#83598=CARTESIAN_POINT('',(33.1001367792487,-53.2968620657921,-0.9));
#83599=CARTESIAN_POINT('',(33.1001367792487,-53.2968620657921,-0.6));
#83600=CARTESIAN_POINT('Ctrl Pts',(33.1001367792487,-53.2968620657921,-0.9));
#83601=CARTESIAN_POINT('Ctrl Pts',(32.9992475733161,-53.2319239974022,-0.9));
#83602=CARTESIAN_POINT('Ctrl Pts',(32.8948869928718,-53.2064120173454,-0.9));
#83603=CARTESIAN_POINT('Ctrl Pts',(33.3285799250007,-53.5241476893425,-0.6));
#83604=CARTESIAN_POINT('Ctrl Pts',(33.3285799250007,-53.5241476893425,-0.9));
#83605=CARTESIAN_POINT('Ctrl Pts',(33.2010259851813,-53.3618007302284,-0.6));
#83606=CARTESIAN_POINT('Ctrl Pts',(33.2010259851813,-53.3618007302284,-0.9));
#83607=CARTESIAN_POINT('Ctrl Pts',(33.1001367792487,-53.2968620657921,-0.6));
#83608=CARTESIAN_POINT('Ctrl Pts',(33.1001367792487,-53.2968620657921,-0.9));
#83609=CARTESIAN_POINT('',(33.3285799250007,-53.5241476893425,-0.6));
#83610=CARTESIAN_POINT('Ctrl Pts',(33.3285799250007,-53.5241476893425,-0.6));
#83611=CARTESIAN_POINT('Ctrl Pts',(33.2010259851813,-53.3618007302284,-0.6));
#83612=CARTESIAN_POINT('Ctrl Pts',(33.1001367792487,-53.2968620657921,-0.6));
#83613=CARTESIAN_POINT('',(33.3285799250007,-53.5241476893425,-0.9));
#83614=CARTESIAN_POINT('',(33.3285799250007,-53.5241476893425,-0.6));
#83615=CARTESIAN_POINT('Ctrl Pts',(33.3285799250007,-53.5241476893425,-0.9));
#83616=CARTESIAN_POINT('Ctrl Pts',(33.2010259851813,-53.3618007302284,-0.9));
#83617=CARTESIAN_POINT('Ctrl Pts',(33.1001367792487,-53.2968620657921,-0.9));
#83618=CARTESIAN_POINT('Ctrl Pts',(33.6532774195075,-53.9926330447197,-0.6));
#83619=CARTESIAN_POINT('Ctrl Pts',(33.6532774195075,-53.9926330447197,-0.9));
#83620=CARTESIAN_POINT('Ctrl Pts',(33.45613386482,-53.6864940524101,-0.6));
#83621=CARTESIAN_POINT('Ctrl Pts',(33.45613386482,-53.6864940524101,-0.9));
#83622=CARTESIAN_POINT('Ctrl Pts',(33.3285799250007,-53.5241476893425,-0.6));
#83623=CARTESIAN_POINT('Ctrl Pts',(33.3285799250007,-53.5241476893425,-0.9));
#83624=CARTESIAN_POINT('',(33.6532774195075,-53.9926330447197,-0.6));
#83625=CARTESIAN_POINT('Ctrl Pts',(33.6532774195075,-53.9926330447197,-0.6));
#83626=CARTESIAN_POINT('Ctrl Pts',(33.45613386482,-53.6864940524101,-0.6));
#83627=CARTESIAN_POINT('Ctrl Pts',(33.3285799250007,-53.5241476893425,-0.6));
#83628=CARTESIAN_POINT('',(33.6532774195075,-53.9926330447197,-0.9));
#83629=CARTESIAN_POINT('',(33.6532774195075,-53.9926330447197,-0.6));
#83630=CARTESIAN_POINT('Ctrl Pts',(33.6532774195075,-53.9926330447197,-0.9));
#83631=CARTESIAN_POINT('Ctrl Pts',(33.45613386482,-53.6864940524101,-0.9));
#83632=CARTESIAN_POINT('Ctrl Pts',(33.3285799250007,-53.5241476893425,-0.9));
#83633=CARTESIAN_POINT('Origin',(34.1032018885016,-54.7000001072884,-0.6));
#83634=CARTESIAN_POINT('',(34.1032018885016,-54.7000001072884,-0.6));
#83635=CARTESIAN_POINT('',(28.806799412831,-46.3730454302682,-0.6));
#83636=CARTESIAN_POINT('',(34.1032018885016,-54.7000001072884,-0.9));
#83637=CARTESIAN_POINT('',(34.1032018885016,-54.7000001072884,-0.6));
#83638=CARTESIAN_POINT('',(34.1032018885016,-54.7000001072884,-0.9));
#83639=CARTESIAN_POINT('Origin',(34.6691026911139,-54.7000001072884,-0.6));
#83640=CARTESIAN_POINT('',(34.6691026911139,-54.7000001072884,-0.6));
#83641=CARTESIAN_POINT('',(17.334551345557,-54.7000001072884,-0.6));
#83642=CARTESIAN_POINT('',(34.6691026911139,-54.7000001072884,-0.9));
#83643=CARTESIAN_POINT('',(34.6691026911139,-54.7000001072884,-0.6));
#83644=CARTESIAN_POINT('',(34.6691026911139,-54.7000001072884,-0.9));
#83645=CARTESIAN_POINT('Origin',(34.0776911005378,-53.7746248841286,-0.6));
#83646=CARTESIAN_POINT('',(34.0776911005378,-53.7746248841286,-0.6));
#83647=CARTESIAN_POINT('',(28.9606432652394,-45.768036312039,-0.6));
#83648=CARTESIAN_POINT('',(34.0776911005378,-53.7746248841286,-0.9));
#83649=CARTESIAN_POINT('',(34.0776911005378,-53.7746248841286,-0.6));
#83650=CARTESIAN_POINT('',(34.0776911005378,-53.7746248841286,-0.9));
#83651=CARTESIAN_POINT('Ctrl Pts',(33.7042989954352,-53.3223740458488,-0.6));
#83652=CARTESIAN_POINT('Ctrl Pts',(33.7042989954352,-53.3223740458488,-0.9));
#83653=CARTESIAN_POINT('Ctrl Pts',(33.9014330133796,-53.5032741427422,-0.6));
#83654=CARTESIAN_POINT('Ctrl Pts',(33.9014330133796,-53.5032741427422,-0.9));
#83655=CARTESIAN_POINT('Ctrl Pts',(34.0776911005378,-53.7746248841286,-0.6));
#83656=CARTESIAN_POINT('Ctrl Pts',(34.0776911005378,-53.7746248841286,-0.9));
#83657=CARTESIAN_POINT('',(33.7042989954352,-53.3223740458488,-0.6));
#83658=CARTESIAN_POINT('Ctrl Pts',(33.7042989954352,-53.3223740458488,-0.6));
#83659=CARTESIAN_POINT('Ctrl Pts',(33.9014330133796,-53.5032741427422,-0.6));
#83660=CARTESIAN_POINT('Ctrl Pts',(34.0776911005378,-53.7746248841286,-0.6));
#83661=CARTESIAN_POINT('',(33.7042989954352,-53.3223740458488,-0.9));
#83662=CARTESIAN_POINT('',(33.7042989954352,-53.3223740458488,-0.6));
#83663=CARTESIAN_POINT('Ctrl Pts',(33.7042989954352,-53.3223740458488,-0.9));
#83664=CARTESIAN_POINT('Ctrl Pts',(33.9014330133796,-53.5032741427422,-0.9));
#83665=CARTESIAN_POINT('Ctrl Pts',(34.0776911005378,-53.7746248841286,-0.9));
#83666=CARTESIAN_POINT('Ctrl Pts',(33.4329500421882,-53.1530694365501,-0.6));
#83667=CARTESIAN_POINT('Ctrl Pts',(33.4329500421882,-53.1530694365501,-0.9));
#83668=CARTESIAN_POINT('Ctrl Pts',(33.6115255579352,-53.2388810515404,-0.6));
#83669=CARTESIAN_POINT('Ctrl Pts',(33.6115255579352,-53.2388810515404,-0.9));
#83670=CARTESIAN_POINT('Ctrl Pts',(33.7042989954352,-53.3223740458488,-0.6));
#83671=CARTESIAN_POINT('Ctrl Pts',(33.7042989954352,-53.3223740458488,-0.9));
#83672=CARTESIAN_POINT('',(33.4329500421882,-53.1530694365501,-0.6));
#83673=CARTESIAN_POINT('Ctrl Pts',(33.4329500421882,-53.1530694365501,-0.6));
#83674=CARTESIAN_POINT('Ctrl Pts',(33.6115255579352,-53.2388810515404,-0.6));
#83675=CARTESIAN_POINT('Ctrl Pts',(33.7042989954352,-53.3223740458488,-0.6));
#83676=CARTESIAN_POINT('',(33.4329500421882,-53.1530694365501,-0.9));
#83677=CARTESIAN_POINT('',(33.4329500421882,-53.1530694365501,-0.6));
#83678=CARTESIAN_POINT('Ctrl Pts',(33.4329500421882,-53.1530694365501,-0.9));
#83679=CARTESIAN_POINT('Ctrl Pts',(33.6115255579352,-53.2388810515404,-0.9));
#83680=CARTESIAN_POINT('Ctrl Pts',(33.7042989954352,-53.3223740458488,-0.9));
#83681=CARTESIAN_POINT('Ctrl Pts',(34.1565504297614,-52.8376535773277,-0.6));
#83682=CARTESIAN_POINT('Ctrl Pts',(34.1565504297614,-52.8376535773277,-0.9));
#83683=CARTESIAN_POINT('Ctrl Pts',(33.9223089441657,-53.0858115553856,-0.6));
#83684=CARTESIAN_POINT('Ctrl Pts',(33.9223089441657,-53.0858115553856,-0.9));
#83685=CARTESIAN_POINT('Ctrl Pts',(33.4329500421882,-53.1530694365501,-0.6));
#83686=CARTESIAN_POINT('Ctrl Pts',(33.4329500421882,-53.1530694365501,-0.9));
#83687=CARTESIAN_POINT('',(34.1565504297614,-52.8376535773277,-0.6));
#83688=CARTESIAN_POINT('Ctrl Pts',(34.1565504297614,-52.8376535773277,-0.6));
#83689=CARTESIAN_POINT('Ctrl Pts',(33.9223089441657,-53.0858115553856,-0.6));
#83690=CARTESIAN_POINT('Ctrl Pts',(33.4329500421882,-53.1530694365501,-0.6));
#83691=CARTESIAN_POINT('',(34.1565504297614,-52.8376535773277,-0.9));
#83692=CARTESIAN_POINT('',(34.1565504297614,-52.8376535773277,-0.6));
#83693=CARTESIAN_POINT('Ctrl Pts',(34.1565504297614,-52.8376535773277,-0.9));
#83694=CARTESIAN_POINT('Ctrl Pts',(33.9223089441657,-53.0858115553856,-0.9));
#83695=CARTESIAN_POINT('Ctrl Pts',(33.4329500421882,-53.1530694365501,-0.9));
#83696=CARTESIAN_POINT('Ctrl Pts',(34.3907919153571,-52.2276942133904,-0.6));
#83697=CARTESIAN_POINT('Ctrl Pts',(34.3907919153571,-52.2276942133904,-0.9));
#83698=CARTESIAN_POINT('Ctrl Pts',(34.3907919153571,-52.5894955992699,-0.6));
#83699=CARTESIAN_POINT('Ctrl Pts',(34.3907919153571,-52.5894955992699,-0.9));
#83700=CARTESIAN_POINT('Ctrl Pts',(34.1565504297614,-52.8376535773277,-0.6));
#83701=CARTESIAN_POINT('Ctrl Pts',(34.1565504297614,-52.8376535773277,-0.9));
#83702=CARTESIAN_POINT('',(34.3907919153571,-52.2276942133904,-0.6));
#83703=CARTESIAN_POINT('Ctrl Pts',(34.3907919153571,-52.2276942133904,-0.6));
#83704=CARTESIAN_POINT('Ctrl Pts',(34.3907919153571,-52.5894955992699,-0.6));
#83705=CARTESIAN_POINT('Ctrl Pts',(34.1565504297614,-52.8376535773277,-0.6));
#83706=CARTESIAN_POINT('',(34.3907919153571,-52.2276942133904,-0.9));
#83707=CARTESIAN_POINT('',(34.3907919153571,-52.2276942133904,-0.6));
#83708=CARTESIAN_POINT('Ctrl Pts',(34.3907919153571,-52.2276942133904,-0.9));
#83709=CARTESIAN_POINT('Ctrl Pts',(34.3907919153571,-52.5894955992699,-0.9));
#83710=CARTESIAN_POINT('Ctrl Pts',(34.1565504297614,-52.8376535773277,-0.9));
#83711=CARTESIAN_POINT('Ctrl Pts',(34.2493143305182,-51.7151431441307,-0.6));
#83712=CARTESIAN_POINT('Ctrl Pts',(34.2493143305182,-51.7151431441307,-0.9));
#83713=CARTESIAN_POINT('Ctrl Pts',(34.3907919153571,-51.9470672011375,-0.6));
#83714=CARTESIAN_POINT('Ctrl Pts',(34.3907919153571,-51.9470672011375,-0.9));
#83715=CARTESIAN_POINT('Ctrl Pts',(34.3907919153571,-52.2276942133904,-0.6));
#83716=CARTESIAN_POINT('Ctrl Pts',(34.3907919153571,-52.2276942133904,-0.9));
#83717=CARTESIAN_POINT('',(34.2493143305182,-51.7151431441307,-0.6));
#83718=CARTESIAN_POINT('Ctrl Pts',(34.2493143305182,-51.7151431441307,-0.6));
#83719=CARTESIAN_POINT('Ctrl Pts',(34.3907919153571,-51.9470672011375,-0.6));
#83720=CARTESIAN_POINT('Ctrl Pts',(34.3907919153571,-52.2276942133904,-0.6));
#83721=CARTESIAN_POINT('',(34.2493143305182,-51.7151431441307,-0.9));
#83722=CARTESIAN_POINT('',(34.2493143305182,-51.7151431441307,-0.6));
#83723=CARTESIAN_POINT('Ctrl Pts',(34.2493143305182,-51.7151431441307,-0.9));
#83724=CARTESIAN_POINT('Ctrl Pts',(34.3907919153571,-51.9470672011375,-0.9));
#83725=CARTESIAN_POINT('Ctrl Pts',(34.3907919153571,-52.2276942133904,-0.9));
#83726=CARTESIAN_POINT('Ctrl Pts',(33.8712778314948,-51.3916097283363,-0.6));
#83727=CARTESIAN_POINT('Ctrl Pts',(33.8712778314948,-51.3916097283363,-0.9));
#83728=CARTESIAN_POINT('Ctrl Pts',(34.1078462824225,-51.4832196831703,-0.6));
#83729=CARTESIAN_POINT('Ctrl Pts',(34.1078462824225,-51.4832196831703,-0.9));
#83730=CARTESIAN_POINT('Ctrl Pts',(34.2493143305182,-51.7151431441307,-0.6));
#83731=CARTESIAN_POINT('Ctrl Pts',(34.2493143305182,-51.7151431441307,-0.9));
#83732=CARTESIAN_POINT('',(33.8712778314948,-51.3916097283363,-0.6));
#83733=CARTESIAN_POINT('Ctrl Pts',(33.8712778314948,-51.3916097283363,-0.6));
#83734=CARTESIAN_POINT('Ctrl Pts',(34.1078462824225,-51.4832196831703,-0.6));
#83735=CARTESIAN_POINT('Ctrl Pts',(34.2493143305182,-51.7151431441307,-0.6));
#83736=CARTESIAN_POINT('',(33.8712778314948,-51.3916097283363,-0.9));
#83737=CARTESIAN_POINT('',(33.8712778314948,-51.3916097283363,-0.6));
#83738=CARTESIAN_POINT('Ctrl Pts',(33.8712778314948,-51.3916097283363,-0.9));
#83739=CARTESIAN_POINT('Ctrl Pts',(34.1078462824225,-51.4832196831703,-0.9));
#83740=CARTESIAN_POINT('Ctrl Pts',(34.2493143305182,-51.7151431441307,-0.9));
#83741=CARTESIAN_POINT('Ctrl Pts',(33.1801500543952,-51.3000003695488,-0.6));
#83742=CARTESIAN_POINT('Ctrl Pts',(33.1801500543952,-51.3000003695488,-0.9));
#83743=CARTESIAN_POINT('Ctrl Pts',(33.6347189173102,-51.3000003695488,-0.6));
#83744=CARTESIAN_POINT('Ctrl Pts',(33.6347189173102,-51.3000003695488,-0.9));
#83745=CARTESIAN_POINT('Ctrl Pts',(33.8712778314948,-51.3916097283363,-0.6));
#83746=CARTESIAN_POINT('Ctrl Pts',(33.8712778314948,-51.3916097283363,-0.9));
#83747=CARTESIAN_POINT('',(33.1801500543952,-51.3000003695488,-0.6));
#83748=CARTESIAN_POINT('Ctrl Pts',(33.1801500543952,-51.3000003695488,-0.6));
#83749=CARTESIAN_POINT('Ctrl Pts',(33.6347189173102,-51.3000003695488,-0.6));
#83750=CARTESIAN_POINT('Ctrl Pts',(33.8712778314948,-51.3916097283363,-0.6));
#83751=CARTESIAN_POINT('',(33.1801500543952,-51.3000003695488,-0.9));
#83752=CARTESIAN_POINT('',(33.1801500543952,-51.3000003695488,-0.6));
#83753=CARTESIAN_POINT('Ctrl Pts',(33.1801500543952,-51.3000003695488,-0.9));
#83754=CARTESIAN_POINT('Ctrl Pts',(33.6347189173102,-51.3000003695488,-0.9));
#83755=CARTESIAN_POINT('Ctrl Pts',(33.8712778314948,-51.3916097283363,-0.9));
#83756=CARTESIAN_POINT('Origin',(31.6726484522223,-51.3000003695488,-0.6));
#83757=CARTESIAN_POINT('',(31.6726484522223,-51.3000003695488,-0.6));
#83758=CARTESIAN_POINT('',(15.8363242261112,-51.3000003695488,-0.6));
#83759=CARTESIAN_POINT('',(31.6726484522223,-51.3000003695488,-0.9));
#83760=CARTESIAN_POINT('',(31.6726484522223,-51.3000003695488,-0.6));
#83761=CARTESIAN_POINT('',(31.6726484522223,-51.3000003695488,-0.9));
#83762=CARTESIAN_POINT('Origin',(31.6726484522223,-54.7000001072884,-0.6));
#83763=CARTESIAN_POINT('',(31.6726484522223,-54.7000001072884,-0.6));
#83764=CARTESIAN_POINT('',(31.6726484522223,-53.8500000536442,-0.6));
#83765=CARTESIAN_POINT('',(31.6726484522223,-54.7000001072884,-0.9));
#83766=CARTESIAN_POINT('',(31.6726484522223,-54.7000001072884,-0.6));
#83767=CARTESIAN_POINT('',(31.6726484522223,-54.7000001072884,-0.9));
#83768=CARTESIAN_POINT('Origin',(32.1225824579597,-54.7000001072884,-0.6));
#83769=CARTESIAN_POINT('',(32.1225824579597,-54.7000001072884,-0.6));
#83770=CARTESIAN_POINT('',(16.0612912289798,-54.7000001072884,-0.6));
#83771=CARTESIAN_POINT('',(32.1225824579597,-54.7000001072884,-0.9));
#83772=CARTESIAN_POINT('',(32.1225824579597,-54.7000001072884,-0.6));
#83773=CARTESIAN_POINT('',(32.1225824579597,-54.7000001072884,-0.9));
#83774=CARTESIAN_POINT('Origin',(32.1225824579597,-53.190177500248,-0.6));
#83775=CARTESIAN_POINT('',(32.1225824579597,-53.095088750124,-0.6));
#83776=CARTESIAN_POINT('',(32.1225824579597,-53.190177500248,-0.9));
#83777=CARTESIAN_POINT('Origin',(33.1708755716681,-53.0000002384186,-0.9));
#83778=CARTESIAN_POINT('Origin',(-36.,-60.,-0.6));
#83779=CARTESIAN_POINT('',(36.,-60.,0.));
#83780=CARTESIAN_POINT('',(-36.,-60.,0.));
#83781=CARTESIAN_POINT('',(-18.,-60.,0.));
#83782=CARTESIAN_POINT('',(36.,-60.,-0.6));
#83783=CARTESIAN_POINT('',(36.,-60.,-0.6));
#83784=CARTESIAN_POINT('',(-36.,-60.,-0.6));
#83785=CARTESIAN_POINT('',(-36.,-60.,-0.6));
#83786=CARTESIAN_POINT('',(-36.,-60.,-0.6));
#83787=CARTESIAN_POINT('Origin',(-36.,-46.,-0.6));
#83788=CARTESIAN_POINT('',(-36.,-46.,0.));
#83789=CARTESIAN_POINT('',(-36.,-23.,0.));
#83790=CARTESIAN_POINT('',(-36.,-46.,-0.6));
#83791=CARTESIAN_POINT('',(-36.,-46.,-0.6));
#83792=CARTESIAN_POINT('',(-36.,-46.,-0.6));
#83793=CARTESIAN_POINT('Origin',(36.,-46.,-0.6));
#83794=CARTESIAN_POINT('',(36.,-46.,0.));
#83795=CARTESIAN_POINT('',(18.,-46.,0.));
#83796=CARTESIAN_POINT('',(36.,-46.,-0.6));
#83797=CARTESIAN_POINT('',(36.,-46.,-0.6));
#83798=CARTESIAN_POINT('',(36.,-46.,-0.6));
#83799=CARTESIAN_POINT('Origin',(36.,-60.,-0.6));
#83800=CARTESIAN_POINT('',(36.,-30.,0.));
#83801=CARTESIAN_POINT('',(36.,-60.,-0.6));
#83802=CARTESIAN_POINT('Origin',(0.,-53.,-0.6));
#83803=CARTESIAN_POINT('Origin',(-75.,-50.,-0.25));
#83804=CARTESIAN_POINT('',(-80.,-50.,0.));
#83805=CARTESIAN_POINT('Origin',(-75.,-50.,0.));
#83806=CARTESIAN_POINT('',(-79.5,-50.,-0.5));
#83807=CARTESIAN_POINT('',(-79.75,-50.,-0.25));
#83808=CARTESIAN_POINT('Origin',(-75.,-50.,-0.5));
#83809=CARTESIAN_POINT('Origin',(-75.,-50.,-16.5));
#83810=CARTESIAN_POINT('',(-79.5,-50.,-15.5));
#83811=CARTESIAN_POINT('Origin',(-75.,-50.,-15.5));
#83812=CARTESIAN_POINT('',(-79.5,-50.,-16.5));
#83813=CARTESIAN_POINT('Origin',(0.,0.,0.));
#83814=CARTESIAN_POINT('',(-89.,-55.,0.));
#83815=CARTESIAN_POINT('',(-89.,55.,0.));
#83816=CARTESIAN_POINT('',(-89.,27.5,0.));
#83817=CARTESIAN_POINT('',(-80.,-64.,0.));
#83818=CARTESIAN_POINT('Origin',(-80.,-55.,0.));
#83819=CARTESIAN_POINT('',(80.,-64.,0.));
#83820=CARTESIAN_POINT('',(-40.,-64.,0.));
#83821=CARTESIAN_POINT('',(89.,-55.,0.));
#83822=CARTESIAN_POINT('Origin',(80.,-55.,0.));
#83823=CARTESIAN_POINT('',(89.,55.,0.));
#83824=CARTESIAN_POINT('',(89.,-27.5,0.));
#83825=CARTESIAN_POINT('',(80.,64.,0.));
#83826=CARTESIAN_POINT('Origin',(80.,55.,0.));
#83827=CARTESIAN_POINT('',(-80.,64.,0.));
#83828=CARTESIAN_POINT('',(40.,64.,0.));
#83829=CARTESIAN_POINT('Origin',(-80.,55.,0.));
#83830=CARTESIAN_POINT('',(70.,-50.,0.));
#83831=CARTESIAN_POINT('Origin',(75.,-50.,0.));
#83832=CARTESIAN_POINT('',(-38.3,4.69039724073436E-15,8.15320033709099E-16));
#83833=CARTESIAN_POINT('Origin',(-35.,4.28626379701574E-15,0.));
#83834=CARTESIAN_POINT('',(31.7,4.04133443718627E-16,8.15320033709099E-16));
#83835=CARTESIAN_POINT('Origin',(35.,0.,0.));
#83836=CARTESIAN_POINT('',(-3.3,35.,8.15320033709099E-16));
#83837=CARTESIAN_POINT('Origin',(2.14313189850787E-15,35.,0.));
#83838=CARTESIAN_POINT('',(-3.30000000000001,-35.,8.15320033709099E-16));
#83839=CARTESIAN_POINT('Origin',(-6.4293956955236E-15,-35.,0.));
#83840=CARTESIAN_POINT('',(-20.025,2.45235521529257E-15,0.));
#83841=CARTESIAN_POINT('Origin',(0.,0.,0.));
#83842=CARTESIAN_POINT('',(-27.7487373415292,-24.7487373415292,0.));
#83843=CARTESIAN_POINT('Origin',(-24.7487373415292,-24.7487373415292,0.));
#83844=CARTESIAN_POINT('',(21.7487373415292,24.7487373415292,0.));
#83845=CARTESIAN_POINT('Origin',(24.7487373415292,24.7487373415292,0.));
#83846=CARTESIAN_POINT('',(-80.,50.,0.));
#83847=CARTESIAN_POINT('Origin',(-75.,50.,0.));
#83848=CARTESIAN_POINT('',(70.,50.,0.));
#83849=CARTESIAN_POINT('Origin',(75.,50.,0.));
#83850=CARTESIAN_POINT('Origin',(-75.,-50.,-15.75));
#83851=CARTESIAN_POINT('',(-80.,-50.,-16.));
#83852=CARTESIAN_POINT('Origin',(-75.,-50.,-16.));
#83853=CARTESIAN_POINT('',(-79.75,-50.,-15.75));
#83854=CARTESIAN_POINT('Origin',(0.,0.,-16.));
#83855=CARTESIAN_POINT('',(80.,-64.5,-16.));
#83856=CARTESIAN_POINT('',(89.5,-55.,-16.));
#83857=CARTESIAN_POINT('Origin',(80.,-55.,-16.));
#83858=CARTESIAN_POINT('',(-80.,-64.5,-16.));
#83859=CARTESIAN_POINT('',(-40.,-64.5,-16.));
#83860=CARTESIAN_POINT('',(-89.5,-55.,-16.));
#83861=CARTESIAN_POINT('Origin',(-80.,-55.,-16.));
#83862=CARTESIAN_POINT('',(-89.5,55.,-16.));
#83863=CARTESIAN_POINT('',(-89.5,27.5,-16.));
#83864=CARTESIAN_POINT('',(-80.,64.5,-16.));
#83865=CARTESIAN_POINT('Origin',(-80.,55.,-16.));
#83866=CARTESIAN_POINT('',(80.,64.5,-16.));
#83867=CARTESIAN_POINT('',(40.,64.5,-16.));
#83868=CARTESIAN_POINT('',(89.5,55.,-16.));
#83869=CARTESIAN_POINT('Origin',(80.,55.,-16.));
#83870=CARTESIAN_POINT('',(89.5,-27.5,-16.));
#83871=CARTESIAN_POINT('',(70.,50.,-16.));
#83872=CARTESIAN_POINT('Origin',(75.,50.,-16.));
#83873=CARTESIAN_POINT('',(-80.,50.,-16.));
#83874=CARTESIAN_POINT('Origin',(-75.,50.,-16.));
#83875=CARTESIAN_POINT('',(70.,-50.,-16.));
#83876=CARTESIAN_POINT('Origin',(75.,-50.,-16.));
#83877=CARTESIAN_POINT('Origin',(75.,50.,-0.25));
#83878=CARTESIAN_POINT('',(70.5,50.,-0.5));
#83879=CARTESIAN_POINT('',(70.25,50.,-0.25));
#83880=CARTESIAN_POINT('Origin',(75.,50.,-0.5));
#83881=CARTESIAN_POINT('Origin',(75.,50.,-16.5));
#83882=CARTESIAN_POINT('',(70.5,50.,-15.5));
#83883=CARTESIAN_POINT('Origin',(75.,50.,-15.5));
#83884=CARTESIAN_POINT('',(70.5,50.,-16.5));
#83885=CARTESIAN_POINT('Origin',(75.,50.,-15.75));
#83886=CARTESIAN_POINT('',(70.25,50.,-15.75));
#83887=CARTESIAN_POINT('Origin',(75.,-50.,-0.25));
#83888=CARTESIAN_POINT('',(70.5,-50.,-0.5));
#83889=CARTESIAN_POINT('',(70.25,-50.,-0.25));
#83890=CARTESIAN_POINT('Origin',(75.,-50.,-0.5));
#83891=CARTESIAN_POINT('Origin',(75.,-50.,-16.5));
#83892=CARTESIAN_POINT('',(70.5,-50.,-15.5));
#83893=CARTESIAN_POINT('Origin',(75.,-50.,-15.5));
#83894=CARTESIAN_POINT('',(70.5,-50.,-16.5));
#83895=CARTESIAN_POINT('Origin',(75.,-50.,-15.75));
#83896=CARTESIAN_POINT('',(70.25,-50.,-15.75));
#83897=CARTESIAN_POINT('Origin',(-75.,50.,-0.25));
#83898=CARTESIAN_POINT('',(-79.5,50.,-0.5));
#83899=CARTESIAN_POINT('',(-79.75,50.,-0.25));
#83900=CARTESIAN_POINT('Origin',(-75.,50.,-0.5));
#83901=CARTESIAN_POINT('Origin',(-75.,50.,-16.5));
#83902=CARTESIAN_POINT('',(-79.5,50.,-15.5));
#83903=CARTESIAN_POINT('Origin',(-75.,50.,-15.5));
#83904=CARTESIAN_POINT('',(-79.5,50.,-16.5));
#83905=CARTESIAN_POINT('Origin',(-75.,50.,-15.75));
#83906=CARTESIAN_POINT('',(-79.75,50.,-15.75));
#83907=CARTESIAN_POINT('Origin',(24.7487373415292,24.7487373415292,-10.9012909285413));
#83908=CARTESIAN_POINT('',(21.7487373415292,24.7487373415292,-10.));
#83909=CARTESIAN_POINT('Origin',(24.7487373415292,24.7487373415292,-10.));
#83910=CARTESIAN_POINT('',(24.7487373415292,24.7487373415292,-11.8025818570827));
#83911=CARTESIAN_POINT('',(23.2487373415292,24.7487373415292,-10.9012909285413));
#83912=CARTESIAN_POINT('Origin',(24.7487373415292,24.7487373415292,-5.));
#83913=CARTESIAN_POINT('',(21.7487373415292,24.7487373415292,-5.));
#83914=CARTESIAN_POINT('Origin',(-24.7487373415292,-24.7487373415292,-10.9012909285413));
#83915=CARTESIAN_POINT('',(-27.7487373415292,-24.7487373415292,-10.));
#83916=CARTESIAN_POINT('Origin',(-24.7487373415292,-24.7487373415292,-10.));
#83917=CARTESIAN_POINT('',(-24.7487373415292,-24.7487373415292,-11.8025818570827));
#83918=CARTESIAN_POINT('',(-26.2487373415292,-24.7487373415292,-10.9012909285413));
#83919=CARTESIAN_POINT('Origin',(-24.7487373415292,-24.7487373415292,-5.));
#83920=CARTESIAN_POINT('',(-27.7487373415292,-24.7487373415292,-5.));
#83921=CARTESIAN_POINT('Origin',(-35.,4.28626379701574E-15,-14.916312444017));
#83922=CARTESIAN_POINT('',(-38.05,4.65978107075568E-15,-14.));
#83923=CARTESIAN_POINT('Origin',(-35.,4.28626379701574E-15,-14.));
#83924=CARTESIAN_POINT('',(-35.,4.28626379701574E-15,-15.8326248880341));
#83925=CARTESIAN_POINT('',(-36.525,4.47302243388571E-15,-14.916312444017));
#83926=CARTESIAN_POINT('Origin',(-35.,4.28626379701574E-15,-0.125));
#83927=CARTESIAN_POINT('',(-38.05,4.65978107075568E-15,-0.250000000000001));
#83928=CARTESIAN_POINT('',(-38.175,4.67508915574502E-15,-0.125));
#83929=CARTESIAN_POINT('Origin',(-35.,4.28626379701574E-15,-0.250000000000001));
#83930=CARTESIAN_POINT('Origin',(-35.,4.28626379701574E-15,-7.));
#83931=CARTESIAN_POINT('',(-38.05,4.65978107075568E-15,-7.));
#83932=CARTESIAN_POINT('Origin',(35.,0.,-14.916312444017));
#83933=CARTESIAN_POINT('',(31.95,3.73517273739943E-16,-14.));
#83934=CARTESIAN_POINT('Origin',(35.,0.,-14.));
#83935=CARTESIAN_POINT('',(35.,0.,-15.8326248880341));
#83936=CARTESIAN_POINT('',(33.475,1.86758636869971E-16,-14.916312444017));
#83937=CARTESIAN_POINT('Origin',(35.,0.,-0.125));
#83938=CARTESIAN_POINT('',(31.95,3.73517273739943E-16,-0.250000000000001));
#83939=CARTESIAN_POINT('',(31.825,3.88825358729285E-16,-0.125));
#83940=CARTESIAN_POINT('Origin',(35.,0.,-0.250000000000001));
#83941=CARTESIAN_POINT('Origin',(35.,0.,-7.));
#83942=CARTESIAN_POINT('',(31.95,3.73517273739943E-16,-7.));
#83943=CARTESIAN_POINT('Origin',(2.14313189850787E-15,35.,-14.916312444017));
#83944=CARTESIAN_POINT('',(-3.05,35.,-14.));
#83945=CARTESIAN_POINT('Origin',(2.14313189850787E-15,35.,-14.));
#83946=CARTESIAN_POINT('',(2.14313189850787E-15,35.,-15.8326248880341));
#83947=CARTESIAN_POINT('',(-1.525,35.,-14.916312444017));
#83948=CARTESIAN_POINT('Origin',(2.14313189850787E-15,35.,-0.125));
#83949=CARTESIAN_POINT('',(-3.05,35.,-0.250000000000001));
#83950=CARTESIAN_POINT('',(-3.175,35.,-0.125));
#83951=CARTESIAN_POINT('Origin',(2.14313189850787E-15,35.,-0.250000000000001));
#83952=CARTESIAN_POINT('Origin',(2.14313189850787E-15,35.,-7.));
#83953=CARTESIAN_POINT('',(-3.05,35.,-7.));
#83954=CARTESIAN_POINT('Origin',(-6.4293956955236E-15,-35.,-14.916312444017));
#83955=CARTESIAN_POINT('',(-3.05000000000001,-35.,-14.));
#83956=CARTESIAN_POINT('Origin',(-6.4293956955236E-15,-35.,-14.));
#83957=CARTESIAN_POINT('',(-6.4293956955236E-15,-35.,-15.8326248880341));
#83958=CARTESIAN_POINT('',(-1.52500000000001,-35.,-14.916312444017));
#83959=CARTESIAN_POINT('Origin',(-6.4293956955236E-15,-35.,-0.125));
#83960=CARTESIAN_POINT('',(-3.05000000000001,-35.,-0.250000000000001));
#83961=CARTESIAN_POINT('',(-3.17500000000001,-35.,-0.125));
#83962=CARTESIAN_POINT('Origin',(-6.4293956955236E-15,-35.,-0.250000000000001));
#83963=CARTESIAN_POINT('Origin',(-6.4293956955236E-15,-35.,-7.));
#83964=CARTESIAN_POINT('',(-3.05000000000001,-35.,-7.));
#83965=CARTESIAN_POINT('Origin',(0.,0.,-4.2));
#83966=CARTESIAN_POINT('',(-20.025,-2.45235521529257E-15,-4.2));
#83967=CARTESIAN_POINT('Origin',(0.,0.,-4.2));
#83968=CARTESIAN_POINT('',(-20.025,-2.45235521529257E-15,-4.2));
#83969=CARTESIAN_POINT('Origin',(0.,0.,-4.2));
#83970=CARTESIAN_POINT('Origin',(80.,-55.,-15.75));
#83971=CARTESIAN_POINT('',(90.,-55.,-15.5));
#83972=CARTESIAN_POINT('',(89.5,-55.,-16.));
#83973=CARTESIAN_POINT('',(80.,-65.,-15.5));
#83974=CARTESIAN_POINT('Origin',(80.,-55.,-15.5));
#83975=CARTESIAN_POINT('',(80.,-65.,-15.5));
#83976=CARTESIAN_POINT('Origin',(89.75,-27.5,-15.75));
#83977=CARTESIAN_POINT('',(90.,55.,-15.5));
#83978=CARTESIAN_POINT('',(89.5,55.,-16.));
#83979=CARTESIAN_POINT('',(90.,-27.5,-15.5));
#83980=CARTESIAN_POINT('Origin',(80.,55.,-15.75));
#83981=CARTESIAN_POINT('',(80.,65.,-15.5));
#83982=CARTESIAN_POINT('',(80.,64.5,-16.));
#83983=CARTESIAN_POINT('Origin',(80.,55.,-15.5));
#83984=CARTESIAN_POINT('Origin',(40.,64.75,-15.75));
#83985=CARTESIAN_POINT('',(-80.,65.,-15.5));
#83986=CARTESIAN_POINT('',(-80.,64.5,-16.));
#83987=CARTESIAN_POINT('',(40.,65.,-15.5));
#83988=CARTESIAN_POINT('Origin',(-80.,55.,-15.75));
#83989=CARTESIAN_POINT('',(-90.,55.,-15.5));
#83990=CARTESIAN_POINT('',(-89.5,55.,-16.));
#83991=CARTESIAN_POINT('Origin',(-80.,55.,-15.5));
#83992=CARTESIAN_POINT('Origin',(-89.75,27.5,-15.75));
#83993=CARTESIAN_POINT('',(-90.,-55.,-15.5));
#83994=CARTESIAN_POINT('',(-89.5,-55.,-16.));
#83995=CARTESIAN_POINT('',(-90.,27.5,-15.5));
#83996=CARTESIAN_POINT('Origin',(-80.,-55.,-15.75));
#83997=CARTESIAN_POINT('',(-80.,-65.,-15.5));
#83998=CARTESIAN_POINT('',(-80.,-64.5,-16.));
#83999=CARTESIAN_POINT('Origin',(-80.,-55.,-15.5));
#84000=CARTESIAN_POINT('Origin',(-40.,-64.75,-15.75));
#84001=CARTESIAN_POINT('',(-40.,-65.,-15.5));
#84002=CARTESIAN_POINT('Origin',(-90.,55.,-16.));
#84003=CARTESIAN_POINT('',(-90.,-55.,-1.));
#84004=CARTESIAN_POINT('',(-90.,-55.,-16.));
#84005=CARTESIAN_POINT('',(-90.,55.,-1.));
#84006=CARTESIAN_POINT('',(-90.,27.5,-1.));
#84007=CARTESIAN_POINT('',(-90.,55.,-16.));
#84008=CARTESIAN_POINT('Origin',(-80.,-55.,-16.));
#84009=CARTESIAN_POINT('',(-80.,-65.,-1.));
#84010=CARTESIAN_POINT('',(-80.,-65.,-16.));
#84011=CARTESIAN_POINT('Origin',(-80.,-55.,-1.));
#84012=CARTESIAN_POINT('Origin',(-80.,-65.,-16.));
#84013=CARTESIAN_POINT('',(80.,-65.,-1.));
#84014=CARTESIAN_POINT('',(80.,-65.,-16.));
#84015=CARTESIAN_POINT('',(-40.,-65.,-1.));
#84016=CARTESIAN_POINT('Origin',(80.,-55.,-16.));
#84017=CARTESIAN_POINT('',(90.,-55.,-1.));
#84018=CARTESIAN_POINT('',(90.,-55.,-16.));
#84019=CARTESIAN_POINT('Origin',(80.,-55.,-1.));
#84020=CARTESIAN_POINT('Origin',(-89.5,27.5,-0.5));
#84021=CARTESIAN_POINT('',(-90.,-55.,-1.));
#84022=CARTESIAN_POINT('',(-89.,55.,0.));
#84023=CARTESIAN_POINT('Origin',(-80.,-55.,-0.5));
#84024=CARTESIAN_POINT('',(-80.,-65.,-1.));
#84025=CARTESIAN_POINT('Origin',(-40.,-64.5,-0.5));
#84026=CARTESIAN_POINT('',(80.,-65.,-1.));
#84027=CARTESIAN_POINT('Origin',(80.,-55.,-0.5));
#84028=CARTESIAN_POINT('',(90.,-55.,-1.));
#84029=CARTESIAN_POINT('Origin',(89.5,-27.5,-0.5));
#84030=CARTESIAN_POINT('',(90.,55.,-1.));
#84031=CARTESIAN_POINT('',(90.,55.,-1.));
#84032=CARTESIAN_POINT('',(90.,-27.5,-1.));
#84033=CARTESIAN_POINT('Origin',(80.,55.,-0.5));
#84034=CARTESIAN_POINT('',(80.,65.,-1.));
#84035=CARTESIAN_POINT('',(80.,65.,-1.));
#84036=CARTESIAN_POINT('Origin',(80.,55.,-1.));
#84037=CARTESIAN_POINT('Origin',(40.,64.5,-0.5));
#84038=CARTESIAN_POINT('',(-80.,65.,-1.));
#84039=CARTESIAN_POINT('',(-80.,65.,-1.));
#84040=CARTESIAN_POINT('',(40.,65.,-1.));
#84041=CARTESIAN_POINT('Origin',(-80.,55.,-0.5));
#84042=CARTESIAN_POINT('Origin',(-80.,55.,-1.));
#84043=CARTESIAN_POINT('Origin',(-80.,55.,-16.));
#84044=CARTESIAN_POINT('',(-80.,65.,-16.));
#84045=CARTESIAN_POINT('Origin',(80.,65.,-16.));
#84046=CARTESIAN_POINT('',(80.,65.,-16.));
#84047=CARTESIAN_POINT('Origin',(80.,55.,-16.));
#84048=CARTESIAN_POINT('',(90.,55.,-16.));
#84049=CARTESIAN_POINT('Origin',(90.,-55.,-16.));
#84050=CARTESIAN_POINT('',(0.,0.,0.));
#84051=CARTESIAN_POINT('Origin',(3.,0.,0.));
#84052=CARTESIAN_POINT('',(5.5,-5.5,-6.73555739531044E-16));
#84053=CARTESIAN_POINT('Origin',(5.5,0.,0.));
#84054=CARTESIAN_POINT('',(0.5,-5.5,-6.73555739531044E-16));
#84055=CARTESIAN_POINT('',(3.,-5.5,-6.73555739531044E-16));
#84056=CARTESIAN_POINT('Origin',(0.5,0.,0.));
#84057=CARTESIAN_POINT('Origin',(0.25,0.,0.));
#84058=CARTESIAN_POINT('',(-2.42861286636753E-16,-6.,-7.34788079488412E-16));
#84059=CARTESIAN_POINT('',(0.25,-5.75,-7.04171909509728E-16));
#84060=CARTESIAN_POINT('Origin',(0.,0.,0.));
#84061=CARTESIAN_POINT('Origin',(0.,27.5,0.));
#84062=CARTESIAN_POINT('',(-7.63278329429795E-16,-27.5,-3.36777869765522E-15));
#84063=CARTESIAN_POINT('Origin',(0.,0.,0.));
#84064=CARTESIAN_POINT('Origin',(0.25,0.,0.));
#84065=CARTESIAN_POINT('',(0.500000000000002,-28.,-3.42901103761259E-15));
#84066=CARTESIAN_POINT('Origin',(0.5,0.,0.));
#84067=CARTESIAN_POINT('',(0.25,-27.75,-3.39839486763391E-15));
#84068=CARTESIAN_POINT('Origin',(2.75,0.,0.));
#84069=CARTESIAN_POINT('',(5.,-28.,-3.42901103761259E-15));
#84070=CARTESIAN_POINT('Origin',(5.,0.,0.));
#84071=CARTESIAN_POINT('',(2.75,-28.,-3.42901103761259E-15));
#84072=CARTESIAN_POINT('Origin',(5.5,0.,0.));
#84073=CARTESIAN_POINT('',(6.,-27.,-3.30654635769785E-15));
#84074=CARTESIAN_POINT('Origin',(6.,0.,0.));
#84075=CARTESIAN_POINT('',(5.5,-27.5,-3.36777869765522E-15));
#84076=CARTESIAN_POINT('Origin',(6.,6.,0.));
#84077=CARTESIAN_POINT('',(6.,-6.,-7.34788079488412E-16));
#84078=CARTESIAN_POINT('Origin',(6.,0.,0.));
#84079=CARTESIAN_POINT('Origin',(5.75,0.,0.));
#84080=CARTESIAN_POINT('',(5.75,-5.75,-7.04171909509728E-16));
#84081=CARTESIAN_POINT('',(0.,0.,0.));
#84082=CARTESIAN_POINT('Origin',(-12.,0.,0.));
#84083=CARTESIAN_POINT('',(-23.5911584740964,-4.92956674790982,0.00292070512225823));
#84084=CARTESIAN_POINT('',(-23.8088415259036,-4.92702269843929,0.00145594308024882));
#84085=CARTESIAN_POINT('',(-12.,-4.925,-6.03138548580071E-16));
#84086=CARTESIAN_POINT('',(-24.075,2.17166274343819,4.42389655029935));
#84087=CARTESIAN_POINT('Ctrl Pts',(-23.5911584740964,-4.92956674790982,
0.00292070512225823));
#84088=CARTESIAN_POINT('Ctrl Pts',(-23.6009614954506,-4.93111317644749,
0.204570992366802));
#84089=CARTESIAN_POINT('Ctrl Pts',(-23.6107645168047,-4.91982886340447,
0.406056936676851));
#84090=CARTESIAN_POINT('Ctrl Pts',(-23.6205675381589,-4.89513422052396,
0.605891441984341));
#84091=CARTESIAN_POINT('Ctrl Pts',(-23.6995490603975,-4.69617306198144,
2.21592908800913));
#84092=CARTESIAN_POINT('Ctrl Pts',(-23.7785305826362,-3.62670832241862,
3.71876701687665));
#84093=CARTESIAN_POINT('Ctrl Pts',(-23.8575121048748,-2.16899469412727,
4.4312955762216));
#84094=CARTESIAN_POINT('Ctrl Pts',(-23.9300080699165,-0.830981026599293,
5.08531494765676));
#84095=CARTESIAN_POINT('Ctrl Pts',(-24.0025040349583,0.834137422466123,
5.07348830853079));
#84096=CARTESIAN_POINT('Ctrl Pts',(-24.075,2.1749296145658,4.42583829068189));
#84097=CARTESIAN_POINT('',(-24.075,-2.16839587231057,4.42195480991682));
#84098=CARTESIAN_POINT('Origin',(-24.075,0.,0.));
#84099=CARTESIAN_POINT('Ctrl Pts',(-24.075,-2.16839587231055,4.42195480991682));
#84100=CARTESIAN_POINT('Ctrl Pts',(-24.0355092388807,-2.89986906309508,
4.0632619883516));
#84101=CARTESIAN_POINT('Ctrl Pts',(-23.9960184777614,-3.53523507248361,
3.51964117664448));
#84102=CARTESIAN_POINT('Ctrl Pts',(-23.956527716642,-4.00941683121766,2.85617839596279));
#84103=CARTESIAN_POINT('Ctrl Pts',(-23.9170369555227,-4.48359858995173,
2.19271561528108));
#84104=CARTESIAN_POINT('Ctrl Pts',(-23.8775461944034,-4.79659609803131,
1.40941086562478));
#84105=CARTESIAN_POINT('Ctrl Pts',(-23.8380554332841,-4.89386793853736,
0.60185165851297));
#84106=CARTESIAN_POINT('Ctrl Pts',(-23.8283174641573,-4.91785405966823,
0.402716812689607));
#84107=CARTESIAN_POINT('Ctrl Pts',(-23.8185794950304,-4.92872278569346,
0.202107152556501));
#84108=CARTESIAN_POINT('Ctrl Pts',(-23.8088415259036,-4.92702269843929,
0.00145594308024882));
#84109=CARTESIAN_POINT('Origin',(-12.,0.,0.));
#84110=CARTESIAN_POINT('',(-22.0911584740964,-4.91737544826784,0.00117139545793843));
#84111=CARTESIAN_POINT('',(-22.3088415259036,-4.91734906814233,0.00115834211832263));
#84112=CARTESIAN_POINT('',(-12.,-4.925,-6.03138548580071E-16));
#84113=CARTESIAN_POINT('Ctrl Pts',(-22.0911584740964,-4.91737544826784,
0.00117139545793843));
#84114=CARTESIAN_POINT('Ctrl Pts',(-22.1270723620188,-4.91897685522205,
0.744760528145342));
#84115=CARTESIAN_POINT('Ctrl Pts',(-22.1629862499411,-4.76069723452924,
1.48770236188821));
#84116=CARTESIAN_POINT('Ctrl Pts',(-22.1989001378635,-4.43900651799258,
2.1514447222654));
#84117=CARTESIAN_POINT('Ctrl Pts',(-22.2778816601021,-3.7315469820872,3.61114137527611));
#84118=CARTESIAN_POINT('Ctrl Pts',(-22.3568631823407,-2.23375885028816,
4.68779421931301));
#84119=CARTESIAN_POINT('Ctrl Pts',(-22.4358447045794,-0.624704128296198,
4.8932036453613));
#84120=CARTESIAN_POINT('Ctrl Pts',(-22.514826226818,0.984350593695766,5.09861307140959));
#84121=CARTESIAN_POINT('Ctrl Pts',(-22.5938077490566,2.70467190588065,4.43277907946927));
#84122=CARTESIAN_POINT('Ctrl Pts',(-22.6727892712953,3.75614713958277,3.19766196357196));
#84123=CARTESIAN_POINT('Ctrl Pts',(-22.7517707935339,4.80762237328489,1.96254484767464));
#84124=CARTESIAN_POINT('Ctrl Pts',(-22.8307523157726,5.19025152850426,0.158144607820335));
#84125=CARTESIAN_POINT('Ctrl Pts',(-22.9097338380112,4.7307378850514,-1.39752590139163));
#84126=CARTESIAN_POINT('Ctrl Pts',(-22.9887153602498,4.27122424159855,-2.95319641060359));
#84127=CARTESIAN_POINT('Ctrl Pts',(-23.0676968824885,2.96956779947348,-4.26013718917321));
#84128=CARTESIAN_POINT('Ctrl Pts',(-23.1466784047271,1.41558592983439,-4.72553140556831));
#84129=CARTESIAN_POINT('Ctrl Pts',(-23.2256599269657,-0.138395939804694,
-5.19092562196341));
#84130=CARTESIAN_POINT('Ctrl Pts',(-23.3046414492044,-1.9447032369578,-4.81477327618398));
#84131=CARTESIAN_POINT('Ctrl Pts',(-23.383622971443,-3.18362809677325,-3.76807842170324));
#84132=CARTESIAN_POINT('Ctrl Pts',(-23.4528014723275,-4.26878019414078,
-2.85129714344818));
#84133=CARTESIAN_POINT('Ctrl Pts',(-23.5219799732119,-4.91865382585283,
-1.42009614555244));
#84134=CARTESIAN_POINT('Ctrl Pts',(-23.5911584740964,-4.92956674790982,
0.00292070512225823));
#84135=CARTESIAN_POINT('Ctrl Pts',(-23.8088415259036,-4.92702269843929,
0.00145594308024882));
#84136=CARTESIAN_POINT('Ctrl Pts',(-23.7395979727918,-4.91493392710047,
-1.42530999747258));
#84137=CARTESIAN_POINT('Ctrl Pts',(-23.67035441968,-4.26734424473369,-2.85417674458798));
#84138=CARTESIAN_POINT('Ctrl Pts',(-23.6011108665682,-3.18148423977708,
-3.76984525036356));
#84139=CARTESIAN_POINT('Ctrl Pts',(-23.5221293443296,-1.94291584928667,
-4.81428750097075));
#84140=CARTESIAN_POINT('Ctrl Pts',(-23.4431478220909,-0.134138057587843,
-5.19103575813942));
#84141=CARTESIAN_POINT('Ctrl Pts',(-23.3641662998523,1.41999380222758,-4.72488423722609));
#84142=CARTESIAN_POINT('Ctrl Pts',(-23.2851847776136,2.974125662043,-4.25873271631276));
#84143=CARTESIAN_POINT('Ctrl Pts',(-23.206203255375,4.27361158997502,-2.94968141731743));
#84144=CARTESIAN_POINT('Ctrl Pts',(-23.1272217331364,4.7315879300895,-1.39338320500447));
#84145=CARTESIAN_POINT('Ctrl Pts',(-23.0482402108977,5.18956427020398,0.162915007308491));
#84146=CARTESIAN_POINT('Ctrl Pts',(-22.9692586886591,4.80603102250092,1.96646013293908));
#84147=CARTESIAN_POINT('Ctrl Pts',(-22.8902771664205,3.75368351489473,3.20058718340981));
#84148=CARTESIAN_POINT('Ctrl Pts',(-22.8112956441818,2.70133600728855,4.43471423388053));
#84149=CARTESIAN_POINT('Ctrl Pts',(-22.7323141219432,0.980174239779238,
5.0994232091914));
#84150=CARTESIAN_POINT('Ctrl Pts',(-22.6533325997046,-0.628783080097548,
4.89276602692514));
#84151=CARTESIAN_POINT('Ctrl Pts',(-22.5743510774659,-2.23774039997434,
4.68610884465887));
#84152=CARTESIAN_POINT('Ctrl Pts',(-22.4953695552273,-3.73449327221861,
3.60808550481548));
#84153=CARTESIAN_POINT('Ctrl Pts',(-22.4163880329886,-4.44072222040884,
2.147775994752));
#84154=CARTESIAN_POINT('Ctrl Pts',(-22.3805391972936,-4.76127169589553,
1.48495772781659));
#84155=CARTESIAN_POINT('Ctrl Pts',(-22.3446903615986,-4.91896128463458,
0.743382726906644));
#84156=CARTESIAN_POINT('Ctrl Pts',(-22.3088415259036,-4.91734906814233,
0.00115834211832263));
#84157=CARTESIAN_POINT('Origin',(-12.,0.,0.));
#84158=CARTESIAN_POINT('',(-20.5911584740964,-4.92589392880443,-0.00432496190080733));
#84159=CARTESIAN_POINT('',(-20.8088415259036,-4.92585352153195,-0.00432860929833674));
#84160=CARTESIAN_POINT('',(-12.,-4.925,-6.03138548580071E-16));
#84161=CARTESIAN_POINT('Ctrl Pts',(-20.5911584740964,-4.92589392880443,
-0.00432496190080733));
#84162=CARTESIAN_POINT('Ctrl Pts',(-20.6531832285869,-4.91428084654241,
1.27427360734497));
#84163=CARTESIAN_POINT('Ctrl Pts',(-20.7152079830775,-4.40421217229855,
2.56109016084293));
#84164=CARTESIAN_POINT('Ctrl Pts',(-20.777232737568,-3.50886170650261,3.46719945285304));
#84165=CARTESIAN_POINT('Ctrl Pts',(-20.8562142598067,-2.36873397352748,
4.62102733633866));
#84166=CARTESIAN_POINT('Ctrl Pts',(-20.9351957820453,-0.603866149587261,
5.1575327966315));
#84167=CARTESIAN_POINT('Ctrl Pts',(-21.0141773042839,0.985531967041327,
4.83345759281197));
#84168=CARTESIAN_POINT('Ctrl Pts',(-21.0931588265226,2.57493008366992,4.50938238899243));
#84169=CARTESIAN_POINT('Ctrl Pts',(-21.1721403487612,3.98885849298689,3.3247265210605));
#84170=CARTESIAN_POINT('Ctrl Pts',(-21.2511218709998,4.58622424309187,1.81662748812464));
#84171=CARTESIAN_POINT('Ctrl Pts',(-21.3301033932385,5.18358999319685,0.308528455188798));
#84172=CARTESIAN_POINT('Ctrl Pts',(-21.4090849154771,4.96439308408986,-1.52301374275097));
#84173=CARTESIAN_POINT('Ctrl Pts',(-21.4880664377157,4.0280236561071,-2.84755980093255));
#84174=CARTESIAN_POINT('Ctrl Pts',(-21.5670479599544,3.09165422812432,-4.17210585911414));
#84175=CARTESIAN_POINT('Ctrl Pts',(-21.646029482193,1.43811228126576,-4.98965577753752));
#84176=CARTESIAN_POINT('Ctrl Pts',(-21.7250110044317,-0.18287507021828,
-4.92951859654145));
#84177=CARTESIAN_POINT('Ctrl Pts',(-21.8039925266703,-1.80386242170232,
-4.86938141554538));
#84178=CARTESIAN_POINT('Ctrl Pts',(-21.8829740489089,-3.39229517781185,
-3.93155713512985));
#84179=CARTESIAN_POINT('Ctrl Pts',(-21.9619555711476,-4.22794608586075,
-2.54127476392983));
#84180=CARTESIAN_POINT('Ctrl Pts',(-22.0050232054638,-4.68361605402348,
-1.78317120929954));
#84181=CARTESIAN_POINT('Ctrl Pts',(-22.0480908397801,-4.91545505442897,
-0.89053447936648));
#84182=CARTESIAN_POINT('Ctrl Pts',(-22.0911584740964,-4.91737544826784,
0.00117139545793843));
#84183=CARTESIAN_POINT('Ctrl Pts',(-22.3088415259036,-4.91734906814233,
0.00115834211832263));
#84184=CARTESIAN_POINT('Ctrl Pts',(-22.26570883936,-4.91540927770695,-0.891872940863008));
#84185=CARTESIAN_POINT('Ctrl Pts',(-22.2225761528164,-4.68285658280413,
-1.78584430297331));
#84186=CARTESIAN_POINT('Ctrl Pts',(-22.1794434662727,-4.22588839382535,
-2.54470959099318));
#84187=CARTESIAN_POINT('Ctrl Pts',(-22.1004619440341,-3.38912059491543,
-3.93428998639135));
#84188=CARTESIAN_POINT('Ctrl Pts',(-22.0214804217955,-1.79987997295941,
-4.87085509690416));
#84189=CARTESIAN_POINT('Ctrl Pts',(-21.9424988995568,-0.178834088830268,
-4.92967666338373));
#84190=CARTESIAN_POINT('Ctrl Pts',(-21.8635173773182,1.44221179529888,-4.98849822986331));
#84191=CARTESIAN_POINT('Ctrl Pts',(-21.7845358550796,3.09506294160113,-4.16957625230965));
#84192=CARTESIAN_POINT('Ctrl Pts',(-21.7055543328409,4.03034398306194,-2.84426032790294));
#84193=CARTESIAN_POINT('Ctrl Pts',(-21.6265728106023,4.96562502452275,-1.51894440349625));
#84194=CARTESIAN_POINT('Ctrl Pts',(-21.5475912883637,5.18333596114214,0.312765467763498));
#84195=CARTESIAN_POINT('Ctrl Pts',(-21.468609766125,4.5847403503353,1.82037297348421));
#84196=CARTESIAN_POINT('Ctrl Pts',(-21.3896282438864,3.98614473952846,3.32798047920493));
#84197=CARTESIAN_POINT('Ctrl Pts',(-21.3106467216477,2.57124258129539,4.51148561938661));
#84198=CARTESIAN_POINT('Ctrl Pts',(-21.2316651994091,0.981578778726861,
4.83426274757768));
#84199=CARTESIAN_POINT('Ctrl Pts',(-21.1526836771705,-0.608085023841661,
5.15703987576876));
#84200=CARTESIAN_POINT('Ctrl Pts',(-21.0737021549319,-2.37251047074563,
4.61908899196923));
#84201=CARTESIAN_POINT('Ctrl Pts',(-20.9947206326932,-3.51169377874649,
3.46432886221565));
#84202=CARTESIAN_POINT('Ctrl Pts',(-20.93276093043,-4.40536430555249,2.55843857551328));
#84203=CARTESIAN_POINT('Ctrl Pts',(-20.8708012281668,-4.91425182481639,
1.27295500491239));
#84204=CARTESIAN_POINT('Ctrl Pts',(-20.8088415259036,-4.92585352153195,
-0.00432860929833674));
#84205=CARTESIAN_POINT('Origin',(-12.,0.,0.));
#84206=CARTESIAN_POINT('',(-19.0911584740964,-4.93036753939865,0.00306120389312589));
#84207=CARTESIAN_POINT('',(-19.3088415259036,-4.93039896058852,0.00304429332654976));
#84208=CARTESIAN_POINT('',(-12.,-4.925,-6.03138548580071E-16));
#84209=CARTESIAN_POINT('Ctrl Pts',(-19.0911584740964,-4.93036753939865,
0.00306120389312589));
#84210=CARTESIAN_POINT('Ctrl Pts',(-19.1003125729165,-4.93174437091004,
0.191322718640612));
#84211=CARTESIAN_POINT('Ctrl Pts',(-19.1094666717366,-4.92188543239957,
0.379438718776696));
#84212=CARTESIAN_POINT('Ctrl Pts',(-19.1186207705567,-4.90030624508457,
0.56620051557689));
#84213=CARTESIAN_POINT('Ctrl Pts',(-19.1976022927953,-4.71412111683668,
2.17758043371112));
#84214=CARTESIAN_POINT('Ctrl Pts',(-19.2765838150339,-3.65545366284497,
3.68815033528921));
#84215=CARTESIAN_POINT('Ctrl Pts',(-19.3555653372726,-2.20431556954579,
4.41300092242343));
#84216=CARTESIAN_POINT('Ctrl Pts',(-19.4345468595112,-0.753177476246607,
5.13785150955766));
#84217=CARTESIAN_POINT('Ctrl Pts',(-19.5135283817499,1.09043125636005,5.07698278224803));
#84218=CARTESIAN_POINT('Ctrl Pts',(-19.5925099039885,2.49059780960012,4.25799328980927));
#84219=CARTESIAN_POINT('Ctrl Pts',(-19.6714914262271,3.89076436284019,3.43900379737051));
#84220=CARTESIAN_POINT('Ctrl Pts',(-19.7504729484657,4.84748873671366,1.86189353980263));
#84221=CARTESIAN_POINT('Ctrl Pts',(-19.8294544707044,4.92698134988234,0.241741989311494));
#84222=CARTESIAN_POINT('Ctrl Pts',(-19.908435992943,5.00647396305102,-1.37840956117965));
#84223=CARTESIAN_POINT('Ctrl Pts',(-19.9874175151817,4.20873481551489,-3.04160240459405));
#84224=CARTESIAN_POINT('Ctrl Pts',(-20.0663990374203,2.89546784338567,-3.99372633407541));
#84225=CARTESIAN_POINT('Ctrl Pts',(-20.1453805596589,1.58220087125645,-4.94585026355678));
#84226=CARTESIAN_POINT('Ctrl Pts',(-20.2243620818976,-0.246593925465854,
-5.18690527910513));
#84227=CARTESIAN_POINT('Ctrl Pts',(-20.3033436041362,-1.76172065737862,
-4.60759424510195));
#84228=CARTESIAN_POINT('Ctrl Pts',(-20.3823251263748,-3.27684738929139,
-4.02828321109877));
#84229=CARTESIAN_POINT('Ctrl Pts',(-20.4613066486135,-4.47830605639462,
-2.62860612754407));
#84230=CARTESIAN_POINT('Ctrl Pts',(-20.5402881708521,-4.82134156894121,
-1.04319243242752));
#84231=CARTESIAN_POINT('Ctrl Pts',(-20.5572449386002,-4.89498883922333,
-0.702815454993217));
#84232=CARTESIAN_POINT('Ctrl Pts',(-20.5742017063483,-4.92906879568418,
-0.353877316599127));
#84233=CARTESIAN_POINT('Ctrl Pts',(-20.5911584740964,-4.92589392880443,
-0.00432496190080733));
#84234=CARTESIAN_POINT('Ctrl Pts',(-20.8088415259036,-4.92585352153195,
-0.00432860929833674));
#84235=CARTESIAN_POINT('Ctrl Pts',(-20.7918197059282,-4.92904078657178,
-0.355229129225151));
#84236=CARTESIAN_POINT('Ctrl Pts',(-20.7747978859527,-4.89469624934525,
-0.705510771380119));
#84237=CARTESIAN_POINT('Ctrl Pts',(-20.7577760659773,-4.82048723932594,
-1.04713290262958));
#84238=CARTESIAN_POINT('Ctrl Pts',(-20.6787945437387,-4.4761562228068,-2.63226516201363));
#84239=CARTESIAN_POINT('Ctrl Pts',(-20.5998130215,-3.27355302067076,-4.03096030507408));
#84240=CARTESIAN_POINT('Ctrl Pts',(-20.5208314992614,-1.75795314101832,
-4.60903271986277));
#84241=CARTESIAN_POINT('Ctrl Pts',(-20.4418499770228,-0.242353261365892,
-5.18710513465145));
#84242=CARTESIAN_POINT('Ctrl Pts',(-20.3628684547841,1.58624329580292,-4.94455482116838));
#84243=CARTESIAN_POINT('Ctrl Pts',(-20.2838869325455,2.89873129214139,-3.99135762699838));
#84244=CARTESIAN_POINT('Ctrl Pts',(-20.2049054103069,4.21121928847986,-3.03816043282837));
#84245=CARTESIAN_POINT('Ctrl Pts',(-20.1259238880682,5.00759872398798,-1.37431635797142));
#84246=CARTESIAN_POINT('Ctrl Pts',(-20.0469423658296,4.92678177190102,0.24576949363086));
#84247=CARTESIAN_POINT('Ctrl Pts',(-19.9679608435909,4.84596481981407,1.86585534523313));
#84248=CARTESIAN_POINT('Ctrl Pts',(-19.8889793213523,3.88795148013202,3.44218297358073));
#84249=CARTESIAN_POINT('Ctrl Pts',(-19.8099977991137,2.48711597359967,4.26002756225397));
#84250=CARTESIAN_POINT('Ctrl Pts',(-19.731016276875,1.08628046706732,5.0778721509272));
#84251=CARTESIAN_POINT('Ctrl Pts',(-19.6520347546364,-0.757377206315341,
5.13723369992608));
#84252=CARTESIAN_POINT('Ctrl Pts',(-19.5730532323978,-2.20792214579921,
4.41119713404449));
#84253=CARTESIAN_POINT('Ctrl Pts',(-19.4940717101591,-3.65846708528308,
3.6851605681629));
#84254=CARTESIAN_POINT('Ctrl Pts',(-19.4150901879205,-4.71589929086815,
2.17372588740081));
#84255=CARTESIAN_POINT('Ctrl Pts',(-19.3361086656819,-4.90076709523542,
0.562194436802809));
#84256=CARTESIAN_POINT('Ctrl Pts',(-19.3270196190891,-4.92204133811868,
0.376742396565921));
#84257=CARTESIAN_POINT('Ctrl Pts',(-19.3179305724964,-4.93176022977169,
0.18996477700119));
#84258=CARTESIAN_POINT('Ctrl Pts',(-19.3088415259036,-4.93039896058852,
0.00304429332654976));
#84259=CARTESIAN_POINT('Origin',(-12.,0.,0.));
#84260=CARTESIAN_POINT('',(-17.5911584740964,-4.91748734336217,0.00138246325145752));
#84261=CARTESIAN_POINT('',(-17.8088415259036,-4.91749844770123,0.00140301643559147));
#84262=CARTESIAN_POINT('',(-12.,-4.925,-6.03138548580071E-16));
#84263=CARTESIAN_POINT('Ctrl Pts',(-17.5911584740964,-4.91748734336217,
0.00138246325145752));
#84264=CARTESIAN_POINT('Ctrl Pts',(-17.6264234394847,-4.9193418852286,0.731498546199545));
#84265=CARTESIAN_POINT('Ctrl Pts',(-17.661688404873,-4.76696687445272,1.46087872121623));
#84266=CARTESIAN_POINT('Ctrl Pts',(-17.6969533702612,-4.45641077730308,
2.11518020197493));
#84267=CARTESIAN_POINT('Ctrl Pts',(-17.7759348924999,-3.76087079808261,
3.58059286818176));
#84268=CARTESIAN_POINT('Ctrl Pts',(-17.8549164147385,-2.27188252680849,
4.66940512599426));
#84269=CARTESIAN_POINT('Ctrl Pts',(-17.9338979369771,-0.664569915601229,
4.88793730824473));
#84270=CARTESIAN_POINT('Ctrl Pts',(-18.0128794592158,0.942742695606023,
5.1064694904952));
#84271=CARTESIAN_POINT('Ctrl Pts',(-18.0918609814544,2.66837964674642,4.45472159718366));
#84272=CARTESIAN_POINT('Ctrl Pts',(-18.170842503693,3.72991782550763,3.22820341940916));
#84273=CARTESIAN_POINT('Ctrl Pts',(-18.2498240259317,4.79145600426884,2.00168524163466));
#84274=CARTESIAN_POINT('Ctrl Pts',(-18.3288055481703,5.18889541065087,0.200396779397185));
#84275=CARTESIAN_POINT('Ctrl Pts',(-18.407787070409,4.74203256755282,-1.3589376120088));
#84276=CARTESIAN_POINT('Ctrl Pts',(-18.4867685926476,4.29516972445477,-2.91827200341478));
#84277=CARTESIAN_POINT('Ctrl Pts',(-18.5657501148862,3.00400463187666,-4.23565232398927));
#84278=CARTESIAN_POINT('Ctrl Pts',(-18.6447316371249,1.45396599931439,-4.7137635888389));
#84279=CARTESIAN_POINT('Ctrl Pts',(-18.7237131593635,-0.096072633247862,
-5.19187485368853));
#84280=CARTESIAN_POINT('Ctrl Pts',(-18.8026946816021,-1.90498480579426,
-4.8307170628133));
#84281=CARTESIAN_POINT('Ctrl Pts',(-18.8816762038408,-3.15258949081541,
-3.79404320003051));
#84282=CARTESIAN_POINT('Ctrl Pts',(-18.9515036272593,-4.25559457517833,
-2.87752168067103));
#84283=CARTESIAN_POINT('Ctrl Pts',(-19.0213310506779,-4.91986507500412,
-1.43299675899955));
#84284=CARTESIAN_POINT('Ctrl Pts',(-19.0911584740964,-4.93036753939865,
0.00306120389312589));
#84285=CARTESIAN_POINT('Ctrl Pts',(-19.3088415259036,-4.93039896058852,
0.00304429332654976));
#84286=CARTESIAN_POINT('Ctrl Pts',(-19.2389490502577,-4.91993114394113,
-1.43432707666567));
#84287=CARTESIAN_POINT('Ctrl Pts',(-19.1690565746118,-4.2542688128935,-2.88014631871502));
#84288=CARTESIAN_POINT('Ctrl Pts',(-19.099164098966,-3.14948667556652,-3.79661879576485));
#84289=CARTESIAN_POINT('Ctrl Pts',(-19.0201825767273,-1.90103504838086,
-4.83227235730055));
#84290=CARTESIAN_POINT('Ctrl Pts',(-18.9412010544887,-0.0918283908600531,
-5.19195125993805));
#84291=CARTESIAN_POINT('Ctrl Pts',(-18.86221953225,1.45781876197131,-4.71257307881752));
#84292=CARTESIAN_POINT('Ctrl Pts',(-18.7832380100114,3.00746591480269,-4.23319489769699));
#84293=CARTESIAN_POINT('Ctrl Pts',(-18.7042564877728,4.29755356294462,-2.91475963281842));
#84294=CARTESIAN_POINT('Ctrl Pts',(-18.6252749655341,4.74314151432189,-1.35506058509819));
#84295=CARTESIAN_POINT('Ctrl Pts',(-18.5462934432955,5.18872946569916,0.204638462622037));
#84296=CARTESIAN_POINT('Ctrl Pts',(-18.4673119210569,4.78981772031176,2.00560129318392));
#84297=CARTESIAN_POINT('Ctrl Pts',(-18.3883303988182,3.72727733438716,3.23125119241768));
#84298=CARTESIAN_POINT('Ctrl Pts',(-18.3093488765796,2.66473694846256,4.45690109165143));
#84299=CARTESIAN_POINT('Ctrl Pts',(-18.230367354341,0.93856792200078,5.10723805955708));
#84300=CARTESIAN_POINT('Ctrl Pts',(-18.1513858321023,-0.668565385932749,
4.88739203645243));
#84301=CARTESIAN_POINT('Ctrl Pts',(-18.0724043098637,-2.27569869386628,
4.66754601334778));
#84302=CARTESIAN_POINT('Ctrl Pts',(-17.9934227876251,-3.76379628327154,
3.57751699923284));
#84303=CARTESIAN_POINT('Ctrl Pts',(-17.9144412653864,-4.45813804603734,
2.11153635114173));
#84304=CARTESIAN_POINT('Ctrl Pts',(-17.8792413522255,-4.76758725720248,
1.45818870670777));
#84305=CARTESIAN_POINT('Ctrl Pts',(-17.8440414390645,-4.91937734376141,
0.73016796568955));
#84306=CARTESIAN_POINT('Ctrl Pts',(-17.8088415259036,-4.91749844770123,
0.00140301643559147));
#84307=CARTESIAN_POINT('Origin',(-12.,0.,0.));
#84308=CARTESIAN_POINT('',(-16.0911584740964,-4.92549411112511,-0.00435654742202807));
#84309=CARTESIAN_POINT('',(-16.3088415259036,-4.92545367141813,-0.00435907189217228));
#84310=CARTESIAN_POINT('',(-12.,-4.925,-6.03138548580071E-16));
#84311=CARTESIAN_POINT('Ctrl Pts',(-16.0911584740964,-4.92549411112511,
-0.00435654742202807));
#84312=CARTESIAN_POINT('Ctrl Pts',(-16.1525343060529,-4.91401305180791,
1.26112872196585));
#84313=CARTESIAN_POINT('Ctrl Pts',(-16.2139101380093,-4.41566061870666,
2.53464705245624));
#84314=CARTESIAN_POINT('Ctrl Pts',(-16.2752859699658,-3.53701851325257,
3.43847122126015));
#84315=CARTESIAN_POINT('Ctrl Pts',(-16.3542674922044,-2.40633744906825,
4.60155783715884));
#84316=CARTESIAN_POINT('Ctrl Pts',(-16.4332490144431,-0.64590265744457,
5.15243672494805));
#84317=CARTESIAN_POINT('Ctrl Pts',(-16.5122305366817,0.946085018446281,
4.84133322963671));
#84318=CARTESIAN_POINT('Ctrl Pts',(-16.5912120589203,2.53807269433713,4.53022973432537));
#84319=CARTESIAN_POINT('Ctrl Pts',(-16.670193581159,3.96161325449515,3.3571438559135));
#84320=CARTESIAN_POINT('Ctrl Pts',(-16.7491751033976,4.57125747194857,1.85396586474963));
#84321=CARTESIAN_POINT('Ctrl Pts',(-16.8281566256362,5.18090168940199,0.350787873585757));
#84322=CARTESIAN_POINT('Ctrl Pts',(-16.9071381478749,4.97664956415081,-1.4824822303301));
#84323=CARTESIAN_POINT('Ctrl Pts',(-16.9861196701135,4.05111129643801,-2.81461925781151));
#84324=CARTESIAN_POINT('Ctrl Pts',(-17.0651011923521,3.12557302872522,-4.14675628529291));
#84325=CARTESIAN_POINT('Ctrl Pts',(-17.1440827145908,1.47874861855081,-4.97776023633987));
#84326=CARTESIAN_POINT('Ctrl Pts',(-17.2230642368294,-0.142673309742003,
-4.93084461620456));
#84327=CARTESIAN_POINT('Ctrl Pts',(-17.3020457590681,-1.76409523803482,
-4.88392899606925));
#84328=CARTESIAN_POINT('Ctrl Pts',(-17.3810272813067,-3.36011468444605,
-3.95909380475167));
#84329=CARTESIAN_POINT('Ctrl Pts',(-17.4600088035453,-4.20707856406823,
-2.57566967179231));
#84330=CARTESIAN_POINT('Ctrl Pts',(-17.5037253603957,-4.67587612005653,
-1.8099394346116));
#84331=CARTESIAN_POINT('Ctrl Pts',(-17.5474419172461,-4.91518834252542,
-0.903713030141044));
#84332=CARTESIAN_POINT('Ctrl Pts',(-17.5911584740964,-4.91748734336217,
0.00138246325145752));
#84333=CARTESIAN_POINT('Ctrl Pts',(-17.8088415259036,-4.91749844770123,
0.00140301643559147));
#84334=CARTESIAN_POINT('Ctrl Pts',(-17.7650599168259,-4.91516147907213,
-0.905033939016169));
#84335=CARTESIAN_POINT('Ctrl Pts',(-17.7212783077482,-4.67509315331331,
-1.81262221095911));
#84336=CARTESIAN_POINT('Ctrl Pts',(-17.6774966986705,-4.20497130464389,
-2.57910777670998));
#84337=CARTESIAN_POINT('Ctrl Pts',(-17.5985151764319,-3.35687686435833,
-3.96183897440324));
#84338=CARTESIAN_POINT('Ctrl Pts',(-17.5195336541932,-1.76010204766094,
-4.88536908772247));
#84339=CARTESIAN_POINT('Ctrl Pts',(-17.4405521319546,-0.138642432499522,
-4.93095922439053));
#84340=CARTESIAN_POINT('Ctrl Pts',(-17.361570609716,1.48281718266189,-4.9765493610586));
#84341=CARTESIAN_POINT('Ctrl Pts',(-17.2825890874773,3.1289615962873,-4.14419952107549));
#84342=CARTESIAN_POINT('Ctrl Pts',(-17.2036075652387,4.05341050192337,-2.81130644015036));
#84343=CARTESIAN_POINT('Ctrl Pts',(-17.1246260430001,4.97785940755944,-1.47841335922522));
#84344=CARTESIAN_POINT('Ctrl Pts',(-17.0456445207614,5.18061280520616,0.355022962641952));
#84345=CARTESIAN_POINT('Ctrl Pts',(-16.9666629985228,4.56974003457753,1.85770197110664));
#84346=CARTESIAN_POINT('Ctrl Pts',(-16.8876814762842,3.9588672639489,3.36038097957132));
#84347=CARTESIAN_POINT('Ctrl Pts',(-16.8086999540455,2.53436832504492,4.53230267463353));
#84348=CARTESIAN_POINT('Ctrl Pts',(-16.7297184318069,0.942126984447272,
4.8421046397495));
#84349=CARTESIAN_POINT('Ctrl Pts',(-16.6507369095683,-0.65011435615038,
5.15190660486548));
#84350=CARTESIAN_POINT('Ctrl Pts',(-16.5717553873296,-2.41009809844172,
4.59958884003522));
#84351=CARTESIAN_POINT('Ctrl Pts',(-16.492773865091,-3.53982791004914,3.43557840318775));
#84352=CARTESIAN_POINT('Ctrl Pts',(-16.4314630853618,-4.41680031662811,
2.53199506529855));
#84353=CARTESIAN_POINT('Ctrl Pts',(-16.3701523056327,-4.91398734347909,
1.25981119608574));
#84354=CARTESIAN_POINT('Ctrl Pts',(-16.3088415259036,-4.92545367141813,
-0.00435907189217227));
#84355=CARTESIAN_POINT('Origin',(-12.,0.,0.));
#84356=CARTESIAN_POINT('',(-14.5911584740964,-4.93067827447104,0.00288827060414214));
#84357=CARTESIAN_POINT('',(-14.8088415259036,-4.93070824935115,0.00287043364757822));
#84358=CARTESIAN_POINT('',(-12.,-4.925,-6.03138548580071E-16));
#84359=CARTESIAN_POINT('Ctrl Pts',(-14.5911584740964,-4.93067827447104,
0.00288827060414214));
#84360=CARTESIAN_POINT('Ctrl Pts',(-14.5996636503824,-4.93190134523225,
0.177775193398353));
#84361=CARTESIAN_POINT('Ctrl Pts',(-14.6081688266684,-4.92339421157364,
0.352541876964962));
#84362=CARTESIAN_POINT('Ctrl Pts',(-14.6166740029544,-4.90476040342235,
0.526222089557762));
#84363=CARTESIAN_POINT('Ctrl Pts',(-14.6956555251931,-4.731721481782,2.1390666811365));
#84364=CARTESIAN_POINT('Ctrl Pts',(-14.7746370474317,-3.68540719144605,
3.65821927729102));
#84365=CARTESIAN_POINT('Ctrl Pts',(-14.8536185696703,-2.24022814548496,
4.39487908351248));
#84366=CARTESIAN_POINT('Ctrl Pts',(-14.932600091909,-0.795049099523871,
5.13153888973394));
#84367=CARTESIAN_POINT('Ctrl Pts',(-15.0115816141476,1.04899470206234,5.08570590602234));
#84368=CARTESIAN_POINT('Ctrl Pts',(-15.0905631363863,2.45579315495828,4.27816132030787));
#84369=CARTESIAN_POINT('Ctrl Pts',(-15.1695446586249,3.86259160785421,3.47061673459341));
#84370=CARTESIAN_POINT('Ctrl Pts',(-15.2485261808635,4.83214471205985,1.90136054687609));
#84371=CARTESIAN_POINT('Ctrl Pts',(-15.3275077031022,4.92484623566303,0.281911081005368));
#84372=CARTESIAN_POINT('Ctrl Pts',(-15.4064892253408,5.0175477592662,-1.33753838486535));
#84373=CARTESIAN_POINT('Ctrl Pts',(-15.4854707475794,4.23339770226691,-3.00718112888947));
#84374=CARTESIAN_POINT('Ctrl Pts',(-15.5644522698181,2.9279384793258,-3.96998243872724));
#84375=CARTESIAN_POINT('Ctrl Pts',(-15.6434337920567,1.62247925638469,-4.93278374856501));
#84376=CARTESIAN_POINT('Ctrl Pts',(-15.7224153142953,-0.204289132498227,
-5.18874362421643));
#84377=CARTESIAN_POINT('Ctrl Pts',(-15.801396836534,-1.72408944853063,-4.62180699250664));
#84378=CARTESIAN_POINT('Ctrl Pts',(-15.8803783587726,-3.24388976456301,
-4.05487036079686));
#84379=CARTESIAN_POINT('Ctrl Pts',(-15.9593598810112,-4.45672200774489,
-2.66503722172589));
#84380=CARTESIAN_POINT('Ctrl Pts',(-16.0383414032499,-4.81267446096336,
-1.08247348018632));
#84381=CARTESIAN_POINT('Ctrl Pts',(-16.0559470935321,-4.89201945798192,
-0.729705816362758));
#84382=CARTESIAN_POINT('Ctrl Pts',(-16.0735527838142,-4.92878745914186,
-0.367361674999108));
#84383=CARTESIAN_POINT('Ctrl Pts',(-16.0911584740964,-4.92549411112511,
-0.00435654742202807));
#84384=CARTESIAN_POINT('Ctrl Pts',(-16.3088415259036,-4.92545367141813,
-0.00435907189217227));
#84385=CARTESIAN_POINT('Ctrl Pts',(-16.2911707833941,-4.92875844962247,
-0.3687130630225));
#84386=CARTESIAN_POINT('Ctrl Pts',(-16.2735000408846,-4.89171517974735,
-0.732401377008249));
#84387=CARTESIAN_POINT('Ctrl Pts',(-16.2558292983751,-4.81178759662622,
-1.08640725425502));
#84388=CARTESIAN_POINT('Ctrl Pts',(-16.1768477761364,-4.45454159067236,
-2.66867936598564));
#84389=CARTESIAN_POINT('Ctrl Pts',(-16.0978662538978,-3.24057369784111,
-4.05752048058219));
#84390=CARTESIAN_POINT('Ctrl Pts',(-16.0188847316592,-1.72031055150433,
-4.62321448816053));
#84391=CARTESIAN_POINT('Ctrl Pts',(-15.9399032094205,-0.200047405167556,
-5.18890849573887));
#84392=CARTESIAN_POINT('Ctrl Pts',(-15.8609216871819,1.62651099467473,-4.931455396299));
#84393=CARTESIAN_POINT('Ctrl Pts',(-15.7819401649433,2.93118262060901,-3.96758730739563));
#84394=CARTESIAN_POINT('Ctrl Pts',(-15.7029586427046,4.23585424654329,-3.00371921849225));
#84395=CARTESIAN_POINT('Ctrl Pts',(-15.623977120466,5.01863909856954,-1.33343614012536));
#84396=CARTESIAN_POINT('Ctrl Pts',(-15.5449955982273,4.92461376124743,0.285936880603985));
#84397=CARTESIAN_POINT('Ctrl Pts',(-15.4660140759887,4.83058842392532,1.90530990133333));
#84398=CARTESIAN_POINT('Ctrl Pts',(-15.3870325537501,3.85975289725486,3.47377286442513));
#84399=CARTESIAN_POINT('Ctrl Pts',(-15.3080510315114,2.45229487785007,4.28016710295635));
#84400=CARTESIAN_POINT('Ctrl Pts',(-15.2290695092728,1.04483685844527,5.08656134148757));
#84401=CARTESIAN_POINT('Ctrl Pts',(-15.1500879870342,-0.799243653693828,
5.13088685545821));
#84402=CARTESIAN_POINT('Ctrl Pts',(-15.0711064647955,-2.24381990927576,
4.39304596059483));
#84403=CARTESIAN_POINT('Ctrl Pts',(-14.9921249425569,-3.68839616485769,
3.65520506573145));
#84404=CARTESIAN_POINT('Ctrl Pts',(-14.9131434203183,-4.73346816388242,
2.13519776203403));
#84405=CARTESIAN_POINT('Ctrl Pts',(-14.8341618980796,-4.90518856206808,
0.522212377980333));
#84406=CARTESIAN_POINT('Ctrl Pts',(-14.825721774021,-4.92353894862701,0.349845521019683));
#84407=CARTESIAN_POINT('Ctrl Pts',(-14.8172816499623,-4.9319161064083,0.17641690191672));
#84408=CARTESIAN_POINT('Ctrl Pts',(-14.8088415259036,-4.93070824935115,
0.00287043364757822));
#84409=CARTESIAN_POINT('Origin',(-12.,0.,0.));
#84410=CARTESIAN_POINT('',(-13.0911584740964,-4.91760946231994,0.00158594389483818));
#84411=CARTESIAN_POINT('',(-13.3088415259036,-4.91762225934298,0.00160614365327011));
#84412=CARTESIAN_POINT('',(-12.,-4.925,-6.03138548580071E-16));
#84413=CARTESIAN_POINT('Ctrl Pts',(-13.0911584740964,-4.91760946231994,
0.00158594389483818));
#84414=CARTESIAN_POINT('Ctrl Pts',(-13.1257745169506,-4.91970084079515,
0.718222392324636));
#84415=CARTESIAN_POINT('Ctrl Pts',(-13.1603905598048,-4.77310485360014,
1.43404408902173));
#84416=CARTESIAN_POINT('Ctrl Pts',(-13.195006602659,-4.47351086752437,2.07877002591911));
#84417=CARTESIAN_POINT('Ctrl Pts',(-13.2739881248976,-3.78994373729305,
3.54980575745473));
#84418=CARTESIAN_POINT('Ctrl Pts',(-13.3529696471363,-2.30988370406987,
4.65072378465739));
#84419=CARTESIAN_POINT('Ctrl Pts',(-13.4319511693749,-0.704406556676555,
4.88235554885441));
#84420=CARTESIAN_POINT('Ctrl Pts',(-13.5109326916135,0.901070590716762,
5.11398731305142));
#84421=CARTESIAN_POINT('Ctrl Pts',(-13.5899142138522,2.63196485228022,4.47633281424283));
#84422=CARTESIAN_POINT('Ctrl Pts',(-13.6688957360908,3.70346939189113,3.25851174094001));
#84423=CARTESIAN_POINT('Ctrl Pts',(-13.7478772583294,4.77497393150204,2.04069066763719));
#84424=CARTESIAN_POINT('Ctrl Pts',(-13.8268587805681,5.18708874916036,0.242703019840158));
#84425=CARTESIAN_POINT('Ctrl Pts',(-13.9058403028067,4.75295637277905,-1.32022347387755));
#84426=CARTESIAN_POINT('Ctrl Pts',(-13.9848218250454,4.31882399639775,-2.88314996759526));
#84427=CARTESIAN_POINT('Ctrl Pts',(-14.063803347284,3.03844442597681,-4.21101530723365));
#84428=CARTESIAN_POINT('Ctrl Pts',(-14.1427848695226,1.49235609301499,-4.70175048191197));
#84429=CARTESIAN_POINT('Ctrl Pts',(-14.2217663917613,-0.0537322399468088,
-5.19248565659028));
#84430=CARTESIAN_POINT('Ctrl Pts',(-14.3007479139999,-1.86552933544948,
-4.84609066630856));
#84431=CARTESIAN_POINT('Ctrl Pts',(-14.3797294362385,-3.12154610672844,
-3.81962487766624));
#84432=CARTESIAN_POINT('Ctrl Pts',(-14.4502057821912,-4.24230789994266,
-2.90369472111239));
#84433=CARTESIAN_POINT('Ctrl Pts',(-14.5206821281438,-4.92054355707158,
-1.44627525745988));
#84434=CARTESIAN_POINT('Ctrl Pts',(-14.5911584740964,-4.93067827447104,
0.00288827060414214));
#84435=CARTESIAN_POINT('Ctrl Pts',(-14.8088415259036,-4.93070824935115,
0.00287043364757822));
#84436=CARTESIAN_POINT('Ctrl Pts',(-14.7383001277236,-4.92061314588811,
-1.44760712281891));
#84437=CARTESIAN_POINT('Ctrl Pts',(-14.6677587295437,-4.24096766997707,
-2.90631689952062));
#84438=CARTESIAN_POINT('Ctrl Pts',(-14.5972173313637,-3.11842239638253,
-3.82217508166485));
#84439=CARTESIAN_POINT('Ctrl Pts',(-14.5182358091251,-1.86156703516476,
-4.84761369284634));
#84440=CARTESIAN_POINT('Ctrl Pts',(-14.4392542868864,-0.0494875153826427,
-5.19252745079936));
#84441=CARTESIAN_POINT('Ctrl Pts',(-14.3602727646478,1.49619902186904,-4.70052859624512));
#84442=CARTESIAN_POINT('Ctrl Pts',(-14.2812912424092,3.04188555912074,-4.20852974169087));
#84443=CARTESIAN_POINT('Ctrl Pts',(-14.2023097201705,4.321179113842,-2.87961827462935));
#84444=CARTESIAN_POINT('Ctrl Pts',(-14.1233281979319,4.75403366621063,-1.31633753182672));
#84445=CARTESIAN_POINT('Ctrl Pts',(-14.0443466756933,5.18688821857927,0.246943210975917));
#84446=CARTESIAN_POINT('Ctrl Pts',(-13.9653651534546,4.77330376859529,2.04459322951967));
#84447=CARTESIAN_POINT('Ctrl Pts',(-13.886383631216,3.70080413609518,3.26153788011432));
#84448=CARTESIAN_POINT('Ctrl Pts',(-13.8074021089774,2.62830450359508,4.47848253070897));
#84449=CARTESIAN_POINT('Ctrl Pts',(-13.7284205867387,0.896889688578863,
5.11472181335452));
#84450=CARTESIAN_POINT('Ctrl Pts',(-13.6494390645001,-0.708397448067476,
4.88177771439169));
#84451=CARTESIAN_POINT('Ctrl Pts',(-13.5704575422615,-2.31368458471381,
4.64883361542886));
#84452=CARTESIAN_POINT('Ctrl Pts',(-13.4914760200228,-3.79284404299027,
3.54670613485765));
#84453=CARTESIAN_POINT('Ctrl Pts',(-13.4124944977842,-4.47520836483826,
2.07511221104824));
#84454=CARTESIAN_POINT('Ctrl Pts',(-13.3779435071573,-4.77371316216336,
1.43135369099267));
#84455=CARTESIAN_POINT('Ctrl Pts',(-13.3433925165305,-4.91973662561568,
0.71689100431942));
#84456=CARTESIAN_POINT('Ctrl Pts',(-13.3088415259036,-4.91762225934298,
0.00160614365327011));
#84457=CARTESIAN_POINT('Origin',(-12.,0.,0.));
#84458=CARTESIAN_POINT('',(-11.5911584740964,-4.92509485823308,-0.00437651270843276));
#84459=CARTESIAN_POINT('',(-11.8088415259036,-4.92505452712729,-0.00437787461885928));
#84460=CARTESIAN_POINT('',(-12.,-4.925,-6.03138548580071E-16));
#84461=CARTESIAN_POINT('Ctrl Pts',(-11.5911584740964,-4.92509485823308,
-0.00437651270843276));
#84462=CARTESIAN_POINT('Ctrl Pts',(-11.6518853835188,-4.91377256362929,
1.24798912490446));
#84463=CARTESIAN_POINT('Ctrl Pts',(-11.7126122929412,-4.42697102096967,
2.50818673560203));
#84464=CARTESIAN_POINT('Ctrl Pts',(-11.7733392023636,-3.56493996274647,
3.40951424172587));
#84465=CARTESIAN_POINT('Ctrl Pts',(-11.8523207246022,-2.44378089433587,
4.58178233747355));
#84466=CARTESIAN_POINT('Ctrl Pts',(-11.9313022468408,-0.687896782440381,
5.14699839364787));
#84467=CARTESIAN_POINT('Ctrl Pts',(-12.0102837690794,0.906574858907132,
4.84888712259997));
#84468=CARTESIAN_POINT('Ctrl Pts',(-12.0892652913181,2.50104650025465,4.55077585155208));
#84469=CARTESIAN_POINT('Ctrl Pts',(-12.1682468135567,3.93410567105417,3.38933725328197));
#84470=CARTESIAN_POINT('Ctrl Pts',(-12.2472283357954,4.55598729969703,1.89118059093196));
#84471=CARTESIAN_POINT('Ctrl Pts',(-12.326209858034,5.17786892833988,0.393023928581957));
#84472=CARTESIAN_POINT('Ctrl Pts',(-12.4051913802726,4.98857301482605,-1.44185079784797));
#84473=CARTESIAN_POINT('Ctrl Pts',(-12.4841729025113,4.07392844557266,-2.78149084536912));
#84474=CARTESIAN_POINT('Ctrl Pts',(-12.5631544247499,3.15928387631926,-4.12113089289029));
#84475=CARTESIAN_POINT('Ctrl Pts',(-12.6421359469885,1.51929065132632,-4.96553626150268));
#84476=CARTESIAN_POINT('Ctrl Pts',(-12.7211174692272,-0.102459940931512,
-4.93184410368197));
#84477=CARTESIAN_POINT('Ctrl Pts',(-12.8000989914658,-1.7242105331893,-4.89815194586127));
#84478=CARTESIAN_POINT('Ctrl Pts',(-12.8790805137045,-3.32771849271198,
-3.98636226160747));
#84479=CARTESIAN_POINT('Ctrl Pts',(-12.9580620359431,-4.18593535885357,
-2.6098907015463));
#84480=CARTESIAN_POINT('Ctrl Pts',(-13.0024275153275,-4.66801270559229,
-1.83669946782132));
#84481=CARTESIAN_POINT('Ctrl Pts',(-13.046792994712,-4.91492905748518,-0.916887600665788));
#84482=CARTESIAN_POINT('Ctrl Pts',(-13.0911584740964,-4.91760946231994,
0.00158594389483818));
#84483=CARTESIAN_POINT('Ctrl Pts',(-13.3088415259036,-4.91762225934298,
0.00160614365327011));
#84484=CARTESIAN_POINT('Ctrl Pts',(-13.2644109942918,-4.91490330929803,
-0.91820790615135));
#84485=CARTESIAN_POINT('Ctrl Pts',(-13.21998046268,-4.66721713029717,-1.83938153902219));
#84486=CARTESIAN_POINT('Ctrl Pts',(-13.1755499310683,-4.18380013351818,
-2.61331150839947));
#84487=CARTESIAN_POINT('Ctrl Pts',(-13.0965684088296,-3.32445839493059,
-3.98908093699027));
#84488=CARTESIAN_POINT('Ctrl Pts',(-13.017586886591,-1.72020573233587,-4.89955942712428));
#84489=CARTESIAN_POINT('Ctrl Pts',(-12.9386053643524,-0.0984282630900391,
-4.93192583826895));
#84490=CARTESIAN_POINT('Ctrl Pts',(-12.8596238421137,1.52334920615579,-4.96429224941362));
#84491=CARTESIAN_POINT('Ctrl Pts',(-12.7806423198751,3.16265148205274,-4.11854658156895));
#84492=CARTESIAN_POINT('Ctrl Pts',(-12.7016607976365,4.07620056018163,-2.77815938893629));
#84493=CARTESIAN_POINT('Ctrl Pts',(-12.6226792753978,4.98974963831051,-1.43777219630362));
#84494=CARTESIAN_POINT('Ctrl Pts',(-12.5436977531592,5.17754551867134,0.397256521117021));
#84495=CARTESIAN_POINT('Ctrl Pts',(-12.4647162309206,4.55443944667193,1.89490419909782));
#84496=CARTESIAN_POINT('Ctrl Pts',(-12.3857347086819,3.93133337467253,3.39255187707859));
#84497=CARTESIAN_POINT('Ctrl Pts',(-12.3067531864433,2.49732535031289,4.55281851561955));
#84498=CARTESIAN_POINT('Ctrl Pts',(-12.2277716642046,0.902610666028616,
4.84962623124001));
#84499=CARTESIAN_POINT('Ctrl Pts',(-12.148790141966,-0.692104018255692,
5.14643394686049));
#84500=CARTESIAN_POINT('Ctrl Pts',(-12.0698086197274,-2.44752536246463,
4.57978273956048));
#84501=CARTESIAN_POINT('Ctrl Pts',(-11.9908270974887,-3.5677256766153,3.40659861057621));
#84502=CARTESIAN_POINT('Ctrl Pts',(-11.9301652402937,-4.42809693258498,
2.505533069184));
#84503=CARTESIAN_POINT('Ctrl Pts',(-11.8695033830986,-4.9137495695897,1.2466721022382));
#84504=CARTESIAN_POINT('Ctrl Pts',(-11.8088415259036,-4.92505452712729,
-0.00437787461885928));
#84505=CARTESIAN_POINT('Origin',(-12.,0.,0.));
#84506=CARTESIAN_POINT('',(-10.0911584740964,-4.93097413974624,0.00270638408970972));
#84507=CARTESIAN_POINT('',(-10.3088415259036,-4.93100255652112,0.00268767346070769));
#84508=CARTESIAN_POINT('',(-12.,-4.925,-6.03138548580071E-16));
#84509=CARTESIAN_POINT('Ctrl Pts',(-10.0911584740964,-4.93097413974624,
0.00270638408970972));
#84510=CARTESIAN_POINT('Ctrl Pts',(-10.0990147278483,-4.93204740412384,
0.164224370369626));
#84511=CARTESIAN_POINT('Ctrl Pts',(-10.1068709816003,-4.92479171726874,
0.325644779964446));
#84512=CARTESIAN_POINT('Ctrl Pts',(-10.1147272353522,-4.90888841078112,
0.486208672297471));
#84513=CARTESIAN_POINT('Ctrl Pts',(-10.1937087575908,-4.74900720089645,
2.10041068682757));
#84514=CARTESIAN_POINT('Ctrl Pts',(-10.2726902798295,-3.71511564509976,
3.62804495438529));
#84515=CARTESIAN_POINT('Ctrl Pts',(-10.3516718020681,-2.27599174954493,
4.3764649956925));
#84516=CARTESIAN_POINT('Ctrl Pts',(-10.4306533243067,-0.836867853990087,
5.12488503699971));
#84517=CARTESIAN_POINT('Ctrl Pts',(-10.5096348465454,1.00748838132291,5.09409085205642));
#84518=CARTESIAN_POINT('Ctrl Pts',(-10.588616368784,2.42082519112922,4.29804486906693));
#84519=CARTESIAN_POINT('Ctrl Pts',(-10.6675978910227,3.83416200093553,3.50199888607743));
#84520=CARTESIAN_POINT('Ctrl Pts',(-10.7465794132613,4.81647938523517,1.94070110504172));
#84521=CARTESIAN_POINT('Ctrl Pts',(-10.8255609354999,4.92238364462085,0.322061419122964));
#84522=CARTESIAN_POINT('Ctrl Pts',(-10.9045424577385,5.02828790400653,-1.29657826679578));
#84523=CARTESIAN_POINT('Ctrl Pts',(-10.9835239799772,4.25777903847828,-2.97255985759757));
#84524=CARTESIAN_POINT('Ctrl Pts',(-11.0625055022158,2.96021439376647,-3.94597453684843));
#84525=CARTESIAN_POINT('Ctrl Pts',(-11.1414870244545,1.66264974905462,-4.91938921609932));
#84526=CARTESIAN_POINT('Ctrl Pts',(-11.2204685466931,-0.16197067484082,
-5.19023698379922));
#84527=CARTESIAN_POINT('Ctrl Pts',(-11.2994500689317,-1.68634355050059,
-4.63571242984327));
#84528=CARTESIAN_POINT('Ctrl Pts',(-11.3784315911704,-3.21071642616031,
-4.08118787588734));
#84529=CARTESIAN_POINT('Ctrl Pts',(-11.457413113409,-4.4348417535844,-2.70129100027559));
#84530=CARTESIAN_POINT('Ctrl Pts',(-11.5363946356476,-4.80368740483359,
-1.12168249480923));
#84531=CARTESIAN_POINT('Ctrl Pts',(-11.5546492484639,-4.88893689562171,
-0.756595309208631));
#84532=CARTESIAN_POINT('Ctrl Pts',(-11.5729038612802,-4.92849835935227,
-0.380839764938135));
#84533=CARTESIAN_POINT('Ctrl Pts',(-11.5911584740964,-4.92509485823308,
-0.00437651270843276));
#84534=CARTESIAN_POINT('Ctrl Pts',(-11.8088415259036,-4.92505452712729,
-0.00437787461885928));
#84535=CARTESIAN_POINT('Ctrl Pts',(-11.79052186086,-4.92846858408164,-0.382190516508843));
#84536=CARTESIAN_POINT('Ctrl Pts',(-11.7722021958164,-4.88862125463388,
-0.759290781644309));
#84537=CARTESIAN_POINT('Ctrl Pts',(-11.7538825307728,-4.80276849198252,
-1.12560890613918));
#84538=CARTESIAN_POINT('Ctrl Pts',(-11.6749010085342,-4.4326317091067,-2.70491524320179));
#84539=CARTESIAN_POINT('Ctrl Pts',(-11.5959194862956,-3.20737885926272,
-4.08381086665851));
#84540=CARTESIAN_POINT('Ctrl Pts',(-11.5169379640569,-1.68255330167799,
-4.6370890636446));
#84541=CARTESIAN_POINT('Ctrl Pts',(-11.4379564418183,-0.157727744093241,
-5.19036726063069));
#84542=CARTESIAN_POINT('Ctrl Pts',(-11.3589749195797,1.66667052123224,-4.91802803114613));
#84543=CARTESIAN_POINT('Ctrl Pts',(-11.279993397341,2.96343889606202,-3.94355303076636));
#84544=CARTESIAN_POINT('Ctrl Pts',(-11.2010118751024,4.26020727089178,-2.9690780303866));
#84545=CARTESIAN_POINT('Ctrl Pts',(-11.1220303528637,5.02934575522583,-1.29246725911162));
#84546=CARTESIAN_POINT('Ctrl Pts',(-11.0430488306251,4.9221183495091,0.326085189154109));
#84547=CARTESIAN_POINT('Ctrl Pts',(-10.9640673083865,4.81489094379237,1.94463763741987));
#84548=CARTESIAN_POINT('Ctrl Pts',(-10.8850857861478,3.83129764802485,3.50513176267639));
#84549=CARTESIAN_POINT('Ctrl Pts',(-10.8061042639092,2.4173106741576,4.30002205828802));
#84550=CARTESIAN_POINT('Ctrl Pts',(-10.7271227416706,1.00332370029034,5.09491235389966));
#84551=CARTESIAN_POINT('Ctrl Pts',(-10.6481412194319,-0.84105695167665,
5.12419881986638));
#84552=CARTESIAN_POINT('Ctrl Pts',(-10.5691596971933,-2.27956844569424,
4.37460264464728));
#84553=CARTESIAN_POINT('Ctrl Pts',(-10.4901781749547,-3.7180799397118,3.62500646942819));
#84554=CARTESIAN_POINT('Ctrl Pts',(-10.411196652716,-4.75072227577999,2.0965276530233));
#84555=CARTESIAN_POINT('Ctrl Pts',(-10.3322151304774,-4.9092838579553,0.482195602613046));
#84556=CARTESIAN_POINT('Ctrl Pts',(-10.3244239289528,-4.92492530428061,
0.322948401801202));
#84557=CARTESIAN_POINT('Ctrl Pts',(-10.3166327274282,-4.93206106288763,
0.162865762393093));
#84558=CARTESIAN_POINT('Ctrl Pts',(-10.3088415259036,-4.93100255652112,
0.00268767346070769));
#84559=CARTESIAN_POINT('Origin',(-12.,0.,0.));
#84560=CARTESIAN_POINT('',(-8.59115847409641,-4.91774836348285,0.00178568346280022));
#84561=CARTESIAN_POINT('',(-8.8088415259036,-4.91776282945141,0.0018054816820188));
#84562=CARTESIAN_POINT('',(-12.,-4.925,-6.03138548580071E-16));
#84563=CARTESIAN_POINT('Ctrl Pts',(-8.59115847409641,-4.91774836348285,
0.00178568346280023));
#84564=CARTESIAN_POINT('Ctrl Pts',(-8.62512559441653,-4.9200628213466,0.704938149616686));
#84565=CARTESIAN_POINT('Ctrl Pts',(-8.65909271473664,-4.77912254938096,
1.40720569299442));
#84566=CARTESIAN_POINT('Ctrl Pts',(-8.69305983505676,-4.49031348205501,
2.04222161760194));
#84567=CARTESIAN_POINT('Ctrl Pts',(-8.77204135729539,-3.81876465605063,
3.51878259476466));
#84568=CARTESIAN_POINT('Ctrl Pts',(-8.85102287953402,-2.34773128053141,
4.63173318336878));
#84569=CARTESIAN_POINT('Ctrl Pts',(-8.93000440177266,-0.744196356661722,
4.87644912669527));
#84570=CARTESIAN_POINT('Ctrl Pts',(-9.0089859240113,0.859338567207992,5.12116507002176));
#84571=CARTESIAN_POINT('Ctrl Pts',(-9.08796744624994,2.59537503942818,4.49764636807061));
#84572=CARTESIAN_POINT('Ctrl Pts',(-9.16694896848857,3.6767746879967,3.28860338080236));
#84573=CARTESIAN_POINT('Ctrl Pts',(-9.24593049072721,4.75817433656521,2.07956039353412));
#84574=CARTESIAN_POINT('Ctrl Pts',(-9.32491201296583,5.18493716148205,0.284993120948776));
#84575=CARTESIAN_POINT('Ctrl Pts',(-9.40389353520447,4.76356412017933,-1.28142154479291));
#84576=CARTESIAN_POINT('Ctrl Pts',(-9.48287505744311,4.34219107887662,-2.84783621053459));
#84577=CARTESIAN_POINT('Ctrl Pts',(-9.56185657968176,3.07268217135434,-4.18609826943261));
#84578=CARTESIAN_POINT('Ctrl Pts',(-9.64083810192039,1.53064694885267,-4.68942472169945));
#84579=CARTESIAN_POINT('Ctrl Pts',(-9.71981962415903,-0.0113882736489851,
-5.19275117396628));
#84580=CARTESIAN_POINT('Ctrl Pts',(-9.79880114639765,-1.82594981113003,
-4.86114201960195));
#84581=CARTESIAN_POINT('Ctrl Pts',(-9.87778266863628,-3.09029514788423,
-3.84495256166855));
#84582=CARTESIAN_POINT('Ctrl Pts',(-9.94890793712299,-4.22887666654442,
-2.92984297678998));
#84583=CARTESIAN_POINT('Ctrl Pts',(-10.0200332056097,-4.92125752169593,
-1.45956946675985));
#84584=CARTESIAN_POINT('Ctrl Pts',(-10.0911584740964,-4.93097413974624,
0.00270638408970972));
#84585=CARTESIAN_POINT('Ctrl Pts',(-10.3088415259036,-4.93100255652112,
0.00268767346070769));
#84586=CARTESIAN_POINT('Ctrl Pts',(-10.2376512051896,-4.92133069686354,
-1.46090295328149));
#84587=CARTESIAN_POINT('Ctrl Pts',(-10.1664608844755,-4.22752191947411,
-2.93246263442317));
#84588=CARTESIAN_POINT('Ctrl Pts',(-10.0952705637615,-3.0871507457315,-3.84747720854709));
#84589=CARTESIAN_POINT('Ctrl Pts',(-10.0162890415228,-1.82197522304997,
-4.86263268488127));
#84590=CARTESIAN_POINT('Ctrl Pts',(-9.93730751928421,-0.00714334940447398,
-5.19275835313399));
#84591=CARTESIAN_POINT('Ctrl Pts',(-9.85832599704557,1.53447978605512,-4.68817153945416));
#84592=CARTESIAN_POINT('Ctrl Pts',(-9.77934447480694,3.07610292151471,-4.18358472577433));
#84593=CARTESIAN_POINT('Ctrl Pts',(-9.70036295256829,4.34451731878839,-2.84428543016197));
#84594=CARTESIAN_POINT('Ctrl Pts',(-9.62138143032966,4.76460968983639,-1.27752694714326));
#84595=CARTESIAN_POINT('Ctrl Pts',(-9.54239990809102,5.18470206088438,0.289231535875453));
#84596=CARTESIAN_POINT('Ctrl Pts',(-9.46341838585239,4.75647240570669,2.08344920630051));
#84597=CARTESIAN_POINT('Ctrl Pts',(-9.38443686361376,3.67408484413261,3.29160768550489));
#84598=CARTESIAN_POINT('Ctrl Pts',(-9.30545534137512,2.59169728255855,4.49976616470925));
#84599=CARTESIAN_POINT('Ctrl Pts',(-9.22647381913649,0.855151814588114,
5.12186545269295));
#84600=CARTESIAN_POINT('Ctrl Pts',(-9.14749229689785,-0.748182403404063,
4.87583876767843));
#84601=CARTESIAN_POINT('Ctrl Pts',(-9.06851077465921,-2.35151662139626,
4.62981208266391));
#84602=CARTESIAN_POINT('Ctrl Pts',(-8.98952925242058,-3.8216395894102,3.51565942465113));
#84603=CARTESIAN_POINT('Ctrl Pts',(-8.91054773018194,-4.49198109523854,
2.03855008208786));
#84604=CARTESIAN_POINT('Ctrl Pts',(-8.87664566208916,-4.77971881833972,
1.40451492940035));
#84605=CARTESIAN_POINT('Ctrl Pts',(-8.84274359399638,-4.92009888102638,
0.703605948803637));
#84606=CARTESIAN_POINT('Ctrl Pts',(-8.8088415259036,-4.91776282945141,0.0018054816820188));
#84607=CARTESIAN_POINT('Origin',(-12.,0.,0.));
#84608=CARTESIAN_POINT('',(-7.0911584740964,-4.92469711254938,-0.00438490361534538));
#84609=CARTESIAN_POINT('',(-7.3088415259036,-4.92465698422042,-0.00438510844452123));
#84610=CARTESIAN_POINT('',(-12.,-4.925,-6.03138548580071E-16));
#84611=CARTESIAN_POINT('Ctrl Pts',(-7.0911584740964,-4.92469711254938,-0.00438490361534538));
#84612=CARTESIAN_POINT('Ctrl Pts',(-7.1512364609847,-4.91355887879697,1.23485426137012));
#84613=CARTESIAN_POINT('Ctrl Pts',(-7.21131444787301,-4.43814412276136,
2.4817098635007));
#84614=CARTESIAN_POINT('Ctrl Pts',(-7.27139243476131,-3.59262435392421,
3.38033053923436));
#84615=CARTESIAN_POINT('Ctrl Pts',(-7.35037395699995,-2.4810618351971,4.56170216236331));
#84616=CARTESIAN_POINT('Ctrl Pts',(-7.42935547923858,-0.729845164256781,
5.14121780162075));
#84617=CARTESIAN_POINT('Ctrl Pts',(-7.50833700147721,0.867004414740713,
4.85611857837648));
#84618=CARTESIAN_POINT('Ctrl Pts',(-7.58731852371585,2.46385399373825,4.5710193551322));
#84619=CARTESIAN_POINT('Ctrl Pts',(-7.66630004595449,3.90633648079293,3.42130526938617));
#84620=CARTESIAN_POINT('Ctrl Pts',(-7.74528156819313,4.54041416726393,1.9282695590024));
#84621=CARTESIAN_POINT('Ctrl Pts',(-7.82426309043176,5.17449185373491,0.435233848618645));
#84622=CARTESIAN_POINT('Ctrl Pts',(-7.9032446126704,5.00016473962219,-1.40112348640288));
#84623=CARTESIAN_POINT('Ctrl Pts',(-7.98222613490903,4.09647469008515,-2.74817747171883));
#84624=CARTESIAN_POINT('Ctrl Pts',(-8.06120765714767,3.19278464054811,-4.09523145703475));
#84625=CARTESIAN_POINT('Ctrl Pts',(-8.14018917938631,1.5597316555868,-4.95298209264516));
#84626=CARTESIAN_POINT('Ctrl Pts',(-8.21917070162494,-0.0622397588378364,
-4.93251563757504));
#84627=CARTESIAN_POINT('Ctrl Pts',(-8.29815222386358,-1.68421117326252,
-4.91204918250491));
#84628=CARTESIAN_POINT('Ctrl Pts',(-8.37713374610222,-3.29510101715048,
-4.0133656367542));
#84629=CARTESIAN_POINT('Ctrl Pts',(-8.45611526834085,-4.1645138008497,-2.64393818101814));
#84630=CARTESIAN_POINT('Ctrl Pts',(-8.50112967025937,-4.66002332471387,
-1.86345236429124));
#84631=CARTESIAN_POINT('Ctrl Pts',(-8.54614407217789,-4.91468116392279,
-0.930056269082769));
#84632=CARTESIAN_POINT('Ctrl Pts',(-8.59115847409641,-4.91774836348285,
0.00178568346280023));
#84633=CARTESIAN_POINT('Ctrl Pts',(-8.8088415259036,-4.91776282945141,0.0018054816820188));
#84634=CARTESIAN_POINT('Ctrl Pts',(-8.76376207175774,-4.91465659034033,
-0.931375995346603));
#84635=CARTESIAN_POINT('Ctrl Pts',(-8.71868261761189,-4.65921509964408,
-1.86613370276596));
#84636=CARTESIAN_POINT('Ctrl Pts',(-8.67360316346604,-4.16235075150242,
-2.64734146241595));
#84637=CARTESIAN_POINT('Ctrl Pts',(-8.5946216412274,-3.29181885829526,-4.0160576372427));
#84638=CARTESIAN_POINT('Ctrl Pts',(-8.51564011898876,-1.6801950282382,-4.91342395978241));
#84639=CARTESIAN_POINT('Ctrl Pts',(-8.43665859675013,-0.058207548536371,
-4.93256449308577));
#84640=CARTESIAN_POINT('Ctrl Pts',(-8.35767707451149,1.56377993116546,-4.95170502638914));
#84641=CARTESIAN_POINT('Ctrl Pts',(-8.27869555227285,3.19613106051205,-4.09261977045616));
#84642=CARTESIAN_POINT('Ctrl Pts',(-8.19971403003422,4.0987195627487,-2.74482759806664));
#84643=CARTESIAN_POINT('Ctrl Pts',(-8.12073250779558,5.00130806498535,-1.39703542567712));
#84644=CARTESIAN_POINT('Ctrl Pts',(-8.04175098555695,5.17413394011204,0.439463663168932));
#84645=CARTESIAN_POINT('Ctrl Pts',(-7.96276946331831,4.53883600150744,1.93198042137454));
#84646=CARTESIAN_POINT('Ctrl Pts',(-7.88378794107968,3.90353806290283,3.42449717958015));
#84647=CARTESIAN_POINT('Ctrl Pts',(-7.80480641884104,2.46011631056691,4.57303160714531));
#84648=CARTESIAN_POINT('Ctrl Pts',(-7.7258248966024,0.863034326582695,4.85682533639864));
#84649=CARTESIAN_POINT('Ctrl Pts',(-7.64684337436377,-0.734047657401497,
5.14061906565198));
#84650=CARTESIAN_POINT('Ctrl Pts',(-7.56786185212513,-2.48478987303398,
4.5596720965935));
#84651=CARTESIAN_POINT('Ctrl Pts',(-7.4888803298865,-3.59538619959974,3.37739228887328));
#84652=CARTESIAN_POINT('Ctrl Pts',(-7.42886739522553,-4.43925629594361,
2.47905456581291));
#84653=CARTESIAN_POINT('Ctrl Pts',(-7.36885446056456,-4.91353853831652,
1.2335376806911));
#84654=CARTESIAN_POINT('Ctrl Pts',(-7.3088415259036,-4.92465698422042,-0.00438510844452123));
#84655=CARTESIAN_POINT('Origin',(-12.,0.,0.));
#84656=CARTESIAN_POINT('',(-5.5911584740964,-4.93125390801305,0.00251598733971681));
#84657=CARTESIAN_POINT('',(-5.80884152590359,-4.93128064513841,0.00249645100189436));
#84658=CARTESIAN_POINT('',(-12.,-4.925,-6.03138548580071E-16));
#84659=CARTESIAN_POINT('Ctrl Pts',(-5.5911584740964,-4.93125390801305,0.00251598733971681));
#84660=CARTESIAN_POINT('Ctrl Pts',(-5.59836580531426,-4.93218240192545,
0.150670486559072));
#84661=CARTESIAN_POINT('Ctrl Pts',(-5.60557313653211,-4.92607803394608,
0.298747450142229));
#84662=CARTESIAN_POINT('Ctrl Pts',(-5.61278046774996,-4.91268998808522,
0.446162921385522));
#84663=CARTESIAN_POINT('Ctrl Pts',(-5.6917619899886,-4.76597711893443,2.06161501709073));
#84664=CARTESIAN_POINT('Ctrl Pts',(-5.77074351222723,-3.74457705430679,
3.59762937694339));
#84665=CARTESIAN_POINT('Ctrl Pts',(-5.84972503446586,-2.31160400818357,
4.35775988654768));
#84666=CARTESIAN_POINT('Ctrl Pts',(-5.9287065567045,-0.878630962060319,
5.11789039615198));
#84667=CARTESIAN_POINT('Ctrl Pts',(-6.00768807894314,0.965915065558466,
5.10213705550793));
#84668=CARTESIAN_POINT('Ctrl Pts',(-6.08666960118177,2.38569625012759,4.31764260950633));
#84669=CARTESIAN_POINT('Ctrl Pts',(-6.16565112342041,3.80547743469666,3.53314816350476));
#84670=CARTESIAN_POINT('Ctrl Pts',(-6.24463264565905,4.80049377621606,1.9799126121456));
#84671=CARTESIAN_POINT('Ctrl Pts',(-6.32361416789768,4.91959372867696,0.362190341378671));
#84672=CARTESIAN_POINT('Ctrl Pts',(-6.40259569013632,5.03869368113786,-1.25553192938831));
#84673=CARTESIAN_POINT('Ctrl Pts',(-6.48157721237495,4.2818772445403,-2.93774091956309));
#84674=CARTESIAN_POINT('Ctrl Pts',(-6.56055873461359,2.99229346260409,-3.92170423906757));
#84675=CARTESIAN_POINT('Ctrl Pts',(-6.63954025685222,1.70270968066789,-4.90566755857204));
#84676=CARTESIAN_POINT('Ctrl Pts',(-6.71852177909086,-0.119641446606939,
-5.19138520740618));
#84677=CARTESIAN_POINT('Ctrl Pts',(-6.7975033013295,-1.64848551554391,-4.64930960543246));
#84678=CARTESIAN_POINT('Ctrl Pts',(-6.87648482356814,-3.17732958448089,
-4.10723400345873));
#84679=CARTESIAN_POINT('Ctrl Pts',(-6.95546634580677,-4.41266659508003,
-2.73736515067713));
#84680=CARTESIAN_POINT('Ctrl Pts',(-7.0344478680454,-4.79438091712263,-1.16081692078609));
#84681=CARTESIAN_POINT('Ctrl Pts',(-7.05335140339573,-4.88574089570925,
-0.783483914906529));
#84682=CARTESIAN_POINT('Ctrl Pts',(-7.07225493874606,-4.92820175720184,
-0.394311440374502));
#84683=CARTESIAN_POINT('Ctrl Pts',(-7.0911584740964,-4.92469711254938,-0.00438490361534538));
#84684=CARTESIAN_POINT('Ctrl Pts',(-7.3088415259036,-4.92465698422042,-0.00438510844452123));
#84685=CARTESIAN_POINT('Ctrl Pts',(-7.28987293832593,-4.92817124687141,
-0.395661538646872));
#84686=CARTESIAN_POINT('Ctrl Pts',(-7.27090435074826,-4.88541387252908,
-0.786179292857178));
#84687=CARTESIAN_POINT('Ctrl Pts',(-7.25193576317059,-4.79343001691259,
-1.16473570824833));
#84688=CARTESIAN_POINT('Ctrl Pts',(-7.17295424093195,-4.41042707016064,
-2.74097125126758));
#84689=CARTESIAN_POINT('Ctrl Pts',(-7.09397271869331,-3.17397073915778,
-4.10982969092408));
#84690=CARTESIAN_POINT('Ctrl Pts',(-7.01499119645468,-1.64468416686737,
-4.65065528590648));
#84691=CARTESIAN_POINT('Ctrl Pts',(-6.93600967421605,-0.11539759457693,
-5.19148088088889));
#84692=CARTESIAN_POINT('Ctrl Pts',(-6.85702815197741,1.70671921900106,-4.90427363119719));
#84693=CARTESIAN_POINT('Ctrl Pts',(-6.77804662973878,2.9954981113016,-3.91925651912733));
#84694=CARTESIAN_POINT('Ctrl Pts',(-6.69906510750014,4.28427700360214,-2.93423940705747));
#84695=CARTESIAN_POINT('Ctrl Pts',(-6.6200835852615,5.03971797462523,-1.25141243260946));
#84696=CARTESIAN_POINT('Ctrl Pts',(-6.54110206302287,4.91929563087673,0.366211814021057));
#84697=CARTESIAN_POINT('Ctrl Pts',(-6.46212054078423,4.79887328712824,1.98383606065158));
#84698=CARTESIAN_POINT('Ctrl Pts',(-6.3831390185456,3.80258762860816,3.5362575794646));
#84699=CARTESIAN_POINT('Ctrl Pts',(-6.30415749630696,2.38216572629362,4.31959107430742));
#84700=CARTESIAN_POINT('Ctrl Pts',(-6.22517597406833,0.96174382397912,5.10292456915022));
#84701=CARTESIAN_POINT('Ctrl Pts',(-6.14619445182969,-0.882814322129821,
5.11717004002285));
#84702=CARTESIAN_POINT('Ctrl Pts',(-6.06721292959106,-2.31516539749777,
4.35586843028431));
#84703=CARTESIAN_POINT('Ctrl Pts',(-5.98823140735242,-3.74751647286578,
3.59456682054574));
#84704=CARTESIAN_POINT('Ctrl Pts',(-5.90924988511379,-4.76766047749277,
2.05771813019591));
#84705=CARTESIAN_POINT('Ctrl Pts',(-5.83026836287515,-4.91305270009236,
0.442146762242162));
#84706=CARTESIAN_POINT('Ctrl Pts',(-5.82312608388463,-4.92620048184465,
0.296051053879439));
#84707=CARTESIAN_POINT('Ctrl Pts',(-5.81598380489411,-4.93219494682612,
0.149311587754206));
#84708=CARTESIAN_POINT('Ctrl Pts',(-5.80884152590359,-4.93128064513841,
0.00249645100189436));
#84709=CARTESIAN_POINT('Origin',(-12.,0.,0.));
#84710=CARTESIAN_POINT('',(-4.0911584740964,-4.91790394892889,0.00198131612508923));
#84711=CARTESIAN_POINT('',(-4.30884152590359,-4.91791992129793,0.00200057189650126));
#84712=CARTESIAN_POINT('',(-12.,-4.925,-6.03138548580071E-16));
#84713=CARTESIAN_POINT('Ctrl Pts',(-4.0911584740964,-4.91790394892889,0.00198131612508923));
#84714=CARTESIAN_POINT('Ctrl Pts',(-4.12447667188244,-4.92042735435566,
0.691645796992671));
#84715=CARTESIAN_POINT('Ctrl Pts',(-4.15779486966848,-4.78502020932576,
1.38036363987776));
#84716=CARTESIAN_POINT('Ctrl Pts',(-4.19111306745451,-4.5068173542973,2.00553729863833));
#84717=CARTESIAN_POINT('Ctrl Pts',(-4.27009458969315,-3.8473313544126,3.48752523656628));
#84718=CARTESIAN_POINT('Ctrl Pts',(-4.34907611193179,-2.38542274738594,
4.61243459072995));
#84719=CARTESIAN_POINT('Ctrl Pts',(-4.42805763417042,-0.783936747380577,
4.87021849115426));
#84720=CARTESIAN_POINT('Ctrl Pts',(-4.50703915640906,0.817549252624831,
5.12800239157858));
#84721=CARTESIAN_POINT('Ctrl Pts',(-4.58602067864769,2.55861264560894,4.51866083826349));
#84722=CARTESIAN_POINT('Ctrl Pts',(-4.66500220088633,3.64983552948727,3.31847630846199));
#84723=CARTESIAN_POINT('Ctrl Pts',(-4.74398372312497,4.7410584133656,2.11829177866049));
#84724=CARTESIAN_POINT('Ctrl Pts',(-4.82296524536361,5.18244078813814,0.327264272372587));
#84725=CARTESIAN_POINT('Ctrl Pts',(-4.90194676760224,4.77385508310388,-1.2425343895004));
#84726=CARTESIAN_POINT('Ctrl Pts',(-4.98092828984088,4.36526937806963,-2.81233305137334));
#84727=CARTESIAN_POINT('Ctrl Pts',(-5.05990981207951,3.10671559322865,-4.16090286883138));
#84728=CARTESIAN_POINT('Ctrl Pts',(-5.13889133431815,1.56883603197956,-4.6767871360847));
#84729=CARTESIAN_POINT('Ctrl Pts',(-5.21787285655678,0.0309564707304835,
-5.19267140333802));
#84730=CARTESIAN_POINT('Ctrl Pts',(-5.29685437879541,-1.78624886692669,
-4.87587012038662));
#84731=CARTESIAN_POINT('Ctrl Pts',(-5.37583590103405,-3.05883869891831,
-3.87002456313205));
#84732=CARTESIAN_POINT('Ctrl Pts',(-5.44761009205483,-4.21530040165052,
-2.95596581726907));
#84733=CARTESIAN_POINT('Ctrl Pts',(-5.51938428307562,-4.92200750356521,
-1.47288024548768));
#84734=CARTESIAN_POINT('Ctrl Pts',(-5.5911584740964,-4.93125390801305,0.00251598733971681));
#84735=CARTESIAN_POINT('Ctrl Pts',(-5.80884152590359,-4.93128064513841,
0.00249645100189436));
#84736=CARTESIAN_POINT('Ctrl Pts',(-5.73700228265547,-4.92208431698711,
-1.47421544105046));
#84737=CARTESIAN_POINT('Ctrl Pts',(-5.66516303940736,-4.21393107993154,
-2.95858289742135));
#84738=CARTESIAN_POINT('Ctrl Pts',(-5.59332379615924,-3.05567380905537,
-3.8725234884491));
#84739=CARTESIAN_POINT('Ctrl Pts',(-5.5143422739206,-1.78226225484658,-4.87732832562897));
#84740=CARTESIAN_POINT('Ctrl Pts',(-5.43536075168197,0.0352012941432209,
-5.19264395443107));
#84741=CARTESIAN_POINT('Ctrl Pts',(-5.35637922944334,1.57265851305555,-4.67550273398319));
#84742=CARTESIAN_POINT('Ctrl Pts',(-5.2773977072047,3.11011573196789,-4.1583615135353));
#84743=CARTESIAN_POINT('Ctrl Pts',(-5.19841618496606,4.36756662080275,-2.80876344383742));
#84744=CARTESIAN_POINT('Ctrl Pts',(-5.11943466272742,4.77486887790956,-1.23863140793454));
#84745=CARTESIAN_POINT('Ctrl Pts',(-5.04045314048879,5.18217113501637,0.331500627968312));
#84746=CARTESIAN_POINT('Ctrl Pts',(-4.96147161825015,4.73932476039516,2.12216663007616));
#84747=CARTESIAN_POINT('Ctrl Pts',(-4.88249009601152,3.64712124096917,3.32145860332436));
#84748=CARTESIAN_POINT('Ctrl Pts',(-4.80350857377289,2.55491772154319,4.52075057657256));
#84749=CARTESIAN_POINT('Ctrl Pts',(-4.72452705153425,0.813357057312425,
5.12866852096113));
#84750=CARTESIAN_POINT('Ctrl Pts',(-4.64554552929562,-0.787917616290547,
4.86957560126685));
#84751=CARTESIAN_POINT('Ctrl Pts',(-4.56656400705698,-2.38919228989357,
4.61048268157256));
#84752=CARTESIAN_POINT('Ctrl Pts',(-4.48758248481834,-3.85018097286878,
3.48437889779535));
#84753=CARTESIAN_POINT('Ctrl Pts',(-4.4086009625797,-4.50845510335787,2.00185237675489));
#84754=CARTESIAN_POINT('Ctrl Pts',(-4.375347817021,-4.78560455373875,1.3776725837921));
#84755=CARTESIAN_POINT('Ctrl Pts',(-4.34209467146229,-4.92046360302658,
0.690312754928868));
#84756=CARTESIAN_POINT('Ctrl Pts',(-4.30884152590359,-4.91791992129793,
0.00200057189650126));
#84757=CARTESIAN_POINT('Origin',(-12.,0.,0.));
#84758=CARTESIAN_POINT('',(-2.5911584740964,-4.92431925468094,-0.00436907230553341));
#84759=CARTESIAN_POINT('',(-2.8088415259036,-4.92426410821032,-0.00437867314108101));
#84760=CARTESIAN_POINT('',(-12.,-4.925,-6.03138548580071E-16));
#84761=CARTESIAN_POINT('Ctrl Pts',(-2.5911584740964,-4.92431925468094,-0.00436907230553341));
#84762=CARTESIAN_POINT('Ctrl Pts',(-2.65058753845062,-4.91338616368288,
1.22173429077995));
#84763=CARTESIAN_POINT('Ctrl Pts',(-2.71001660280484,-4.44917797193856,
2.45521514120874));
#84764=CARTESIAN_POINT('Ctrl Pts',(-2.76944566715907,-3.62006233571212,
3.35091658286247));
#84765=CARTESIAN_POINT('Ctrl Pts',(-2.8484271893977,-2.51816352958756,4.54130825572287));
#84766=CARTESIAN_POINT('Ctrl Pts',(-2.92740871163635,-0.77174540757938,
5.13509562040796));
#84767=CARTESIAN_POINT('Ctrl Pts',(-3.00639023387498,0.827372408670279,
4.86302996372663));
#84768=CARTESIAN_POINT('Ctrl Pts',(-3.08537175611362,2.42649022491994,4.5909643070453));
#84769=CARTESIAN_POINT('Ctrl Pts',(-3.16435327835225,3.87830773541108,3.45304562899755));
#84770=CARTESIAN_POINT('Ctrl Pts',(-3.24333480059088,4.52454114442089,1.9652288206206));
#84771=CARTESIAN_POINT('Ctrl Pts',(-3.32231632282952,5.1707745534307,0.47741201224366));
#84772=CARTESIAN_POINT('Ctrl Pts',(-3.40129784506816,5.01142386095919,-1.36030292646248));
#84773=CARTESIAN_POINT('Ctrl Pts',(-3.4802793673068,4.11874747202576,-2.71468058079156));
#84774=CARTESIAN_POINT('Ctrl Pts',(-3.55926088954543,3.22607108309233,-4.06905823512064));
#84775=CARTESIAN_POINT('Ctrl Pts',(-3.63824241178406,1.60006899769698,-4.94009860507265));
#84776=CARTESIAN_POINT('Ctrl Pts',(-3.7172239340227,-0.0220148869955472,
-4.9328595746569));
#84777=CARTESIAN_POINT('Ctrl Pts',(-3.79620545626133,-1.64409877168807,
-4.92562054424115));
#84778=CARTESIAN_POINT('Ctrl Pts',(-3.87518697849998,-3.26226445567777,
-4.04010211345763));
#84779=CARTESIAN_POINT('Ctrl Pts',(-3.95416850073861,-4.14281560130125,
-2.67780963721974));
#84780=CARTESIAN_POINT('Ctrl Pts',(-3.99983182519121,-4.65190800063768,
-1.89019752772115));
#84781=CARTESIAN_POINT('Ctrl Pts',(-4.0454951496438,-4.91444556617158,-0.943219056221707));
#84782=CARTESIAN_POINT('Ctrl Pts',(-4.0911584740964,-4.91790394892889,0.00198131612508923));
#84783=CARTESIAN_POINT('Ctrl Pts',(-4.30884152590359,-4.91791992129793,
0.00200057189650126));
#84784=CARTESIAN_POINT('Ctrl Pts',(-4.26311314922366,-4.9144219533828,-0.944538417130053));
#84785=CARTESIAN_POINT('Ctrl Pts',(-4.21738477254373,-4.65108670196389,
-1.89287836832389));
#84786=CARTESIAN_POINT('Ctrl Pts',(-4.1716563958638,-4.14062462025537,-2.68119534003646));
#84787=CARTESIAN_POINT('Ctrl Pts',(-4.09267487362516,-3.25896042866083,
-4.04276727748366));
#84788=CARTESIAN_POINT('Ctrl Pts',(-4.01369335138653,-1.64007246746879,
-4.92696189407442));
#84789=CARTESIAN_POINT('Ctrl Pts',(-3.93471182914789,-0.017982895669106,
-4.93287521506465));
#84790=CARTESIAN_POINT('Ctrl Pts',(-3.85573030690925,1.60410667613065,-4.93878853605489));
#84791=CARTESIAN_POINT('Ctrl Pts',(-3.77674878467062,3.22939785853806,-4.06642056144451));
#84792=CARTESIAN_POINT('Ctrl Pts',(-3.69776726243198,4.12096588213986,-2.71131315212336));
#84793=CARTESIAN_POINT('Ctrl Pts',(-3.61878574019335,5.01253390574162,-1.35620574280227));
#84794=CARTESIAN_POINT('Ctrl Pts',(-3.53980421795471,5.17037877053785,0.481641101229505));
#84795=CARTESIAN_POINT('Ctrl Pts',(-3.46082269571608,4.52293098642232,1.96892791915868));
#84796=CARTESIAN_POINT('Ctrl Pts',(-3.38184117347744,3.87548320230678,3.45621473708788));
#84797=CARTESIAN_POINT('Ctrl Pts',(-3.3028596512388,2.42274276927944,4.59294152891443));
#84798=CARTESIAN_POINT('Ctrl Pts',(-3.22387812900017,0.823400118075912,
4.86370196309625));
#84799=CARTESIAN_POINT('Ctrl Pts',(-3.14489660676153,-0.775942533127614,
5.13446239727806));
#84800=CARTESIAN_POINT('Ctrl Pts',(-3.0659150845229,-2.52188740250734,4.53925647381515));
#84801=CARTESIAN_POINT('Ctrl Pts',(-2.98693356228426,-3.62280671808846,
3.34796044550116));
#84802=CARTESIAN_POINT('Ctrl Pts',(-2.92756955015737,-4.4502785842728,2.45255972559769));
#84803=CARTESIAN_POINT('Ctrl Pts',(-2.86820553803048,-4.91335544898741,
1.22040916167002));
#84804=CARTESIAN_POINT('Ctrl Pts',(-2.8088415259036,-4.92426410821032,-0.00437867314108101));
#84805=CARTESIAN_POINT('Origin',(-12.,0.,0.));
#84806=CARTESIAN_POINT('',(-1.0911584740964,-4.93200687334489,0.00268308223936954));
#84807=CARTESIAN_POINT('',(-1.30884152590359,-4.93160574955951,0.00236265628207036));
#84808=CARTESIAN_POINT('',(-12.,-4.925,-6.03138548580071E-16));
#84809=CARTESIAN_POINT('Ctrl Pts',(-1.0911584740964,-4.93200687334489,0.00268308223936954));
#84810=CARTESIAN_POINT('Ctrl Pts',(-1.09771688278017,-4.93287970031965,
0.137538864357011));
#84811=CARTESIAN_POINT('Ctrl Pts',(-1.10427529146395,-4.92789883599096,
0.272326647907248));
#84812=CARTESIAN_POINT('Ctrl Pts',(-1.11083370014772,-4.9168679637995,0.406605328980769));
#84813=CARTESIAN_POINT('Ctrl Pts',(-1.18981522238635,-4.78402551385315,
2.02369495342365));
#84814=CARTESIAN_POINT('Ctrl Pts',(-1.26879674462499,-3.77375809971144,
3.56695009160872));
#84815=CARTESIAN_POINT('Ctrl Pts',(-1.34777826686363,-2.3466871175824,4.33849087224895));
#84816=CARTESIAN_POINT('Ctrl Pts',(-1.42675978910226,-0.919616135453348,
5.11003165288917));
#84817=CARTESIAN_POINT('Ctrl Pts',(-1.5057413113409,0.924258414663064,5.10985807598457));
#84818=CARTESIAN_POINT('Ctrl Pts',(-1.58472283357954,2.35021224641849,4.33709640744291));
#84819=CARTESIAN_POINT('Ctrl Pts',(-1.66370435581817,3.77616607817389,3.56433473890127));
#84820=CARTESIAN_POINT('Ctrl Pts',(-1.74268587805681,4.78419919156834,2.01898497872259));
#84821=CARTESIAN_POINT('Ctrl Pts',(-1.82166740029545,4.91657901060328,0.402220613908327));
#84822=CARTESIAN_POINT('Ctrl Pts',(-1.90064892253408,5.04895882963822,-1.21454375090592));
#84823=CARTESIAN_POINT('Ctrl Pts',(-1.97963044477271,4.30568535431372,-2.90272272035571));
#84824=CARTESIAN_POINT('Ctrl Pts',(-2.05861196701135,3.02412028001077,-3.89713434643312));
#84825=CARTESIAN_POINT('Ctrl Pts',(-2.13759348924998,1.74255520570778,-4.89154597251055));
#84826=CARTESIAN_POINT('Ctrl Pts',(-2.21657501148862,-0.0773014675737066,
-5.1921902552155));
#84827=CARTESIAN_POINT('Ctrl Pts',(-2.29555653372726,-1.61049013445835,
-4.66261781559276));
#84828=CARTESIAN_POINT('Ctrl Pts',(-2.3745380559659,-3.143678801343,-4.13304537597002));
#84829=CARTESIAN_POINT('Ctrl Pts',(-2.45351957820454,-4.39019946183083,
-2.7732562140196));
#84830=CARTESIAN_POINT('Ctrl Pts',(-2.53250110044317,-4.78477004695423,
-1.19986364252654));
#84831=CARTESIAN_POINT('Ctrl Pts',(-2.55205355832758,-4.88244890308899,
-0.810358716338717));
#84832=CARTESIAN_POINT('Ctrl Pts',(-2.57160601621199,-4.92791629602104,
-0.407763179703401));
#84833=CARTESIAN_POINT('Ctrl Pts',(-2.5911584740964,-4.92431925468094,-0.00436907230553341));
#84834=CARTESIAN_POINT('Ctrl Pts',(-2.8088415259036,-4.92426410821032,-0.00437867314108101));
#84835=CARTESIAN_POINT('Ctrl Pts',(-2.78922401579185,-4.92786899819237,
-0.409123684020632));
#84836=CARTESIAN_POINT('Ctrl Pts',(-2.7696065056801,-4.88209500064219,-0.813064650368606));
#84837=CARTESIAN_POINT('Ctrl Pts',(-2.74998899556835,-4.78377456269397,
-1.20378326321075));
#84838=CARTESIAN_POINT('Ctrl Pts',(-2.67100747332972,-4.38792932993585,
-2.77684481044359));
#84839=CARTESIAN_POINT('Ctrl Pts',(-2.59202595109108,-3.14034510263708,
-4.13558177174419));
#84840=CARTESIAN_POINT('Ctrl Pts',(-2.51304442885244,-1.60670226458731,
-4.66391570202061));
#84841=CARTESIAN_POINT('Ctrl Pts',(-2.43406290661381,-0.0730594265375867,
-5.19224963229702));
#84842=CARTESIAN_POINT('Ctrl Pts',(-2.35508138437518,1.74664202226318,-4.89018053154927));
#84843=CARTESIAN_POINT('Ctrl Pts',(-2.27609986213654,3.02735160190436,-3.89469276235409));
#84844=CARTESIAN_POINT('Ctrl Pts',(-2.19711833989791,4.30806118154559,-2.89920499315886));
#84845=CARTESIAN_POINT('Ctrl Pts',(-2.11813681765927,5.04977889202728,-1.21029855551616));
#84846=CARTESIAN_POINT('Ctrl Pts',(-2.03915529542063,4.91615834188518,0.406301359031337));
#84847=CARTESIAN_POINT('Ctrl Pts',(-1.96017377318199,4.78253779174308,2.02290127357878));
#84848=CARTESIAN_POINT('Ctrl Pts',(-1.88119225094336,3.77357898097728,3.56719466503099));
#84849=CARTESIAN_POINT('Ctrl Pts',(-1.80221072870473,2.34683826566193,4.33889729935906));
#84850=CARTESIAN_POINT('Ctrl Pts',(-1.72322920646609,0.920097550346556,
5.11059993368714));
#84851=CARTESIAN_POINT('Ctrl Pts',(-1.64424768422745,-0.924425069518355,
5.10971181089104));
#84852=CARTESIAN_POINT('Ctrl Pts',(-1.56526616198882,-2.35056209376295,
4.33679759797832));
#84853=CARTESIAN_POINT('Ctrl Pts',(-1.48628463975018,-3.77669911800752,
3.56388338506561));
#84854=CARTESIAN_POINT('Ctrl Pts',(-1.40730311751155,-4.78445054663177,
2.01894308203631));
#84855=CARTESIAN_POINT('Ctrl Pts',(-1.32832159527291,-4.91658376485791,
0.402158723870856));
#84856=CARTESIAN_POINT('Ctrl Pts',(-1.32182823881647,-4.9274469143815,0.269237037212939));
#84857=CARTESIAN_POINT('Ctrl Pts',(-1.31533488236003,-4.93239169170165,
0.135829750947967));
#84858=CARTESIAN_POINT('Ctrl Pts',(-1.30884152590359,-4.93160574955951,
0.00236265628207036));
#84859=CARTESIAN_POINT('Origin',(-26.8478126690739,0.,0.));
#84860=CARTESIAN_POINT('',(-0.597812669073861,-4.07629116303561,0.00221756066080352));
#84861=CARTESIAN_POINT('',(-0.4,-4.0705,-3.86641296674787E-13));
#84862=CARTESIAN_POINT('',(-26.8478126690739,-4.0705,-3.86641296674787E-13));
#84863=CARTESIAN_POINT('',(-0.399999999999999,-2.75232012058015,-3.00608727173434));
#84864=CARTESIAN_POINT('Ctrl Pts',(-0.597812669073861,-4.07629116303561,
0.00221756066080327));
#84865=CARTESIAN_POINT('Ctrl Pts',(-0.531875112715907,-4.06903839051772,
-1.11836915205891));
#84866=CARTESIAN_POINT('Ctrl Pts',(-0.465937556357953,-3.57275045796359,
-2.24463667173769));
#84867=CARTESIAN_POINT('Ctrl Pts',(-0.399999999999999,-2.75232012058015,
-3.00608727173434));
#84868=CARTESIAN_POINT('Origin',(-0.4,0.,0.));
#84869=CARTESIAN_POINT('Origin',(-26.8478126690739,0.,0.));
#84870=CARTESIAN_POINT('',(-2.09781266907387,-4.06993736572157,-0.00361102717157364));
#84871=CARTESIAN_POINT('',(-1.80218733092609,-4.07595963524507,0.00195272942007198));
#84872=CARTESIAN_POINT('',(-26.8478126690739,-4.0705,-3.86641296674787E-13));
#84873=CARTESIAN_POINT('Ctrl Pts',(-2.09781266907387,-4.06993736572157,
-0.00361102717157308));
#84874=CARTESIAN_POINT('Ctrl Pts',(-2.07826021118946,-4.07291031125962,
-0.337015233093018));
#84875=CARTESIAN_POINT('Ctrl Pts',(-1.97972623106641,-3.88353374239935,
-2.01386882969969));
#84876=CARTESIAN_POINT('Ctrl Pts',(-1.80221072870472,-1.56799638829454,
-4.53981380438684));
#84877=CARTESIAN_POINT('Ctrl Pts',(-1.56526616198882,2.94432437633009,-3.79436859458956));
#84878=CARTESIAN_POINT('Ctrl Pts',(-1.32832159527291,4.78726529895451,0.391458306006858));
#84879=CARTESIAN_POINT('Ctrl Pts',(-1.091377028557,2.2878548696719,4.22314126974725));
#84880=CARTESIAN_POINT('Ctrl Pts',(-0.854432461841093,-2.28401803768771,
4.22357165236047));
#84881=CARTESIAN_POINT('Ctrl Pts',(-0.689911008680048,-4.02331967771076,
1.56666502026864));
#84882=CARTESIAN_POINT('Ctrl Pts',(-0.604371077757637,-4.07701255231495,
0.113675522307533));
#84883=CARTESIAN_POINT('Ctrl Pts',(-0.597812669073861,-4.07629116303561,
0.00221756066080327));
#84884=CARTESIAN_POINT('',(-0.4,-3.73359974356525,1.62148179294418));
#84885=CARTESIAN_POINT('Origin',(-0.4,0.,0.));
#84886=CARTESIAN_POINT('Ctrl Pts',(-1.8021873309261,-4.07595963524507,0.0019527294200722));
#84887=CARTESIAN_POINT('Ctrl Pts',(-1.72969916514391,-4.06870809992297,
-1.22948823727804));
#84888=CARTESIAN_POINT('Ctrl Pts',(-1.57822947712309,-2.82015237778342,
-3.81555274243349));
#84889=CARTESIAN_POINT('Ctrl Pts',(-1.34777826686363,1.56724719957269,-4.53861602703052));
#84890=CARTESIAN_POINT('Ctrl Pts',(-1.11083370014772,4.66076829913842,-1.17009430681153));
#84891=CARTESIAN_POINT('Ctrl Pts',(-0.873889133431818,3.52050501373642,
3.26683163619313));
#84892=CARTESIAN_POINT('Ctrl Pts',(-0.676435327835224,-0.0771870156949762,
4.48297617612786));
#84893=CARTESIAN_POINT('Ctrl Pts',(-0.518472283357957,-2.61623498089622,
3.32972304474434));
#84894=CARTESIAN_POINT('Ctrl Pts',(-0.439490761119318,-3.46537663594235,
2.23908831199168));
#84895=CARTESIAN_POINT('Ctrl Pts',(-0.4,-3.73359974356525,1.62148179294418));
#84896=CARTESIAN_POINT('Origin',(-26.8478126690739,0.,0.));
#84897=CARTESIAN_POINT('',(-3.59781266907387,-4.06463513180001,0.00163755274865575));
#84898=CARTESIAN_POINT('',(-3.3021873309261,-4.06989178730358,-0.00361896223824931));
#84899=CARTESIAN_POINT('',(-26.8478126690739,-4.0705,-3.86641296674787E-13));
#84900=CARTESIAN_POINT('Ctrl Pts',(-3.59781266907387,-4.06463513180001,
0.00163755274865576));
#84901=CARTESIAN_POINT('Ctrl Pts',(-3.55214934462127,-4.06177678722871,
-0.779568156010273));
#84902=CARTESIAN_POINT('Ctrl Pts',(-3.42750449793004,-3.46947945121757,
-2.91599699349249));
#84903=CARTESIAN_POINT('Ctrl Pts',(-3.22387812900017,-0.021433631162604,
-4.80289161377419));
#84904=CARTESIAN_POINT('Ctrl Pts',(-2.98693356228425,4.01022615884859,-2.64315364876519));
#84905=CARTESIAN_POINT('Ctrl Pts',(-2.74998899556836,4.40533498750148,1.91344654900335));
#84906=CARTESIAN_POINT('Ctrl Pts',(-2.51304442885244,0.805564524686711,
4.73490724686727));
#84907=CARTESIAN_POINT('Ctrl Pts',(-2.29565232002095,-3.1673390925526,3.38410818030933));
#84908=CARTESIAN_POINT('Ctrl Pts',(-2.15724173342809,-4.06090119376066,
1.00976029048111));
#84909=CARTESIAN_POINT('Ctrl Pts',(-2.09781266907387,-4.06993736572157,
-0.00361102717157308));
#84910=CARTESIAN_POINT('Ctrl Pts',(-3.3021873309261,-4.06989178730358,-0.00361896223824917));
#84911=CARTESIAN_POINT('Ctrl Pts',(-3.28256982081436,-4.07287121972424,
-0.338139686458441));
#84912=CARTESIAN_POINT('Ctrl Pts',(-3.18397078846399,-3.8827243702829,-2.01612514156527));
#84913=CARTESIAN_POINT('Ctrl Pts',(-3.00639023387498,-1.56436205950543,
-4.54104048789013));
#84914=CARTESIAN_POINT('Ctrl Pts',(-2.76944566715907,2.94757382720121,-3.79206245260455));
#84915=CARTESIAN_POINT('Ctrl Pts',(-2.53250110044317,4.78665724274367,0.395568199836796));
#84916=CARTESIAN_POINT('Ctrl Pts',(-2.29555653372726,2.28495155387725,4.2246319053635));
#84917=CARTESIAN_POINT('Ctrl Pts',(-2.05861196701135,-2.28852823748934,
4.22242981165284));
#84918=CARTESIAN_POINT('Ctrl Pts',(-1.89415556607763,-4.02281228208769,
1.56367365284633));
#84919=CARTESIAN_POINT('Ctrl Pts',(-1.80868068738254,-4.07660921443078,
0.11226294441258));
#84920=CARTESIAN_POINT('Ctrl Pts',(-1.8021873309261,-4.07595963524507,0.0019527294200722));
#84921=CARTESIAN_POINT('Origin',(-26.8478126690739,0.,0.));
#84922=CARTESIAN_POINT('',(-5.09781266907386,-4.07566883909993,0.00207945715039542));
#84923=CARTESIAN_POINT('',(-4.8021873309261,-4.06464833292248,0.00165346759433443));
#84924=CARTESIAN_POINT('',(-26.8478126690739,-4.0705,-3.86641296674787E-13));
#84925=CARTESIAN_POINT('Ctrl Pts',(-5.09781266907386,-4.07566883909993,
0.00207945715039548));
#84926=CARTESIAN_POINT('Ctrl Pts',(-5.02603847805308,-4.06802670929178,
-1.21733178462092));
#84927=CARTESIAN_POINT('Ctrl Pts',(-4.87528276479367,-2.84119087257745,
-3.79195219447061));
#84928=CARTESIAN_POINT('Ctrl Pts',(-4.6455455292956,1.52750104386647,-4.55356519178499));
#84929=CARTESIAN_POINT('Ctrl Pts',(-4.40860096257971,4.64807557048283,-1.20979659769575));
#84930=CARTESIAN_POINT('Ctrl Pts',(-4.17165639586379,3.55367133301375,3.23104246687973));
#84931=CARTESIAN_POINT('Ctrl Pts',(-3.93471182914789,-0.763282093062437,
4.74190020866793));
#84932=CARTESIAN_POINT('Ctrl Pts',(-3.74343058688458,-3.68951325648252,
2.49022401471519));
#84933=CARTESIAN_POINT('Ctrl Pts',(-3.6311308668599,-4.06672071998065,0.571643495768228));
#84934=CARTESIAN_POINT('Ctrl Pts',(-3.59781266907387,-4.06463513180001,
0.00163755274865576));
#84935=CARTESIAN_POINT('Ctrl Pts',(-4.8021873309261,-4.06464833292248,0.00165346759433443));
#84936=CARTESIAN_POINT('Ctrl Pts',(-4.75645895424617,-4.06175727131862,
-0.78065860445274));
#84937=CARTESIAN_POINT('Ctrl Pts',(-4.63174905532762,-3.46819584903415,
-2.91823041531605));
#84938=CARTESIAN_POINT('Ctrl Pts',(-4.42805763417042,-0.0175089406698063,
-4.80290610693659));
#84939=CARTESIAN_POINT('Ctrl Pts',(-4.19111306745452,4.01238817079558,-2.63987635628594));
#84940=CARTESIAN_POINT('Ctrl Pts',(-3.9541685007386,4.40376331119336,1.91705089973334));
#84941=CARTESIAN_POINT('Ctrl Pts',(-3.71722393402271,0.801704468977416,
4.73555632478705));
#84942=CARTESIAN_POINT('Ctrl Pts',(-3.49989687741853,-3.16893402598616,
3.38193537513361));
#84943=CARTESIAN_POINT('Ctrl Pts',(-3.361551343053,-4.06087580814292,1.00866507463471));
#84944=CARTESIAN_POINT('Ctrl Pts',(-3.3021873309261,-4.06989178730358,-0.00361896223824917));
#84945=CARTESIAN_POINT('Origin',(-26.8478126690739,0.,0.));
#84946=CARTESIAN_POINT('',(-6.59781266907387,-4.07024966429081,-0.00362411170895328));
#84947=CARTESIAN_POINT('',(-6.3021873309261,-4.07569093726617,0.00206331041636865));
#84948=CARTESIAN_POINT('',(-26.8478126690739,-4.0705,-3.86641296674787E-13));
#84949=CARTESIAN_POINT('Ctrl Pts',(-6.59781266907387,-4.07024966429081,
-0.00362411170895308));
#84950=CARTESIAN_POINT('Ctrl Pts',(-6.57890913372353,-4.07314624420103,
-0.325897404679135));
#84951=CARTESIAN_POINT('Ctrl Pts',(-6.48102407613457,-3.89142584068926,
-1.99144484346476));
#84952=CARTESIAN_POINT('Ctrl Pts',(-6.30415749630696,-1.60505193339804,
-4.52681160940636));
#84953=CARTESIAN_POINT('Ctrl Pts',(-6.06721292959105,2.91345381090988,-3.81837687463714));
#84954=CARTESIAN_POINT('Ctrl Pts',(-5.83026836287515,4.78997440289178,0.352647507803434));
#84955=CARTESIAN_POINT('Ctrl Pts',(-5.59332379615923,2.322838960361,4.20388323073168));
#84956=CARTESIAN_POINT('Ctrl Pts',(-5.35637922944334,-2.25069887035317,
4.24294351890926));
#84957=CARTESIAN_POINT('Ctrl Pts',(-5.1912088537482,-4.01610269075381,1.58807231517304));
#84958=CARTESIAN_POINT('Ctrl Pts',(-5.10502000029171,-4.07643623696194,
0.124528774728565));
#84959=CARTESIAN_POINT('Ctrl Pts',(-5.09781266907386,-4.07566883909993,
0.00207945715039548));
#84960=CARTESIAN_POINT('Ctrl Pts',(-6.3021873309261,-4.07569093726617,0.00206331041636901));
#84961=CARTESIAN_POINT('Ctrl Pts',(-6.23034808767799,-4.06809019538989,
-1.21843532036503));
#84962=CARTESIAN_POINT('Ctrl Pts',(-6.07952732219125,-2.83932709572212,
-3.79405859128264));
#84963=CARTESIAN_POINT('Ctrl Pts',(-5.84972503446587,1.53122279065449,-4.55231461594934));
#84964=CARTESIAN_POINT('Ctrl Pts',(-5.61278046774996,4.6490626950213,-1.20599647826086));
#84965=CARTESIAN_POINT('Ctrl Pts',(-5.37583590103405,3.55102848107464,3.23394623945287));
#84966=CARTESIAN_POINT('Ctrl Pts',(-5.13889133431815,-0.767157925271441,
4.74127415374739));
#84967=CARTESIAN_POINT('Ctrl Pts',(-4.94767514428216,-3.69055317518662,
2.48797370675018));
#84968=CARTESIAN_POINT('Ctrl Pts',(-4.83544047648481,-4.06675067941523,
0.570541739885505));
#84969=CARTESIAN_POINT('Ctrl Pts',(-4.8021873309261,-4.06464833292248,0.00165346759433443));
#84970=CARTESIAN_POINT('Origin',(-26.8478126690739,0.,0.));
#84971=CARTESIAN_POINT('',(-8.09781266907387,-4.06450654082374,0.00147586284968758));
#84972=CARTESIAN_POINT('',(-7.8021873309261,-4.07021649832878,-0.00362428100020962));
#84973=CARTESIAN_POINT('',(-26.8478126690739,-4.0705,-3.86641296674787E-13));
#84974=CARTESIAN_POINT('Ctrl Pts',(-8.09781266907387,-4.06450654082374,
0.00147586284968748));
#84975=CARTESIAN_POINT('Ctrl Pts',(-8.05279826715535,-4.0619715081721,-0.768689145848125));
#84976=CARTESIAN_POINT('Ctrl Pts',(-7.9288023429982,-3.48220316311878,-2.89371114037708));
#84977=CARTESIAN_POINT('Ctrl Pts',(-7.7258248966024,-0.0605998926332336,
-4.80255585185065));
#84978=CARTESIAN_POINT('Ctrl Pts',(-7.48888032988651,3.98854254916481,-2.67576968195071));
#84979=CARTESIAN_POINT('Ctrl Pts',(-7.25193576317058,4.42078530124335,1.87746434781877));
#84980=CARTESIAN_POINT('Ctrl Pts',(-7.01499119645469,0.844160957960478,
4.72817166925782));
#84981=CARTESIAN_POINT('Ctrl Pts',(-6.79695016508911,-3.15155064707133,
3.40590389765473));
#84982=CARTESIAN_POINT('Ctrl Pts',(-6.65789065596217,-4.06104394236409,
1.02060391287446));
#84983=CARTESIAN_POINT('Ctrl Pts',(-6.59781266907387,-4.07024966429081,
-0.00362411170895308));
#84984=CARTESIAN_POINT('Ctrl Pts',(-7.8021873309261,-4.07021649832878,-0.00362428100020934));
#84985=CARTESIAN_POINT('Ctrl Pts',(-7.78321874334844,-4.07312102749033,
-0.327013257474892));
#84986=CARTESIAN_POINT('Ctrl Pts',(-7.68526863353215,-3.89063799663387,
-1.99369332115123));
#84987=CARTESIAN_POINT('Ctrl Pts',(-7.50833700147722,-1.60135074079071,
-4.52812183462507));
#84988=CARTESIAN_POINT('Ctrl Pts',(-7.2713924347613,2.91657402449002,-3.81599364587164));
#84989=CARTESIAN_POINT('Ctrl Pts',(-7.03444786804541,4.78968416005308,0.356563023868872));
#84990=CARTESIAN_POINT('Ctrl Pts',(-6.79750330132949,2.31940145568391,4.2057803592973));
#84991=CARTESIAN_POINT('Ctrl Pts',(-6.5605587346136,-2.25416642273435,4.24110189585783));
#84992=CARTESIAN_POINT('Ctrl Pts',(-6.39545341114579,-4.01670480150413,
1.58583480923292));
#84993=CARTESIAN_POINT('Ctrl Pts',(-6.30932960991663,-4.07644660529051,
0.123405648315058));
#84994=CARTESIAN_POINT('Ctrl Pts',(-6.3021873309261,-4.07569093726617,0.00206331041636901));
#84995=CARTESIAN_POINT('Origin',(-26.8478126690739,0.,0.));
#84996=CARTESIAN_POINT('',(-9.59781266907388,-4.07543761133748,0.00223681958108363));
#84997=CARTESIAN_POINT('',(-9.30218733092611,-4.06451849691004,0.00149222602727483));
#84998=CARTESIAN_POINT('',(-26.8478126690739,-4.0705,-3.86641296674787E-13));
#84999=CARTESIAN_POINT('Ctrl Pts',(-9.59781266907388,-4.07543761133748,
0.00223681958108334));
#85000=CARTESIAN_POINT('Ctrl Pts',(-9.52668740058717,-4.06740685118034,
-1.20633045978605));
#85001=CARTESIAN_POINT('Ctrl Pts',(-9.37658060986182,-2.85969592298694,
-3.77090943721607));
#85002=CARTESIAN_POINT('Ctrl Pts',(-9.14749229689786,1.49031812597541,-4.56586979014612));
#85003=CARTESIAN_POINT('Ctrl Pts',(-8.91054773018194,4.63805579586533,-1.24765920492107));
#85004=CARTESIAN_POINT('Ctrl Pts',(-8.67360316346604,3.57990062094709,3.20195668323646));
#85005=CARTESIAN_POINT('Ctrl Pts',(-8.43665859675013,-0.724588593371072,
4.74796655711994));
#85006=CARTESIAN_POINT('Ctrl Pts',(-8.24472843195274,-3.67907357692905,
2.51267002599099));
#85007=CARTESIAN_POINT('Ctrl Pts',(-8.13177978939398,-4.06641943437389,
0.582629591474945));
#85008=CARTESIAN_POINT('Ctrl Pts',(-8.09781266907387,-4.06450654082374,
0.00147586284968748));
#85009=CARTESIAN_POINT('Ctrl Pts',(-9.30218733092611,-4.06451849691004,
0.00149222602727511));
#85010=CARTESIAN_POINT('Ctrl Pts',(-9.25710787678026,-4.06195119816851,
-0.76977989625584));
#85011=CARTESIAN_POINT('Ctrl Pts',(-9.13304690039577,-3.48093330077731,
-2.89594568183173));
#85012=CARTESIAN_POINT('Ctrl Pts',(-8.93000440177266,-0.0566739212580544,
-4.80260342014054));
#85013=CARTESIAN_POINT('Ctrl Pts',(-8.69305983505675,3.99072827488727,-2.67250806931295));
#85014=CARTESIAN_POINT('Ctrl Pts',(-8.45611526834084,4.41924871633079,1.88107743798526));
#85015=CARTESIAN_POINT('Ctrl Pts',(-8.21917070162494,0.840295471934814,
4.72885980594699));
#85016=CARTESIAN_POINT('Ctrl Pts',(-8.00119472248669,-3.15314178729772,
3.40372167243926));
#85017=CARTESIAN_POINT('Ctrl Pts',(-7.86220026558708,-4.06102713100874,
1.01951576228452));
#85018=CARTESIAN_POINT('Ctrl Pts',(-7.8021873309261,-4.07021649832878,-0.00362428100020934));
#85019=CARTESIAN_POINT('Origin',(-26.8478126690739,0.,0.));
#85020=CARTESIAN_POINT('',(-11.0978126690739,-4.07057840008889,-0.00361717664568562));
#85021=CARTESIAN_POINT('',(-10.8021873309261,-4.07546109772978,0.00222135529329905));
#85022=CARTESIAN_POINT('',(-26.8478126690739,-4.0705,-3.86641296674787E-13));
#85023=CARTESIAN_POINT('Ctrl Pts',(-11.0978126690739,-4.07057840008889,
-0.00361717664568554));
#85024=CARTESIAN_POINT('Ctrl Pts',(-11.0795580562576,-4.07339138512556,
-0.314763099123047));
#85025=CARTESIAN_POINT('Ctrl Pts',(-10.9823219212027,-3.8992231551958,-1.96901630061212));
#85026=CARTESIAN_POINT('Ctrl Pts',(-10.8061042639092,-1.64191250099602,
-4.51357268649284));
#85027=CARTESIAN_POINT('Ctrl Pts',(-10.5691596971933,2.88221994700369,-3.84200770877353));
#85028=CARTESIAN_POINT('Ctrl Pts',(-10.3322151304774,4.79269081226222,0.313575884338453));
#85029=CARTESIAN_POINT('Ctrl Pts',(-10.0952705637615,2.35704233746519,4.18480184436228));
#85030=CARTESIAN_POINT('Ctrl Pts',(-9.85832599704557,-2.21602490467178,
4.26115579145559));
#85031=CARTESIAN_POINT('Ctrl Pts',(-9.69250669881637,-4.0100399692706,1.61039529938039));
#85032=CARTESIAN_POINT('Ctrl Pts',(-9.6056689228258,-4.07632466162154,0.135731025297307));
#85033=CARTESIAN_POINT('Ctrl Pts',(-9.59781266907388,-4.07543761133748,
0.00223681958108334));
#85034=CARTESIAN_POINT('Ctrl Pts',(-10.8021873309261,-4.07546109772978,
0.00222135529329927));
#85035=CARTESIAN_POINT('Ctrl Pts',(-10.7309970102121,-4.06746733027052,
-1.20743258301197));
#85036=CARTESIAN_POINT('Ctrl Pts',(-10.5808251672594,-2.85784756339483,
-3.7730208783109));
#85037=CARTESIAN_POINT('Ctrl Pts',(-10.3516718020681,1.49404997724334,-4.56464962620395));
#85038=CARTESIAN_POINT('Ctrl Pts',(-10.1147272353522,4.63907381730574,-1.24386722044341));
#85039=CARTESIAN_POINT('Ctrl Pts',(-9.8777826686363,3.57728164792448,3.20488183181962));
#85040=CARTESIAN_POINT('Ctrl Pts',(-9.64083810192037,-0.728469617480856,
4.74737227957853));
#85041=CARTESIAN_POINT('Ctrl Pts',(-9.44897298935032,-3.68012533608753,
2.51041990486184));
#85042=CARTESIAN_POINT('Ctrl Pts',(-9.3360893990189,-4.06644923760776,0.581528530883969));
#85043=CARTESIAN_POINT('Ctrl Pts',(-9.30218733092611,-4.06451849691004,
0.00149222602727511));
#85044=CARTESIAN_POINT('Origin',(-26.8478126690739,0.,0.));
#85045=CARTESIAN_POINT('',(-12.5978126690739,-4.06439173936514,0.00131077860369149));
#85046=CARTESIAN_POINT('',(-12.3021873309261,-4.07054506653231,-0.00361830226162985));
#85047=CARTESIAN_POINT('',(-26.8478126690739,-4.0705,-3.86641296674787E-13));
#85048=CARTESIAN_POINT('Ctrl Pts',(-12.5978126690739,-4.06439173936514,
0.00131077860369144));
#85049=CARTESIAN_POINT('Ctrl Pts',(-12.5534471896894,-4.06217639157224,
-0.757805274824507));
#85050=CARTESIAN_POINT('Ctrl Pts',(-12.4301001880664,-3.49479538377389,
-2.87141087514505));
#85051=CARTESIAN_POINT('Ctrl Pts',(-12.2277716642046,-0.0997603707836814,
-4.80190201124536));
#85052=CARTESIAN_POINT('Ctrl Pts',(-11.9908270974887,3.96659034332826,-2.70820532925335));
#85053=CARTESIAN_POINT('Ctrl Pts',(-11.7538825307728,4.43594811954626,1.84135258380226));
#85054=CARTESIAN_POINT('Ctrl Pts',(-11.5169379640569,0.882688817166835,
4.72113074477184));
#85055=CARTESIAN_POINT('Ctrl Pts',(-11.2982480101573,-3.1355959094005,3.4276518469622));
#85056=CARTESIAN_POINT('Ctrl Pts',(-11.1585395784963,-4.06122055233565,
1.03145984424838));
#85057=CARTESIAN_POINT('Ctrl Pts',(-11.0978126690739,-4.07057840008889,
-0.00361717664568554));
#85058=CARTESIAN_POINT('Ctrl Pts',(-12.3021873309261,-4.07054506653231,
-0.00361830226162995));
#85059=CARTESIAN_POINT('Ctrl Pts',(-12.2838676658825,-4.07336677593993,
-0.315879491868212));
#85060=CARTESIAN_POINT('Ctrl Pts',(-12.1865664786003,-3.89844601596142,
-1.97126432893802));
#85061=CARTESIAN_POINT('Ctrl Pts',(-12.0102837690795,-1.63822211600786,
-4.514913049343));
#85062=CARTESIAN_POINT('Ctrl Pts',(-11.7733392023635,2.88535949150936,-3.83965000348491));
#85063=CARTESIAN_POINT('Ctrl Pts',(-11.5363946356477,4.79243250703115,0.317493637819545));
#85064=CARTESIAN_POINT('Ctrl Pts',(-11.2994500689317,2.35362041946459,4.18672693945812));
#85065=CARTESIAN_POINT('Ctrl Pts',(-11.0625055022158,-2.21950736358003,
4.25934250882913));
#85066=CARTESIAN_POINT('Ctrl Pts',(-10.8967512562139,-4.0106518183616,1.60815703963873));
#85067=CARTESIAN_POINT('Ctrl Pts',(-10.8099785324507,-4.07633595055516,
0.134608139252678));
#85068=CARTESIAN_POINT('Ctrl Pts',(-10.8021873309261,-4.07546109772978,
0.00222135529329927));
#85069=CARTESIAN_POINT('Origin',(-26.8478126690739,0.,0.));
#85070=CARTESIAN_POINT('',(-14.0978126690739,-4.07519307943845,0.00238714832353424));
#85071=CARTESIAN_POINT('',(-13.8021873309261,-4.0644023160722,0.00132747365239078));
#85072=CARTESIAN_POINT('',(-26.8478126690739,-4.0705,-3.86641296674787E-13));
#85073=CARTESIAN_POINT('Ctrl Pts',(-14.0978126690739,-4.07519307943845,
0.00238714832353427));
#85074=CARTESIAN_POINT('Ctrl Pts',(-14.0273363231212,-4.06681676123038,
-1.19534282954133));
#85075=CARTESIAN_POINT('Ctrl Pts',(-13.87787845493,-2.87804755341778,-3.74981687266502));
#85076=CARTESIAN_POINT('Ctrl Pts',(-13.6494390645001,1.45303614102348,-4.57787079656698));
#85077=CARTESIAN_POINT('Ctrl Pts',(-13.4124944977842,4.6277275367991,-1.28543879758337));
#85078=CARTESIAN_POINT('Ctrl Pts',(-13.1755499310683,3.6058919843453,3.17265788486808));
#85079=CARTESIAN_POINT('Ctrl Pts',(-12.9386053643524,-0.68584715780348,
4.75371735942664));
#85080=CARTESIAN_POINT('Ctrl Pts',(-12.7460262770209,-3.66851217096832,
2.53511162155732));
#85081=CARTESIAN_POINT('Ctrl Pts',(-12.6324287119281,-4.06612025836685,
0.593608984356713));
#85082=CARTESIAN_POINT('Ctrl Pts',(-12.5978126690739,-4.06439173936514,
0.00131077860369144));
#85083=CARTESIAN_POINT('Ctrl Pts',(-13.8021873309261,-4.0644023160722,0.00132747365239085));
#85084=CARTESIAN_POINT('Ctrl Pts',(-13.7577567993143,-4.06215511076084,
-0.758896503957548));
#85085=CARTESIAN_POINT('Ctrl Pts',(-13.6343447454639,-3.49353872825462,
-2.87364679360195));
#85086=CARTESIAN_POINT('Ctrl Pts',(-13.4319511693749,-0.0958349178438527,
-4.80198159232485));
#85087=CARTESIAN_POINT('Ctrl Pts',(-13.195006602659,3.96880259324556,-2.70496164859175));
#85088=CARTESIAN_POINT('Ctrl Pts',(-12.9580620359431,4.43444104868229,1.84497808395286));
#85089=CARTESIAN_POINT('Ctrl Pts',(-12.7211174692272,0.878829071125367,
4.72185037969754));
#85090=CARTESIAN_POINT('Ctrl Pts',(-12.5024925675548,-3.13720164930185,
3.42547292377134));
#85091=CARTESIAN_POINT('Ctrl Pts',(-12.3628491881212,-4.06120154782041,
1.03037132835712));
#85092=CARTESIAN_POINT('Ctrl Pts',(-12.3021873309261,-4.07054506653231,
-0.00361830226162995));
#85093=CARTESIAN_POINT('Origin',(-26.8478126690739,0.,0.));
#85094=CARTESIAN_POINT('',(-15.5978126690739,-4.07090838159082,-0.0036006753872044));
#85095=CARTESIAN_POINT('',(-15.3021873309261,-4.07521785360078,0.00237240612388764));
#85096=CARTESIAN_POINT('',(-26.8478126690739,-4.0705,-3.86641296674787E-13));
#85097=CARTESIAN_POINT('Ctrl Pts',(-15.5978126690739,-4.07090838159082,
-0.00360067538720397));
#85098=CARTESIAN_POINT('Ctrl Pts',(-15.5802069787917,-4.0736303253679,-0.303623491996831));
#85099=CARTESIAN_POINT('Ctrl Pts',(-15.4836197662709,-3.90691400355826,
-1.94659239353253));
#85100=CARTESIAN_POINT('Ctrl Pts',(-15.3080510315115,-1.6786638864531,-4.50003362359639));
#85101=CARTESIAN_POINT('Ctrl Pts',(-15.0711064647955,2.85079442437809,-3.86538306085168));
#85102=CARTESIAN_POINT('Ctrl Pts',(-14.8341618980796,4.79508852002207,0.274483409940331));
#85103=CARTESIAN_POINT('Ctrl Pts',(-14.5972173313637,2.39108898052815,4.16544217873422));
#85104=CARTESIAN_POINT('Ctrl Pts',(-14.3602727646478,-2.18120358456222,
4.27908471286496));
#85105=CARTESIAN_POINT('Ctrl Pts',(-14.1938045438845,-4.00387976925298,
1.632725694837));
#85106=CARTESIAN_POINT('Ctrl Pts',(-14.1063178453599,-4.07620394431835,
0.14693074613754));
#85107=CARTESIAN_POINT('Ctrl Pts',(-14.0978126690739,-4.07519307943845,
0.00238714832353427));
#85108=CARTESIAN_POINT('Ctrl Pts',(-15.3021873309261,-4.07521785360078,
0.0023724061238877));
#85109=CARTESIAN_POINT('Ctrl Pts',(-15.2316459327462,-4.06687427621052,
-1.19644361288041));
#85110=CARTESIAN_POINT('Ctrl Pts',(-15.0821230123276,-2.87621455521643,
-3.75193325755229));
#85111=CARTESIAN_POINT('Ctrl Pts',(-14.8536185696703,1.45677781805249,-4.57668110461451));
#85112=CARTESIAN_POINT('Ctrl Pts',(-14.6166740029544,4.62877644616991,-1.28165524065066));
#85113=CARTESIAN_POINT('Ctrl Pts',(-14.3797294362385,3.60329695155474,3.17560429263805));
#85114=CARTESIAN_POINT('Ctrl Pts',(-14.1427848695226,-0.689732898916454,
4.75315474949608));
#85115=CARTESIAN_POINT('Ctrl Pts',(-13.9502708344185,-3.66957612834082,
2.53286193889574));
#85116=CARTESIAN_POINT('Ctrl Pts',(-13.836738321553,-4.06614983443025,0.59250859554932));
#85117=CARTESIAN_POINT('Ctrl Pts',(-13.8021873309261,-4.0644023160722,0.00132747365239085));
#85118=CARTESIAN_POINT('Origin',(-26.8478126690739,0.,0.));
#85119=CARTESIAN_POINT('',(-17.0978126690739,-4.06429080835649,0.00114260236847386));
#85120=CARTESIAN_POINT('',(-16.8021873309261,-4.07087495827563,-0.00360276185568886));
#85121=CARTESIAN_POINT('',(-26.8478126690739,-4.0705,-3.86641296674787E-13));
#85122=CARTESIAN_POINT('Ctrl Pts',(-17.0978126690739,-4.06429080835649,
0.00114260236847394));
#85123=CARTESIAN_POINT('Ctrl Pts',(-17.0540961122235,-4.06239068999993,
-0.746916525723744));
#85124=CARTESIAN_POINT('Ctrl Pts',(-16.9313980331345,-3.50725618954384,
-2.84909725496437));
#85125=CARTESIAN_POINT('Ctrl Pts',(-16.7297184318069,-0.138914215188535,
-4.80092885781891));
#85126=CARTESIAN_POINT('Ctrl Pts',(-16.492773865091,3.94437437056674,-2.74046088863915));
#85127=CARTESIAN_POINT('Ctrl Pts',(-16.2558292983751,4.45081595990773,1.8051183751108));
#85128=CARTESIAN_POINT('Ctrl Pts',(-16.0188847316592,0.921157980137197,
4.71377587850701));
#85129=CARTESIAN_POINT('Ctrl Pts',(-15.7995458552254,-3.11949526030155,
3.44936632830614));
#85130=CARTESIAN_POINT('Ctrl Pts',(-15.6591885010303,-4.06141931520493,
1.04231968787035));
#85131=CARTESIAN_POINT('Ctrl Pts',(-15.5978126690739,-4.07090838159082,
-0.00360067538720397));
#85132=CARTESIAN_POINT('Ctrl Pts',(-16.8021873309261,-4.07087495827563,
-0.00360276185568931));
#85133=CARTESIAN_POINT('Ctrl Pts',(-16.7845165884166,-4.07360634907373,
-0.304740410768458));
#85134=CARTESIAN_POINT('Ctrl Pts',(-16.6878643236685,-3.90614750997477,
-1.94883994785539));
#85135=CARTESIAN_POINT('Ctrl Pts',(-16.5122305366817,-1.67498455417103,
-4.50140403516247));
#85136=CARTESIAN_POINT('Ctrl Pts',(-16.2752859699658,2.85395309043288,-3.86305103540403));
#85137=CARTESIAN_POINT('Ctrl Pts',(-16.0383414032499,4.79486217074114,0.278403139515235));
#85138=CARTESIAN_POINT('Ctrl Pts',(-15.801396836534,2.38768287451035,4.16739511388991));
#85139=CARTESIAN_POINT('Ctrl Pts',(-15.5644522698181,-2.18470071411643,
4.27729988827614));
#85140=CARTESIAN_POINT('Ctrl Pts',(-15.3980491012821,-4.00450141399627,
1.63048669485744));
#85141=CARTESIAN_POINT('Ctrl Pts',(-15.3106274549848,-4.07621614439291,
0.145808121675198));
#85142=CARTESIAN_POINT('Ctrl Pts',(-15.3021873309261,-4.07521785360078,
0.0023724061238877));
#85143=CARTESIAN_POINT('Origin',(-26.8478126690739,0.,0.));
#85144=CARTESIAN_POINT('',(-18.5978126690739,-4.07493625768978,0.00253007724807807));
#85145=CARTESIAN_POINT('',(-18.3021873309261,-4.06429998606454,0.00115958952258771));
#85146=CARTESIAN_POINT('',(-26.8478126690739,-4.0705,-3.86641296674787E-13));
#85147=CARTESIAN_POINT('Ctrl Pts',(-18.5978126690739,-4.07493625768978,
0.00253007724807795));
#85148=CARTESIAN_POINT('Ctrl Pts',(-18.5279852456553,-4.06625599752369,
-1.18436818426556));
#85149=CARTESIAN_POINT('Ctrl Pts',(-18.3791762999982,-2.89624616201064,
-3.72867561089757));
#85150=CARTESIAN_POINT('Ctrl Pts',(-18.1513858321023,1.41565753192185,-4.58956738674043));
#85151=CARTESIAN_POINT('Ctrl Pts',(-17.9144412653864,4.61709154776294,-1.32313291269056));
#85152=CARTESIAN_POINT('Ctrl Pts',(-17.6774966986705,3.63164356582701,3.14314811403285));
#85153=CARTESIAN_POINT('Ctrl Pts',(-17.4405521319546,-0.647060115157983,
4.75915205295132));
#85154=CARTESIAN_POINT('Ctrl Pts',(-17.247324122089,-3.65782874417121,2.55754855348124));
#85155=CARTESIAN_POINT('Ctrl Pts',(-17.1330776344621,-4.06582358250215,
0.604581691838573));
#85156=CARTESIAN_POINT('Ctrl Pts',(-17.0978126690739,-4.06429080835649,
0.00114260236847394));
#85157=CARTESIAN_POINT('Ctrl Pts',(-18.3021873309261,-4.06429998606454,
0.00115958952258736));
#85158=CARTESIAN_POINT('Ctrl Pts',(-18.2584057218484,-4.0623684874239,-0.74800825355675));
#85159=CARTESIAN_POINT('Ctrl Pts',(-18.1356425905321,-3.50601267898312,
-2.8513344844204));
#85160=CARTESIAN_POINT('Ctrl Pts',(-17.9338979369771,-0.134989541855146,
-4.801040446262));
#85161=CARTESIAN_POINT('Ctrl Pts',(-17.6969533702612,3.94661299763452,-2.73723535571292));
#85162=CARTESIAN_POINT('Ctrl Pts',(-17.4600088035453,4.44933850329186,1.80875604418168));
#85163=CARTESIAN_POINT('Ctrl Pts',(-17.2230642368294,0.917304230718045,
4.71452696382671));
#85164=CARTESIAN_POINT('Ctrl Pts',(-17.003790412623,-3.12111565197432,3.44719080073753));
#85165=CARTESIAN_POINT('Ctrl Pts',(-16.8634981106552,-4.06139806733649,
1.0412307560742));
#85166=CARTESIAN_POINT('Ctrl Pts',(-16.8021873309261,-4.07087495827563,
-0.00360276185568931));
#85167=CARTESIAN_POINT('Origin',(-26.8478126690739,0.,0.));
#85168=CARTESIAN_POINT('',(-20.0978126690739,-4.071238829888,-0.00357457003402451));
#85169=CARTESIAN_POINT('',(-19.8021873309261,-4.07496222722346,0.00251610070729075));
#85170=CARTESIAN_POINT('',(-26.8478126690739,-4.0705,-3.86641296674787E-13));
#85171=CARTESIAN_POINT('Ctrl Pts',(-20.0978126690739,-4.071238829888,-0.00357457003402478));
#85172=CARTESIAN_POINT('Ctrl Pts',(-20.0808559013258,-4.07386284930607,
-0.292478704003469));
#85173=CARTESIAN_POINT('Ctrl Pts',(-19.9849176113391,-3.91449912999133,
-1.92417326350588));
#85174=CARTESIAN_POINT('Ctrl Pts',(-19.8099977991137,-1.71530351140438,
-4.48619540698215));
#85175=CARTESIAN_POINT('Ctrl Pts',(-19.5730532323978,2.8191792622351,-3.88850133137423));
#85176=CARTESIAN_POINT('Ctrl Pts',(-19.3361086656818,4.79716740439492,0.23537265996686));
#85177=CARTESIAN_POINT('Ctrl Pts',(-19.099164098966,2.42497660407891,4.14580553515268));
#85178=CARTESIAN_POINT('Ctrl Pts',(-18.86221953225,-2.14623721078936,4.29672908104936));
#85179=CARTESIAN_POINT('Ctrl Pts',(-18.6951023889527,-3.99762156681033,
1.65506339659562));
#85180=CARTESIAN_POINT('Ctrl Pts',(-18.606966767894,-4.07607420543945,0.158127741365762));
#85181=CARTESIAN_POINT('Ctrl Pts',(-18.5978126690739,-4.07493625768978,
0.00253007724807795));
#85182=CARTESIAN_POINT('Ctrl Pts',(-19.8021873309261,-4.07496222722346,
0.0025161007072908));
#85183=CARTESIAN_POINT('Ctrl Pts',(-19.7322948552802,-4.06631060333232,
-1.18546768844045));
#85184=CARTESIAN_POINT('Ctrl Pts',(-19.5834208573957,-2.89442846977801,
-3.73079684269773));
#85185=CARTESIAN_POINT('Ctrl Pts',(-19.3555653372726,1.4194087785671,-4.58840823893679));
#85186=CARTESIAN_POINT('Ctrl Pts',(-19.1186207705567,4.61817127913257,-1.31935803851751));
#85187=CARTESIAN_POINT('Ctrl Pts',(-18.8816762038408,3.62907264384353,3.14611558694568));
#85188=CARTESIAN_POINT('Ctrl Pts',(-18.6447316371248,-0.650950313849541,
4.75862114706335));
#85189=CARTESIAN_POINT('Ctrl Pts',(-18.4515686794867,-3.65890496319905,
2.55529935938178));
#85190=CARTESIAN_POINT('Ctrl Pts',(-18.3373872440871,-4.06585288888957,
0.603481970423879));
#85191=CARTESIAN_POINT('Ctrl Pts',(-18.3021873309261,-4.06429998606454,
0.00115958952258736));
#85192=CARTESIAN_POINT('Origin',(-26.8478126690739,0.,0.));
#85193=CARTESIAN_POINT('',(-21.5978126690739,-4.06419832734502,0.00096815537284884));
#85194=CARTESIAN_POINT('',(-21.3021873309261,-4.07120543337986,-0.00357758459923085));
#85195=CARTESIAN_POINT('',(-26.8478126690739,-4.0705,-3.86641296674787E-13));
#85196=CARTESIAN_POINT('Ctrl Pts',(-21.5978126690739,-4.06419832734502,
0.000968155372848833));
#85197=CARTESIAN_POINT('Ctrl Pts',(-21.5547450347576,-4.06261112671129,
-0.736024486956658));
#85198=CARTESIAN_POINT('Ctrl Pts',(-21.4326958782027,-3.51959617795593,
-2.826764557928));
#85199=CARTESIAN_POINT('Ctrl Pts',(-21.2316651994091,-0.178052071836572,
-4.79964076861094));
#85200=CARTESIAN_POINT('Ctrl Pts',(-20.9947206326932,3.92189259497827,-2.77253197087948));
#85201=CARTESIAN_POINT('Ctrl Pts',(-20.7577760659773,4.46538966209699,1.76876296315944));
#85202=CARTESIAN_POINT('Ctrl Pts',(-20.5208314992614,0.959564937147886,
4.70610816747424));
#85203=CARTESIAN_POINT('Ctrl Pts',(-20.3008437002936,-3.10324779081687,
3.47104615142249));
#85204=CARTESIAN_POINT('Ctrl Pts',(-20.1598374235644,-4.06164064687329,
1.05318390227358));
#85205=CARTESIAN_POINT('Ctrl Pts',(-20.0978126690739,-4.071238829888,-0.00357457003402478));
#85206=CARTESIAN_POINT('Ctrl Pts',(-21.3021873309261,-4.07120543337986,
-0.00357758459923137));
#85207=CARTESIAN_POINT('Ctrl Pts',(-21.2851655109507,-4.07383969984574,
-0.293595973708156));
#85208=CARTESIAN_POINT('Ctrl Pts',(-21.1891621687366,-3.91374404213,-1.92641954377506));
#85209=CARTESIAN_POINT('Ctrl Pts',(-21.0141773042839,-1.71163476880105,
-4.48759644703182));
#85210=CARTESIAN_POINT('Ctrl Pts',(-20.777232737568,2.82235647137499,-3.88619479158027));
#85211=CARTESIAN_POINT('Ctrl Pts',(-20.5402881708521,4.79697321791449,0.239293923164062));
#85212=CARTESIAN_POINT('Ctrl Pts',(-20.3033436041362,2.42158643669063,4.14778627515724));
#85213=CARTESIAN_POINT('Ctrl Pts',(-20.0663990374203,-2.14974872645911,
4.2949727839084));
#85214=CARTESIAN_POINT('Ctrl Pts',(-19.8993469463503,-3.99825306426731,
1.65282367123152));
#85215=CARTESIAN_POINT('Ctrl Pts',(-19.8112763775189,-4.07608731274838,
0.157005406047044));
#85216=CARTESIAN_POINT('Ctrl Pts',(-19.8021873309261,-4.07496222722346,
0.0025161007072908));
#85217=CARTESIAN_POINT('Origin',(-26.8478126690739,0.,0.));
#85218=CARTESIAN_POINT('',(-23.0978126690739,-4.07427440555673,0.00241395537052257));
#85219=CARTESIAN_POINT('',(-22.8021873309261,-4.06417652423825,0.000957366820343863));
#85220=CARTESIAN_POINT('',(-26.8478126690739,-4.0705,-3.86641296674787E-13));
#85221=CARTESIAN_POINT('Ctrl Pts',(-23.0978126690739,-4.07427440555673,
0.002413955370523));
#85222=CARTESIAN_POINT('Ctrl Pts',(-23.0286341681894,-4.06525490317439,
-1.17370585999422));
#85223=CARTESIAN_POINT('Ctrl Pts',(-22.8804741450663,-2.91490401827704,
-3.70709582083626));
#85224=CARTESIAN_POINT('Ctrl Pts',(-22.6533325997046,1.37852450357098,-4.60117581069992));
#85225=CARTESIAN_POINT('Ctrl Pts',(-22.4163880329887,4.60597174073038,-1.36062610156221));
#85226=CARTESIAN_POINT('Ctrl Pts',(-22.1794434662727,3.65724566378385,3.11337055406841));
#85227=CARTESIAN_POINT('Ctrl Pts',(-21.9424988995569,-0.608277930885338,
4.76430086728238));
#85228=CARTESIAN_POINT('Ctrl Pts',(-21.7486219671572,-3.64701097805702,
2.57997285182622));
#85229=CARTESIAN_POINT('Ctrl Pts',(-21.6337265569962,-4.0655218861282,0.615542686256921));
#85230=CARTESIAN_POINT('Ctrl Pts',(-21.5978126690739,-4.06419832734502,
0.000968155372848833));
#85231=CARTESIAN_POINT('Ctrl Pts',(-22.8021873309261,-4.06417652423825,
0.000957366820343933));
#85232=CARTESIAN_POINT('Ctrl Pts',(-22.7590546443825,-4.06257329236665,
-0.737130721986723));
#85233=CARTESIAN_POINT('Ctrl Pts',(-22.6369404356002,-3.51841833318712,
-2.82895318080592));
#85234=CARTESIAN_POINT('Ctrl Pts',(-22.4358447045794,-0.174092888986568,
-4.79981806178492));
#85235=CARTESIAN_POINT('Ctrl Pts',(-22.1989001378634,3.92413894310881,-2.76930725388711));
#85236=CARTESIAN_POINT('Ctrl Pts',(-21.9619555711476,4.46395155275901,1.77240342487198));
#85237=CARTESIAN_POINT('Ctrl Pts',(-21.7250110044316,0.955712424786761,
4.70689540849193));
#85238=CARTESIAN_POINT('Ctrl Pts',(-21.5050882576912,-3.10488082295939,
3.46887215836906));
#85239=CARTESIAN_POINT('Ctrl Pts',(-21.3641470331893,-4.0616166604905,1.05209408070949));
#85240=CARTESIAN_POINT('Ctrl Pts',(-21.3021873309261,-4.07120543337986,
-0.00357758459923137));
#85241=CARTESIAN_POINT('Origin',(-0.4,4.52129938221115E-16,0.));
#85242=CARTESIAN_POINT('',(-0.4,4.77615934004777,-1.20163511869221));
#85243=CARTESIAN_POINT('Ctrl Pts',(-0.399999999999999,-2.75232012058015,
-3.00608727173434));
#85244=CARTESIAN_POINT('Ctrl Pts',(-0.399999999999999,-2.67884530085595,
-3.08970388103118));
#85245=CARTESIAN_POINT('Ctrl Pts',(-0.399999999999998,-2.60192581722023,
-3.16993140988783));
#85246=CARTESIAN_POINT('Ctrl Pts',(-0.399999999999999,-2.52168473419593,
-3.24649039328315));
#85247=CARTESIAN_POINT('Ctrl Pts',(-0.4,-2.43283015801532,-3.33126761420314));
#85248=CARTESIAN_POINT('Ctrl Pts',(-0.399999999999997,-2.33990343083429,
-3.41154791660084));
#85249=CARTESIAN_POINT('Ctrl Pts',(-0.399999999999995,-2.24331760456818,
-3.48732708244347));
#85250=CARTESIAN_POINT('Ctrl Pts',(-0.399999999999994,-2.17934863242522,
-3.53751576473985));
#85251=CARTESIAN_POINT('Ctrl Pts',(-0.399999999999999,-2.11377364367761,
-3.5857294623203));
#85252=CARTESIAN_POINT('Ctrl Pts',(-0.4,-2.04670293396042,-3.63195924784765));
#85253=CARTESIAN_POINT('Ctrl Pts',(-0.4,-2.02167655430602,-3.64920916467166));
#85254=CARTESIAN_POINT('Ctrl Pts',(-0.400000000000003,-1.99644185707205,
-3.66618279846621));
#85255=CARTESIAN_POINT('Ctrl Pts',(-0.400000000000003,-1.97100433623467,
-3.68287944933743));
#85256=CARTESIAN_POINT('Ctrl Pts',(-0.400000000000003,-1.94833071868495,
-3.69776193252576));
#85257=CARTESIAN_POINT('Ctrl Pts',(-0.399999999999998,-1.92549295693954,
-3.71242611279588));
#85258=CARTESIAN_POINT('Ctrl Pts',(-0.399999999999998,-1.90251718347535,
-3.72685775571483));
#85259=CARTESIAN_POINT('Ctrl Pts',(-0.399999999999998,-1.79577386745123,
-3.79390583238766));
#85260=CARTESIAN_POINT('Ctrl Pts',(-0.400000000000007,-1.68596470474815,
-3.85599838796523));
#85261=CARTESIAN_POINT('Ctrl Pts',(-0.400000000000006,-1.57352241925111,
-3.91313343837503));
#85262=CARTESIAN_POINT('Ctrl Pts',(-0.400000000000006,-1.45755473669459,
-3.97205984101337));
#85263=CARTESIAN_POINT('Ctrl Pts',(-0.400000000000004,-1.33878571496281,
-4.02571347884009));
#85264=CARTESIAN_POINT('Ctrl Pts',(-0.400000000000004,-1.21764940630657,
-4.07405401109807));
#85265=CARTESIAN_POINT('Ctrl Pts',(-0.400000000000004,-1.16465227126946,
-4.09520299396094));
#85266=CARTESIAN_POINT('Ctrl Pts',(-0.4,-1.11120155664704,-4.11533448914209));
#85267=CARTESIAN_POINT('Ctrl Pts',(-0.4,-1.05733168943948,-4.13444256176185));
#85268=CARTESIAN_POINT('Ctrl Pts',(-0.4,-1.02977013518471,-4.14421886542683));
#85269=CARTESIAN_POINT('Ctrl Pts',(-0.400000000000004,-1.00209884390297,
-4.15372724442471));
#85270=CARTESIAN_POINT('Ctrl Pts',(-0.400000000000005,-0.974322331280067,
-4.16296673702109));
#85271=CARTESIAN_POINT('Ctrl Pts',(-0.400000000000005,-0.950830465098206,
-4.17078099817797));
#85272=CARTESIAN_POINT('Ctrl Pts',(-0.400000000000003,-0.927260172172898,
-4.1784038296046));
#85273=CARTESIAN_POINT('Ctrl Pts',(-0.400000000000003,-0.903638597056394,
-4.18582717574358));
#85274=CARTESIAN_POINT('Ctrl Pts',(-0.400000000000003,-0.777616734918826,
-4.22543096588513));
#85275=CARTESIAN_POINT('Ctrl Pts',(-0.400000000000009,-0.650003521738759,
-4.25940648821455));
#85276=CARTESIAN_POINT('Ctrl Pts',(-0.400000000000008,-0.521253026605198,
-4.28774813192643));
#85277=CARTESIAN_POINT('Ctrl Pts',(-0.400000000000007,-0.390643175835227,
-4.31649907266608));
#85278=CARTESIAN_POINT('Ctrl Pts',(-0.399999999999999,-0.258862245080765,
-4.33945261889705));
#85279=CARTESIAN_POINT('Ctrl Pts',(-0.4,-0.126350901762778,-4.35656076619393));
#85280=CARTESIAN_POINT('Ctrl Pts',(-0.4,0.00669532870704109,-4.3737379711877));
#85281=CARTESIAN_POINT('Ctrl Pts',(-0.400000000000008,0.140478697090108,
-4.38502282639319));
#85282=CARTESIAN_POINT('Ctrl Pts',(-0.400000000000009,0.274574911972207,
-4.39031924043944));
#85283=CARTESIAN_POINT('Ctrl Pts',(-0.40000000000001,0.375147073133782,
-4.39429155097413));
#85284=CARTESIAN_POINT('Ctrl Pts',(-0.400000000000009,0.475895739149746,
-4.39489441889364));
#85285=CARTESIAN_POINT('Ctrl Pts',(-0.40000000000001,0.576645629621254,
-4.39206814261951));
#85286=CARTESIAN_POINT('Ctrl Pts',(-0.40000000000001,0.621564747135451,
-4.39080805354654));
#85287=CARTESIAN_POINT('Ctrl Pts',(-0.400000000000001,0.666484127834017,
-4.38886609187459));
#85288=CARTESIAN_POINT('Ctrl Pts',(-0.400000000000001,0.711388257581674,
-4.38623584493183));
#85289=CARTESIAN_POINT('Ctrl Pts',(-0.4,0.729692703889777,-4.38516366706731));
#85290=CARTESIAN_POINT('Ctrl Pts',(-0.400000000000005,0.747994987199218,
-4.3839770260269));
#85291=CARTESIAN_POINT('Ctrl Pts',(-0.400000000000005,0.76627878126558,
-4.3826767175198));
#85292=CARTESIAN_POINT('Ctrl Pts',(-0.400000000000004,0.903799577305213,
-4.37289650120665));
#85293=CARTESIAN_POINT('Ctrl Pts',(-0.400000000000001,1.04048239370559,
-4.35667845015307));
#85294=CARTESIAN_POINT('Ctrl Pts',(-0.400000000000001,1.17587220890522,
-4.33397675466201));
#85295=CARTESIAN_POINT('Ctrl Pts',(-0.400000000000001,1.27545468382726,
-4.31727911002314));
#85296=CARTESIAN_POINT('Ctrl Pts',(-0.400000000000001,1.37433826386558,
-4.29707290664842));
#85297=CARTESIAN_POINT('Ctrl Pts',(-0.400000000000001,1.47234696797353,
-4.27332264316194));
#85298=CARTESIAN_POINT('Ctrl Pts',(-0.400000000000001,1.60147130364406,
-4.24203218766002));
#85299=CARTESIAN_POINT('Ctrl Pts',(-0.400000000000009,1.72907757991282,
-4.20459238895073));
#85300=CARTESIAN_POINT('Ctrl Pts',(-0.400000000000011,1.85486206446225,
-4.16133352902126));
#85301=CARTESIAN_POINT('Ctrl Pts',(-0.400000000000013,1.98260002701008,
-4.11740284353705));
#85302=CARTESIAN_POINT('Ctrl Pts',(-0.400000000000002,2.10845986782647,
-4.06747070160946));
#85303=CARTESIAN_POINT('Ctrl Pts',(-0.400000000000002,2.23211522018608,
-4.01182989632834));
#85304=CARTESIAN_POINT('Ctrl Pts',(-0.400000000000003,2.27057077740154,
-3.99452617165995));
#85305=CARTESIAN_POINT('Ctrl Pts',(-0.399999999999999,2.30881302678684,
-3.97666996889792));
#85306=CARTESIAN_POINT('Ctrl Pts',(-0.399999999999999,2.34683182515979,
-3.9582691309213));
#85307=CARTESIAN_POINT('Ctrl Pts',(-0.399999999999999,2.36665698110855,
-3.94867389124813));
#85308=CARTESIAN_POINT('Ctrl Pts',(-0.400000000000004,2.38642137382624,
-3.93893054872392));
#85309=CARTESIAN_POINT('Ctrl Pts',(-0.400000000000004,2.4061235432385,-3.92904016894681));
#85310=CARTESIAN_POINT('Ctrl Pts',(-0.400000000000004,2.42353838620782,
-3.92029801435859));
#85311=CARTESIAN_POINT('Ctrl Pts',(-0.399999999999997,2.44089803817829,
-3.91144424865044));
#85312=CARTESIAN_POINT('Ctrl Pts',(-0.399999999999997,2.45819532721275,
-3.90248319304769));
#85313=CARTESIAN_POINT('Ctrl Pts',(-0.399999999999998,2.5798934217451,-3.83943612308888));
#85314=CARTESIAN_POINT('Ctrl Pts',(-0.400000000000001,2.69860205934974,
-3.77103373158167));
#85315=CARTESIAN_POINT('Ctrl Pts',(-0.400000000000001,2.81401193712609,
-3.69765307721598));
#85316=CARTESIAN_POINT('Ctrl Pts',(-0.400000000000001,2.93213331951802,
-3.62254837646153));
#85317=CARTESIAN_POINT('Ctrl Pts',(-0.400000000000009,3.04679984508726,
-3.54222851204289));
#85318=CARTESIAN_POINT('Ctrl Pts',(-0.400000000000008,3.15767190543002,
-3.45704308422265));
#85319=CARTESIAN_POINT('Ctrl Pts',(-0.400000000000006,3.26771397659399,
-3.37249535523351));
#85320=CARTESIAN_POINT('Ctrl Pts',(-0.400000000000003,3.37401887476973,
-3.28315413650226));
#85321=CARTESIAN_POINT('Ctrl Pts',(-0.400000000000004,3.47623612856816,
-3.18931392989282));
#85322=CARTESIAN_POINT('Ctrl Pts',(-0.400000000000004,3.54991652696762,
-3.12167188755712));
#85323=CARTESIAN_POINT('Ctrl Pts',(-0.400000000000001,3.62147269323696,
-3.05169124259841));
#85324=CARTESIAN_POINT('Ctrl Pts',(-0.400000000000002,3.69082794584072,
-2.97947697283326));
#85325=CARTESIAN_POINT('Ctrl Pts',(-0.400000000000002,3.72117086885487,
-2.94788322981101));
#85326=CARTESIAN_POINT('Ctrl Pts',(-0.399999999999995,3.75109241135012,
-2.91586182386534));
#85327=CARTESIAN_POINT('Ctrl Pts',(-0.399999999999995,3.78058559715336,
-2.88342095501289));
#85328=CARTESIAN_POINT('Ctrl Pts',(-0.399999999999995,3.79948466987934,
-2.86263302305373));
#85329=CARTESIAN_POINT('Ctrl Pts',(-0.400000000000004,3.81820784472281,
-2.8416728452019));
#85330=CARTESIAN_POINT('Ctrl Pts',(-0.400000000000004,3.83675320660352,
-2.82054250757437));
#85331=CARTESIAN_POINT('Ctrl Pts',(-0.400000000000004,3.84994386245842,
-2.80551325047303));
#85332=CARTESIAN_POINT('Ctrl Pts',(-0.399999999999998,3.86303916500851,
-2.79040401859846));
#85333=CARTESIAN_POINT('Ctrl Pts',(-0.399999999999998,3.87603459396517,
-2.77522058695776));
#85334=CARTESIAN_POINT('Ctrl Pts',(-0.399999999999999,3.96865254349779,
-2.66700882187327));
#85335=CARTESIAN_POINT('Ctrl Pts',(-0.400000000000009,4.0562655215007,-2.55495685843537));
#85336=CARTESIAN_POINT('Ctrl Pts',(-0.400000000000009,4.13871251510199,
-2.43943448304065));
#85337=CARTESIAN_POINT('Ctrl Pts',(-0.400000000000009,4.22224141115088,
-2.32239617680077));
#85338=CARTESIAN_POINT('Ctrl Pts',(-0.400000000000003,4.30046841967742,
-2.20179534626246));
#85339=CARTESIAN_POINT('Ctrl Pts',(-0.400000000000003,4.37319725428977,
-2.07797192475027));
#85340=CARTESIAN_POINT('Ctrl Pts',(-0.400000000000002,4.44584600861285,
-1.954284842772));
#85341=CARTESIAN_POINT('Ctrl Pts',(-0.400000000000005,4.51300920794952,
-1.82738171523173));
#85342=CARTESIAN_POINT('Ctrl Pts',(-0.400000000000006,4.574454549482,-1.69756469246434));
#85343=CARTESIAN_POINT('Ctrl Pts',(-0.400000000000006,4.63508808389366,
-1.56946279375448));
#85344=CARTESIAN_POINT('Ctrl Pts',(-0.4,4.69015427300349,-1.43852290445209));
#85345=CARTESIAN_POINT('Ctrl Pts',(-0.4,4.73938732007769,-1.3050081252555));
#85346=CARTESIAN_POINT('Ctrl Pts',(-0.4,4.75203130269614,-1.27071899127353));
#85347=CARTESIAN_POINT('Ctrl Pts',(-0.4,4.76429031498248,-1.23625991144432));
#85348=CARTESIAN_POINT('Ctrl Pts',(-0.4,4.77615934004777,-1.20163511869221));
#85349=CARTESIAN_POINT('',(-0.4,-6.03138548580071E-16,4.925));
#85350=CARTESIAN_POINT('Origin',(-0.4,0.,0.));
#85351=CARTESIAN_POINT('',(-0.4,3.87692992261799,3.04758435726506));
#85352=CARTESIAN_POINT('Origin',(-0.4,0.,0.));
#85353=CARTESIAN_POINT('Ctrl Pts',(-0.400000000000003,3.87692992261803,
3.04758435726501));
#85354=CARTESIAN_POINT('Ctrl Pts',(-0.400000000000002,3.7866811565513,3.14569047611427));
#85355=CARTESIAN_POINT('Ctrl Pts',(-0.400000000000005,3.69239500566201,
3.23969491248585));
#85356=CARTESIAN_POINT('Ctrl Pts',(-0.400000000000002,3.59413579950762,
3.32924783641162));
#85357=CARTESIAN_POINT('Ctrl Pts',(-0.4,3.48778565756658,3.42617479667806));
#85358=CARTESIAN_POINT('Ctrl Pts',(-0.399999999999996,3.37678079498109,
3.51788765012915));
#85359=CARTESIAN_POINT('Ctrl Pts',(-0.399999999999994,3.2615705131932,3.60429059305081));
#85360=CARTESIAN_POINT('Ctrl Pts',(-0.399999999999993,3.19124267296232,
3.65703356243664));
#85361=CARTESIAN_POINT('Ctrl Pts',(-0.399999999999997,3.11934726363608,
3.70779701613254));
#85362=CARTESIAN_POINT('Ctrl Pts',(-0.399999999999996,3.04598312559039,
3.75655034537377));
#85363=CARTESIAN_POINT('Ctrl Pts',(-0.399999999999996,3.00363685050327,
3.78469109569754));
#85364=CARTESIAN_POINT('Ctrl Pts',(-0.399999999999999,2.96080120507407,
3.81216201228181));
#85365=CARTESIAN_POINT('Ctrl Pts',(-0.399999999999999,2.9174949863662,3.83895616530978));
#85366=CARTESIAN_POINT('Ctrl Pts',(-0.4,2.89770430810063,3.85120093009869));
#85367=CARTESIAN_POINT('Ctrl Pts',(-0.400000000000002,2.87781497051338,
3.86330449470594));
#85368=CARTESIAN_POINT('Ctrl Pts',(-0.400000000000001,2.85784196930167,
3.87525848021691));
#85369=CARTESIAN_POINT('Ctrl Pts',(-0.4,2.73551505654073,3.94847202119883));
#85370=CARTESIAN_POINT('Ctrl Pts',(-0.400000000000002,2.60993309562182,
4.01615280664636));
#85371=CARTESIAN_POINT('Ctrl Pts',(-0.400000000000003,2.48153782508233,
4.07821468153474));
#85372=CARTESIAN_POINT('Ctrl Pts',(-0.400000000000004,2.35692693580737,
4.13844731617477));
#85373=CARTESIAN_POINT('Ctrl Pts',(-0.4,2.22966530561295,4.19338727339985));
#85374=CARTESIAN_POINT('Ctrl Pts',(-0.399999999999998,2.10014532784416,
4.24291112487635));
#85375=CARTESIAN_POINT('Ctrl Pts',(-0.399999999999998,2.03971372870769,
4.26601802770075));
#85376=CARTESIAN_POINT('Ctrl Pts',(-0.400000000000003,1.97879040175326,
4.28794521994513));
#85377=CARTESIAN_POINT('Ctrl Pts',(-0.400000000000004,1.91741505878211,
4.30867678401833));
#85378=CARTESIAN_POINT('Ctrl Pts',(-0.400000000000004,1.88122280084346,
4.32090192326947));
#85379=CARTESIAN_POINT('Ctrl Pts',(-0.399999999999999,1.84487336389223,
4.33271126438745));
#85380=CARTESIAN_POINT('Ctrl Pts',(-0.399999999999999,1.8083749234927,4.34410118547454));
#85381=CARTESIAN_POINT('Ctrl Pts',(-0.399999999999999,1.7905238413653,4.34967190067565));
#85382=CARTESIAN_POINT('Ctrl Pts',(-0.399999999999998,1.77263621214053,
4.35514255273796));
#85383=CARTESIAN_POINT('Ctrl Pts',(-0.399999999999998,1.75471579018526,
4.36051185834341));
#85384=CARTESIAN_POINT('Ctrl Pts',(-0.399999999999997,1.61980899273671,
4.40093254852367));
#85385=CARTESIAN_POINT('Ctrl Pts',(-0.399999999999992,1.48344756261164,
4.4354938576941));
#85386=CARTESIAN_POINT('Ctrl Pts',(-0.399999999999992,1.34604936009094,
4.4641147523174));
#85387=CARTESIAN_POINT('Ctrl Pts',(-0.399999999999992,1.20915742171099,
4.49263018899178));
#85388=CARTESIAN_POINT('Ctrl Pts',(-0.399999999999996,1.07123549650562,
4.51524897193337));
#85389=CARTESIAN_POINT('Ctrl Pts',(-0.399999999999997,0.932692055242528,
4.53183975365004));
#85390=CARTESIAN_POINT('Ctrl Pts',(-0.399999999999998,0.791946814713625,
4.54869420408079));
#85391=CARTESIAN_POINT('Ctrl Pts',(-0.399999999999994,0.650559268185746,
4.55932778291634));
#85392=CARTESIAN_POINT('Ctrl Pts',(-0.399999999999993,0.508965718232696,
4.56354719544793));
#85393=CARTESIAN_POINT('Ctrl Pts',(-0.399999999999993,0.402770555767909,
4.56671175484662));
#85394=CARTESIAN_POINT('Ctrl Pts',(-0.400000000000001,0.296459603189304,
4.5662672082447));
#85395=CARTESIAN_POINT('Ctrl Pts',(-0.400000000000002,0.190224357752561,
4.56211075806113));
#85396=CARTESIAN_POINT('Ctrl Pts',(-0.400000000000002,0.149138750040393,
4.56050328512674));
#85397=CARTESIAN_POINT('Ctrl Pts',(-0.4,0.108064552956015,4.5583404300336));
#85398=CARTESIAN_POINT('Ctrl Pts',(-0.4,0.0670132119983308,4.55561550073097));
#85399=CARTESIAN_POINT('Ctrl Pts',(-0.4,0.0389733158602479,4.55375425252697));
#85400=CARTESIAN_POINT('Ctrl Pts',(-0.400000000000004,0.0109440877756324,
4.55163075999061));
#85401=CARTESIAN_POINT('Ctrl Pts',(-0.400000000000004,-0.017070759942624,
4.54924277763623));
#85402=CARTESIAN_POINT('Ctrl Pts',(-0.400000000000004,-0.0352366249698258,
4.54769432141853));
#85403=CARTESIAN_POINT('Ctrl Pts',(-0.400000000000003,-0.0533870669854209,
4.5460354437308));
#85404=CARTESIAN_POINT('Ctrl Pts',(-0.400000000000003,-0.0715190897426694,
4.5442660769587));
#85405=CARTESIAN_POINT('Ctrl Pts',(-0.400000000000003,-0.204503034352091,
4.53128918100152));
#85406=CARTESIAN_POINT('Ctrl Pts',(-0.400000000000005,-0.336533808014188,
4.51236994685749));
#85407=CARTESIAN_POINT('Ctrl Pts',(-0.400000000000005,-0.467248957372364,
4.48738348767377));
#85408=CARTESIAN_POINT('Ctrl Pts',(-0.400000000000005,-0.563130622195358,
4.4690555179141));
#85409=CARTESIAN_POINT('Ctrl Pts',(-0.400000000000008,-0.658304353226521,
4.44746208615338));
#85410=CARTESIAN_POINT('Ctrl Pts',(-0.400000000000007,-0.752621900496299,
4.42253677366799));
#85411=CARTESIAN_POINT('Ctrl Pts',(-0.400000000000006,-0.882855492363467,
4.38811992264345));
#85412=CARTESIAN_POINT('Ctrl Pts',(-0.399999999999997,-1.01145813828583,
4.34735181884672));
#85413=CARTESIAN_POINT('Ctrl Pts',(-0.399999999999995,-1.13804025543659,
4.30050936743311));
#85414=CARTESIAN_POINT('Ctrl Pts',(-0.399999999999993,-1.26429577728981,
4.25378777451596));
#85415=CARTESIAN_POINT('Ctrl Pts',(-0.40000000000001,-1.38854185763495,
4.20102250581896));
#85416=CARTESIAN_POINT('Ctrl Pts',(-0.40000000000001,-1.51035703949907,
4.14245041098922));
#85417=CARTESIAN_POINT('Ctrl Pts',(-0.40000000000001,-1.55643596961048,
4.12029439215119));
#85418=CARTESIAN_POINT('Ctrl Pts',(-0.400000000000005,-1.60216665890396,
4.09730714941568));
#85419=CARTESIAN_POINT('Ctrl Pts',(-0.400000000000005,-1.64752468421034,
4.07350036769371));
#85420=CARTESIAN_POINT('Ctrl Pts',(-0.400000000000005,-1.66484982409097,
4.06440703039221));
#85421=CARTESIAN_POINT('Ctrl Pts',(-0.400000000000003,-1.68212182349379,
4.05519337578249));
#85422=CARTESIAN_POINT('Ctrl Pts',(-0.400000000000003,-1.69932318947039,
4.04586897304114));
#85423=CARTESIAN_POINT('Ctrl Pts',(-0.400000000000004,-1.81540496360726,
3.98294413239445));
#85424=CARTESIAN_POINT('Ctrl Pts',(-0.399999999999996,-1.92844024788491,
3.91489260676169));
#85425=CARTESIAN_POINT('Ctrl Pts',(-0.399999999999998,-2.03808463169202,
3.84200800987513));
#85426=CARTESIAN_POINT('Ctrl Pts',(-0.399999999999999,-2.14729220487318,
3.76941377684746));
#85427=CARTESIAN_POINT('Ctrl Pts',(-0.400000000000001,-2.25313646136716,
3.69202425594331));
#85428=CARTESIAN_POINT('Ctrl Pts',(-0.400000000000001,-2.35524312129288,
3.61009135281258));
#85429=CARTESIAN_POINT('Ctrl Pts',(-0.400000000000001,-2.45294910305158,
3.53168966241793));
#85430=CARTESIAN_POINT('Ctrl Pts',(-0.400000000000005,-2.54723297607989,
3.4491270787068));
#85431=CARTESIAN_POINT('Ctrl Pts',(-0.400000000000005,-2.63772970486551,
3.36259935817761));
#85432=CARTESIAN_POINT('Ctrl Pts',(-0.400000000000005,-2.70045032911986,
3.30262953695066));
#85433=CARTESIAN_POINT('Ctrl Pts',(-0.400000000000001,-2.76135096672307,
3.2407545396391));
#85434=CARTESIAN_POINT('Ctrl Pts',(-0.400000000000001,-2.82034722332256,
3.17704902576884));
#85435=CARTESIAN_POINT('Ctrl Pts',(-0.400000000000001,-2.84998809096459,
3.14504213561113));
#85436=CARTESIAN_POINT('Ctrl Pts',(-0.400000000000005,-2.8791480950544,
3.11257312640867));
#85437=CARTESIAN_POINT('Ctrl Pts',(-0.400000000000005,-2.90781559435835,
3.07965121601423));
#85438=CARTESIAN_POINT('Ctrl Pts',(-0.400000000000005,-2.92363627213933,
3.06148266455593));
#85439=CARTESIAN_POINT('Ctrl Pts',(-0.400000000000008,-2.93930694212779,
3.04317617572848));
#85440=CARTESIAN_POINT('Ctrl Pts',(-0.400000000000008,-2.95482556230634,
3.02473328303618));
#85441=CARTESIAN_POINT('Ctrl Pts',(-0.400000000000008,-2.96600453499757,
3.01144778526754));
#85442=CARTESIAN_POINT('Ctrl Pts',(-0.400000000000003,-2.97710217566663,
2.99809433168513));
#85443=CARTESIAN_POINT('Ctrl Pts',(-0.400000000000003,-2.98811180444513,
2.98468107674361));
#85444=CARTESIAN_POINT('Ctrl Pts',(-0.400000000000003,-3.07107784142571,
2.88360186436529));
#85445=CARTESIAN_POINT('Ctrl Pts',(-0.400000000000007,-3.14915436767407,
2.77900529093076));
#85446=CARTESIAN_POINT('Ctrl Pts',(-0.400000000000006,-3.22213021391048,
2.67119388412099));
#85447=CARTESIAN_POINT('Ctrl Pts',(-0.400000000000005,-3.2932206471212,
2.56616790620585));
#85448=CARTESIAN_POINT('Ctrl Pts',(-0.4,-3.35947070624474,2.45809028694776));
#85449=CARTESIAN_POINT('Ctrl Pts',(-0.399999999999998,-3.42063827617722,
2.34721892088016));
#85450=CARTESIAN_POINT('Ctrl Pts',(-0.399999999999997,-3.48423921431184,
2.23193687024534));
#85451=CARTESIAN_POINT('Ctrl Pts',(-0.400000000000001,-3.54234599826298,
2.11363372392856));
#85452=CARTESIAN_POINT('Ctrl Pts',(-0.400000000000001,-3.59462745933778,
1.99258608284811));
#85453=CARTESIAN_POINT('Ctrl Pts',(-0.400000000000002,-3.64331564762821,
1.87985797196755));
#85454=CARTESIAN_POINT('Ctrl Pts',(-0.399999999999998,-3.68695142065924,
1.76474903921935));
#85455=CARTESIAN_POINT('Ctrl Pts',(-0.399999999999998,-3.72521579217317,
1.64748078441541));
#85456=CARTESIAN_POINT('Ctrl Pts',(-0.399999999999998,-3.728039769191,1.63882618371547));
#85457=CARTESIAN_POINT('Ctrl Pts',(-0.4,-3.73083446619856,1.63015982325057));
#85458=CARTESIAN_POINT('Ctrl Pts',(-0.4,-3.73359974356525,1.62148179294418));
#85459=CARTESIAN_POINT('Ctrl Pts',(-24.5683458050225,-1.79217368492185,
3.6547344271607));
#85460=CARTESIAN_POINT('Ctrl Pts',(-24.5288550439032,-2.39673442057434,
3.3582757205249));
#85461=CARTESIAN_POINT('Ctrl Pts',(-24.4498735216646,-3.44699120888544,
2.45967327826949));
#85462=CARTESIAN_POINT('Ctrl Pts',(-24.2919104771873,-4.48175779295681,
-0.129924271761729));
#85463=CARTESIAN_POINT('Ctrl Pts',(-24.0944566715907,-3.10076527220938,
-3.66761492221252));
#85464=CARTESIAN_POINT('Ctrl Pts',(-23.8575121048748,1.38408548988815,-4.60175935722059));
#85465=CARTESIAN_POINT('Ctrl Pts',(-23.6205675381589,4.60615095363263,-1.3559766287573));
#85466=CARTESIAN_POINT('Ctrl Pts',(-23.383622971443,3.65518318625674,3.11589977766662));
#85467=CARTESIAN_POINT('Ctrl Pts',(-23.1466784047271,-0.612424310989975,
4.764040620714));
#85468=CARTESIAN_POINT('Ctrl Pts',(-22.9097338380112,-4.32361166112413,
2.09108995787177));
#85469=CARTESIAN_POINT('Ctrl Pts',(-22.6727892712952,-4.11460291030966,
-2.47761200147492));
#85470=CARTESIAN_POINT('Ctrl Pts',(-22.4358447045794,-0.174092888986568,
-4.79981806178492));
#85471=CARTESIAN_POINT('Ctrl Pts',(-22.1989001378634,3.92413894310881,-2.76930725388711));
#85472=CARTESIAN_POINT('Ctrl Pts',(-21.9619555711476,4.46395155275901,1.77240342487198));
#85473=CARTESIAN_POINT('Ctrl Pts',(-21.7250110044316,0.955712424786761,
4.70689540849193));
#85474=CARTESIAN_POINT('Ctrl Pts',(-21.4880664377158,-3.4191670361001,3.37305028818365));
#85475=CARTESIAN_POINT('Ctrl Pts',(-21.2511218709998,-4.69348025162024,
-1.01954248977653));
#85476=CARTESIAN_POINT('Ctrl Pts',(-21.0141773042839,-1.71163476880105,
-4.48759644703182));
#85477=CARTESIAN_POINT('Ctrl Pts',(-20.777232737568,2.82235647137499,-3.88619479158027));
#85478=CARTESIAN_POINT('Ctrl Pts',(-20.5402881708521,4.79697321791449,0.239293923164062));
#85479=CARTESIAN_POINT('Ctrl Pts',(-20.3033436041362,2.42158643669063,4.14778627515724));
#85480=CARTESIAN_POINT('Ctrl Pts',(-20.0663990374203,-2.14974872645911,
4.2949727839084));
#85481=CARTESIAN_POINT('Ctrl Pts',(-19.8294544707044,-4.77164382869297,
0.547382001344689));
#85482=CARTESIAN_POINT('Ctrl Pts',(-19.5925099039885,-3.06650535307055,
-3.69658713851903));
#85483=CARTESIAN_POINT('Ctrl Pts',(-19.3555653372726,1.4194087785671,-4.58840823893679));
#85484=CARTESIAN_POINT('Ctrl Pts',(-19.1186207705567,4.61817127913257,-1.31935803851751));
#85485=CARTESIAN_POINT('Ctrl Pts',(-18.8816762038408,3.62907264384353,3.14611558694568));
#85486=CARTESIAN_POINT('Ctrl Pts',(-18.6447316371248,-0.650950313849541,
4.75862114706335));
#85487=CARTESIAN_POINT('Ctrl Pts',(-18.407787070409,-4.34067695608756,2.05590250627856));
#85488=CARTESIAN_POINT('Ctrl Pts',(-18.170842503693,-4.09418054167253,-2.51115456224217));
#85489=CARTESIAN_POINT('Ctrl Pts',(-17.9338979369771,-0.134989541855146,
-4.801040446262));
#85490=CARTESIAN_POINT('Ctrl Pts',(-17.6969533702612,3.94661299763452,-2.73723535571292));
#85491=CARTESIAN_POINT('Ctrl Pts',(-17.4600088035453,4.44933850329186,1.80875604418168));
#85492=CARTESIAN_POINT('Ctrl Pts',(-17.2230642368294,0.917304230718045,
4.71452696382671));
#85493=CARTESIAN_POINT('Ctrl Pts',(-16.9861196701135,-3.44656205740185,
3.34505927139524));
#85494=CARTESIAN_POINT('Ctrl Pts',(-16.7491751033976,-4.6850087010358,-1.05778306645274));
#85495=CARTESIAN_POINT('Ctrl Pts',(-16.5122305366817,-1.67498455417103,
-4.50140403516247));
#85496=CARTESIAN_POINT('Ctrl Pts',(-16.2752859699658,2.85395309043288,-3.86305103540403));
#85497=CARTESIAN_POINT('Ctrl Pts',(-16.0383414032499,4.79486217074114,0.278403139515235));
#85498=CARTESIAN_POINT('Ctrl Pts',(-15.801396836534,2.38768287451035,4.16739511388991));
#85499=CARTESIAN_POINT('Ctrl Pts',(-15.5644522698181,-2.18470071411643,
4.27729988827614));
#85500=CARTESIAN_POINT('Ctrl Pts',(-15.3275077031021,-4.77594877829719,
0.508453352418028));
#85501=CARTESIAN_POINT('Ctrl Pts',(-15.0905631363863,-3.03625955368752,
-3.72147006801695));
#85502=CARTESIAN_POINT('Ctrl Pts',(-14.8536185696703,1.45677781805249,-4.57668110461451));
#85503=CARTESIAN_POINT('Ctrl Pts',(-14.6166740029544,4.62877644616991,-1.28165524065066));
#85504=CARTESIAN_POINT('Ctrl Pts',(-14.3797294362385,3.60329695155474,3.17560429263805));
#85505=CARTESIAN_POINT('Ctrl Pts',(-14.1427848695226,-0.689732898916454,
4.75315474949608));
#85506=CARTESIAN_POINT('Ctrl Pts',(-13.9058403028067,-4.35729751307742,
2.02043805325335));
#85507=CARTESIAN_POINT('Ctrl Pts',(-13.6688957360908,-4.07356717962569,
-2.54445710861498));
#85508=CARTESIAN_POINT('Ctrl Pts',(-13.4319511693749,-0.0958349178438527,
-4.80198159232485));
#85509=CARTESIAN_POINT('Ctrl Pts',(-13.195006602659,3.96880259324556,-2.70496164859175));
#85510=CARTESIAN_POINT('Ctrl Pts',(-12.9580620359431,4.43444104868229,1.84497808395286));
#85511=CARTESIAN_POINT('Ctrl Pts',(-12.7211174692272,0.878829071125367,
4.72185037969754));
#85512=CARTESIAN_POINT('Ctrl Pts',(-12.4841729025113,-3.47372478568834,
3.31684302580018));
#85513=CARTESIAN_POINT('Ctrl Pts',(-12.2472283357954,-4.67622722785964,
-1.09595185018732));
#85514=CARTESIAN_POINT('Ctrl Pts',(-12.0102837690795,-1.63822211600786,
-4.514913049343));
#85515=CARTESIAN_POINT('Ctrl Pts',(-11.7733392023635,2.88535949150936,-3.83965000348491));
#85516=CARTESIAN_POINT('Ctrl Pts',(-11.5363946356477,4.79243250703115,0.317493637819545));
#85517=CARTESIAN_POINT('Ctrl Pts',(-11.2994500689317,2.35362041946459,4.18672693945812));
#85518=CARTESIAN_POINT('Ctrl Pts',(-11.0625055022158,-2.21950736358003,
4.25934250882913));
#85519=CARTESIAN_POINT('Ctrl Pts',(-10.8255609354999,-4.77993617310215,
0.469490921716715));
#85520=CARTESIAN_POINT('Ctrl Pts',(-10.588616368784,-3.00581183494387,-3.74610554541864));
#85521=CARTESIAN_POINT('Ctrl Pts',(-10.3516718020681,1.49404997724334,-4.56464962620395));
#85522=CARTESIAN_POINT('Ctrl Pts',(-10.1147272353522,4.63907381730574,-1.24386722044341));
#85523=CARTESIAN_POINT('Ctrl Pts',(-9.8777826686363,3.57728164792448,3.20488183181962));
#85524=CARTESIAN_POINT('Ctrl Pts',(-9.64083810192037,-0.728469617480856,
4.74737227957853));
#85525=CARTESIAN_POINT('Ctrl Pts',(-9.40389353520448,-4.37362832284165,
1.9848392474317));
#85526=CARTESIAN_POINT('Ctrl Pts',(-9.16694896848857,-4.05268293663714,
-2.5775904561419));
#85527=CARTESIAN_POINT('Ctrl Pts',(-8.93000440177266,-0.0566739212580544,
-4.80260342014054));
#85528=CARTESIAN_POINT('Ctrl Pts',(-8.69305983505675,3.99072827488727,-2.67250806931295));
#85529=CARTESIAN_POINT('Ctrl Pts',(-8.45611526834084,4.41924871633079,1.88107743798526));
#85530=CARTESIAN_POINT('Ctrl Pts',(-8.21917070162494,0.840295471934814,
4.72885980594699));
#85531=CARTESIAN_POINT('Ctrl Pts',(-7.98222613490903,-3.50065652120147,
3.28840621962052));
#85532=CARTESIAN_POINT('Ctrl Pts',(-7.74528156819312,-4.66713479887029,
-1.13404775627675));
#85533=CARTESIAN_POINT('Ctrl Pts',(-7.50833700147722,-1.60135074079071,
-4.52812183462507));
#85534=CARTESIAN_POINT('Ctrl Pts',(-7.2713924347613,2.91657402449002,-3.81599364587164));
#85535=CARTESIAN_POINT('Ctrl Pts',(-7.03444786804541,4.78968416005308,0.356563023868872));
#85536=CARTESIAN_POINT('Ctrl Pts',(-6.79750330132949,2.31940145568391,4.2057803592973));
#85537=CARTESIAN_POINT('Ctrl Pts',(-6.5605587346136,-2.25416642273435,4.24110189585783));
#85538=CARTESIAN_POINT('Ctrl Pts',(-6.32361416789768,-4.78360571461287,
0.430497270029063));
#85539=CARTESIAN_POINT('Ctrl Pts',(-6.08666960118177,-2.9751642405108,-3.77049191521503));
#85540=CARTESIAN_POINT('Ctrl Pts',(-5.84972503446587,1.53122279065449,-4.55231461594934));
#85541=CARTESIAN_POINT('Ctrl Pts',(-5.61278046774996,4.6490626950213,-1.20599647826086));
#85542=CARTESIAN_POINT('Ctrl Pts',(-5.37583590103405,3.55102848107464,3.23394623945287));
#85543=CARTESIAN_POINT('Ctrl Pts',(-5.13889133431815,-0.767157925271441,
4.74127415374739));
#85544=CARTESIAN_POINT('Ctrl Pts',(-4.90194676760223,-4.38966824042904,
1.9491083962661));
#85545=CARTESIAN_POINT('Ctrl Pts',(-4.66500220088633,-4.03152931388751,
-2.61055228754619));
#85546=CARTESIAN_POINT('Ctrl Pts',(-4.42805763417042,-0.0175089406698063,
-4.80290610693659));
#85547=CARTESIAN_POINT('Ctrl Pts',(-4.19111306745452,4.01238817079558,-2.63987635628594));
#85548=CARTESIAN_POINT('Ctrl Pts',(-3.9541685007386,4.40376331119336,1.91705089973334));
#85549=CARTESIAN_POINT('Ctrl Pts',(-3.71722393402271,0.801704468977416,
4.73555632478705));
#85550=CARTESIAN_POINT('Ctrl Pts',(-3.48027936730679,-3.5273525406531,3.25974776958548));
#85551=CARTESIAN_POINT('Ctrl Pts',(-3.24333480059089,-4.6577376517205,-1.17206253805825));
#85552=CARTESIAN_POINT('Ctrl Pts',(-3.00639023387498,-1.56436205950543,
-4.54104048789013));
#85553=CARTESIAN_POINT('Ctrl Pts',(-2.76944566715907,2.94757382720121,-3.79206245260455));
#85554=CARTESIAN_POINT('Ctrl Pts',(-2.53250110044317,4.78665724274367,0.395568199836796));
#85555=CARTESIAN_POINT('Ctrl Pts',(-2.29555653372726,2.28495155387725,4.2246319053635));
#85556=CARTESIAN_POINT('Ctrl Pts',(-2.05861196701135,-2.28852823748934,
4.22242981165284));
#85557=CARTESIAN_POINT('Ctrl Pts',(-1.82166740029544,-4.7872402315289,0.391762093796413));
#85558=CARTESIAN_POINT('Ctrl Pts',(-1.58472283357954,-2.9437748544915,-3.79517919940816));
#85559=CARTESIAN_POINT('Ctrl Pts',(-1.34777826686363,1.56724719957269,-4.53861602703052));
#85560=CARTESIAN_POINT('Ctrl Pts',(-1.11083370014772,4.66076829913842,-1.17009430681153));
#85561=CARTESIAN_POINT('Ctrl Pts',(-0.873889133431818,3.52050501373642,
3.26683163619313));
#85562=CARTESIAN_POINT('Ctrl Pts',(-0.676435327835224,-0.0771870156949762,
4.48297617612786));
#85563=CARTESIAN_POINT('Ctrl Pts',(-0.518472283357957,-2.61623498089622,
3.32972304474434));
#85564=CARTESIAN_POINT('Ctrl Pts',(-0.439490761119318,-3.46537663594235,
2.23908831199168));
#85565=CARTESIAN_POINT('Ctrl Pts',(-0.4,-3.73359974356525,1.62148179294418));
#85566=CARTESIAN_POINT('Ctrl Pts',(-24.4038972033484,-1.91758108071806,
3.91047455474609));
#85567=CARTESIAN_POINT('Ctrl Pts',(-24.364406442229,-2.56444596808124,3.59327114313381));
#85568=CARTESIAN_POINT('Ctrl Pts',(-24.2854249199904,-3.68819449988101,
2.63178897382545));
#85569=CARTESIAN_POINT('Ctrl Pts',(-24.1274618755131,-4.7953689000347,-0.139015725737088));
#85570=CARTESIAN_POINT('Ctrl Pts',(-23.9300080699165,-3.31774139513474,
-3.92425636274236));
#85571=CARTESIAN_POINT('Ctrl Pts',(-23.6930635032006,1.4809369046291,-4.9237675765831));
#85572=CARTESIAN_POINT('Ctrl Pts',(-23.4561189364847,4.92846647505743,-1.4508611252789));
#85573=CARTESIAN_POINT('Ctrl Pts',(-23.2191743697688,3.91095471577045,3.33393493796763));
#85574=CARTESIAN_POINT('Ctrl Pts',(-22.9822298030529,-0.65527871657001,
5.09740447531009));
#85575=CARTESIAN_POINT('Ctrl Pts',(-22.745285236337,-4.62615648890371,2.23741402690521));
#85576=CARTESIAN_POINT('Ctrl Pts',(-22.5083406696211,-4.40252234583026,
-2.65098295960946));
#85577=CARTESIAN_POINT('Ctrl Pts',(-22.2713961029052,-0.18627504299217,
-5.13568544366227));
#85578=CARTESIAN_POINT('Ctrl Pts',(-22.0344515361893,4.19873065804033,-2.96308959417674));
#85579=CARTESIAN_POINT('Ctrl Pts',(-21.7975069694734,4.77631666775984,1.89642739625574));
#85580=CARTESIAN_POINT('Ctrl Pts',(-21.5605624027575,1.02258842421195,5.03626052551738));
#85581=CARTESIAN_POINT('Ctrl Pts',(-21.3236178360416,-3.65842332994994,
3.60907956151234));
#85582=CARTESIAN_POINT('Ctrl Pts',(-21.0866732693257,-5.02190664272777,
-1.09088499950208));
#85583=CARTESIAN_POINT('Ctrl Pts',(-20.8497287026098,-1.83140645204561,
-4.80161611406605));
#85584=CARTESIAN_POINT('Ctrl Pts',(-20.6127841358938,3.01985093190725,-4.15813136361528));
#85585=CARTESIAN_POINT('Ctrl Pts',(-20.375839569178,5.13264153177503,0.256038521071223));
#85586=CARTESIAN_POINT('Ctrl Pts',(-20.138895002462,2.59103700461042,4.43802771741427));
#85587=CARTESIAN_POINT('Ctrl Pts',(-19.9019504357462,-2.30017744420541,
4.59551360558059));
#85588=CARTESIAN_POINT('Ctrl Pts',(-19.6650058690302,-5.10553971794639,
0.58568506977604));
#85589=CARTESIAN_POINT('Ctrl Pts',(-19.4280613023143,-3.28108413734759,
-3.95525591056704));
#85590=CARTESIAN_POINT('Ctrl Pts',(-19.1911167355984,1.51873194126499,-4.90948221348304));
#85591=CARTESIAN_POINT('Ctrl Pts',(-18.9541721688825,4.94132792311723,-1.41168014832495));
#85592=CARTESIAN_POINT('Ctrl Pts',(-18.7172276021666,3.88301708753714,3.36626509921239));
#85593=CARTESIAN_POINT('Ctrl Pts',(-18.4802830354507,-0.696500577386702,
5.09160577386314));
#85594=CARTESIAN_POINT('Ctrl Pts',(-18.2433384687348,-4.64441592828398,
2.19976433255833));
#85595=CARTESIAN_POINT('Ctrl Pts',(-18.0063939020189,-4.38067092146694,
-2.68687266185611));
#85596=CARTESIAN_POINT('Ctrl Pts',(-17.769449335303,-0.144435438224605,
-5.1369933645219));
#85597=CARTESIAN_POINT('Ctrl Pts',(-17.532504768587,4.2227773350606,-2.92877346417273));
#85598=CARTESIAN_POINT('Ctrl Pts',(-17.2955602018711,4.76068106981219,1.9353237909575));
#85599=CARTESIAN_POINT('Ctrl Pts',(-17.0586156351552,0.981492615859015,
5.04442609911638));
#85600=CARTESIAN_POINT('Ctrl Pts',(-16.8216710684393,-3.68773531851224,
3.57912987266515));
#85601=CARTESIAN_POINT('Ctrl Pts',(-16.5847265017234,-5.01284229519173,
-1.13180146143153));
#85602=CARTESIAN_POINT('Ctrl Pts',(-16.3477819350075,-1.79219163778398,
-4.81638988850122));
#85603=CARTESIAN_POINT('Ctrl Pts',(-16.1108373682916,3.0536585251276,-4.13336812255573));
#85604=CARTESIAN_POINT('Ctrl Pts',(-15.8738928015757,5.13038276402602,0.297884405757334));
#85605=CARTESIAN_POINT('Ctrl Pts',(-15.6369482348598,2.55476103986837,4.45900868509891));
#85606=CARTESIAN_POINT('Ctrl Pts',(-15.4000036681439,-2.33757519802194,
4.57660404866038));
#85607=CARTESIAN_POINT('Ctrl Pts',(-15.163059101428,-5.11014590650051,0.544032387724225));
#85608=CARTESIAN_POINT('Ctrl Pts',(-14.9261145347121,-3.24872188744064,
-3.98188002364241));
#85609=CARTESIAN_POINT('Ctrl Pts',(-14.6891699679962,1.55871588016816,-4.89693447266046));
#85610=CARTESIAN_POINT('Ctrl Pts',(-14.4522254012803,4.95267518696769,-1.37133909628972));
#85611=CARTESIAN_POINT('Ctrl Pts',(-14.2152808345644,3.85543774057359,3.39781727777984));
#85612=CARTESIAN_POINT('Ctrl Pts',(-13.9783362678484,-0.737996974756748,
5.08575686499741));
#85613=CARTESIAN_POINT('Ctrl Pts',(-13.7413917011325,-4.66219950914051,
2.16181825359773));
#85614=CARTESIAN_POINT('Ctrl Pts',(-13.5044471344166,-4.35861513892556,
-2.7225055546954));
#85615=CARTESIAN_POINT('Ctrl Pts',(-13.2675025677007,-0.102540968476285,
-5.13800036730267));
#85616=CARTESIAN_POINT('Ctrl Pts',(-13.0305580009848,4.24651964814693,-2.89424140363592));
#85617=CARTESIAN_POINT('Ctrl Pts',(-12.7936134342689,4.74474116546558,1.97408046881445));
#85618=CARTESIAN_POINT('Ctrl Pts',(-12.556668867553,0.940325156068005,5.05226197118519));
#85619=CARTESIAN_POINT('Ctrl Pts',(-12.3197243008371,-3.71679875935009,
3.54893919462028));
#85620=CARTESIAN_POINT('Ctrl Pts',(-12.0827797341212,-5.00344633822333,
-1.17264110670656));
#85621=CARTESIAN_POINT('Ctrl Pts',(-11.8458351674053,-1.75285674714482,
-4.83084419626708));
#85622=CARTESIAN_POINT('Ctrl Pts',(-11.6088906006894,3.08726258985882,-4.10832960287713));
#85623=CARTESIAN_POINT('Ctrl Pts',(-11.3719460339735,5.12778308454073,0.33971026260081));
#85624=CARTESIAN_POINT('Ctrl Pts',(-11.1350014672576,2.51831506372883,4.47969325561639));
#85625=CARTESIAN_POINT('Ctrl Pts',(-10.8980569005416,-2.37481744360122,
4.55739010116378));
#85626=CARTESIAN_POINT('Ctrl Pts',(-10.6611123338258,-5.11441231935083,
0.502343560017281));
#85627=CARTESIAN_POINT('Ctrl Pts',(-10.4241677671098,-3.21614358886106,
-4.00823936915529));
#85628=CARTESIAN_POINT('Ctrl Pts',(-10.1872232003939,1.59859615957589,-4.88406109126486));
#85629=CARTESIAN_POINT('Ctrl Pts',(-9.95027863367802,4.96369311689119,-1.33090685847881));
#85630=CARTESIAN_POINT('Ctrl Pts',(-9.7133340669621,3.82760201545932,3.42914351345493));
#85631=CARTESIAN_POINT('Ctrl Pts',(-9.47638950024621,-0.779444296114679,
5.07956976661125));
#85632=CARTESIAN_POINT('Ctrl Pts',(-9.23944493353029,-4.67967306770249,
2.12372842050058));
#85633=CARTESIAN_POINT('Ctrl Pts',(-9.00250036681439,-4.33626952054219,
-2.75795740899559));
#85634=CARTESIAN_POINT('Ctrl Pts',(-8.76555580009848,-0.0606396802324226,
-5.1386657075344));
#85635=CARTESIAN_POINT('Ctrl Pts',(-8.52861123338258,4.26997957987774,-2.85951688438303));
#85636=CARTESIAN_POINT('Ctrl Pts',(-8.29166666666666,4.72848574930011,2.01270587599516));
#85637=CARTESIAN_POINT('Ctrl Pts',(-8.05472209995076,0.899095167366884,
5.05976188220148));
#85638=CARTESIAN_POINT('Ctrl Pts',(-7.81777753323486,-3.74561504368981,
3.51851252225869));
#85639=CARTESIAN_POINT('Ctrl Pts',(-7.58083296651895,-4.99371766630138,
-1.2134027747215));
#85640=CARTESIAN_POINT('Ctrl Pts',(-7.34388839980304,-1.71340529657878,
-4.84497726661025));
#85641=CARTESIAN_POINT('Ctrl Pts',(-7.10694383308713,3.1206613605197,-4.08301789108291));
#85642=CARTESIAN_POINT('Ctrl Pts',(-6.86999926637123,5.12484242191816,0.38151352985876));
#85643=CARTESIAN_POINT('Ctrl Pts',(-6.63305469965531,2.48170162715197,4.50007993895741));
#85644=CARTESIAN_POINT('Ctrl Pts',(-6.39611013293941,-2.41190177123586,
4.53787310087038));
#85645=CARTESIAN_POINT('Ctrl Pts',(-6.1591655662235,-5.11833863711515,0.460621326634736));
#85646=CARTESIAN_POINT('Ctrl Pts',(-5.9222209995076,-3.18335142828599,-4.03433217575231));
#85647=CARTESIAN_POINT('Ctrl Pts',(-5.68527643279169,1.63837014148066,-4.87086293837728));
#85648=CARTESIAN_POINT('Ctrl Pts',(-5.44833186607578,4.97438096656006,-1.29038611022042));
#85649=CARTESIAN_POINT('Ctrl Pts',(-5.21138729935987,3.79951178264107,3.46024170369659));
#85650=CARTESIAN_POINT('Ctrl Pts',(-4.97444273264398,-0.820839819153767,
5.07304492428149));
#85651=CARTESIAN_POINT('Ctrl Pts',(-4.73749816592805,-4.69683537890069,
2.08549730218345));
#85652=CARTESIAN_POINT('Ctrl Pts',(-4.50055359921216,-4.31363567254264,
-2.79322574532843));
#85653=CARTESIAN_POINT('Ctrl Pts',(-4.26360903249624,-0.0187341292054296,
-5.13898957484612));
#85654=CARTESIAN_POINT('Ctrl Pts',(-4.02666446578034,4.29315512751217,-2.82460176646869));
#85655=CARTESIAN_POINT('Ctrl Pts',(-3.78971989906443,4.71191675257361,2.05119658157601));
#85656=CARTESIAN_POINT('Ctrl Pts',(-3.55277533234853,0.857803758068979,
5.06692699010502));
#85657=CARTESIAN_POINT('Ctrl Pts',(-3.31583076563262,-3.77417911773109,
3.48784869650773));
#85658=CARTESIAN_POINT('Ctrl Pts',(-3.07888619891671,-4.98366295355854,
-1.25407764175316));
#85659=CARTESIAN_POINT('Ctrl Pts',(-2.8419416322008,-1.67382833144973,-4.85879990294167));
#85660=CARTESIAN_POINT('Ctrl Pts',(-2.6049970654849,3.15383037515544,-4.05741211200355));
#85661=CARTESIAN_POINT('Ctrl Pts',(-2.36805249876899,5.12160369599876,0.42324809393336));
#85662=CARTESIAN_POINT('Ctrl Pts',(-2.13110793205308,2.44484109265533,4.52025062240341));
#85663=CARTESIAN_POINT('Ctrl Pts',(-1.89416336533717,-2.44866805478732,
4.51789443713354));
#85664=CARTESIAN_POINT('Ctrl Pts',(-1.65721879862127,-5.12222747943796,
0.419175655533249));
#85665=CARTESIAN_POINT('Ctrl Pts',(-1.42027423190536,-3.14976556924097,
-4.06074695323808));
#85666=CARTESIAN_POINT('Ctrl Pts',(-1.18332966518945,1.67691535926105,-4.85620579037636));
#85667=CARTESIAN_POINT('Ctrl Pts',(-0.946385098473546,4.98690567060087,
-1.25197168347867));
#85668=CARTESIAN_POINT('Ctrl Pts',(-0.70944053175764,3.76685243495724,3.49542825684799));
#85669=CARTESIAN_POINT('Ctrl Pts',(-0.511986726161047,-0.0825881789354425,
4.79667253959683));
#85670=CARTESIAN_POINT('Ctrl Pts',(-0.354023681683779,-2.79930608527943,
3.56272049319328));
#85671=CARTESIAN_POINT('Ctrl Pts',(-0.27504215944514,-3.70786644762908,
2.39576856933903));
#85672=CARTESIAN_POINT('Ctrl Pts',(-0.235551398325822,-3.99485847352278,
1.73494501958064));
#85673=CARTESIAN_POINT('Ctrl Pts',(-24.2394486016742,-2.04298847651427,
4.16621468233147));
#85674=CARTESIAN_POINT('Ctrl Pts',(-24.1999578405549,-2.73215751558814,
3.82826656574272));
#85675=CARTESIAN_POINT('Ctrl Pts',(-24.1209763183162,-3.92939779087658,
2.80390466938141));
#85676=CARTESIAN_POINT('Ctrl Pts',(-23.963013273839,-5.10898000711258,-0.14810717971244));
#85677=CARTESIAN_POINT('Ctrl Pts',(-23.7655594682423,-3.53471751806012,
-4.18089780327223));
#85678=CARTESIAN_POINT('Ctrl Pts',(-23.5286149015265,1.57778831937005,-5.24577579594559));
#85679=CARTESIAN_POINT('Ctrl Pts',(-23.2916703348105,5.25078199648223,-1.5457456218005));
#85680=CARTESIAN_POINT('Ctrl Pts',(-23.0547257680946,4.16672624528416,3.55197009826865));
#85681=CARTESIAN_POINT('Ctrl Pts',(-22.8177812013787,-0.698133122150042,
5.43076832990618));
#85682=CARTESIAN_POINT('Ctrl Pts',(-22.5808366346628,-4.92870131668329,
2.38373809593864));
#85683=CARTESIAN_POINT('Ctrl Pts',(-22.3438920679469,-4.69044178135086,
-2.824353917744));
#85684=CARTESIAN_POINT('Ctrl Pts',(-22.106947501231,-0.198457196997771,
-5.47155282553962));
#85685=CARTESIAN_POINT('Ctrl Pts',(-21.8700029345151,4.47332237297185,-3.15687193446637));
#85686=CARTESIAN_POINT('Ctrl Pts',(-21.6330583677992,5.08868178276068,2.0204513676395));
#85687=CARTESIAN_POINT('Ctrl Pts',(-21.3961138010833,1.08946442363714,5.36562564254283));
#85688=CARTESIAN_POINT('Ctrl Pts',(-21.1591692343674,-3.89767962379977,
3.84510883484102));
#85689=CARTESIAN_POINT('Ctrl Pts',(-20.9222246676515,-5.3503330338353,-1.16222750922764));
#85690=CARTESIAN_POINT('Ctrl Pts',(-20.6852801009356,-1.95117813529016,
-5.11563578110029));
#85691=CARTESIAN_POINT('Ctrl Pts',(-20.4483355342197,3.2173453924395,-4.4300679356503));
#85692=CARTESIAN_POINT('Ctrl Pts',(-20.2113909675038,5.46830984563556,0.272783118978384));
#85693=CARTESIAN_POINT('Ctrl Pts',(-19.9744464007879,2.76048757253021,4.72826915967129));
#85694=CARTESIAN_POINT('Ctrl Pts',(-19.7375018340719,-2.45060616195172,
4.89605442725277));
#85695=CARTESIAN_POINT('Ctrl Pts',(-19.500557267356,-5.4394356071998,0.623988138207389));
#85696=CARTESIAN_POINT('Ctrl Pts',(-19.2636127006401,-3.49566292162464,
-4.21392468261504));
#85697=CARTESIAN_POINT('Ctrl Pts',(-19.0266681339242,1.61805510396288,-5.2305561880293));
#85698=CARTESIAN_POINT('Ctrl Pts',(-18.7897235672083,5.26448456710188,-1.5040022581324));
#85699=CARTESIAN_POINT('Ctrl Pts',(-18.5527790004924,4.13696153123076,3.58641461147908));
#85700=CARTESIAN_POINT('Ctrl Pts',(-18.3158344337765,-0.742050840923869,
5.42459040066293));
#85701=CARTESIAN_POINT('Ctrl Pts',(-18.0788898670606,-4.94815490048041,
2.34362615883809));
#85702=CARTESIAN_POINT('Ctrl Pts',(-17.8419453003447,-4.66716130126134,
-2.86259076147005));
#85703=CARTESIAN_POINT('Ctrl Pts',(-17.6050007336288,-0.153881334594059,
-5.47294628278181));
#85704=CARTESIAN_POINT('Ctrl Pts',(-17.3680561669129,4.49894167248667,-3.12031157263254));
#85705=CARTESIAN_POINT('Ctrl Pts',(-17.1311116001969,5.07202363633252,2.06189153773331));
#85706=CARTESIAN_POINT('Ctrl Pts',(-16.8941670334811,1.04568100099998,5.37432523440605));
#85707=CARTESIAN_POINT('Ctrl Pts',(-16.6572224667651,-3.92890857962264,
3.81320047393507));
#85708=CARTESIAN_POINT('Ctrl Pts',(-16.4202779000492,-5.34067588934766,
-1.20581985641032));
#85709=CARTESIAN_POINT('Ctrl Pts',(-16.1833333333333,-1.90939872139693,
-5.13137574183997));
#85710=CARTESIAN_POINT('Ctrl Pts',(-15.9463887666174,3.25336395982232,-4.40368520970743));
#85711=CARTESIAN_POINT('Ctrl Pts',(-15.7094441999015,5.46590335731091,0.31736567199943));
#85712=CARTESIAN_POINT('Ctrl Pts',(-15.4724996331856,2.72183920522639,4.75062225630792));
#85713=CARTESIAN_POINT('Ctrl Pts',(-15.2355550664697,-2.49044968192745,
4.87590820904461));
#85714=CARTESIAN_POINT('Ctrl Pts',(-14.9986104997538,-5.44434303470384,
0.579611423030416));
#85715=CARTESIAN_POINT('Ctrl Pts',(-14.7616659330379,-3.46118422119377,
-4.24228997926785));
#85716=CARTESIAN_POINT('Ctrl Pts',(-14.524721366322,1.66065394228382,-5.21718784070642));
#85717=CARTESIAN_POINT('Ctrl Pts',(-14.2877767996061,5.27657392776547,-1.46102295192877));
#85718=CARTESIAN_POINT('Ctrl Pts',(-14.0508322328902,4.10757852959245,3.62003026292162));
#85719=CARTESIAN_POINT('Ctrl Pts',(-13.8138876661743,-0.786261050597038,
5.41835898049874));
#85720=CARTESIAN_POINT('Ctrl Pts',(-13.5769430994584,-4.9671015052036,2.3031984539421));
#85721=CARTESIAN_POINT('Ctrl Pts',(-13.3399985327424,-4.64366309822542,
-2.90055400077583));
#85722=CARTESIAN_POINT('Ctrl Pts',(-13.1030539660265,-0.109247019108718,
-5.47401914228049));
#85723=CARTESIAN_POINT('Ctrl Pts',(-12.8661093993106,4.5242367030483,-3.08352115868009));
#85724=CARTESIAN_POINT('Ctrl Pts',(-12.6291648325947,5.05504128224888,2.10318285367604));
#85725=CARTESIAN_POINT('Ctrl Pts',(-12.3922202658788,1.00182124101064,5.38267356267285));
#85726=CARTESIAN_POINT('Ctrl Pts',(-12.1552756991629,-3.95987273301183,
3.78103536344037));
#85727=CARTESIAN_POINT('Ctrl Pts',(-11.918331132447,-5.33066544858701,-1.2493303632258));
#85728=CARTESIAN_POINT('Ctrl Pts',(-11.6813865657311,-1.86749137828179,
-5.14677534319116));
#85729=CARTESIAN_POINT('Ctrl Pts',(-11.4444419990152,3.28916568820829,-4.37700920226935));
#85730=CARTESIAN_POINT('Ctrl Pts',(-11.2074974322993,5.4631336620503,0.361926887382075));
#85731=CARTESIAN_POINT('Ctrl Pts',(-10.9705528655834,2.68300970799308,4.77265957177466));
#85732=CARTESIAN_POINT('Ctrl Pts',(-10.7336082988675,-2.53012752362241,
4.85543769349845));
#85733=CARTESIAN_POINT('Ctrl Pts',(-10.4966637321516,-5.44888846559951,
0.535196198317838));
#85734=CARTESIAN_POINT('Ctrl Pts',(-10.2597191654356,-3.42647534277826,
-4.27037319289192));
#85735=CARTESIAN_POINT('Ctrl Pts',(-10.0227745987198,1.70314234190846,-5.20347255632578));
#85736=CARTESIAN_POINT('Ctrl Pts',(-9.78583003200384,5.28831241647663,-1.41794649651421));
#85737=CARTESIAN_POINT('Ctrl Pts',(-9.54888546528793,4.07792238299417,3.65340519509024));
#85738=CARTESIAN_POINT('Ctrl Pts',(-9.31194089857203,-0.830418974748515,
5.41176725364395));
#85739=CARTESIAN_POINT('Ctrl Pts',(-9.07499633185612,-4.98571781256332,
2.26261759356947));
#85740=CARTESIAN_POINT('Ctrl Pts',(-8.83805176514021,-4.61985610444725,
-2.93832436184929));
#85741=CARTESIAN_POINT('Ctrl Pts',(-8.60110719842431,-0.0646054392067775,
-5.47472799492826));
#85742=CARTESIAN_POINT('Ctrl Pts',(-8.36416263170839,4.54923088486819,-3.0465256994531));
#85743=CARTESIAN_POINT('Ctrl Pts',(-8.12721806499249,5.03772278226943,2.14433431400508));
#85744=CARTESIAN_POINT('Ctrl Pts',(-7.89027349827659,0.957894862798949,
5.39066395845597));
#85745=CARTESIAN_POINT('Ctrl Pts',(-7.65332893156067,-3.99057356617815,
3.74861882489686));
#85746=CARTESIAN_POINT('Ctrl Pts',(-7.41638436484478,-5.32030053373246,
-1.29275779316626));
#85747=CARTESIAN_POINT('Ctrl Pts',(-7.17943979812886,-1.82545985236685,
-5.16183269859543));
#85748=CARTESIAN_POINT('Ctrl Pts',(-6.94249523141296,3.32474869654938,-4.35004213629419));
#85749=CARTESIAN_POINT('Ctrl Pts',(-6.70555066469704,5.46000068378324,0.406464035848652));
#85750=CARTESIAN_POINT('Ctrl Pts',(-6.46860609798114,2.64400179862004,4.79437951861751));
#85751=CARTESIAN_POINT('Ctrl Pts',(-6.23166153126523,-2.56963711973737,
4.83464430588292));
#85752=CARTESIAN_POINT('Ctrl Pts',(-5.99471696454932,-5.45307155961744,
0.490745383240414));
#85753=CARTESIAN_POINT('Ctrl Pts',(-5.75777239783342,-3.39153861606119,
-4.29817243628959));
#85754=CARTESIAN_POINT('Ctrl Pts',(-5.52082783111751,1.74551749230684,-5.18941126080523));
#85755=CARTESIAN_POINT('Ctrl Pts',(-5.28388326440161,5.29969923809883,-1.37477574217999));
#85756=CARTESIAN_POINT('Ctrl Pts',(-5.04693869768569,4.04799508420751,3.68653716794031));
#85757=CARTESIAN_POINT('Ctrl Pts',(-4.80999413096979,-0.874521713036094,
5.4048156948156));
#85758=CARTESIAN_POINT('Ctrl Pts',(-4.57304956425388,-5.00400251737233,
2.22188620810079));
#85759=CARTESIAN_POINT('Ctrl Pts',(-4.33610499753798,-4.59574203119776,
-2.97589920311067));
#85760=CARTESIAN_POINT('Ctrl Pts',(-4.09916043082206,-0.0199593177410495,
-5.47507304275567));
#85761=CARTESIAN_POINT('Ctrl Pts',(-3.86221586410616,4.57392208422876,-3.00932717665144));
#85762=CARTESIAN_POINT('Ctrl Pts',(-3.62527129739025,5.02007019395386,2.18534226341869));
#85763=CARTESIAN_POINT('Ctrl Pts',(-3.38832673067435,0.913903047160537,
5.398297655423));
#85764=CARTESIAN_POINT('Ctrl Pts',(-3.15138216395844,-4.02100569480907,
3.71594962342999));
#85765=CARTESIAN_POINT('Ctrl Pts',(-2.91443759724253,-5.30958825539658,
-1.33609274544807));
#85766=CARTESIAN_POINT('Ctrl Pts',(-2.67749303052662,-1.78329460339402,
-5.17655931799322));
#85767=CARTESIAN_POINT('Ctrl Pts',(-2.44054846381072,3.36008692310967,-4.32276177140254));
#85768=CARTESIAN_POINT('Ctrl Pts',(-2.20360389709481,5.45655014925385,0.450927988029921));
#85769=CARTESIAN_POINT('Ctrl Pts',(-1.96665933037891,2.6047306314334,4.81586933944332));
#85770=CARTESIAN_POINT('Ctrl Pts',(-1.72971476366299,-2.6088078720853,4.81335906261424));
#85771=CARTESIAN_POINT('Ctrl Pts',(-1.49277019694709,-5.45721472734701,
0.44658921727009));
#85772=CARTESIAN_POINT('Ctrl Pts',(-1.25582563023118,-3.35575628399046,
-4.326314707068));
#85773=CARTESIAN_POINT('Ctrl Pts',(-1.01888106351528,1.78658351894942,-5.17379555372219));
#85774=CARTESIAN_POINT('Ctrl Pts',(-0.781936496799368,5.31304304206331,
-1.33384906014582));
#85775=CARTESIAN_POINT('Ctrl Pts',(-0.544991930083462,4.01319985617806,
3.72402487750285));
#85776=CARTESIAN_POINT('Ctrl Pts',(-0.347538124486869,-0.0879893421759137,
5.11036890306578));
#85777=CARTESIAN_POINT('Ctrl Pts',(-0.189575080009601,-2.98237718966264,
3.79571794164222));
#85778=CARTESIAN_POINT('Ctrl Pts',(-0.110593557770963,-3.95035625931582,
2.55244882668638));
#85779=CARTESIAN_POINT('Ctrl Pts',(-0.0711027966516446,-4.25611720348031,
1.8484082462171));
#85780=CARTESIAN_POINT('Ctrl Pts',(-24.075,-2.16839587231048,4.42195480991686));
#85781=CARTESIAN_POINT('Ctrl Pts',(-24.0355092388807,-2.89986906309504,
4.06326198835163));
#85782=CARTESIAN_POINT('Ctrl Pts',(-23.956527716642,-4.17060108187215,2.97602036493736));
#85783=CARTESIAN_POINT('Ctrl Pts',(-23.7985646721648,-5.42259111419047,
-0.157198633687794));
#85784=CARTESIAN_POINT('Ctrl Pts',(-23.6011108665682,-3.75169364098549,
-4.43753924380208));
#85785=CARTESIAN_POINT('Ctrl Pts',(-23.3641662998523,1.67463973411099,-5.56778401530808));
#85786=CARTESIAN_POINT('Ctrl Pts',(-23.1272217331364,5.57309751790704,-1.6406301183221));
#85787=CARTESIAN_POINT('Ctrl Pts',(-22.8902771664205,4.42249777479786,3.77000525856966));
#85788=CARTESIAN_POINT('Ctrl Pts',(-22.6533325997046,-0.740987527730072,
5.76413218450227));
#85789=CARTESIAN_POINT('Ctrl Pts',(-22.4163880329886,-5.23124614446287,
2.53006216497207));
#85790=CARTESIAN_POINT('Ctrl Pts',(-22.1794434662727,-4.97836121687146,
-2.99772487587854));
#85791=CARTESIAN_POINT('Ctrl Pts',(-21.9424988995568,-0.210639351003371,
-5.80742020741697));
#85792=CARTESIAN_POINT('Ctrl Pts',(-21.7055543328409,4.74791408790337,-3.350654274756));
#85793=CARTESIAN_POINT('Ctrl Pts',(-21.468609766125,5.40104689776153,2.14447533902325));
#85794=CARTESIAN_POINT('Ctrl Pts',(-21.2316651994091,1.15634042306232,5.69499075956829));
#85795=CARTESIAN_POINT('Ctrl Pts',(-20.9947206326932,-4.13693591764961,
4.0811381081697));
#85796=CARTESIAN_POINT('Ctrl Pts',(-20.7577760659773,-5.67875942494283,
-1.23357001895319));
#85797=CARTESIAN_POINT('Ctrl Pts',(-20.5208314992614,-2.07094981853471,
-5.42965544813453));
#85798=CARTESIAN_POINT('Ctrl Pts',(-20.2838869325455,3.41483985297175,-4.70200450768531));
#85799=CARTESIAN_POINT('Ctrl Pts',(-20.0469423658296,5.8039781594961,0.289527716885543));
#85800=CARTESIAN_POINT('Ctrl Pts',(-19.8099977991137,2.92993814044999,5.01851060192832));
#85801=CARTESIAN_POINT('Ctrl Pts',(-19.5730532323978,-2.60103487969802,
5.19659524892496));
#85802=CARTESIAN_POINT('Ctrl Pts',(-19.3361086656819,-5.77333149645322,
0.662291206638737));
#85803=CARTESIAN_POINT('Ctrl Pts',(-19.099164098966,-3.71024170590167,-4.47259345466305));
#85804=CARTESIAN_POINT('Ctrl Pts',(-18.86221953225,1.71737826666076,-5.55163016257556));
#85805=CARTESIAN_POINT('Ctrl Pts',(-18.6252749655341,5.58764121108655,-1.59632436793984));
#85806=CARTESIAN_POINT('Ctrl Pts',(-18.3883303988182,4.39090597492436,3.80656412374579));
#85807=CARTESIAN_POINT('Ctrl Pts',(-18.1513858321023,-0.787601104461023,
5.75757502746272));
#85808=CARTESIAN_POINT('Ctrl Pts',(-17.9144412653864,-5.25189387267684,
2.48748798511786));
#85809=CARTESIAN_POINT('Ctrl Pts',(-17.6774966986705,-4.95365168105575,
-3.03830886108399));
#85810=CARTESIAN_POINT('Ctrl Pts',(-17.4405521319546,-0.163327230963516,
-5.80889920104172));
#85811=CARTESIAN_POINT('Ctrl Pts',(-17.2036075652387,4.77510600991274,-3.31184968109235));
#85812=CARTESIAN_POINT('Ctrl Pts',(-16.9666629985228,5.38336620285286,2.18845928450913));
#85813=CARTESIAN_POINT('Ctrl Pts',(-16.7297184318069,1.10986938614095,5.70422436969573));
#85814=CARTESIAN_POINT('Ctrl Pts',(-16.492773865091,-4.17008184073304,4.04727107520497));
#85815=CARTESIAN_POINT('Ctrl Pts',(-16.2558292983751,-5.6685094835036,-1.27983825138911));
#85816=CARTESIAN_POINT('Ctrl Pts',(-16.0188847316592,-2.02660580500988,
-5.44636159517873));
#85817=CARTESIAN_POINT('Ctrl Pts',(-15.7819401649432,3.45306939451705,-4.67400229685913));
#85818=CARTESIAN_POINT('Ctrl Pts',(-15.5449955982273,5.80142395059578,0.336846938241531));
#85819=CARTESIAN_POINT('Ctrl Pts',(-15.3080510315114,2.88891737058441,5.04223582751692));
#85820=CARTESIAN_POINT('Ctrl Pts',(-15.0711064647955,-2.64332416583296,
5.17521236942885));
#85821=CARTESIAN_POINT('Ctrl Pts',(-14.8341618980796,-5.77854016290716,
0.615190458336615));
#85822=CARTESIAN_POINT('Ctrl Pts',(-14.5972173313637,-3.67364655494689,
-4.50269993489332));
#85823=CARTESIAN_POINT('Ctrl Pts',(-14.3602727646478,1.76259200439949,-5.53744120875238));
#85824=CARTESIAN_POINT('Ctrl Pts',(-14.1233281979319,5.60047266856326,-1.55070680756783));
#85825=CARTESIAN_POINT('Ctrl Pts',(-13.886383631216,4.3597193186113,3.84224324806341));
#85826=CARTESIAN_POINT('Ctrl Pts',(-13.6494390645001,-0.834525126437326,
5.75096109600007));
#85827=CARTESIAN_POINT('Ctrl Pts',(-13.4124944977842,-5.2720035012667,2.44457865428648));
#85828=CARTESIAN_POINT('Ctrl Pts',(-13.1755499310683,-4.92871105752529,
-3.07860244685626));
#85829=CARTESIAN_POINT('Ctrl Pts',(-12.9386053643524,-0.115953069741155,
-5.8100379172583));
#85830=CARTESIAN_POINT('Ctrl Pts',(-12.7016607976365,4.80195375794968,-3.27280091372428));
#85831=CARTESIAN_POINT('Ctrl Pts',(-12.4647162309206,5.36534139903216,2.23228523853764));
#85832=CARTESIAN_POINT('Ctrl Pts',(-12.2277716642046,1.06331732595328,5.7130851541605));
#85833=CARTESIAN_POINT('Ctrl Pts',(-11.9908270974887,-4.20294670667358,
4.01313153226046));
#85834=CARTESIAN_POINT('Ctrl Pts',(-11.7538825307728,-5.6578845589507,-1.32601961974504));
#85835=CARTESIAN_POINT('Ctrl Pts',(-11.5169379640569,-1.98212600941875,
-5.46270649011525));
#85836=CARTESIAN_POINT('Ctrl Pts',(-11.279993397341,3.49106878655774,-4.64568880166157));
#85837=CARTESIAN_POINT('Ctrl Pts',(-11.0430488306251,5.79848423955988,0.384143512163343));
#85838=CARTESIAN_POINT('Ctrl Pts',(-10.8061042639092,2.84770435225732,5.06562588793293));
#85839=CARTESIAN_POINT('Ctrl Pts',(-10.5691596971933,-2.6854376036436,5.15348528583311));
#85840=CARTESIAN_POINT('Ctrl Pts',(-10.3322151304774,-5.78336461184819,
0.5680488366184));
#85841=CARTESIAN_POINT('Ctrl Pts',(-10.0952705637615,-3.63680709669546,
-4.53250701662856));
#85842=CARTESIAN_POINT('Ctrl Pts',(-9.85832599704558,1.80768852424102,-5.5228840213867));
#85843=CARTESIAN_POINT('Ctrl Pts',(-9.62138143032965,5.61293171606208,-1.5049861345496));
#85844=CARTESIAN_POINT('Ctrl Pts',(-9.38443686361376,4.328242750529,3.87766687672554));
#85845=CARTESIAN_POINT('Ctrl Pts',(-9.14749229689785,-0.881393653382343,
5.74396474067666));
#85846=CARTESIAN_POINT('Ctrl Pts',(-8.91054773018194,-5.29176255742414,
2.40150676663836));
#85847=CARTESIAN_POINT('Ctrl Pts',(-8.67360316346604,-4.90344268835231,
-3.11869131470298));
#85848=CARTESIAN_POINT('Ctrl Pts',(-8.43665859675012,-0.0685711981811391,
-5.81079028232212));
#85849=CARTESIAN_POINT('Ctrl Pts',(-8.19971403003422,4.82848218985865,-3.23353451452318));
#85850=CARTESIAN_POINT('Ctrl Pts',(-7.96276946331831,5.34695981523874,2.27596275201499));
#85851=CARTESIAN_POINT('Ctrl Pts',(-7.7258248966024,1.01669455823101,5.72156603471045));
#85852=CARTESIAN_POINT('Ctrl Pts',(-7.4888803298865,-4.23553208866649,3.97872512753503));
#85853=CARTESIAN_POINT('Ctrl Pts',(-7.2519357631706,-5.64688340116356,-1.37211281161101));
#85854=CARTESIAN_POINT('Ctrl Pts',(-7.01499119645468,-1.93751440815492,
-5.4786881305806));
#85855=CARTESIAN_POINT('Ctrl Pts',(-6.77804662973878,3.52883603257905,-4.61706638150548));
#85856=CARTESIAN_POINT('Ctrl Pts',(-6.54110206302287,5.79515894564832,0.431414541838547));
#85857=CARTESIAN_POINT('Ctrl Pts',(-6.30415749630696,2.8063019700881,5.08867909827761));
#85858=CARTESIAN_POINT('Ctrl Pts',(-6.06721292959106,-2.72737246823887,
5.13141551089547));
#85859=CARTESIAN_POINT('Ctrl Pts',(-5.83026836287515,-5.78780448211972,
0.520869439846087));
#85860=CARTESIAN_POINT('Ctrl Pts',(-5.59332379615924,-3.59972580383638,
-4.56201269682687));
#85861=CARTESIAN_POINT('Ctrl Pts',(-5.35637922944334,1.85266484313302,-5.50795958323318));
#85862=CARTESIAN_POINT('Ctrl Pts',(-5.11943466272742,5.62501750963759,-1.45916537413956));
#85863=CARTESIAN_POINT('Ctrl Pts',(-4.88249009601152,4.29647838577394,3.91283263218402));
#85864=CARTESIAN_POINT('Ctrl Pts',(-4.64554552929562,-0.928203606918421,
5.73658646534971));
#85865=CARTESIAN_POINT('Ctrl Pts',(-4.4086009625797,-5.31116965584398,2.35827511401814));
#85866=CARTESIAN_POINT('Ctrl Pts',(-4.1716563958638,-4.87784838985289,-3.15857266089292));
#85867=CARTESIAN_POINT('Ctrl Pts',(-3.93471182914789,-0.0211845062766748,
-5.8111565106652));
#85868=CARTESIAN_POINT('Ctrl Pts',(-3.69776726243199,4.85468904094535,-3.19405258683419));
#85869=CARTESIAN_POINT('Ctrl Pts',(-3.46082269571607,5.3282236353341,2.31948794526136));
#85870=CARTESIAN_POINT('Ctrl Pts',(-3.22387812900017,0.970002336252103,
5.72966832074098));
#85871=CARTESIAN_POINT('Ctrl Pts',(-2.98693356228426,-4.26783227188706,
3.94405055035223));
#85872=CARTESIAN_POINT('Ctrl Pts',(-2.74998899556836,-5.63551355723462,
-1.41810784914298));
#85873=CARTESIAN_POINT('Ctrl Pts',(-2.51304442885244,-1.89276087533832,
-5.49431873304477));
#85874=CARTESIAN_POINT('Ctrl Pts',(-2.27609986213654,3.56634347106391,-4.58811143080153));
#85875=CARTESIAN_POINT('Ctrl Pts',(-2.03915529542063,5.79149660250893,0.478607882126479));
#85876=CARTESIAN_POINT('Ctrl Pts',(-1.80221072870473,2.76462017021148,5.11148805648324));
#85877=CARTESIAN_POINT('Ctrl Pts',(-1.56526616198882,-2.76894768938328,
5.10882368809493));
#85878=CARTESIAN_POINT('Ctrl Pts',(-1.32832159527291,-5.79220197525607,
0.474002779006931));
#85879=CARTESIAN_POINT('Ctrl Pts',(-1.091377028557,-3.56174699873994,-4.59188246089791));
#85880=CARTESIAN_POINT('Ctrl Pts',(-0.854432461841098,1.89625167863778,
-5.49138531706803));
#85881=CARTESIAN_POINT('Ctrl Pts',(-0.61748789512519,5.63918041352576,-1.41572643681296));
#85882=CARTESIAN_POINT('Ctrl Pts',(-0.380543328409284,4.25954727739888,
3.9526214981577));
#85883=CARTESIAN_POINT('Ctrl Pts',(-0.183089522812691,-0.0933905054163845,
5.42406526653476));
#85884=CARTESIAN_POINT('Ctrl Pts',(-0.0251264783354233,-3.16544829404585,
4.02871539009116));
#85885=CARTESIAN_POINT('Ctrl Pts',(0.0538550439032153,-4.19284607100255,
2.70912908403373));
#85886=CARTESIAN_POINT('Ctrl Pts',(0.0933458050225333,-4.51737593343784,
1.96187147285355));
#85887=CARTESIAN_POINT('Ctrl Pts',(-1.30884152590359,-4.93160574955951,
0.00236265628207036));
#85888=CARTESIAN_POINT('Ctrl Pts',(-1.23635336012139,-4.92283193517292,
-1.48758864232717));
#85889=CARTESIAN_POINT('Ctrl Pts',(-1.1638651943392,-4.199882729552,-2.98499340090942));
#85890=CARTESIAN_POINT('Ctrl Pts',(-1.091377028557,-3.02382304859632,-3.89748539694214));
#85891=CARTESIAN_POINT('Ctrl Pts',(-1.01239550631837,-1.74241410628069,
-4.89171674628795));
#85892=CARTESIAN_POINT('Ctrl Pts',(-0.933413984079733,0.0769187861785456,
-5.19155103167799));
#85893=CARTESIAN_POINT('Ctrl Pts',(-0.854432461841099,1.6104066882228,-4.66219169433051));
#85894=CARTESIAN_POINT('Ctrl Pts',(-0.775450939602464,3.14389459026709,
-4.13283235698302));
#85895=CARTESIAN_POINT('Ctrl Pts',(-0.696469417363827,4.39153750189643,
-2.77427939689798));
#85896=CARTESIAN_POINT('Ctrl Pts',(-0.617487895125191,4.78542010168994,
-1.20027826102703));
#85897=CARTESIAN_POINT('Ctrl Pts',(-0.54499193008346,5.14695908417373,0.244473980857804));
#85898=CARTESIAN_POINT('Ctrl Pts',(-0.472495965041731,4.78919380489134,
1.87074413694423));
#85899=CARTESIAN_POINT('Ctrl Pts',(-0.4,3.87692992261799,3.04758435726506));
#85900=CARTESIAN_POINT('',(-24.075,-2.36230756092325,-3.31488661006751));
#85901=CARTESIAN_POINT('Ctrl Pts',(-24.075,-2.36815640427391,-3.31717604989033));
#85902=CARTESIAN_POINT('Ctrl Pts',(-24.075,-2.46522217779123,-3.26269169255296));
#85903=CARTESIAN_POINT('Ctrl Pts',(-24.075,-2.55968914443286,-3.20413331253052));
#85904=CARTESIAN_POINT('Ctrl Pts',(-24.075,-2.65125836302674,-3.14156318060015));
#85905=CARTESIAN_POINT('Ctrl Pts',(-24.075,-2.75265715944677,-3.07227640315455));
#85906=CARTESIAN_POINT('Ctrl Pts',(-24.075,-2.85050398777766,-2.99807148801027));
#85907=CARTESIAN_POINT('Ctrl Pts',(-24.075,-2.94470883192884,-2.91935158607538));
#85908=CARTESIAN_POINT('Ctrl Pts',(-24.075,-3.00710083212058,-2.86721528479628));
#85909=CARTESIAN_POINT('Ctrl Pts',(-24.075,-3.06789492736163,-2.81309743864922));
#85910=CARTESIAN_POINT('Ctrl Pts',(-24.075,-3.12705945033238,-2.75710407731575));
#85911=CARTESIAN_POINT('Ctrl Pts',(-24.075,-3.14913589562531,-2.73621090829861));
#85912=CARTESIAN_POINT('Ctrl Pts',(-24.075,-3.17098540543271,-2.71505652816831));
#85913=CARTESIAN_POINT('Ctrl Pts',(-24.075,-3.1926061526888,-2.69364616544278));
#85914=CARTESIAN_POINT('Ctrl Pts',(-24.075,-3.21187742140056,-2.6745624192423));
#85915=CARTESIAN_POINT('Ctrl Pts',(-24.075,-3.23096928898991,-2.65527273168143));
#85916=CARTESIAN_POINT('Ctrl Pts',(-24.075,-3.24986239903768,-2.63579970423287));
#85917=CARTESIAN_POINT('Ctrl Pts',(-24.075,-3.33763886311812,-2.54532897230711));
#85918=CARTESIAN_POINT('Ctrl Pts',(-24.075,-3.42120552992453,-2.45082907208921));
#85919=CARTESIAN_POINT('Ctrl Pts',(-24.075,-3.50047047807597,-2.35272286112832));
#85920=CARTESIAN_POINT('Ctrl Pts',(-24.075,-3.58222055611672,-2.25154080538519));
#85921=CARTESIAN_POINT('Ctrl Pts',(-24.075,-3.65939552565808,-2.14652235759255));
#85922=CARTESIAN_POINT('Ctrl Pts',(-24.075,-3.73186566997445,-2.03808369899882));
#85923=CARTESIAN_POINT('Ctrl Pts',(-24.075,-3.76357135811286,-1.99064178586406));
#85924=CARTESIAN_POINT('Ctrl Pts',(-24.075,-3.79437609562932,-1.94254465774222));
#85925=CARTESIAN_POINT('Ctrl Pts',(-24.075,-3.82426691847838,-1.89382475550747));
#85926=CARTESIAN_POINT('Ctrl Pts',(-24.075,-3.83956001467533,-1.86889810309161));
#85927=CARTESIAN_POINT('Ctrl Pts',(-24.075,-3.85461385608546,-1.84380840731357));
#85928=CARTESIAN_POINT('Ctrl Pts',(-24.075,-3.86942656298479,-1.81855988523347));
#85929=CARTESIAN_POINT('Ctrl Pts',(-24.075,-3.88195432078001,-1.79720609949691));
#85930=CARTESIAN_POINT('Ctrl Pts',(-24.075,-3.8943111380858,-1.77573580108553));
#85931=CARTESIAN_POINT('Ctrl Pts',(-24.075,-3.90648349164623,-1.75417386639733));
#85932=CARTESIAN_POINT('Ctrl Pts',(-24.075,-3.97142359119054,-1.63913989387354));
#85933=CARTESIAN_POINT('Ctrl Pts',(-24.075,-4.0311892465264,-1.52137916274476));
#85934=CARTESIAN_POINT('Ctrl Pts',(-24.075,-4.08568055028152,-1.4013346551155));
#85935=CARTESIAN_POINT('Ctrl Pts',(-24.075,-4.14095875510494,-1.27955660204347));
#85936=CARTESIAN_POINT('Ctrl Pts',(-24.075,-4.19080969883921,-1.15542771938113));
#85937=CARTESIAN_POINT('Ctrl Pts',(-24.075,-4.23509479303713,-1.02936906546279));
#85938=CARTESIAN_POINT('Ctrl Pts',(-24.075,-4.27955865607226,-0.902801541474532));
#85939=CARTESIAN_POINT('Ctrl Pts',(-24.075,-4.31841214000889,-0.774287905363049));
#85940=CARTESIAN_POINT('Ctrl Pts',(-24.075,-4.35147302458191,-0.644223199816743));
#85941=CARTESIAN_POINT('Ctrl Pts',(-24.075,-4.37626868801167,-0.546674670657014));
#85942=CARTESIAN_POINT('Ctrl Pts',(-24.075,-4.39780520039582,-0.448252951430205));
#85943=CARTESIAN_POINT('Ctrl Pts',(-24.075,-4.41598771602322,-0.349117080270156));
#85944=CARTESIAN_POINT('Ctrl Pts',(-24.075,-4.42409435259613,-0.304917559406111));
#85945=CARTESIAN_POINT('Ctrl Pts',(-24.075,-4.43153406314493,-0.260576012738608));
#85946=CARTESIAN_POINT('Ctrl Pts',(-24.075,-4.43829734901448,-0.216106282184517));
#85947=CARTESIAN_POINT('Ctrl Pts',(-24.075,-4.44105429138625,-0.197978927110287));
#85948=CARTESIAN_POINT('Ctrl Pts',(-24.075,-4.44369882081601,-0.179829889752053));
#85949=CARTESIAN_POINT('Ctrl Pts',(-24.075,-4.44622832119494,-0.161675304990112));
#85950=CARTESIAN_POINT('Ctrl Pts',(-24.075,-4.46525383825745,-0.0251264572304002));
#85951=CARTESIAN_POINT('Ctrl Pts',(-24.075,-4.47780790977246,0.111941212499941));
#85952=CARTESIAN_POINT('Ctrl Pts',(-24.075,-4.48375110993555,0.249092150554736));
#85953=CARTESIAN_POINT('Ctrl Pts',(-24.075,-4.48812249139626,0.349970305669875));
#85954=CARTESIAN_POINT('Ctrl Pts',(-24.075,-4.48891660930822,0.45089430308268));
#85955=CARTESIAN_POINT('Ctrl Pts',(-24.075,-4.48606214368721,0.551699386922404));
#85956=CARTESIAN_POINT('Ctrl Pts',(-24.075,-4.48230147276619,0.684506993605575));
#85957=CARTESIAN_POINT('Ctrl Pts',(-24.075,-4.47221017375029,0.817108224592498));
#85958=CARTESIAN_POINT('Ctrl Pts',(-24.075,-4.45604820619817,0.949137326263566));
#85959=CARTESIAN_POINT('Ctrl Pts',(-24.075,-4.43963517353196,1.08321740974537));
#85960=CARTESIAN_POINT('Ctrl Pts',(-24.075,-4.41696130249557,1.21670818235846));
#85961=CARTESIAN_POINT('Ctrl Pts',(-24.075,-4.38824518180506,1.34922954103877));
#85962=CARTESIAN_POINT('Ctrl Pts',(-24.075,-4.37931508605012,1.39044083261068));
#85963=CARTESIAN_POINT('Ctrl Pts',(-24.075,-4.36980027908974,1.43155835145695));
#85964=CARTESIAN_POINT('Ctrl Pts',(-24.075,-4.35970632441813,1.47257054689663));
#85965=CARTESIAN_POINT('Ctrl Pts',(-24.075,-4.35444366245617,1.49395298103058));
#85966=CARTESIAN_POINT('Ctrl Pts',(-24.075,-4.3490235663563,1.5153067841905));
#85967=CARTESIAN_POINT('Ctrl Pts',(-24.075,-4.34344677462285,1.53663030771368));
#85968=CARTESIAN_POINT('Ctrl Pts',(-24.075,-4.33851478916861,1.55548833807884));
#85969=CARTESIAN_POINT('Ctrl Pts',(-24.075,-4.33346207484754,1.57431558186746));
#85970=CARTESIAN_POINT('Ctrl Pts',(-24.075,-4.32829137421139,1.59310410207121));
#85971=CARTESIAN_POINT('Ctrl Pts',(-24.075,-4.29192404049517,1.72525029121772));
#85972=CARTESIAN_POINT('Ctrl Pts',(-24.075,-4.24969695453619,1.85558580736706));
#85973=CARTESIAN_POINT('Ctrl Pts',(-24.075,-4.2019146732641,1.98372972318377));
#85974=CARTESIAN_POINT('Ctrl Pts',(-24.075,-4.15300946825373,2.11488512863962));
#85975=CARTESIAN_POINT('Ctrl Pts',(-24.075,-4.09828482443508,2.24374547578093));
#85976=CARTESIAN_POINT('Ctrl Pts',(-24.075,-4.03801214778829,2.36990589624912));
#85977=CARTESIAN_POINT('Ctrl Pts',(-24.075,-3.97819023957664,2.49512278577635));
#85978=CARTESIAN_POINT('Ctrl Pts',(-24.075,-3.9129026279478,2.61768076524124));
#85979=CARTESIAN_POINT('Ctrl Pts',(-24.075,-3.84236456925686,2.73717578743023));
#85980=CARTESIAN_POINT('Ctrl Pts',(-24.075,-3.79151963980002,2.82330965737785));
#85981=CARTESIAN_POINT('Ctrl Pts',(-24.075,-3.73794565441772,2.90785194850061));
#85982=CARTESIAN_POINT('Ctrl Pts',(-24.075,-3.68172933073621,2.99070582618902));
#85983=CARTESIAN_POINT('Ctrl Pts',(-24.075,-3.65713468912554,3.0269543976777));
#85984=CARTESIAN_POINT('Ctrl Pts',(-24.075,-3.63203413392643,3.06287971452895));
#85985=CARTESIAN_POINT('Ctrl Pts',(-24.075,-3.60643423361074,3.0984732479178));
#85986=CARTESIAN_POINT('Ctrl Pts',(-24.075,-3.59002992000832,3.12128144157202));
#85987=CARTESIAN_POINT('Ctrl Pts',(-24.075,-3.57342055722774,3.14395339301573));
#85988=CARTESIAN_POINT('Ctrl Pts',(-24.075,-3.55660778713698,3.16648679521622));
#85989=CARTESIAN_POINT('Ctrl Pts',(-24.075,-3.54464951465408,3.18251393185257));
#85990=CARTESIAN_POINT('Ctrl Pts',(-24.075,-3.53259319266495,3.19846442704866));
#85991=CARTESIAN_POINT('Ctrl Pts',(-24.075,-3.52044352982494,3.2143326587511));
#85992=CARTESIAN_POINT('Ctrl Pts',(-24.075,-3.43385204863387,3.32742663552169));
#85993=CARTESIAN_POINT('Ctrl Pts',(-24.075,-3.34246367499149,3.43642334193498));
#85994=CARTESIAN_POINT('Ctrl Pts',(-24.075,-3.24660658320202,3.54108838415155));
#85995=CARTESIAN_POINT('Ctrl Pts',(-24.075,-3.14949239534693,3.64712603229974));
#85996=CARTESIAN_POINT('Ctrl Pts',(-24.075,-3.04779120566173,3.74871830265496));
#85997=CARTESIAN_POINT('Ctrl Pts',(-24.075,-2.94179464465091,3.84560251040417));
#85998=CARTESIAN_POINT('Ctrl Pts',(-24.075,-2.83591529575862,3.94237958257149));
#85999=CARTESIAN_POINT('Ctrl Pts',(-24.075,-2.72574964233738,4.03445961903589));
#86000=CARTESIAN_POINT('Ctrl Pts',(-24.075,-2.61154486618463,4.12155256477766));
#86001=CARTESIAN_POINT('Ctrl Pts',(-24.075,-2.49884949462962,4.20749443350531));
#86002=CARTESIAN_POINT('Ctrl Pts',(-24.075,-2.38222058031806,4.28858070101923));
#86003=CARTESIAN_POINT('Ctrl Pts',(-24.075,-2.26186014424435,4.36449667397723));
#86004=CARTESIAN_POINT('Ctrl Pts',(-24.075,-2.23095061393297,4.38399250785596));
#86005=CARTESIAN_POINT('Ctrl Pts',(-24.075,-2.19979482468899,4.40314714871446));
#86006=CARTESIAN_POINT('Ctrl Pts',(-24.075,-2.16839587231048,4.42195480991686));
#86007=CARTESIAN_POINT('Ctrl Pts',(-24.075,-2.36815640427393,-3.31717604989031));
#86008=CARTESIAN_POINT('Ctrl Pts',(-24.0025040349583,-1.3617188644407,-4.02543705998425));
#86009=CARTESIAN_POINT('Ctrl Pts',(-23.8510265476779,1.47227864893343,-4.51291701816237));
#86010=CARTESIAN_POINT('Ctrl Pts',(-23.6205675381589,4.60615095363263,-1.3559766287573));
#86011=CARTESIAN_POINT('Ctrl Pts',(-23.383622971443,3.65518318625674,3.11589977766662));
#86012=CARTESIAN_POINT('Ctrl Pts',(-23.1466784047271,-0.612424310989975,
4.764040620714));
#86013=CARTESIAN_POINT('Ctrl Pts',(-22.9528665245548,-3.64803811708131,
2.57766597303378));
#86014=CARTESIAN_POINT('Ctrl Pts',(-22.8380361666211,-4.06550901707725,
0.614403937029799));
#86015=CARTESIAN_POINT('Ctrl Pts',(-22.8021873309261,-4.06417652423825,
0.000957366820343933));
#86016=CARTESIAN_POINT('Origin',(-24.075,-4.52129938221115E-16,0.));
#86017=CARTESIAN_POINT('',(-24.075,-4.925,-6.03138548580072E-16));
#86018=CARTESIAN_POINT('Origin',(-24.075,0.,0.));
#86019=CARTESIAN_POINT('Origin',(-24.075,0.,0.));
#86020=CARTESIAN_POINT('',(-24.075,2.36230756092324,-3.31488661006752));
#86021=CARTESIAN_POINT('Ctrl Pts',(-24.075,2.17492961456583,4.42583829068187));
#86022=CARTESIAN_POINT('Ctrl Pts',(-24.075,2.28965550950647,4.35795907372157));
#86023=CARTESIAN_POINT('Ctrl Pts',(-24.075,2.40120874042602,4.2852779095045));
#86024=CARTESIAN_POINT('Ctrl Pts',(-24.075,2.50923374297498,4.20778498795177));
#86025=CARTESIAN_POINT('Ctrl Pts',(-24.075,2.62615380967427,4.12391109447456));
#86026=CARTESIAN_POINT('Ctrl Pts',(-24.075,2.73894143904689,4.03440012317382));
#86027=CARTESIAN_POINT('Ctrl Pts',(-24.075,2.84740951963401,3.93967163892028));
#86028=CARTESIAN_POINT('Ctrl Pts',(-24.075,2.91362172535409,3.88184649945993));
#86029=CARTESIAN_POINT('Ctrl Pts',(-24.075,2.97822357748513,3.82207648115163));
#86030=CARTESIAN_POINT('Ctrl Pts',(-24.075,3.04116458918038,3.76045190069527));
#86031=CARTESIAN_POINT('Ctrl Pts',(-24.075,3.07749457133285,3.72488177165171));
#86032=CARTESIAN_POINT('Ctrl Pts',(-24.075,3.1132711002268,3.68869369961702));
#86033=CARTESIAN_POINT('Ctrl Pts',(-24.075,3.14848348994726,3.65190463013972));
#86034=CARTESIAN_POINT('Ctrl Pts',(-24.075,3.16457534766412,3.63509223892561));
#86035=CARTESIAN_POINT('Ctrl Pts',(-24.075,3.18054960258019,3.61815398695129));
#86036=CARTESIAN_POINT('Ctrl Pts',(-24.075,3.19639494117543,3.60110280017532));
#86037=CARTESIAN_POINT('Ctrl Pts',(-24.075,3.29344145236556,3.49667093976963));
#86038=CARTESIAN_POINT('Ctrl Pts',(-24.075,3.38575286062018,3.38790483579936));
#86039=CARTESIAN_POINT('Ctrl Pts',(-24.075,3.47315306439507,3.27521866189171));
#86040=CARTESIAN_POINT('Ctrl Pts',(-24.075,3.55797717983118,3.16585387084138));
#86041=CARTESIAN_POINT('Ctrl Pts',(-24.075,3.63817539662055,3.05279585502674));
#86042=CARTESIAN_POINT('Ctrl Pts',(-24.075,3.7135454129426,2.93640277138696));
#86043=CARTESIAN_POINT('Ctrl Pts',(-24.075,3.74871167292264,2.88209590455991));
#86044=CARTESIAN_POINT('Ctrl Pts',(-24.075,3.78282623953752,2.82706277914621));
#86045=CARTESIAN_POINT('Ctrl Pts',(-24.075,3.81586528773782,2.7713389298113));
#86046=CARTESIAN_POINT('Ctrl Pts',(-24.075,3.83534796990618,2.73847932564811));
#86047=CARTESIAN_POINT('Ctrl Pts',(-24.075,3.85445662143509,2.70537952834091));
#86048=CARTESIAN_POINT('Ctrl Pts',(-24.075,3.87318600005773,2.67204678176061));
#86049=CARTESIAN_POINT('Ctrl Pts',(-24.075,3.88234637995079,2.65574401872149));
#86050=CARTESIAN_POINT('Ctrl Pts',(-24.075,3.89141648248476,2.63938470305005));
#86051=CARTESIAN_POINT('Ctrl Pts',(-24.075,3.90039427182564,2.62297224029516));
#86052=CARTESIAN_POINT('Ctrl Pts',(-24.075,3.96798015327673,2.49941724028842));
#86053=CARTESIAN_POINT('Ctrl Pts',(-24.075,4.03013714290421,2.37322115583376));
#86054=CARTESIAN_POINT('Ctrl Pts',(-24.075,4.08669911225055,2.2447758702003));
#86055=CARTESIAN_POINT('Ctrl Pts',(-24.075,4.14305273718887,2.11680370912927));
#86056=CARTESIAN_POINT('Ctrl Pts',(-24.075,4.19385272226738,1.98659807729368));
#86057=CARTESIAN_POINT('Ctrl Pts',(-24.075,4.23888567590795,1.85453121402251));
#86058=CARTESIAN_POINT('Ctrl Pts',(-24.075,4.28463415928028,1.7203659370429));
#86059=CARTESIAN_POINT('Ctrl Pts',(-24.075,4.32443131919811,1.58427900590199));
#86060=CARTESIAN_POINT('Ctrl Pts',(-24.075,4.35799738760436,1.4466570002418));
#86061=CARTESIAN_POINT('Ctrl Pts',(-24.075,4.38317193890905,1.34344049599666));
#86062=CARTESIAN_POINT('Ctrl Pts',(-24.075,4.40484037060623,1.23936036076217));
#86063=CARTESIAN_POINT('Ctrl Pts',(-24.075,4.42286232376388,1.13458253413241));
#86064=CARTESIAN_POINT('Ctrl Pts',(-24.075,4.42983214075538,1.09406071776829));
#86065=CARTESIAN_POINT('Ctrl Pts',(-24.075,4.43625635126417,1.05343459359125));
#86066=CARTESIAN_POINT('Ctrl Pts',(-24.075,4.44212603033172,1.01271396551675));
#86067=CARTESIAN_POINT('Ctrl Pts',(-24.075,4.44613530083295,0.984899836149257));
#86068=CARTESIAN_POINT('Ctrl Pts',(-24.075,4.44988584300443,0.957041618230944));
#86069=CARTESIAN_POINT('Ctrl Pts',(-24.075,4.45337468872272,0.929142476094225));
#86070=CARTESIAN_POINT('Ctrl Pts',(-24.075,4.45563697462939,0.911051725983625));
#86071=CARTESIAN_POINT('Ctrl Pts',(-24.075,4.4577880479084,0.892953104338779));
#86072=CARTESIAN_POINT('Ctrl Pts',(-24.075,4.45982721955001,0.874849527478534));
#86073=CARTESIAN_POINT('Ctrl Pts',(-24.075,4.47478304533433,0.742073092150142));
#86074=CARTESIAN_POINT('Ctrl Pts',(-24.075,4.48372824823947,0.60899351884243));
#86075=CARTESIAN_POINT('Ctrl Pts',(-24.075,4.48646532204813,0.475939379020343));
#86076=CARTESIAN_POINT('Ctrl Pts',(-24.075,4.48847299247554,0.378342865210339));
#86077=CARTESIAN_POINT('Ctrl Pts',(-24.075,4.48713945358514,0.280759890275653));
#86078=CARTESIAN_POINT('Ctrl Pts',(-24.075,4.48236892158366,0.183321653579532));
#86079=CARTESIAN_POINT('Ctrl Pts',(-24.075,4.47578175720543,0.0487786546766431));
#86080=CARTESIAN_POINT('Ctrl Pts',(-24.075,4.46264317126887,-0.0854895344690163));
#86081=CARTESIAN_POINT('Ctrl Pts',(-24.075,4.44314296552314,-0.21904427821751));
#86082=CARTESIAN_POINT('Ctrl Pts',(-24.075,4.42369313349789,-0.352254017948207));
#86083=CARTESIAN_POINT('Ctrl Pts',(-24.075,4.39791402784372,-0.484754784643175));
#86084=CARTESIAN_POINT('Ctrl Pts',(-24.075,4.36594964169936,-0.61608509773256));
#86085=CARTESIAN_POINT('Ctrl Pts',(-24.075,4.35385913591727,-0.665760693021671));
#86086=CARTESIAN_POINT('Ctrl Pts',(-24.075,4.34088326963657,-0.715268498642894));
#86087=CARTESIAN_POINT('Ctrl Pts',(-24.075,4.32702839056672,-0.764582200478806));
#86088=CARTESIAN_POINT('Ctrl Pts',(-24.075,4.32173468134526,-0.78342411146457));
#86089=CARTESIAN_POINT('Ctrl Pts',(-24.075,4.3163121694248,-0.802239047480007));
#86090=CARTESIAN_POINT('Ctrl Pts',(-24.075,4.31076658107729,-0.821007896647057));
#86091=CARTESIAN_POINT('Ctrl Pts',(-24.075,4.27335222769683,-0.947635462790869));
#86092=CARTESIAN_POINT('Ctrl Pts',(-24.075,4.23028981465208,-1.07234901794428));
#86093=CARTESIAN_POINT('Ctrl Pts',(-24.075,4.18179488094431,-1.19475063707284));
#86094=CARTESIAN_POINT('Ctrl Pts',(-24.075,4.13349333262168,-1.3166641498685));
#86095=CARTESIAN_POINT('Ctrl Pts',(-24.075,4.07980199860719,-1.43628486967417));
#86096=CARTESIAN_POINT('Ctrl Pts',(-24.075,4.0208894094103,-1.55319433159216));
#86097=CARTESIAN_POINT('Ctrl Pts',(-24.075,3.96451542589954,-1.66506604132794));
#86098=CARTESIAN_POINT('Ctrl Pts',(-24.075,3.90335983940973,-1.77445551914991));
#86099=CARTESIAN_POINT('Ctrl Pts',(-24.075,3.83753818876811,-1.88096500634148));
#86100=CARTESIAN_POINT('Ctrl Pts',(-24.075,3.79191922374558,-1.95478346156703));
#86101=CARTESIAN_POINT('Ctrl Pts',(-24.075,3.74405823914087,-2.02721781351839));
#86102=CARTESIAN_POINT('Ctrl Pts',(-24.075,3.69401073517597,-2.09816998853326));
#86103=CARTESIAN_POINT('Ctrl Pts',(-24.075,3.66886589076295,-2.13381774836491));
#86104=CARTESIAN_POINT('Ctrl Pts',(-24.075,3.64316903300121,-2.16909123324359));
#86105=CARTESIAN_POINT('Ctrl Pts',(-24.075,3.61692676036711,-2.2039771396978));
#86106=CARTESIAN_POINT('Ctrl Pts',(-24.075,3.60244455312235,-2.22322947101209));
#86107=CARTESIAN_POINT('Ctrl Pts',(-24.075,3.58779623189004,-2.24236375257261));
#86108=CARTESIAN_POINT('Ctrl Pts',(-24.075,3.57298287249688,-2.26137766816133));
#86109=CARTESIAN_POINT('Ctrl Pts',(-24.075,3.56231194413342,-2.27507450260456));
#86110=CARTESIAN_POINT('Ctrl Pts',(-24.075,3.55155763390175,-2.28870591199351));
#86111=CARTESIAN_POINT('Ctrl Pts',(-24.075,3.5407265295119,-2.30226366689239));
#86112=CARTESIAN_POINT('Ctrl Pts',(-24.075,3.45910540154826,-2.40443231079706));
#86113=CARTESIAN_POINT('Ctrl Pts',(-24.075,3.37302709147514,-2.50254959411214));
#86114=CARTESIAN_POINT('Ctrl Pts',(-24.075,3.28274367897956,-2.59634605947702));
#86115=CARTESIAN_POINT('Ctrl Pts',(-24.075,3.19479267636066,-2.68771935766017));
#86116=CARTESIAN_POINT('Ctrl Pts',(-24.075,3.10285030444394,-2.77499251082065));
#86117=CARTESIAN_POINT('Ctrl Pts',(-24.075,3.00711854707771,-2.85787507032547));
#86118=CARTESIAN_POINT('Ctrl Pts',(-24.075,2.90757866320222,-2.94405462636194));
#86119=CARTESIAN_POINT('Ctrl Pts',(-24.075,2.80394144723911,-3.02548821247834));
#86120=CARTESIAN_POINT('Ctrl Pts',(-24.075,2.69640867303135,-3.10179438524463));
#86121=CARTESIAN_POINT('Ctrl Pts',(-24.075,2.59626634490311,-3.17285623450566));
#86122=CARTESIAN_POINT('Ctrl Pts',(-24.075,2.49274485090672,-3.23947105721393));
#86123=CARTESIAN_POINT('Ctrl Pts',(-24.075,2.38599459059339,-3.30128078051072));
#86124=CARTESIAN_POINT('Ctrl Pts',(-24.075,2.37811648292838,-3.30584230245407));
#86125=CARTESIAN_POINT('Ctrl Pts',(-24.075,2.37022078672256,-3.3103776307273));
#86126=CARTESIAN_POINT('Ctrl Pts',(-24.075,2.3623075609233,-3.31488661006747));
#86127=CARTESIAN_POINT('Origin',(-24.075,0.,0.));
#86128=CARTESIAN_POINT('Origin',(-26.8478126690739,0.,0.));
#86129=CARTESIAN_POINT('Ctrl Pts',(-24.075,2.36230756092323,-3.31488661006752));
#86130=CARTESIAN_POINT('Ctrl Pts',(-24.0355092388807,2.91065117590484,-2.92411720524959));
#86131=CARTESIAN_POINT('Ctrl Pts',(-23.956527716642,3.8009161537758,-1.86677512529004));
#86132=CARTESIAN_POINT('Ctrl Pts',(-23.7985646721648,4.40104888295471,0.856562345338821));
#86133=CARTESIAN_POINT('Ctrl Pts',(-23.6011108665681,2.46349467463415,4.12278630825743));
#86134=CARTESIAN_POINT('Ctrl Pts',(-23.3641662998523,-2.11355533076443,
4.31564323485309));
#86135=CARTESIAN_POINT('Ctrl Pts',(-23.1964002340208,-3.99108416375442,
1.67729393881811));
#86136=CARTESIAN_POINT('Ctrl Pts',(-23.107615690428,-4.07555252481818,0.169077405975379));
#86137=CARTESIAN_POINT('Ctrl Pts',(-23.0978126690739,-4.07427440555673,
0.002413955370523));
#86138=CARTESIAN_POINT('Ctrl Pts',(-24.5683458050225,2.8582151425001,-4.01076441581691));
#86139=CARTESIAN_POINT('Ctrl Pts',(-24.5288550439032,3.52166982958631,-3.53796271609248));
#86140=CARTESIAN_POINT('Ctrl Pts',(-24.4498735216646,4.59882374581641,-2.25865802531723));
#86141=CARTESIAN_POINT('Ctrl Pts',(-24.2919104771873,5.32493938055571,1.03637625618311));
#86142=CARTESIAN_POINT('Ctrl Pts',(-24.0944566715907,2.9806439682038,4.9882625152113));
#86143=CARTESIAN_POINT('Ctrl Pts',(-23.8575121048748,-2.55724358285579,
5.22160494574418));
#86144=CARTESIAN_POINT('Ctrl Pts',(-23.6205675381589,-5.76563780154427,
0.713091159141606));
#86145=CARTESIAN_POINT('Ctrl Pts',(-23.383622971443,-3.75101053411091,-4.43862093040455));
#86146=CARTESIAN_POINT('Ctrl Pts',(-23.1466784047271,1.66791135734842,-5.56707796774283));
#86147=CARTESIAN_POINT('Ctrl Pts',(-22.9097338380112,5.57288068372362,-1.64625563203397));
#86148=CARTESIAN_POINT('Ctrl Pts',(-22.6727892712953,4.42499321806552,3.76694508752895));
#86149=CARTESIAN_POINT('Ctrl Pts',(-22.4358447045794,-0.735970718489106,
5.76444706334991));
#86150=CARTESIAN_POINT('Ctrl Pts',(-22.1989001378635,-5.22933511388625,
2.53448853123921));
#86151=CARTESIAN_POINT('Ctrl Pts',(-21.9619555711475,-4.98072793392136,
-2.99373285471432));
#86152=CARTESIAN_POINT('Ctrl Pts',(-21.7250110044317,-0.215429665592803,
-5.80720569596091));
#86153=CARTESIAN_POINT('Ctrl Pts',(-21.4880664377157,4.74519617498286,-3.35455594069076));
#86154=CARTESIAN_POINT('Ctrl Pts',(-21.2511218709998,5.40278690230385,2.14007065312858));
#86155=CARTESIAN_POINT('Ctrl Pts',(-21.0141773042839,1.16100167435296,5.69403825692435));
#86156=CARTESIAN_POINT('Ctrl Pts',(-20.777232737568,-4.13360179746769,4.08452187604581));
#86157=CARTESIAN_POINT('Ctrl Pts',(-20.5402881708521,-5.67976472349785,
-1.22892904398937));
#86158=CARTESIAN_POINT('Ctrl Pts',(-20.3033436041362,-2.07538872218816,
-5.42796029465347));
#86159=CARTESIAN_POINT('Ctrl Pts',(-20.0663990374203,3.41099566797876,-4.70479524800842));
#86160=CARTESIAN_POINT('Ctrl Pts',(-19.8294544707044,5.80421311058715,0.284783282234712));
#86161=CARTESIAN_POINT('Ctrl Pts',(-19.5925099039885,2.9340399889667,5.0161140549384));
#86162=CARTESIAN_POINT('Ctrl Pts',(-19.3555653372726,-2.59678620885327,
5.19872023686729));
#86163=CARTESIAN_POINT('Ctrl Pts',(-19.1186207705567,-5.77278857082837,
0.667010532133052));
#86164=CARTESIAN_POINT('Ctrl Pts',(-18.8816762038408,-3.71389697834065,
-4.46955927193808));
#86165=CARTESIAN_POINT('Ctrl Pts',(-18.6447316371249,1.71283953929854,-5.55303264456375));
#86166=CARTESIAN_POINT('Ctrl Pts',(-18.407787070409,5.58633481703289,-1.60089168284028));
#86167=CARTESIAN_POINT('Ctrl Pts',(-18.170842503693,4.39401659788682,3.80297370387212));
#86168=CARTESIAN_POINT('Ctrl Pts',(-17.9338979369771,-0.782894255534373,
5.75821738380674));
#86169=CARTESIAN_POINT('Ctrl Pts',(-17.6969533702612,-5.24985906935669,
2.4917806103693));
#86170=CARTESIAN_POINT('Ctrl Pts',(-17.4600088035453,-4.95613413085725,
-3.0342586134341));
#86171=CARTESIAN_POINT('Ctrl Pts',(-17.2230642368294,-0.168075791623614,
-5.80876418738683));
#86172=CARTESIAN_POINT('Ctrl Pts',(-16.9861196701135,4.77239743889964,-3.31575233424595));
#86173=CARTESIAN_POINT('Ctrl Pts',(-16.7491751033976,5.38515381465317,2.18405797750162));
#86174=CARTESIAN_POINT('Ctrl Pts',(-16.5122305366817,1.11453213417911,5.70331561273725));
#86175=CARTESIAN_POINT('Ctrl Pts',(-16.2752859699658,-4.16677224069193,
4.05067894936963));
#86176=CARTESIAN_POINT('Ctrl Pts',(-16.0383414032499,-5.66955425092678,
-1.2752040826549));
#86177=CARTESIAN_POINT('Ctrl Pts',(-15.801396836534,-2.03105752138112,-5.44470349986785));
#86178=CARTESIAN_POINT('Ctrl Pts',(-15.564452269818,3.44924764526761,-4.67682387291358));
#86179=CARTESIAN_POINT('Ctrl Pts',(-15.3275077031022,5.8016978162655,0.332104359158765));
#86180=CARTESIAN_POINT('Ctrl Pts',(-15.0905631363862,2.89303850364856,5.03987292231073));
#86181=CARTESIAN_POINT('Ctrl Pts',(-14.8536185696703,-2.63909290111009,
5.17737187344555));
#86182=CARTESIAN_POINT('Ctrl Pts',(-14.6166740029544,-5.77803577211796,
0.619914084981969));
#86183=CARTESIAN_POINT('Ctrl Pts',(-14.3797294362385,-3.67732643095217,
-4.49969567602683));
#86184=CARTESIAN_POINT('Ctrl Pts',(-14.1427848695226,1.75806485555589,-5.53888064687201));
#86185=CARTESIAN_POINT('Ctrl Pts',(-13.9058403028067,5.59920356681868,-1.55528462795688));
#86186=CARTESIAN_POINT('Ctrl Pts',(-13.6688957360908,4.36285911384371,3.83867831543423));
#86187=CARTESIAN_POINT('Ctrl Pts',(-13.4319511693749,-0.829823670846763,
5.75164181186002));
#86188=CARTESIAN_POINT('Ctrl Pts',(-13.195006602659,-5.2700037705162,2.44888773025208));
#86189=CARTESIAN_POINT('Ctrl Pts',(-12.9580620359431,-4.93122645223466,
-3.07457257735367));
#86190=CARTESIAN_POINT('Ctrl Pts',(-12.7211174692272,-0.120702573666628,
-5.80994163011507));
#86191=CARTESIAN_POINT('Ctrl Pts',(-12.4841729025113,4.79927710131223,-3.27672552427787));
#86192=CARTESIAN_POINT('Ctrl Pts',(-12.2472283357954,5.3671648418537,2.22789865501186));
#86193=CARTESIAN_POINT('Ctrl Pts',(-12.0102837690794,1.06798732945511,5.71221444982219));
#86194=CARTESIAN_POINT('Ctrl Pts',(-11.7733392023636,-4.19966500623136,
4.01656628129922));
#86195=CARTESIAN_POINT('Ctrl Pts',(-11.5363946356476,-5.6589670810085,-1.32139412466384));
#86196=CARTESIAN_POINT('Ctrl Pts',(-11.2994500689317,-1.98659109873622,
-5.4610847514991));
#86197=CARTESIAN_POINT('Ctrl Pts',(-11.0625055022158,3.48727017294997,-4.64854144839944));
#86198=CARTESIAN_POINT('Ctrl Pts',(-10.8255609354999,5.79879676953481,0.379403324006022));
#86199=CARTESIAN_POINT('Ctrl Pts',(-10.588616368784,2.85184461663589,5.06329666711314));
#86200=CARTESIAN_POINT('Ctrl Pts',(-10.3516718020681,-2.68122408930307,
5.15567922194299));
#86201=CARTESIAN_POINT('Ctrl Pts',(-10.1147272353522,-5.78289875669314,
0.572776419269867));
#86202=CARTESIAN_POINT('Ctrl Pts',(-9.87778266863627,-3.6405113486111,-4.52953286523761));
#86203=CARTESIAN_POINT('Ctrl Pts',(-9.6408381019204,1.80317326383209,-5.52436032833061));
#86204=CARTESIAN_POINT('Ctrl Pts',(-9.40389353520446,5.61169998639889,-1.50957415163656));
#86205=CARTESIAN_POINT('Ctrl Pts',(-9.16694896848858,4.33141151164837,3.87412766611946));
#86206=CARTESIAN_POINT('Ctrl Pts',(-8.93000440177265,-0.876697905012197,
5.74468377197292));
#86207=CARTESIAN_POINT('Ctrl Pts',(-8.69305983505676,-5.28979803156989,
2.4058320061605));
#86208=CARTESIAN_POINT('Ctrl Pts',(-8.45611526834085,-4.90599086103837,
-3.11468209100355));
#86209=CARTESIAN_POINT('Ctrl Pts',(-8.21917070162494,-0.0733213293745337,
-5.8107327282556));
#86210=CARTESIAN_POINT('Ctrl Pts',(-7.98222613490903,4.82583762550951,-3.23748082142428));
#86211=CARTESIAN_POINT('Ctrl Pts',(-7.74528156819313,5.3488189678476,2.27159118364012));
#86212=CARTESIAN_POINT('Ctrl Pts',(-7.50833700147721,1.02137150668363,5.72073344087819));
#86213=CARTESIAN_POINT('Ctrl Pts',(-7.27139243476131,-4.23227850613741,
3.9821865231059));
#86214=CARTESIAN_POINT('Ctrl Pts',(-7.0344478680454,-5.64800360567914,-1.36749629789557));
#86215=CARTESIAN_POINT('Ctrl Pts',(-6.7975033013295,-1.94199257388176,-5.47710285624032));
#86216=CARTESIAN_POINT('Ctrl Pts',(-6.56055873461358,3.52506080794271,-4.61994990973791));
#86217=CARTESIAN_POINT('Ctrl Pts',(-6.32361416789768,5.79551011773543,0.426677060786518));
#86218=CARTESIAN_POINT('Ctrl Pts',(-6.08666960118177,2.81046109317731,5.08638371486386));
#86219=CARTESIAN_POINT('Ctrl Pts',(-5.84972503446586,-2.72317698967916,
5.13364373679603));
#86220=CARTESIAN_POINT('Ctrl Pts',(-5.61278046774996,-5.78737718356205,
0.525600657238108));
#86221=CARTESIAN_POINT('Ctrl Pts',(-5.37583590103405,-3.60345420458392,
-4.55906883743519));
#86222=CARTESIAN_POINT('Ctrl Pts',(-5.13889133431814,1.84816180838766,-5.50947268628944));
#86223=CARTESIAN_POINT('Ctrl Pts',(-4.90194676760224,5.62382316291067,-1.46376323391524));
#86224=CARTESIAN_POINT('Ctrl Pts',(-4.66500220088632,4.29967603859304,3.90931928494839));
#86225=CARTESIAN_POINT('Ctrl Pts',(-4.42805763417043,-0.923514140359199,
5.73734394489365));
#86226=CARTESIAN_POINT('Ctrl Pts',(-4.19111306745451,-5.30923996143927,
2.36261588240264));
#86227=CARTESIAN_POINT('Ctrl Pts',(-3.95416850073861,-4.88043013966745,
-3.15458368267413));
#86228=CARTESIAN_POINT('Ctrl Pts',(-3.71722393402269,-0.0259330876983714,
-5.81113897502467));
#86229=CARTESIAN_POINT('Ctrl Pts',(-3.4802793673068,4.85207316848768,-3.19801786516862));
#86230=CARTESIAN_POINT('Ctrl Pts',(-3.24333480059088,5.33012524590221,2.3151269509498));
#86231=CARTESIAN_POINT('Ctrl Pts',(-3.00639023387499,0.9746727144288,5.72888298509305));
#86232=CARTESIAN_POINT('Ctrl Pts',(-2.76944566715907,-4.26458165159571,
3.94752089103779));
#86233=CARTESIAN_POINT('Ctrl Pts',(-2.53250110044317,-5.63672012231858,
-1.41346705206928));
#86234=CARTESIAN_POINT('Ctrl Pts',(-2.29555653372726,-1.89715814085517,
-5.49283453792041));
#86235=CARTESIAN_POINT('Ctrl Pts',(-2.05861196701135,3.56241187898916,-4.59090168980564));
#86236=CARTESIAN_POINT('Ctrl Pts',(-1.82166740029544,5.79223230496278,0.473635218544011));
#86237=CARTESIAN_POINT('Ctrl Pts',(-1.58472283357953,2.76813296477938,5.10968449907998));
#86238=CARTESIAN_POINT('Ctrl Pts',(-1.34777826686363,-2.76349068556974,
5.11020522979376));
#86239=CARTESIAN_POINT('Ctrl Pts',(-1.11083370014772,-5.79429292799479,
0.480439815238698));
#86240=CARTESIAN_POINT('Ctrl Pts',(-0.873889133431811,-3.56054538524804,
-4.59233251686338));
#86241=CARTESIAN_POINT('Ctrl Pts',(-0.676435327835228,0.973652097174675,
-5.33676463268154));
#86242=CARTESIAN_POINT('Ctrl Pts',(-0.518472283357948,3.77810762024814,
-3.46072517404051));
#86243=CARTESIAN_POINT('Ctrl Pts',(-0.439490761119318,4.57738664511715,
-1.99170029627505));
#86244=CARTESIAN_POINT('Ctrl Pts',(-0.4,4.77615934004777,-1.20163511869221));
#86245=CARTESIAN_POINT('Ctrl Pts',(-24.4038972033484,2.69291261530781,-3.77880514723378));
#86246=CARTESIAN_POINT('Ctrl Pts',(-24.364406442229,3.31799694502582,-3.33334754581152));
#86247=CARTESIAN_POINT('Ctrl Pts',(-24.2854249199904,4.33285454846954,-2.12803039197483));
#86248=CARTESIAN_POINT('Ctrl Pts',(-24.1274618755131,5.01697588135538,0.976438285901677));
#86249=CARTESIAN_POINT('Ctrl Pts',(-23.9300080699166,2.80826087034725,4.69977044622668));
#86250=CARTESIAN_POINT('Ctrl Pts',(-23.6930635032006,-2.40934749882534,
4.91961770878048));
#86251=CARTESIAN_POINT('Ctrl Pts',(-23.4561189364847,-5.43218687082214,
0.671850117145879));
#86252=CARTESIAN_POINT('Ctrl Pts',(-23.2191743697688,-3.53407391811104,
-4.18191693141772));
#86253=CARTESIAN_POINT('Ctrl Pts',(-22.9822298030529,1.57144907275594,-5.24511058206187));
#86254=CARTESIAN_POINT('Ctrl Pts',(-22.745285236337,5.25057770272587,-1.55104578854338));
#86255=CARTESIAN_POINT('Ctrl Pts',(-22.5083406696211,4.1690773666383,3.54908690970877));
#86256=CARTESIAN_POINT('Ctrl Pts',(-22.2713961029052,-0.693406455954522,
5.43106499799406));
#86257=CARTESIAN_POINT('Ctrl Pts',(-22.0344515361893,-4.92690080899178,
2.38790846694518));
#86258=CARTESIAN_POINT('Ctrl Pts',(-21.7975069694733,-4.69267162126242,
-2.82059277184779));
#86259=CARTESIAN_POINT('Ctrl Pts',(-21.5605624027575,-0.202970467674054,
-5.47135072017758));
#86260=CARTESIAN_POINT('Ctrl Pts',(-21.3236178360415,4.47076164831466,-3.16054795075367));
#86261=CARTESIAN_POINT('Ctrl Pts',(-21.0866732693257,5.09032115556824,2.01630142313886));
#86262=CARTESIAN_POINT('Ctrl Pts',(-20.8497287026097,1.09385609528459,5.36472822710765));
#86263=CARTESIAN_POINT('Ctrl Pts',(-20.6127841358939,-3.89453832972245,
3.84829690527888));
#86264=CARTESIAN_POINT('Ctrl Pts',(-20.3758395691779,-5.35128019177339,
-1.15785494124226));
#86265=CARTESIAN_POINT('Ctrl Pts',(-20.138895002462,-1.95536031859356,-5.1140386654297));
#86266=CARTESIAN_POINT('Ctrl Pts',(-19.9019504357461,3.21372353273086,-4.43269727579702));
#86267=CARTESIAN_POINT('Ctrl Pts',(-19.6650058690302,5.46853120852308,0.268313074812095));
#86268=CARTESIAN_POINT('Ctrl Pts',(-19.4280613023143,2.7643521940041,4.72601121500983));
#86269=CARTESIAN_POINT('Ctrl Pts',(-19.1911167355984,-2.44660320949863,
4.89805651826131));
#86270=CARTESIAN_POINT('Ctrl Pts',(-18.9541721688825,-5.43892408123292,
0.628434525384623));
#86271=CARTESIAN_POINT('Ctrl Pts',(-18.7172276021666,-3.49910679438177,
-4.21106597935799));
#86272=CARTESIAN_POINT('Ctrl Pts',(-18.4802830354507,1.61377887017298,-5.23187755862264));
#86273=CARTESIAN_POINT('Ctrl Pts',(-18.2433384687348,5.26325372727624,-1.50830542612371));
#86274=CARTESIAN_POINT('Ctrl Pts',(-18.0063939020189,4.13989225386688,3.58303184059237));
#86275=CARTESIAN_POINT('Ctrl Pts',(-17.769449335303,-0.737616208742238,
5.42519560685493));
#86276=CARTESIAN_POINT('Ctrl Pts',(-17.532504768587,-4.94623777834044,2.34767052363083));
#86277=CARTESIAN_POINT('Ctrl Pts',(-17.2955602018711,-4.66950018061578,
-2.85877475656918));
#86278=CARTESIAN_POINT('Ctrl Pts',(-17.0586156351552,-0.158355266145258,
-5.47281907753085));
#86279=CARTESIAN_POINT('Ctrl Pts',(-16.8216710684393,4.49638974945534,-3.12398851904368));
#86280=CARTESIAN_POINT('Ctrl Pts',(-16.5847265017234,5.07370786307136,2.05774477670468));
#86281=CARTESIAN_POINT('Ctrl Pts',(-16.3477819350075,1.05007408283181,5.3734690346605));
#86282=CARTESIAN_POINT('Ctrl Pts',(-16.1108373682916,-3.92579038758392,
3.81641125649406));
#86283=CARTESIAN_POINT('Ctrl Pts',(-15.8738928015757,-5.3416602335043,-1.20145370102185));
#86284=CARTESIAN_POINT('Ctrl Pts',(-15.6369482348598,-1.91359297640511,
-5.1298135411107));
#86285=CARTESIAN_POINT('Ctrl Pts',(-15.4000036681439,3.24976323830444,-4.40634360222628));
#86286=CARTESIAN_POINT('Ctrl Pts',(-15.163059101428,5.46616138418435,0.312897376085954));
#86287=CARTESIAN_POINT('Ctrl Pts',(-14.926114534712,2.72572199594175,4.74839600778522));
#86288=CARTESIAN_POINT('Ctrl Pts',(-14.6891699679962,-2.48646312892746,
4.87794281991868));
#86289=CARTESIAN_POINT('Ctrl Pts',(-14.4522254012802,-5.443867814942,0.584061862605154));
#86290=CARTESIAN_POINT('Ctrl Pts',(-14.2152808345644,-3.46465127459014,
-4.2394594692475));
#86291=CARTESIAN_POINT('Ctrl Pts',(-13.9783362678484,1.65638861737841,-5.21854403010367));
#86292=CARTESIAN_POINT('Ctrl Pts',(-13.7413917011325,5.27537822347882,-1.46533601783238));
#86293=CARTESIAN_POINT('Ctrl Pts',(-13.5044471344166,4.11053673734424,3.61667150524551));
#86294=CARTESIAN_POINT('Ctrl Pts',(-13.2675025677007,-0.781831499832336,
5.41900032771556));
#86295=CARTESIAN_POINT('Ctrl Pts',(-13.0305580009848,-4.96521742723999,
2.30725831803544));
#86296=CARTESIAN_POINT('Ctrl Pts',(-12.7936134342689,-4.64603301714601,
-2.89675719546884));
#86297=CARTESIAN_POINT('Ctrl Pts',(-12.556668867553,-0.113721839372316,
-5.47392842382517));
#86298=CARTESIAN_POINT('Ctrl Pts',(-12.3197243008371,4.52171484865091,-3.08721879260303));
#86299=CARTESIAN_POINT('Ctrl Pts',(-12.0827797341212,5.05675926775122,2.09904996460866));
#86300=CARTESIAN_POINT('Ctrl Pts',(-11.8458351674053,1.00622115869235,5.3818532148054));
#86301=CARTESIAN_POINT('Ctrl Pts',(-11.6088906006894,-3.95678082702158,
3.78427146658718));
#86302=CARTESIAN_POINT('Ctrl Pts',(-11.3719460339735,-5.33168536386997,
-1.24497237985674));
#86303=CARTESIAN_POINT('Ctrl Pts',(-11.1350014672575,-1.87169823282282,
-5.14524739649701));
#86304=CARTESIAN_POINT('Ctrl Pts',(-10.8980569005417,3.28558676430121,-4.37969686852414));
#86305=CARTESIAN_POINT('Ctrl Pts',(-10.6611123338257,5.46342811711062,0.357460844116834));
#86306=CARTESIAN_POINT('Ctrl Pts',(-10.4241677671098,2.68691052357899,4.77046505952951));
#86307=CARTESIAN_POINT('Ctrl Pts',(-10.1872232003939,-2.52615769442597,
4.85750474511386));
#86308=CARTESIAN_POINT('Ctrl Pts',(-9.95027863367801,-5.44844955279505,
0.539650365106313));
#86309=CARTESIAN_POINT('Ctrl Pts',(-9.71333406696212,-3.42996536232423,
-4.26757104910595));
#86310=CARTESIAN_POINT('Ctrl Pts',(-9.47638950024621,1.69888821787986,-5.20486348226912));
#86311=CARTESIAN_POINT('Ctrl Pts',(-9.23944493353029,5.2871519228877,-1.42226916939806));
#86312=CARTESIAN_POINT('Ctrl Pts',(-9.00250036681439,4.08090788141461,3.65007067182512));
#86313=CARTESIAN_POINT('Ctrl Pts',(-8.76555580009848,-0.825994801131819,
5.41244470035525));
#86314=CARTESIAN_POINT('Ctrl Pts',(-8.52861123338258,-4.98386690344967,
2.26669268641333));
#86315=CARTESIAN_POINT('Ctrl Pts',(-8.29166666666667,-4.62225690565715,
-2.93454700831237));
#86316=CARTESIAN_POINT('Ctrl Pts',(-8.05472209995076,-0.0690808504607675,
-5.47467376945395));
#86317=CARTESIAN_POINT('Ctrl Pts',(-7.81777753323485,4.54673926672794,-3.05024377493309));
#86318=CARTESIAN_POINT('Ctrl Pts',(-7.58083296651895,5.03947441231285,2.14021557169967));
#86319=CARTESIAN_POINT('Ctrl Pts',(-7.34388839980303,0.962301323775909,
5.38987951700474));
#86320=CARTESIAN_POINT('Ctrl Pts',(-7.10694383308713,-3.98750815192461,
3.75188003349546));
#86321=CARTESIAN_POINT('Ctrl Pts',(-6.86999926637122,-5.32135595213918,
-1.28840827173304));
#86322=CARTESIAN_POINT('Ctrl Pts',(-6.63305469965532,-1.82967902705385,
-5.16033910729566));
#86323=CARTESIAN_POINT('Ctrl Pts',(-6.39611013293941,3.32119180893176,-4.35275889803766));
#86324=CARTESIAN_POINT('Ctrl Pts',(-6.1591655662235,5.46033154612088,0.402000543125495));
#86325=CARTESIAN_POINT('Ctrl Pts',(-5.92222099950759,2.64792038223854,4.79221688681979));
#86326=CARTESIAN_POINT('Ctrl Pts',(-5.68527643279169,-2.56568428323716,
4.83674366416711));
#86327=CARTESIAN_POINT('Ctrl Pts',(-5.44833186607578,-5.45266897352119,
0.495202974557197));
#86328=CARTESIAN_POINT('Ctrl Pts',(-5.21138729935988,-3.39505138781118,
-4.29539883258997));
#86329=CARTESIAN_POINT('Ctrl Pts',(-4.97444273264396,1.7412748868806,-5.19083685478796));
#86330=CARTESIAN_POINT('Ctrl Pts',(-4.73749816592806,5.29857396543472,-1.37910768850874));
#86331=CARTESIAN_POINT('Ctrl Pts',(-4.50055359921215,4.05100780339995,3.68322701225883));
#86332=CARTESIAN_POINT('Ctrl Pts',(-4.26360903249624,-0.870103457926947,
5.40552936615175));
#86333=CARTESIAN_POINT('Ctrl Pts',(-4.02666446578034,-5.00218442525993,
2.22597593170799));
#86334=CARTESIAN_POINT('Ctrl Pts',(-3.78971989906444,-4.5981744676305,-2.97214092417364));
#86335=CARTESIAN_POINT('Ctrl Pts',(-3.55277533234852,-0.0244332688531125,
-5.47505652127451));
#86336=CARTESIAN_POINT('Ctrl Pts',(-3.31583076563262,4.57145749860798,-3.01306312636748));
#86337=CARTESIAN_POINT('Ctrl Pts',(-3.0788861989167,5.0218618264353,2.18123348363432));
#86338=CARTESIAN_POINT('Ctrl Pts',(-2.84194163220081,0.918303317848106,
5.39755773901779));
#86339=CARTESIAN_POINT('Ctrl Pts',(-2.60499706548489,-4.01794307147468,
3.7192192598099));
#86340=CARTESIAN_POINT('Ctrl Pts',(-2.36805249876899,-5.31072503977907,
-1.33172034506469));
#86341=CARTESIAN_POINT('Ctrl Pts',(-2.13110793205308,-1.78743755666829,
-5.17516096007589));
#86342=CARTESIAN_POINT('Ctrl Pts',(-1.89416336533717,3.35638271143614,-4.32539065806695));
#86343=CARTESIAN_POINT('Ctrl Pts',(-1.65721879862126,5.45724330296002,0.446242914364961));
#86344=CARTESIAN_POINT('Ctrl Pts',(-1.42027423190536,2.60804026641022,4.8141700893024));
#86345=CARTESIAN_POINT('Ctrl Pts',(-1.18332966518945,-2.60366646960906,
4.81466070398266));
#86346=CARTESIAN_POINT('Ctrl Pts',(-0.946385098473544,-5.45918475155002,
0.452653972793905));
#86347=CARTESIAN_POINT('Ctrl Pts',(-0.709440531757633,-3.35462416482876,
-4.32673873441604));
#86348=CARTESIAN_POINT('Ctrl Pts',(-0.51198672616105,0.917341727155359,
-5.02811722972881));
#86349=CARTESIAN_POINT('Ctrl Pts',(-0.354023681683771,3.55960386650859,
-3.26057697361968));
#86350=CARTESIAN_POINT('Ctrl Pts',(-0.27504215944514,4.31265724489702,-1.87651194411482));
#86351=CARTESIAN_POINT('Ctrl Pts',(-0.235551398325822,4.49993408413774,
-1.13213953771605));
#86352=CARTESIAN_POINT('Ctrl Pts',(-24.2394486016742,2.52761008811552,-3.54684587865065));
#86353=CARTESIAN_POINT('Ctrl Pts',(-24.1999578405549,3.11432406046533,-3.12873237553055));
#86354=CARTESIAN_POINT('Ctrl Pts',(-24.1209763183162,4.06688535112267,-1.99740275863244));
#86355=CARTESIAN_POINT('Ctrl Pts',(-23.963013273839,4.70901238215504,0.916500315620253));
#86356=CARTESIAN_POINT('Ctrl Pts',(-23.7655594682423,2.6358777724907,4.41127837724205));
#86357=CARTESIAN_POINT('Ctrl Pts',(-23.5286149015265,-2.26145141479489,
4.61763047181679));
#86358=CARTESIAN_POINT('Ctrl Pts',(-23.2916703348105,-5.0987359401,0.630609075150145));
#86359=CARTESIAN_POINT('Ctrl Pts',(-23.0547257680947,-3.31713730211117,
-3.92521293243088));
#86360=CARTESIAN_POINT('Ctrl Pts',(-22.8177812013787,1.47498678816346,-4.9231431963809));
#86361=CARTESIAN_POINT('Ctrl Pts',(-22.5808366346628,4.92827472172813,-1.45583594505279));
#86362=CARTESIAN_POINT('Ctrl Pts',(-22.3438920679469,3.91316151521107,3.33122873188859));
#86363=CARTESIAN_POINT('Ctrl Pts',(-22.106947501231,-0.650842193419926,
5.09768293263822));
#86364=CARTESIAN_POINT('Ctrl Pts',(-21.8700029345151,-4.62446650409733,
2.24132840265115));
#86365=CARTESIAN_POINT('Ctrl Pts',(-21.6330583677992,-4.40461530860346,
-2.64745268898125));
#86366=CARTESIAN_POINT('Ctrl Pts',(-21.3961138010833,-0.190511269755314,
-5.13549574439427));
#86367=CARTESIAN_POINT('Ctrl Pts',(-21.1591692343674,4.19632712164646,-2.96653996081657));
#86368=CARTESIAN_POINT('Ctrl Pts',(-20.9222246676515,4.77785540883261,1.89253219314915));
#86369=CARTESIAN_POINT('Ctrl Pts',(-20.6852801009356,1.02671051621624,5.03541819729095));
#86370=CARTESIAN_POINT('Ctrl Pts',(-20.4483355342197,-3.65547486197721,
3.61207193451195));
#86371=CARTESIAN_POINT('Ctrl Pts',(-20.2113909675038,-5.02279566004892,
-1.08678083849515));
#86372=CARTESIAN_POINT('Ctrl Pts',(-19.9744464007879,-1.83533191499897,
-4.80011703620592));
#86373=CARTESIAN_POINT('Ctrl Pts',(-19.7375018340719,3.01645139748298,-4.16059930358563));
#86374=CARTESIAN_POINT('Ctrl Pts',(-19.500557267356,5.132849306459,0.25184286738948));
#86375=CARTESIAN_POINT('Ctrl Pts',(-19.2636127006401,2.59466439904151,4.43590837508125));
#86376=CARTESIAN_POINT('Ctrl Pts',(-19.0266681339242,-2.29642021014399,
4.59739279965534));
#86377=CARTESIAN_POINT('Ctrl Pts',(-18.7897235672083,-5.10505959163747,
0.58985851863619));
#86378=CARTESIAN_POINT('Ctrl Pts',(-18.5527790004924,-3.2843166104229,-3.9525726867779));
#86379=CARTESIAN_POINT('Ctrl Pts',(-18.3158344337765,1.51471820104741,-4.91072247268154));
#86380=CARTESIAN_POINT('Ctrl Pts',(-18.0788898670606,4.94017263751959,-1.41571916940714));
#86381=CARTESIAN_POINT('Ctrl Pts',(-17.8419453003447,3.88576790984695,3.36308997731261));
#86382=CARTESIAN_POINT('Ctrl Pts',(-17.6050007336288,-0.692338161950112,
5.09217382990313));
#86383=CARTESIAN_POINT('Ctrl Pts',(-17.3680561669129,-4.64261648732419,
2.20356043689236));
#86384=CARTESIAN_POINT('Ctrl Pts',(-17.131111600197,-4.38286623037431,-2.68329089970427));
#86385=CARTESIAN_POINT('Ctrl Pts',(-16.8941670334811,-0.1486347406669,-5.13687396767488));
#86386=CARTESIAN_POINT('Ctrl Pts',(-16.6572224667652,4.22038206001104,-2.93222470384142));
#86387=CARTESIAN_POINT('Ctrl Pts',(-16.4202779000492,4.76226191148954,1.93143157590774));
#86388=CARTESIAN_POINT('Ctrl Pts',(-16.1833333333333,0.985616031484506,
5.04362245658377));
#86389=CARTESIAN_POINT('Ctrl Pts',(-15.9463887666174,-3.6848085344759,3.58214356361848));
#86390=CARTESIAN_POINT('Ctrl Pts',(-15.7094441999015,-5.01376621608183,
-1.12770331938881));
#86391=CARTESIAN_POINT('Ctrl Pts',(-15.4724996331856,-1.7961284314291,-4.81492358235354));
#86392=CARTESIAN_POINT('Ctrl Pts',(-15.2355550664697,3.05027883134127,-4.13586333153898));
#86393=CARTESIAN_POINT('Ctrl Pts',(-14.9986104997538,5.13062495210321,0.293690393013142));
#86394=CARTESIAN_POINT('Ctrl Pts',(-14.7616659330379,2.55840548823495,4.45691909325972));
#86395=CARTESIAN_POINT('Ctrl Pts',(-14.524721366322,-2.33383335674485,4.57851376639182));
#86396=CARTESIAN_POINT('Ctrl Pts',(-14.2877767996061,-5.10969985776604,
0.548209640228335));
#86397=CARTESIAN_POINT('Ctrl Pts',(-14.0508322328902,-3.25197611822812,
-3.97922326246816));
#86398=CARTESIAN_POINT('Ctrl Pts',(-13.8138876661743,1.55471237920095,-4.89820741333533));
#86399=CARTESIAN_POINT('Ctrl Pts',(-13.5769430994583,4.95155288013896,-1.37538740770787));
#86400=CARTESIAN_POINT('Ctrl Pts',(-13.3399985327425,3.85821436084477,3.3946646950568));
#86401=CARTESIAN_POINT('Ctrl Pts',(-13.1030539660265,-0.733839328817908,
5.0863588435711));
#86402=CARTESIAN_POINT('Ctrl Pts',(-12.8661093993107,-4.66043108396379,
2.16562890581881));
#86403=CARTESIAN_POINT('Ctrl Pts',(-12.6291648325947,-4.36083958205737,
-2.718941813584));
#86404=CARTESIAN_POINT('Ctrl Pts',(-12.3922202658788,-0.106741105077996,
-5.13791521753527));
#86405=CARTESIAN_POINT('Ctrl Pts',(-12.1552756991629,4.24415259598959,-2.89771206092819));
#86406=CARTESIAN_POINT('Ctrl Pts',(-11.918331132447,4.74635369364874,1.97020127420546));
#86407=CARTESIAN_POINT('Ctrl Pts',(-11.6813865657311,0.944454987929595,
5.05149197978862));
#86408=CARTESIAN_POINT('Ctrl Pts',(-11.4444419990152,-3.71389664781181,
3.55197665187513));
#86409=CARTESIAN_POINT('Ctrl Pts',(-11.2074974322993,-5.00440364673143,
-1.16855063504964));
#86410=CARTESIAN_POINT('Ctrl Pts',(-10.9705528655834,-1.75680536690942,
-4.82941004149492));
#86411=CARTESIAN_POINT('Ctrl Pts',(-10.7336082988675,3.08390335565245,-4.11085228864884));
#86412=CARTESIAN_POINT('Ctrl Pts',(-10.4966637321515,5.12805946468642,0.335518364227643));
#86413=CARTESIAN_POINT('Ctrl Pts',(-10.2597191654357,2.52197643052209,4.4776334519459));
#86414=CARTESIAN_POINT('Ctrl Pts',(-10.0227745987197,-2.37109129954888,
4.55933026828472));
#86415=CARTESIAN_POINT('Ctrl Pts',(-9.78583003200384,-5.11400034889696,
0.506524310942766));
#86416=CARTESIAN_POINT('Ctrl Pts',(-9.54888546528793,-3.21941937603737,
-4.00560923297429));
#86417=CARTESIAN_POINT('Ctrl Pts',(-9.31194089857203,1.59460317192763,-4.88536663620762));
#86418=CARTESIAN_POINT('Ctrl Pts',(-9.07499633185612,4.96260385937652,-1.33496418715956));
#86419=CARTESIAN_POINT('Ctrl Pts',(-8.83805176514022,3.83040425118085,3.42601367753078));
#86420=CARTESIAN_POINT('Ctrl Pts',(-8.60110719842429,-0.775291697251443,
5.0802056287376));
#86421=CARTESIAN_POINT('Ctrl Pts',(-8.36416263170841,-4.67793577532945,
2.12755336666615));
#86422=CARTESIAN_POINT('Ctrl Pts',(-8.12721806499248,-4.33852295027593,
-2.75441192562119));
#86423=CARTESIAN_POINT('Ctrl Pts',(-7.8902734982766,-0.0648403715470012,
-5.13861481065229));
#86424=CARTESIAN_POINT('Ctrl Pts',(-7.65332893156067,4.26764090794638,-2.8630067284419));
#86425=CARTESIAN_POINT('Ctrl Pts',(-7.41638436484477,4.7301298567781,2.00883995975922));
#86426=CARTESIAN_POINT('Ctrl Pts',(-7.17943979812886,0.903231140868191,
5.05902559313128));
#86427=CARTESIAN_POINT('Ctrl Pts',(-6.94249523141296,-3.74273779771181,
3.52157354388502));
#86428=CARTESIAN_POINT('Ctrl Pts',(-6.70555066469705,-4.99470829859922,
-1.20932024557051));
#86429=CARTESIAN_POINT('Ctrl Pts',(-6.46860609798114,-1.71736548022594,
-4.84357535835101));
#86430=CARTESIAN_POINT('Ctrl Pts',(-6.23166153126523,3.11732280992082,-4.0855678863374));
#86431=CARTESIAN_POINT('Ctrl Pts',(-5.99471696454932,5.12515297450633,0.377324025464465));
#86432=CARTESIAN_POINT('Ctrl Pts',(-5.75777239783342,2.48537967129977,4.49805005877574));
#86433=CARTESIAN_POINT('Ctrl Pts',(-5.52082783111751,-2.40819157679517,
4.53984359153818));
#86434=CARTESIAN_POINT('Ctrl Pts',(-5.28388326440161,-5.11796076348032,
0.464805291876296));
#86435=CARTESIAN_POINT('Ctrl Pts',(-5.04693869768569,-3.18664857103844,
-4.03172882774475));
#86436=CARTESIAN_POINT('Ctrl Pts',(-4.8099941309698,1.63438796537354,-4.87220102328648));
#86437=CARTESIAN_POINT('Ctrl Pts',(-4.57304956425387,4.97332476795878,-1.29445214310224));
#86438=CARTESIAN_POINT('Ctrl Pts',(-4.33610499753798,3.80233956820685,3.45713473956928));
#86439=CARTESIAN_POINT('Ctrl Pts',(-4.09916043082206,-0.816692775494692,
5.07371478740984));
#86440=CARTESIAN_POINT('Ctrl Pts',(-3.86221586410616,-4.6951288890806,2.08933598101334));
#86441=CARTESIAN_POINT('Ctrl Pts',(-3.62527129739025,-4.31591879559353,
-2.78969816567315));
#86442=CARTESIAN_POINT('Ctrl Pts',(-3.38832673067434,-0.0229334500078643,
-5.13897406752435));
#86443=CARTESIAN_POINT('Ctrl Pts',(-3.15138216395844,4.29084182872829,-2.82810838756633));
#86444=CARTESIAN_POINT('Ctrl Pts',(-2.91443759724252,4.71359840696839,2.04734001631884));
#86445=CARTESIAN_POINT('Ctrl Pts',(-2.67749303052663,0.861933921267414,
5.06623249294253));
#86446=CARTESIAN_POINT('Ctrl Pts',(-2.44054846381071,-3.77130449135365,
3.49091762858201));
#86447=CARTESIAN_POINT('Ctrl Pts',(-2.20360389709481,-4.98472995723955,
-1.2499736380601));
#86448=CARTESIAN_POINT('Ctrl Pts',(-1.9666593303789,-1.67771697248142,-4.85748738223137));
#86449=CARTESIAN_POINT('Ctrl Pts',(-1.729714763663,3.15035354388312,-4.05987962632826));
#86450=CARTESIAN_POINT('Ctrl Pts',(-1.49277019694709,5.12225430095726,0.418850610185909));
#86451=CARTESIAN_POINT('Ctrl Pts',(-1.25582563023118,2.44794756804106,4.51865567952482));
#86452=CARTESIAN_POINT('Ctrl Pts',(-1.01888106351527,-2.44384225364839,
4.51911617817157));
#86453=CARTESIAN_POINT('Ctrl Pts',(-0.781936496799366,-5.12407657510525,
0.424868130349103));
#86454=CARTESIAN_POINT('Ctrl Pts',(-0.544991930083454,-3.14870294440949,
-4.06114495196868));
#86455=CARTESIAN_POINT('Ctrl Pts',(-0.347538124486872,0.861031357136043,
-4.7194698267761));
#86456=CARTESIAN_POINT('Ctrl Pts',(-0.189575080009593,3.34110011276904,
-3.06042877319883));
#86457=CARTESIAN_POINT('Ctrl Pts',(-0.110593557770963,4.04792784467689,
-1.7613235919546));
#86458=CARTESIAN_POINT('Ctrl Pts',(-0.0711027966516446,4.2237088282277,
-1.06264395673989));
#86459=CARTESIAN_POINT('Ctrl Pts',(-24.075,2.36230756092323,-3.31488661006752));
#86460=CARTESIAN_POINT('Ctrl Pts',(-24.0355092388807,2.91065117590484,-2.92411720524959));
#86461=CARTESIAN_POINT('Ctrl Pts',(-23.956527716642,3.8009161537758,-1.86677512529004));
#86462=CARTESIAN_POINT('Ctrl Pts',(-23.7985646721648,4.40104888295471,0.856562345338821));
#86463=CARTESIAN_POINT('Ctrl Pts',(-23.6011108665681,2.46349467463415,4.12278630825743));
#86464=CARTESIAN_POINT('Ctrl Pts',(-23.3641662998523,-2.11355533076443,
4.31564323485309));
#86465=CARTESIAN_POINT('Ctrl Pts',(-23.1272217331364,-4.76528500937787,
0.589368033154422));
#86466=CARTESIAN_POINT('Ctrl Pts',(-22.8902771664205,-3.1002006861113,-3.66850893344406));
#86467=CARTESIAN_POINT('Ctrl Pts',(-22.6533325997046,1.37852450357098,-4.60117581069992));
#86468=CARTESIAN_POINT('Ctrl Pts',(-22.4163880329887,4.60597174073038,-1.36062610156221));
#86469=CARTESIAN_POINT('Ctrl Pts',(-22.1794434662727,3.65724566378385,3.11337055406841));
#86470=CARTESIAN_POINT('Ctrl Pts',(-21.9424988995569,-0.608277930885338,
4.76430086728238));
#86471=CARTESIAN_POINT('Ctrl Pts',(-21.7055543328409,-4.32203219920287,
2.09474833835713));
#86472=CARTESIAN_POINT('Ctrl Pts',(-21.468609766125,-4.11655899594451,-2.47431260611472));
#86473=CARTESIAN_POINT('Ctrl Pts',(-21.2316651994091,-0.178052071836572,
-4.79964076861094));
#86474=CARTESIAN_POINT('Ctrl Pts',(-20.9947206326932,3.92189259497827,-2.77253197087948));
#86475=CARTESIAN_POINT('Ctrl Pts',(-20.7577760659773,4.46538966209699,1.76876296315944));
#86476=CARTESIAN_POINT('Ctrl Pts',(-20.5208314992614,0.959564937147886,
4.70610816747424));
#86477=CARTESIAN_POINT('Ctrl Pts',(-20.2838869325455,-3.41641139423198,
3.37584696374503));
#86478=CARTESIAN_POINT('Ctrl Pts',(-20.0469423658296,-4.69431112832445,
-1.01570673574804));
#86479=CARTESIAN_POINT('Ctrl Pts',(-19.8099977991137,-1.71530351140438,
-4.48619540698215));
#86480=CARTESIAN_POINT('Ctrl Pts',(-19.5730532323978,2.8191792622351,-3.88850133137423));
#86481=CARTESIAN_POINT('Ctrl Pts',(-19.3361086656818,4.79716740439492,0.23537265996686));
#86482=CARTESIAN_POINT('Ctrl Pts',(-19.099164098966,2.42497660407891,4.14580553515268));
#86483=CARTESIAN_POINT('Ctrl Pts',(-18.86221953225,-2.14623721078936,4.29672908104936));
#86484=CARTESIAN_POINT('Ctrl Pts',(-18.6252749655341,-4.77119510204201,
0.551282511887758));
#86485=CARTESIAN_POINT('Ctrl Pts',(-18.3883303988183,-3.06952642646402,
-3.69407939419781));
#86486=CARTESIAN_POINT('Ctrl Pts',(-18.1513858321023,1.41565753192185,-4.58956738674043));
#86487=CARTESIAN_POINT('Ctrl Pts',(-17.9144412653864,4.61709154776294,-1.32313291269056));
#86488=CARTESIAN_POINT('Ctrl Pts',(-17.6774966986705,3.63164356582701,3.14314811403285));
#86489=CARTESIAN_POINT('Ctrl Pts',(-17.4405521319546,-0.647060115157983,
4.75915205295132));
#86490=CARTESIAN_POINT('Ctrl Pts',(-17.2036075652387,-4.33899519630793,
2.05945035015389));
#86491=CARTESIAN_POINT('Ctrl Pts',(-16.9666629985228,-4.09623228013284,
-2.50780704283935));
#86492=CARTESIAN_POINT('Ctrl Pts',(-16.7297184318069,-0.138914215188535,
-4.80092885781891));
#86493=CARTESIAN_POINT('Ctrl Pts',(-16.492773865091,3.94437437056674,-2.74046088863915));
#86494=CARTESIAN_POINT('Ctrl Pts',(-16.2558292983751,4.45081595990773,1.8051183751108));
#86495=CARTESIAN_POINT('Ctrl Pts',(-16.0188847316592,0.921157980137197,
4.71377587850701));
#86496=CARTESIAN_POINT('Ctrl Pts',(-15.7819401649433,-3.44382668136788,
3.34787587074291));
#86497=CARTESIAN_POINT('Ctrl Pts',(-15.5449955982273,-4.68587219865936,
-1.05395293775576));
#86498=CARTESIAN_POINT('Ctrl Pts',(-15.3080510315115,-1.6786638864531,-4.50003362359639));
#86499=CARTESIAN_POINT('Ctrl Pts',(-15.0711064647955,2.85079442437809,-3.86538306085168));
#86500=CARTESIAN_POINT('Ctrl Pts',(-14.8341618980796,4.79508852002207,0.274483409940331));
#86501=CARTESIAN_POINT('Ctrl Pts',(-14.5972173313637,2.39108898052815,4.16544217873422));
#86502=CARTESIAN_POINT('Ctrl Pts',(-14.3602727646478,-2.18120358456222,
4.27908471286496));
#86503=CARTESIAN_POINT('Ctrl Pts',(-14.1233281979319,-4.77553190059009,
0.512357417851518));
#86504=CARTESIAN_POINT('Ctrl Pts',(-13.886383631216,-3.0393009618661,-3.71898705568882));
#86505=CARTESIAN_POINT('Ctrl Pts',(-13.6494390645001,1.45303614102348,-4.57787079656698));
#86506=CARTESIAN_POINT('Ctrl Pts',(-13.4124944977842,4.6277275367991,-1.28543879758337));
#86507=CARTESIAN_POINT('Ctrl Pts',(-13.1755499310683,3.6058919843453,3.17265788486808));
#86508=CARTESIAN_POINT('Ctrl Pts',(-12.9386053643524,-0.68584715780348,
4.75371735942664));
#86509=CARTESIAN_POINT('Ctrl Pts',(-12.7016607976364,-4.35564474068758,
2.02399949360218));
#86510=CARTESIAN_POINT('Ctrl Pts',(-12.4647162309206,-4.07564614696872,
-2.54112643169917));
#86511=CARTESIAN_POINT('Ctrl Pts',(-12.2277716642046,-0.0997603707836814,
-4.80190201124536));
#86512=CARTESIAN_POINT('Ctrl Pts',(-11.9908270974887,3.96659034332826,-2.70820532925335));
#86513=CARTESIAN_POINT('Ctrl Pts',(-11.7538825307728,4.43594811954626,1.84135258380226));
#86514=CARTESIAN_POINT('Ctrl Pts',(-11.5169379640569,0.882688817166835,
4.72113074477184));
#86515=CARTESIAN_POINT('Ctrl Pts',(-11.279993397341,-3.47101246860204,3.31968183716308));
#86516=CARTESIAN_POINT('Ctrl Pts',(-11.0430488306251,-4.67712192959289,
-1.09212889024254));
#86517=CARTESIAN_POINT('Ctrl Pts',(-10.8061042639092,-1.64191250099602,
-4.51357268649284));
#86518=CARTESIAN_POINT('Ctrl Pts',(-10.5691596971933,2.88221994700369,-3.84200770877353));
#86519=CARTESIAN_POINT('Ctrl Pts',(-10.3322151304774,4.79269081226222,0.313575884338453));
#86520=CARTESIAN_POINT('Ctrl Pts',(-10.0952705637615,2.35704233746519,4.18480184436228));
#86521=CARTESIAN_POINT('Ctrl Pts',(-9.85832599704557,-2.21602490467178,
4.26115579145559));
#86522=CARTESIAN_POINT('Ctrl Pts',(-9.62138143032966,-4.77955114499888,
0.473398256779212));
#86523=CARTESIAN_POINT('Ctrl Pts',(-9.38443686361375,-3.00887338975049,
-3.74364741684263));
#86524=CARTESIAN_POINT('Ctrl Pts',(-9.14749229689786,1.49031812597541,-4.56586979014612));
#86525=CARTESIAN_POINT('Ctrl Pts',(-8.91054773018194,4.63805579586533,-1.24765920492107));
#86526=CARTESIAN_POINT('Ctrl Pts',(-8.67360316346604,3.57990062094709,3.20195668323646));
#86527=CARTESIAN_POINT('Ctrl Pts',(-8.43665859675013,-0.724588593371072,
4.74796655711994));
#86528=CARTESIAN_POINT('Ctrl Pts',(-8.19971403003422,-4.37200464720922,
1.98841404691898));
#86529=CARTESIAN_POINT('Ctrl Pts',(-7.96276946331832,-4.05478899489471,
-2.57427684293));
#86530=CARTESIAN_POINT('Ctrl Pts',(-7.7258248966024,-0.0605998926332336,
-4.80255585185065));
#86531=CARTESIAN_POINT('Ctrl Pts',(-7.48888032988651,3.98854254916481,-2.67576968195071));
#86532=CARTESIAN_POINT('Ctrl Pts',(-7.25193576317058,4.42078530124335,1.87746434781877));
#86533=CARTESIAN_POINT('Ctrl Pts',(-7.01499119645469,0.844160957960478,
4.72817166925782));
#86534=CARTESIAN_POINT('Ctrl Pts',(-6.77804662973878,-3.49796744349901,
3.29126705427458));
#86535=CARTESIAN_POINT('Ctrl Pts',(-6.54110206302287,-4.66806064505926,
-1.13023221940798));
#86536=CARTESIAN_POINT('Ctrl Pts',(-6.30415749630696,-1.60505193339804,
-4.52681160940636));
#86537=CARTESIAN_POINT('Ctrl Pts',(-6.06721292959105,2.91345381090988,-3.81837687463714));
#86538=CARTESIAN_POINT('Ctrl Pts',(-5.83026836287515,4.78997440289178,0.352647507803434));
#86539=CARTESIAN_POINT('Ctrl Pts',(-5.59332379615923,2.322838960361,4.20388323073168));
#86540=CARTESIAN_POINT('Ctrl Pts',(-5.35637922944334,-2.25069887035317,
4.24294351890926));
#86541=CARTESIAN_POINT('Ctrl Pts',(-5.11943466272741,-4.78325255343947,
0.434407609195393));
#86542=CARTESIAN_POINT('Ctrl Pts',(-4.88249009601153,-2.9782457542657,-3.76805882289953));
#86543=CARTESIAN_POINT('Ctrl Pts',(-4.6455455292956,1.52750104386647,-4.55356519178499));
#86544=CARTESIAN_POINT('Ctrl Pts',(-4.40860096257971,4.64807557048283,-1.20979659769575));
#86545=CARTESIAN_POINT('Ctrl Pts',(-4.17165639586379,3.55367133301375,3.23104246687973));
#86546=CARTESIAN_POINT('Ctrl Pts',(-3.93471182914789,-0.763282093062437,
4.74190020866793));
#86547=CARTESIAN_POINT('Ctrl Pts',(-3.69776726243198,-4.38807335290126,
1.9526960303187));
#86548=CARTESIAN_POINT('Ctrl Pts',(-3.46082269571607,-4.03366312355658,
-2.60725540717266));
#86549=CARTESIAN_POINT('Ctrl Pts',(-3.22387812900017,-0.021433631162604,
-4.80289161377419));
#86550=CARTESIAN_POINT('Ctrl Pts',(-2.98693356228425,4.01022615884859,-2.64315364876519));
#86551=CARTESIAN_POINT('Ctrl Pts',(-2.74998899556836,4.40533498750148,1.91344654900335));
#86552=CARTESIAN_POINT('Ctrl Pts',(-2.51304442885244,0.805564524686711,
4.73490724686727));
#86553=CARTESIAN_POINT('Ctrl Pts',(-2.27609986213654,-3.52466591123261,
3.26261599735412));
#86554=CARTESIAN_POINT('Ctrl Pts',(-2.03915529542063,-4.65873487470004,
-1.16822693105551));
#86555=CARTESIAN_POINT('Ctrl Pts',(-1.80221072870472,-1.56799638829454,
-4.53981380438684));
#86556=CARTESIAN_POINT('Ctrl Pts',(-1.56526616198882,2.94432437633009,-3.79436859458956));
#86557=CARTESIAN_POINT('Ctrl Pts',(-1.32832159527291,4.78726529895451,0.391458306006858));
#86558=CARTESIAN_POINT('Ctrl Pts',(-1.091377028557,2.2878548696719,4.22314126974725));
#86559=CARTESIAN_POINT('Ctrl Pts',(-0.854432461841093,-2.28401803768771,
4.22357165236047));
#86560=CARTESIAN_POINT('Ctrl Pts',(-0.617487895125189,-4.78896839866047,
0.397082287904312));
#86561=CARTESIAN_POINT('Ctrl Pts',(-0.380543328409276,-2.94278172399022,
-3.79555116952135));
#86562=CARTESIAN_POINT('Ctrl Pts',(-0.183089522812695,0.804720987116727,
-4.41082242382338));
#86563=CARTESIAN_POINT('Ctrl Pts',(-0.0251264783354149,3.1225963590295,
-2.860280572778));
#86564=CARTESIAN_POINT('Ctrl Pts',(0.0538550439032153,3.78319844445675,
-1.64613523979437));
#86565=CARTESIAN_POINT('Ctrl Pts',(0.0933458050225333,3.94748357231767,
-0.993148375763724));
#86566=CARTESIAN_POINT('Ctrl Pts',(-0.400000000000003,4.77615934004775,
-1.20163511869228));
#86567=CARTESIAN_POINT('Ctrl Pts',(-0.439490761119319,4.57738664511713,
-1.99170029627507));
#86568=CARTESIAN_POINT('Ctrl Pts',(-0.478981522238631,4.17774713268266,
-2.72621273515775));
#86569=CARTESIAN_POINT('Ctrl Pts',(-0.518472283357947,3.62737043608126,
-3.32797388692922));
#86570=CARTESIAN_POINT('Ctrl Pts',(-0.557963044477266,3.07699373947981,
-3.92973503870074));
#86571=CARTESIAN_POINT('Ctrl Pts',(-0.597453805596586,2.37587985871143,
-4.39874490336101));
#86572=CARTESIAN_POINT('Ctrl Pts',(-0.636944566715907,1.60619077270431,
-4.66178933874665));
#86573=CARTESIAN_POINT('Ctrl Pts',(-0.715926088954544,0.0668126006901387,
-5.1878782095179));
#86574=CARTESIAN_POINT('Ctrl Pts',(-0.794907611193176,-1.74686639227891,
-4.89010536319065));
#86575=CARTESIAN_POINT('Ctrl Pts',(-0.873889133431811,-3.02599714588792,
-3.89575688467669));
#86576=CARTESIAN_POINT('Ctrl Pts',(-0.946312246986672,-4.19891239485264,
-2.98397637283827));
#86577=CARTESIAN_POINT('Ctrl Pts',(-1.01873536054154,-4.92236843052219,
-1.48650066533691));
#86578=CARTESIAN_POINT('Ctrl Pts',(-1.0911584740964,-4.93200687334489,0.00268308223936954));
#86579=CARTESIAN_POINT('Origin',(-0.4,0.,0.));
#86580=CARTESIAN_POINT('',(0.,-6.52124420545966E-16,5.325));
#86581=CARTESIAN_POINT('Origin',(-0.4,-6.52124420545966E-16,5.325));
#86582=CARTESIAN_POINT('Origin',(0.,0.,0.));
#86583=CARTESIAN_POINT('Origin',(-0.4,0.,0.));
#86584=CARTESIAN_POINT('Origin',(-12.,0.,0.));
#86585=CARTESIAN_POINT('Origin',(0.,8.,0.));
#86586=CARTESIAN_POINT('',(0.,-8.,-9.79717439317883E-16));
#86587=CARTESIAN_POINT('Origin',(0.,0.,0.));
#86588=CARTESIAN_POINT('Origin',(0.3,7.53377931054339,-1.32840855915202));
#86589=CARTESIAN_POINT('',(0.3,7.84576201581982,-1.56333566169231));
#86590=CARTESIAN_POINT('',(9.,7.84576201581982,-1.56333566169231));
#86591=CARTESIAN_POINT('',(4.5,7.84576201581982,-1.56333566169231));
#86592=CARTESIAN_POINT('',(0.3,7.53377931054339,-1.32840855915202));
#86593=CARTESIAN_POINT('',(0.3,8.02680208495337,-1.69966122771225));
#86594=CARTESIAN_POINT('',(9.,7.53377931054339,-1.32840855915202));
#86595=CARTESIAN_POINT('',(0.3,7.53377931054339,-1.32840855915202));
#86596=CARTESIAN_POINT('',(9.,8.02680208495337,-1.69966122771225));
#86597=CARTESIAN_POINT('Origin',(9.,7.80460144262175,-1.37616180801042));
#86598=CARTESIAN_POINT('',(9.,7.90729695778639,-1.21435366404606));
#86599=CARTESIAN_POINT('Origin',(9.,0.,0.));
#86600=CARTESIAN_POINT('',(9.,7.53377931054339,-1.32840855915202));
#86601=CARTESIAN_POINT('Origin',(0.3,8.12404506444685,-1.14816888602541));
#86602=CARTESIAN_POINT('',(0.3,7.90729695778639,-1.21435366404606));
#86603=CARTESIAN_POINT('',(4.5,7.90729695778639,-1.21435366404606));
#86604=CARTESIAN_POINT('',(0.3,7.53377931054339,-1.32840855915202));
#86605=CARTESIAN_POINT('Origin',(0.3,7.80460144262175,-1.37616180801042));
#86606=CARTESIAN_POINT('Origin',(0.3,0.,0.));
#86607=CARTESIAN_POINT('Origin',(0.3,7.1886485490122,-2.61645409644137));
#86608=CARTESIAN_POINT('',(0.3,7.45509687273345,-2.9019873566506));
#86609=CARTESIAN_POINT('',(9.,7.45509687273345,-2.9019873566506));
#86610=CARTESIAN_POINT('',(4.5,7.45509687273345,-2.9019873566506));
#86611=CARTESIAN_POINT('',(0.3,7.1886485490122,-2.61645409644137));
#86612=CARTESIAN_POINT('',(0.3,7.60971385031326,-3.06767910909054));
#86613=CARTESIAN_POINT('',(9.,7.1886485490122,-2.61645409644137));
#86614=CARTESIAN_POINT('',(0.3,7.1886485490122,-2.61645409644137));
#86615=CARTESIAN_POINT('',(9.,7.60971385031326,-3.06767910909054));
#86616=CARTESIAN_POINT('Origin',(9.,7.44706401972832,-2.71050963585593));
#86617=CARTESIAN_POINT('',(9.,7.57629704859312,-2.56899261024222));
#86618=CARTESIAN_POINT('Origin',(9.,0.,0.));
#86619=CARTESIAN_POINT('',(9.,7.1886485490122,-2.61645409644137));
#86620=CARTESIAN_POINT('Origin',(0.3,7.80124513057563,-2.54145124145043));
#86621=CARTESIAN_POINT('',(0.3,7.57629704859312,-2.56899261024222));
#86622=CARTESIAN_POINT('',(4.5,7.57629704859312,-2.56899261024222));
#86623=CARTESIAN_POINT('',(0.3,7.1886485490122,-2.61645409644137));
#86624=CARTESIAN_POINT('Origin',(0.3,7.44706401972832,-2.71050963585593));
#86625=CARTESIAN_POINT('Origin',(0.3,0.,0.));
#86626=CARTESIAN_POINT('Origin',(0.3,6.62509433895095,-3.825));
#86627=CARTESIAN_POINT('',(0.3,6.83791238363012,-4.15246363425351));
#86628=CARTESIAN_POINT('',(9.,6.83791238363012,-4.15246363425351));
#86629=CARTESIAN_POINT('',(4.5,6.83791238363012,-4.15246363425351));
#86630=CARTESIAN_POINT('',(0.3,6.62509433895095,-3.825));
#86631=CARTESIAN_POINT('',(0.3,6.96140831103239,-4.34248711305965));
#86632=CARTESIAN_POINT('',(9.,6.62509433895095,-3.825));
#86633=CARTESIAN_POINT('',(0.3,6.62509433895095,-3.825));
#86634=CARTESIAN_POINT('',(9.,6.96140831103239,-4.34248711305965));
#86635=CARTESIAN_POINT('Origin',(9.,6.86325132499167,-3.9625));
#86636=CARTESIAN_POINT('',(9.,7.01509518736965,-3.84557401594914));
#86637=CARTESIAN_POINT('Origin',(9.,0.,0.));
#86638=CARTESIAN_POINT('',(9.,6.62509433895095,-3.825));
#86639=CARTESIAN_POINT('Origin',(0.3,7.24140831103239,-3.85751288694036));
#86640=CARTESIAN_POINT('',(0.3,7.01509518736965,-3.84557401594914));
#86641=CARTESIAN_POINT('',(4.5,7.01509518736965,-3.84557401594914));
#86642=CARTESIAN_POINT('',(0.3,6.62509433895095,-3.825));
#86643=CARTESIAN_POINT('Origin',(0.3,6.86325132499167,-3.9625));
#86644=CARTESIAN_POINT('Origin',(0.3,0.,0.));
#86645=CARTESIAN_POINT('Origin',(0.3,5.86023998986018,-4.91732521410203));
#86646=CARTESIAN_POINT('',(0.3,6.01296138690081,-5.27676940557761));
#86647=CARTESIAN_POINT('',(9.,6.01296138690081,-5.27676940557761));
#86648=CARTESIAN_POINT('',(4.5,6.01296138690081,-5.27676940557761));
#86649=CARTESIAN_POINT('',(0.3,5.86023998986018,-4.91732521410203));
#86650=CARTESIAN_POINT('',(0.3,6.10158390286339,-5.48535084350294));
#86651=CARTESIAN_POINT('',(9.,5.86023998986018,-4.91732521410203));
#86652=CARTESIAN_POINT('',(0.3,5.86023998986018,-4.91732521410203));
#86653=CARTESIAN_POINT('',(9.,6.10158390286339,-5.48535084350294));
#86654=CARTESIAN_POINT('Origin',(9.,6.0709022117179,-5.09409180676583));
#86655=CARTESIAN_POINT('',(9.,6.24074320868739,-5.0053096011358));
#86656=CARTESIAN_POINT('Origin',(9.,0.,0.));
#86657=CARTESIAN_POINT('',(9.,5.86023998986018,-4.91732521410203));
#86658=CARTESIAN_POINT('Origin',(0.3,6.46154496428785,-5.05636595535631));
#86659=CARTESIAN_POINT('',(0.3,6.24074320868739,-5.0053096011358));
#86660=CARTESIAN_POINT('',(4.5,6.24074320868739,-5.0053096011358));
#86661=CARTESIAN_POINT('',(0.3,5.86023998986018,-4.91732521410203));
#86662=CARTESIAN_POINT('Origin',(0.3,6.0709022117179,-5.09409180676583));
#86663=CARTESIAN_POINT('Origin',(0.3,0.,0.));
#86664=CARTESIAN_POINT('Origin',(0.3,4.91732521410202,-5.86023998986018));
#86665=CARTESIAN_POINT('',(0.3,5.0053096011358,-6.24074320868739));
#86666=CARTESIAN_POINT('',(9.,5.0053096011358,-6.24074320868739));
#86667=CARTESIAN_POINT('',(4.5,5.0053096011358,-6.24074320868739));
#86668=CARTESIAN_POINT('',(0.3,4.91732521410202,-5.86023998986018));
#86669=CARTESIAN_POINT('',(0.3,5.05636595535631,-6.46154496428785));
#86670=CARTESIAN_POINT('',(9.,4.91732521410202,-5.86023998986018));
#86671=CARTESIAN_POINT('',(0.3,4.91732521410202,-5.86023998986018));
#86672=CARTESIAN_POINT('',(9.,5.05636595535631,-6.46154496428785));
#86673=CARTESIAN_POINT('Origin',(9.,5.09409180676582,-6.0709022117179));
#86674=CARTESIAN_POINT('',(9.,5.27676940557761,-6.01296138690081));
#86675=CARTESIAN_POINT('Origin',(9.,0.,0.));
#86676=CARTESIAN_POINT('',(9.,4.91732521410202,-5.86023998986018));
#86677=CARTESIAN_POINT('Origin',(0.3,5.48535084350294,-6.10158390286339));
#86678=CARTESIAN_POINT('',(0.3,5.27676940557761,-6.01296138690081));
#86679=CARTESIAN_POINT('',(4.5,5.27676940557761,-6.01296138690081));
#86680=CARTESIAN_POINT('',(0.3,4.91732521410202,-5.86023998986018));
#86681=CARTESIAN_POINT('Origin',(0.3,5.09409180676582,-6.0709022117179));
#86682=CARTESIAN_POINT('Origin',(0.3,0.,0.));
#86683=CARTESIAN_POINT('Origin',(0.3,3.825,-6.62509433895096));
#86684=CARTESIAN_POINT('',(0.3,3.84557401594914,-7.01509518736965));
#86685=CARTESIAN_POINT('',(9.,3.84557401594914,-7.01509518736965));
#86686=CARTESIAN_POINT('',(4.5,3.84557401594914,-7.01509518736965));
#86687=CARTESIAN_POINT('',(0.3,3.825,-6.62509433895096));
#86688=CARTESIAN_POINT('',(0.3,3.85751288694036,-7.2414083110324));
#86689=CARTESIAN_POINT('',(9.,3.825,-6.62509433895096));
#86690=CARTESIAN_POINT('',(0.3,3.825,-6.62509433895096));
#86691=CARTESIAN_POINT('',(9.,3.85751288694036,-7.2414083110324));
#86692=CARTESIAN_POINT('Origin',(9.,3.9625,-6.86325132499168));
#86693=CARTESIAN_POINT('',(9.,4.15246363425351,-6.83791238363012));
#86694=CARTESIAN_POINT('Origin',(9.,0.,0.));
#86695=CARTESIAN_POINT('',(9.,3.825,-6.62509433895096));
#86696=CARTESIAN_POINT('Origin',(0.3,4.34248711305964,-6.96140831103239));
#86697=CARTESIAN_POINT('',(0.3,4.15246363425351,-6.83791238363012));
#86698=CARTESIAN_POINT('',(4.5,4.15246363425351,-6.83791238363012));
#86699=CARTESIAN_POINT('',(0.3,3.825,-6.62509433895096));
#86700=CARTESIAN_POINT('Origin',(0.3,3.9625,-6.86325132499168));
#86701=CARTESIAN_POINT('Origin',(0.3,0.,0.));
#86702=CARTESIAN_POINT('Origin',(0.3,2.61645409644136,-7.1886485490122));
#86703=CARTESIAN_POINT('',(0.3,2.56899261024221,-7.57629704859313));
#86704=CARTESIAN_POINT('',(9.,2.56899261024221,-7.57629704859313));
#86705=CARTESIAN_POINT('',(4.5,2.56899261024221,-7.57629704859313));
#86706=CARTESIAN_POINT('',(0.3,2.61645409644136,-7.1886485490122));
#86707=CARTESIAN_POINT('',(0.3,2.54145124145042,-7.80124513057564));
#86708=CARTESIAN_POINT('',(9.,2.61645409644136,-7.1886485490122));
#86709=CARTESIAN_POINT('',(0.3,2.61645409644136,-7.1886485490122));
#86710=CARTESIAN_POINT('',(9.,2.54145124145042,-7.80124513057564));
#86711=CARTESIAN_POINT('Origin',(9.,2.71050963585592,-7.44706401972833));
#86712=CARTESIAN_POINT('',(9.,2.90198735665059,-7.45509687273345));
#86713=CARTESIAN_POINT('Origin',(9.,0.,0.));
#86714=CARTESIAN_POINT('',(9.,2.61645409644136,-7.1886485490122));
#86715=CARTESIAN_POINT('Origin',(0.3,3.06767910909053,-7.60971385031326));
#86716=CARTESIAN_POINT('',(0.3,2.90198735665059,-7.45509687273345));
#86717=CARTESIAN_POINT('',(4.5,2.90198735665059,-7.45509687273345));
#86718=CARTESIAN_POINT('',(0.3,2.61645409644136,-7.1886485490122));
#86719=CARTESIAN_POINT('Origin',(0.3,2.71050963585592,-7.44706401972833));
#86720=CARTESIAN_POINT('Origin',(0.3,0.,0.));
#86721=CARTESIAN_POINT('Origin',(0.3,1.32840855915201,-7.53377931054339));
#86722=CARTESIAN_POINT('',(0.3,1.21435366404606,-7.90729695778639));
#86723=CARTESIAN_POINT('',(9.,1.21435366404606,-7.90729695778639));
#86724=CARTESIAN_POINT('',(4.5,1.21435366404606,-7.90729695778639));
#86725=CARTESIAN_POINT('',(0.3,1.32840855915201,-7.53377931054339));
#86726=CARTESIAN_POINT('',(0.3,1.14816888602541,-8.12404506444685));
#86727=CARTESIAN_POINT('',(9.,1.32840855915201,-7.53377931054339));
#86728=CARTESIAN_POINT('',(0.3,1.32840855915201,-7.53377931054339));
#86729=CARTESIAN_POINT('',(9.,1.14816888602541,-8.12404506444685));
#86730=CARTESIAN_POINT('Origin',(9.,1.37616180801042,-7.80460144262175));
#86731=CARTESIAN_POINT('',(9.,1.56333566169231,-7.84576201581982));
#86732=CARTESIAN_POINT('Origin',(9.,0.,0.));
#86733=CARTESIAN_POINT('',(9.,1.32840855915201,-7.53377931054339));
#86734=CARTESIAN_POINT('Origin',(0.3,1.69966122771224,-8.02680208495337));
#86735=CARTESIAN_POINT('',(0.3,1.56333566169231,-7.84576201581982));
#86736=CARTESIAN_POINT('',(4.5,1.56333566169231,-7.84576201581982));
#86737=CARTESIAN_POINT('',(0.3,1.32840855915201,-7.53377931054339));
#86738=CARTESIAN_POINT('Origin',(0.3,1.37616180801042,-7.80460144262175));
#86739=CARTESIAN_POINT('Origin',(0.3,0.,0.));
#86740=CARTESIAN_POINT('Origin',(0.3,-1.40528220202159E-15,-7.65));
#86741=CARTESIAN_POINT('',(0.3,-0.177182803739528,-7.99803765020264));
#86742=CARTESIAN_POINT('',(9.,-0.177182803739528,-7.99803765020264));
#86743=CARTESIAN_POINT('',(4.5,-0.177182803739529,-7.99803765020264));
#86744=CARTESIAN_POINT('',(0.3,-1.40528220202159E-15,-7.65));
#86745=CARTESIAN_POINT('',(0.3,-0.280000000000001,-8.2));
#86746=CARTESIAN_POINT('',(9.,-1.40528220202159E-15,-7.65));
#86747=CARTESIAN_POINT('',(0.3,-1.40528220202159E-15,-7.65));
#86748=CARTESIAN_POINT('',(9.,-0.280000000000001,-8.2));
#86749=CARTESIAN_POINT('Origin',(9.,-1.45579888248642E-15,-7.925));
#86750=CARTESIAN_POINT('',(9.,0.177182803739525,-7.99803765020264));
#86751=CARTESIAN_POINT('Origin',(9.,0.,0.));
#86752=CARTESIAN_POINT('',(9.,-1.40528220202159E-15,-7.65));
#86753=CARTESIAN_POINT('Origin',(0.3,0.279999999999998,-8.2));
#86754=CARTESIAN_POINT('',(0.3,0.177182803739525,-7.99803765020264));
#86755=CARTESIAN_POINT('',(4.5,0.177182803739526,-7.99803765020264));
#86756=CARTESIAN_POINT('',(0.3,-1.40528220202159E-15,-7.65));
#86757=CARTESIAN_POINT('Origin',(0.3,-1.45579888248642E-15,-7.925));
#86758=CARTESIAN_POINT('Origin',(0.3,0.,0.));
#86759=CARTESIAN_POINT('Origin',(0.3,-1.32840855915202,-7.53377931054339));
#86760=CARTESIAN_POINT('',(0.3,-1.56333566169232,-7.84576201581982));
#86761=CARTESIAN_POINT('',(9.,-1.56333566169232,-7.84576201581982));
#86762=CARTESIAN_POINT('',(4.5,-1.56333566169231,-7.84576201581982));
#86763=CARTESIAN_POINT('',(0.3,-1.32840855915202,-7.53377931054339));
#86764=CARTESIAN_POINT('',(0.3,-1.69966122771225,-8.02680208495337));
#86765=CARTESIAN_POINT('',(9.,-1.32840855915202,-7.53377931054339));
#86766=CARTESIAN_POINT('',(0.3,-1.32840855915202,-7.53377931054339));
#86767=CARTESIAN_POINT('',(9.,-1.69966122771225,-8.02680208495337));
#86768=CARTESIAN_POINT('Origin',(9.,-1.37616180801042,-7.80460144262175));
#86769=CARTESIAN_POINT('',(9.,-1.21435366404606,-7.90729695778639));
#86770=CARTESIAN_POINT('Origin',(9.,0.,0.));
#86771=CARTESIAN_POINT('',(9.,-1.32840855915202,-7.53377931054339));
#86772=CARTESIAN_POINT('Origin',(0.3,-1.14816888602541,-8.12404506444685));
#86773=CARTESIAN_POINT('',(0.3,-1.21435366404606,-7.90729695778639));
#86774=CARTESIAN_POINT('',(4.5,-1.21435366404606,-7.90729695778639));
#86775=CARTESIAN_POINT('',(0.3,-1.32840855915202,-7.53377931054339));
#86776=CARTESIAN_POINT('Origin',(0.3,-1.37616180801042,-7.80460144262175));
#86777=CARTESIAN_POINT('Origin',(0.3,0.,0.));
#86778=CARTESIAN_POINT('Origin',(0.3,-2.61645409644137,-7.1886485490122));
#86779=CARTESIAN_POINT('',(0.3,-2.9019873566506,-7.45509687273345));
#86780=CARTESIAN_POINT('',(9.,-2.9019873566506,-7.45509687273345));
#86781=CARTESIAN_POINT('',(4.5,-2.9019873566506,-7.45509687273345));
#86782=CARTESIAN_POINT('',(0.3,-2.61645409644137,-7.1886485490122));
#86783=CARTESIAN_POINT('',(0.3,-3.06767910909054,-7.60971385031326));
#86784=CARTESIAN_POINT('',(9.,-2.61645409644137,-7.1886485490122));
#86785=CARTESIAN_POINT('',(0.3,-2.61645409644137,-7.1886485490122));
#86786=CARTESIAN_POINT('',(9.,-3.06767910909054,-7.60971385031326));
#86787=CARTESIAN_POINT('Origin',(9.,-2.71050963585593,-7.44706401972832));
#86788=CARTESIAN_POINT('',(9.,-2.56899261024222,-7.57629704859313));
#86789=CARTESIAN_POINT('Origin',(9.,0.,0.));
#86790=CARTESIAN_POINT('',(9.,-2.61645409644137,-7.1886485490122));
#86791=CARTESIAN_POINT('Origin',(0.3,-2.54145124145043,-7.80124513057563));
#86792=CARTESIAN_POINT('',(0.3,-2.56899261024222,-7.57629704859313));
#86793=CARTESIAN_POINT('',(4.5,-2.56899261024222,-7.57629704859312));
#86794=CARTESIAN_POINT('',(0.3,-2.61645409644137,-7.1886485490122));
#86795=CARTESIAN_POINT('Origin',(0.3,-2.71050963585593,-7.44706401972832));
#86796=CARTESIAN_POINT('Origin',(0.3,0.,0.));
#86797=CARTESIAN_POINT('Origin',(0.3,-3.825,-6.62509433895095));
#86798=CARTESIAN_POINT('',(0.3,-4.15246363425351,-6.83791238363012));
#86799=CARTESIAN_POINT('',(9.,-4.15246363425351,-6.83791238363012));
#86800=CARTESIAN_POINT('',(4.5,-4.15246363425351,-6.83791238363012));
#86801=CARTESIAN_POINT('',(0.3,-3.825,-6.62509433895095));
#86802=CARTESIAN_POINT('',(0.3,-4.34248711305965,-6.96140831103239));
#86803=CARTESIAN_POINT('',(9.,-3.825,-6.62509433895095));
#86804=CARTESIAN_POINT('',(0.3,-3.825,-6.62509433895095));
#86805=CARTESIAN_POINT('',(9.,-4.34248711305965,-6.96140831103239));
#86806=CARTESIAN_POINT('Origin',(9.,-3.9625,-6.86325132499167));
#86807=CARTESIAN_POINT('',(9.,-3.84557401594914,-7.01509518736965));
#86808=CARTESIAN_POINT('Origin',(9.,0.,0.));
#86809=CARTESIAN_POINT('',(9.,-3.825,-6.62509433895095));
#86810=CARTESIAN_POINT('Origin',(0.3,-3.85751288694036,-7.24140831103239));
#86811=CARTESIAN_POINT('',(0.3,-3.84557401594914,-7.01509518736965));
#86812=CARTESIAN_POINT('',(4.5,-3.84557401594914,-7.01509518736965));
#86813=CARTESIAN_POINT('',(0.3,-3.825,-6.62509433895095));
#86814=CARTESIAN_POINT('Origin',(0.3,-3.9625,-6.86325132499167));
#86815=CARTESIAN_POINT('Origin',(0.3,0.,0.));
#86816=CARTESIAN_POINT('Origin',(0.3,-4.91732521410203,-5.86023998986018));
#86817=CARTESIAN_POINT('',(0.3,-5.27676940557761,-6.01296138690081));
#86818=CARTESIAN_POINT('',(9.,-5.27676940557761,-6.01296138690081));
#86819=CARTESIAN_POINT('',(4.5,-5.27676940557761,-6.01296138690081));
#86820=CARTESIAN_POINT('',(0.3,-4.91732521410203,-5.86023998986018));
#86821=CARTESIAN_POINT('',(0.3,-5.48535084350294,-6.10158390286339));
#86822=CARTESIAN_POINT('',(9.,-4.91732521410203,-5.86023998986018));
#86823=CARTESIAN_POINT('',(0.3,-4.91732521410203,-5.86023998986018));
#86824=CARTESIAN_POINT('',(9.,-5.48535084350294,-6.10158390286339));
#86825=CARTESIAN_POINT('Origin',(9.,-5.09409180676582,-6.0709022117179));
#86826=CARTESIAN_POINT('',(9.,-5.0053096011358,-6.24074320868739));
#86827=CARTESIAN_POINT('Origin',(9.,0.,0.));
#86828=CARTESIAN_POINT('',(9.,-4.91732521410203,-5.86023998986018));
#86829=CARTESIAN_POINT('Origin',(0.3,-5.05636595535631,-6.46154496428785));
#86830=CARTESIAN_POINT('',(0.3,-5.0053096011358,-6.24074320868739));
#86831=CARTESIAN_POINT('',(4.5,-5.0053096011358,-6.24074320868739));
#86832=CARTESIAN_POINT('',(0.3,-4.91732521410203,-5.86023998986018));
#86833=CARTESIAN_POINT('Origin',(0.3,-5.09409180676582,-6.0709022117179));
#86834=CARTESIAN_POINT('Origin',(0.3,0.,0.));
#86835=CARTESIAN_POINT('Origin',(0.3,-5.86023998986018,-4.91732521410203));
#86836=CARTESIAN_POINT('',(0.3,-6.24074320868739,-5.0053096011358));
#86837=CARTESIAN_POINT('',(9.,-6.24074320868739,-5.0053096011358));
#86838=CARTESIAN_POINT('',(4.5,-6.24074320868739,-5.0053096011358));
#86839=CARTESIAN_POINT('',(0.3,-5.86023998986018,-4.91732521410203));
#86840=CARTESIAN_POINT('',(0.3,-6.46154496428785,-5.05636595535631));
#86841=CARTESIAN_POINT('',(9.,-5.86023998986018,-4.91732521410203));
#86842=CARTESIAN_POINT('',(0.3,-5.86023998986018,-4.91732521410203));
#86843=CARTESIAN_POINT('',(9.,-6.46154496428785,-5.05636595535631));
#86844=CARTESIAN_POINT('Origin',(9.,-6.0709022117179,-5.09409180676582));
#86845=CARTESIAN_POINT('',(9.,-6.01296138690081,-5.27676940557761));
#86846=CARTESIAN_POINT('Origin',(9.,0.,0.));
#86847=CARTESIAN_POINT('',(9.,-5.86023998986018,-4.91732521410203));
#86848=CARTESIAN_POINT('Origin',(0.3,-6.10158390286339,-5.48535084350294));
#86849=CARTESIAN_POINT('',(0.3,-6.01296138690081,-5.27676940557761));
#86850=CARTESIAN_POINT('',(4.5,-6.01296138690081,-5.27676940557761));
#86851=CARTESIAN_POINT('',(0.3,-5.86023998986018,-4.91732521410203));
#86852=CARTESIAN_POINT('Origin',(0.3,-6.0709022117179,-5.09409180676582));
#86853=CARTESIAN_POINT('Origin',(0.3,0.,0.));
#86854=CARTESIAN_POINT('Origin',(0.3,-6.62509433895096,-3.825));
#86855=CARTESIAN_POINT('',(0.3,-7.01509518736965,-3.84557401594914));
#86856=CARTESIAN_POINT('',(9.,-7.01509518736965,-3.84557401594914));
#86857=CARTESIAN_POINT('',(4.5,-7.01509518736965,-3.84557401594914));
#86858=CARTESIAN_POINT('',(0.3,-6.62509433895096,-3.825));
#86859=CARTESIAN_POINT('',(0.3,-7.2414083110324,-3.85751288694035));
#86860=CARTESIAN_POINT('',(9.,-6.62509433895096,-3.825));
#86861=CARTESIAN_POINT('',(0.3,-6.62509433895096,-3.825));
#86862=CARTESIAN_POINT('',(9.,-7.2414083110324,-3.85751288694035));
#86863=CARTESIAN_POINT('Origin',(9.,-6.86325132499168,-3.9625));
#86864=CARTESIAN_POINT('',(9.,-6.83791238363012,-4.1524636342535));
#86865=CARTESIAN_POINT('Origin',(9.,0.,0.));
#86866=CARTESIAN_POINT('',(9.,-6.62509433895096,-3.825));
#86867=CARTESIAN_POINT('Origin',(0.3,-6.9614083110324,-4.34248711305964));
#86868=CARTESIAN_POINT('',(0.3,-6.83791238363012,-4.1524636342535));
#86869=CARTESIAN_POINT('',(4.5,-6.83791238363012,-4.1524636342535));
#86870=CARTESIAN_POINT('',(0.3,-6.62509433895096,-3.825));
#86871=CARTESIAN_POINT('Origin',(0.3,-6.86325132499168,-3.9625));
#86872=CARTESIAN_POINT('Origin',(0.3,0.,0.));
#86873=CARTESIAN_POINT('Origin',(0.3,-7.1886485490122,-2.61645409644137));
#86874=CARTESIAN_POINT('',(0.3,-7.57629704859313,-2.56899261024221));
#86875=CARTESIAN_POINT('',(9.,-7.57629704859313,-2.56899261024221));
#86876=CARTESIAN_POINT('',(4.5,-7.57629704859313,-2.56899261024221));
#86877=CARTESIAN_POINT('',(0.3,-7.1886485490122,-2.61645409644137));
#86878=CARTESIAN_POINT('',(0.3,-7.80124513057564,-2.54145124145043));
#86879=CARTESIAN_POINT('',(9.,-7.1886485490122,-2.61645409644137));
#86880=CARTESIAN_POINT('',(0.3,-7.1886485490122,-2.61645409644137));
#86881=CARTESIAN_POINT('',(9.,-7.80124513057564,-2.54145124145043));
#86882=CARTESIAN_POINT('Origin',(9.,-7.44706401972832,-2.71050963585592));
#86883=CARTESIAN_POINT('',(9.,-7.45509687273345,-2.90198735665059));
#86884=CARTESIAN_POINT('Origin',(9.,0.,0.));
#86885=CARTESIAN_POINT('',(9.,-7.1886485490122,-2.61645409644137));
#86886=CARTESIAN_POINT('Origin',(0.3,-7.60971385031326,-3.06767910909054));
#86887=CARTESIAN_POINT('',(0.3,-7.45509687273345,-2.90198735665059));
#86888=CARTESIAN_POINT('',(4.5,-7.45509687273345,-2.90198735665059));
#86889=CARTESIAN_POINT('',(0.3,-7.1886485490122,-2.61645409644137));
#86890=CARTESIAN_POINT('Origin',(0.3,-7.44706401972832,-2.71050963585592));
#86891=CARTESIAN_POINT('Origin',(0.3,0.,0.));
#86892=CARTESIAN_POINT('Origin',(0.3,-7.53377931054339,-1.32840855915201));
#86893=CARTESIAN_POINT('',(0.3,-7.90729695778639,-1.21435366404606));
#86894=CARTESIAN_POINT('',(9.,-7.90729695778639,-1.21435366404606));
#86895=CARTESIAN_POINT('',(4.5,-7.90729695778639,-1.21435366404606));
#86896=CARTESIAN_POINT('',(0.3,-7.53377931054339,-1.32840855915201));
#86897=CARTESIAN_POINT('',(0.3,-8.12404506444685,-1.14816888602541));
#86898=CARTESIAN_POINT('',(9.,-7.53377931054339,-1.32840855915201));
#86899=CARTESIAN_POINT('',(0.3,-7.53377931054339,-1.32840855915201));
#86900=CARTESIAN_POINT('',(9.,-8.12404506444685,-1.14816888602541));
#86901=CARTESIAN_POINT('Origin',(9.,-7.80460144262175,-1.37616180801042));
#86902=CARTESIAN_POINT('',(9.,-7.84576201581982,-1.56333566169231));
#86903=CARTESIAN_POINT('Origin',(9.,0.,0.));
#86904=CARTESIAN_POINT('',(9.,-7.53377931054339,-1.32840855915201));
#86905=CARTESIAN_POINT('Origin',(0.3,-8.02680208495337,-1.69966122771224));
#86906=CARTESIAN_POINT('',(0.3,-7.84576201581982,-1.56333566169231));
#86907=CARTESIAN_POINT('',(4.5,-7.84576201581982,-1.56333566169231));
#86908=CARTESIAN_POINT('',(0.3,-7.53377931054339,-1.32840855915201));
#86909=CARTESIAN_POINT('Origin',(0.3,-7.80460144262175,-1.37616180801042));
#86910=CARTESIAN_POINT('Origin',(0.3,0.,0.));
#86911=CARTESIAN_POINT('Origin',(0.3,-7.65,9.36854801347725E-16));
#86912=CARTESIAN_POINT('',(0.3,-7.99803765020264,0.177182803739527));
#86913=CARTESIAN_POINT('',(9.,-7.99803765020264,0.177182803739527));
#86914=CARTESIAN_POINT('',(4.5,-7.99803765020264,0.177182803739528));
#86915=CARTESIAN_POINT('',(0.3,-7.65,9.36854801347725E-16));
#86916=CARTESIAN_POINT('',(0.3,-8.2,0.280000000000001));
#86917=CARTESIAN_POINT('',(9.,-7.65,9.36854801347725E-16));
#86918=CARTESIAN_POINT('',(0.3,-7.65,9.36854801347725E-16));
#86919=CARTESIAN_POINT('',(9.,-8.2,0.280000000000001));
#86920=CARTESIAN_POINT('Origin',(9.,-7.925,9.70532588324277E-16));
#86921=CARTESIAN_POINT('',(9.,-8.,-9.79717439317883E-16));
#86922=CARTESIAN_POINT('Origin',(9.,0.,0.));
#86923=CARTESIAN_POINT('',(9.,-7.99803765020264,-0.177182803739526));
#86924=CARTESIAN_POINT('',(9.,-7.65,9.36854801347725E-16));
#86925=CARTESIAN_POINT('Origin',(9.,0.,0.));
#86926=CARTESIAN_POINT('Origin',(0.3,-8.2,-0.279999999999999));
#86927=CARTESIAN_POINT('',(0.3,-7.99803765020264,-0.177182803739526));
#86928=CARTESIAN_POINT('',(4.5,-7.99803765020264,-0.177182803739526));
#86929=CARTESIAN_POINT('',(0.3,-7.65,9.36854801347725E-16));
#86930=CARTESIAN_POINT('Origin',(0.3,-7.925,9.70532588324277E-16));
#86931=CARTESIAN_POINT('',(0.3,-8.,-9.79717439317883E-16));
#86932=CARTESIAN_POINT('Origin',(0.3,0.,0.));
#86933=CARTESIAN_POINT('Origin',(0.3,0.,0.));
#86934=CARTESIAN_POINT('Origin',(0.3,-7.53377931054339,1.32840855915202));
#86935=CARTESIAN_POINT('',(0.3,-7.84576201581982,1.56333566169232));
#86936=CARTESIAN_POINT('',(9.,-7.84576201581982,1.56333566169232));
#86937=CARTESIAN_POINT('',(4.5,-7.84576201581982,1.56333566169232));
#86938=CARTESIAN_POINT('',(0.3,-7.53377931054339,1.32840855915202));
#86939=CARTESIAN_POINT('',(0.3,-8.02680208495337,1.69966122771225));
#86940=CARTESIAN_POINT('',(9.,-7.53377931054339,1.32840855915202));
#86941=CARTESIAN_POINT('',(0.3,-7.53377931054339,1.32840855915202));
#86942=CARTESIAN_POINT('',(9.,-8.02680208495337,1.69966122771225));
#86943=CARTESIAN_POINT('Origin',(9.,-7.80460144262175,1.37616180801043));
#86944=CARTESIAN_POINT('',(9.,-7.90729695778639,1.21435366404606));
#86945=CARTESIAN_POINT('Origin',(9.,0.,0.));
#86946=CARTESIAN_POINT('',(9.,-7.53377931054339,1.32840855915202));
#86947=CARTESIAN_POINT('Origin',(0.3,-8.12404506444685,1.14816888602541));
#86948=CARTESIAN_POINT('',(0.3,-7.90729695778639,1.21435366404606));
#86949=CARTESIAN_POINT('',(4.5,-7.90729695778639,1.21435366404606));
#86950=CARTESIAN_POINT('',(0.3,-7.53377931054339,1.32840855915202));
#86951=CARTESIAN_POINT('Origin',(0.3,-7.80460144262175,1.37616180801043));
#86952=CARTESIAN_POINT('Origin',(0.3,0.,0.));
#86953=CARTESIAN_POINT('Origin',(0.3,-7.1886485490122,2.61645409644137));
#86954=CARTESIAN_POINT('',(0.3,-7.45509687273345,2.90198735665059));
#86955=CARTESIAN_POINT('',(9.,-7.45509687273345,2.90198735665059));
#86956=CARTESIAN_POINT('',(4.5,-7.45509687273345,2.90198735665059));
#86957=CARTESIAN_POINT('',(0.3,-7.1886485490122,2.61645409644137));
#86958=CARTESIAN_POINT('',(0.3,-7.60971385031326,3.06767910909054));
#86959=CARTESIAN_POINT('',(9.,-7.1886485490122,2.61645409644137));
#86960=CARTESIAN_POINT('',(0.3,-7.1886485490122,2.61645409644137));
#86961=CARTESIAN_POINT('',(9.,-7.60971385031326,3.06767910909054));
#86962=CARTESIAN_POINT('Origin',(9.,-7.44706401972832,2.71050963585593));
#86963=CARTESIAN_POINT('',(9.,-7.57629704859313,2.56899261024221));
#86964=CARTESIAN_POINT('Origin',(9.,0.,0.));
#86965=CARTESIAN_POINT('',(9.,-7.1886485490122,2.61645409644137));
#86966=CARTESIAN_POINT('Origin',(0.3,-7.80124513057564,2.54145124145043));
#86967=CARTESIAN_POINT('',(0.3,-7.57629704859313,2.56899261024221));
#86968=CARTESIAN_POINT('',(4.5,-7.57629704859313,2.56899261024221));
#86969=CARTESIAN_POINT('',(0.3,-7.1886485490122,2.61645409644137));
#86970=CARTESIAN_POINT('Origin',(0.3,-7.44706401972832,2.71050963585593));
#86971=CARTESIAN_POINT('Origin',(0.3,0.,0.));
#86972=CARTESIAN_POINT('Origin',(0.3,-6.62509433895096,3.825));
#86973=CARTESIAN_POINT('',(0.3,-6.83791238363012,4.1524636342535));
#86974=CARTESIAN_POINT('',(9.,-6.83791238363012,4.1524636342535));
#86975=CARTESIAN_POINT('',(4.5,-6.83791238363012,4.1524636342535));
#86976=CARTESIAN_POINT('',(0.3,-6.62509433895096,3.825));
#86977=CARTESIAN_POINT('',(0.3,-6.9614083110324,4.34248711305964));
#86978=CARTESIAN_POINT('',(9.,-6.62509433895096,3.825));
#86979=CARTESIAN_POINT('',(0.3,-6.62509433895096,3.825));
#86980=CARTESIAN_POINT('',(9.,-6.9614083110324,4.34248711305964));
#86981=CARTESIAN_POINT('Origin',(9.,-6.86325132499168,3.9625));
#86982=CARTESIAN_POINT('',(9.,-7.01509518736965,3.84557401594914));
#86983=CARTESIAN_POINT('Origin',(9.,0.,0.));
#86984=CARTESIAN_POINT('',(9.,-6.62509433895096,3.825));
#86985=CARTESIAN_POINT('Origin',(0.3,-7.2414083110324,3.85751288694036));
#86986=CARTESIAN_POINT('',(0.3,-7.01509518736965,3.84557401594914));
#86987=CARTESIAN_POINT('',(4.5,-7.01509518736965,3.84557401594914));
#86988=CARTESIAN_POINT('',(0.3,-6.62509433895096,3.825));
#86989=CARTESIAN_POINT('Origin',(0.3,-6.86325132499168,3.9625));
#86990=CARTESIAN_POINT('Origin',(0.3,0.,0.));
#86991=CARTESIAN_POINT('Origin',(0.3,-5.86023998986018,4.91732521410203));
#86992=CARTESIAN_POINT('',(0.3,-6.01296138690081,5.27676940557761));
#86993=CARTESIAN_POINT('',(9.,-6.01296138690081,5.27676940557761));
#86994=CARTESIAN_POINT('',(4.5,-6.01296138690081,5.27676940557761));
#86995=CARTESIAN_POINT('',(0.3,-5.86023998986018,4.91732521410203));
#86996=CARTESIAN_POINT('',(0.3,-6.10158390286339,5.48535084350294));
#86997=CARTESIAN_POINT('',(9.,-5.86023998986018,4.91732521410203));
#86998=CARTESIAN_POINT('',(0.3,-5.86023998986018,4.91732521410203));
#86999=CARTESIAN_POINT('',(9.,-6.10158390286339,5.48535084350294));
#87000=CARTESIAN_POINT('Origin',(9.,-6.0709022117179,5.09409180676582));
#87001=CARTESIAN_POINT('',(9.,-6.24074320868739,5.0053096011358));
#87002=CARTESIAN_POINT('Origin',(9.,0.,0.));
#87003=CARTESIAN_POINT('',(9.,-5.86023998986018,4.91732521410203));
#87004=CARTESIAN_POINT('Origin',(0.3,-6.46154496428785,5.05636595535631));
#87005=CARTESIAN_POINT('',(0.3,-6.24074320868739,5.0053096011358));
#87006=CARTESIAN_POINT('',(4.5,-6.24074320868739,5.0053096011358));
#87007=CARTESIAN_POINT('',(0.3,-5.86023998986018,4.91732521410203));
#87008=CARTESIAN_POINT('Origin',(0.3,-6.0709022117179,5.09409180676582));
#87009=CARTESIAN_POINT('Origin',(0.3,0.,0.));
#87010=CARTESIAN_POINT('Origin',(0.3,-4.91732521410203,5.86023998986018));
#87011=CARTESIAN_POINT('',(0.3,-5.0053096011358,6.24074320868739));
#87012=CARTESIAN_POINT('',(9.,-5.0053096011358,6.24074320868739));
#87013=CARTESIAN_POINT('',(4.5,-5.0053096011358,6.24074320868739));
#87014=CARTESIAN_POINT('',(0.3,-4.91732521410203,5.86023998986018));
#87015=CARTESIAN_POINT('',(0.3,-5.05636595535631,6.46154496428785));
#87016=CARTESIAN_POINT('',(9.,-4.91732521410203,5.86023998986018));
#87017=CARTESIAN_POINT('',(0.3,-4.91732521410203,5.86023998986018));
#87018=CARTESIAN_POINT('',(9.,-5.05636595535631,6.46154496428785));
#87019=CARTESIAN_POINT('Origin',(9.,-5.09409180676582,6.0709022117179));
#87020=CARTESIAN_POINT('',(9.,-5.27676940557761,6.01296138690081));
#87021=CARTESIAN_POINT('Origin',(9.,0.,0.));
#87022=CARTESIAN_POINT('',(9.,-4.91732521410203,5.86023998986018));
#87023=CARTESIAN_POINT('Origin',(0.3,-5.48535084350294,6.10158390286339));
#87024=CARTESIAN_POINT('',(0.3,-5.27676940557761,6.01296138690081));
#87025=CARTESIAN_POINT('',(4.5,-5.27676940557761,6.01296138690081));
#87026=CARTESIAN_POINT('',(0.3,-4.91732521410203,5.86023998986018));
#87027=CARTESIAN_POINT('Origin',(0.3,-5.09409180676582,6.0709022117179));
#87028=CARTESIAN_POINT('Origin',(0.3,0.,0.));
#87029=CARTESIAN_POINT('Origin',(0.3,-3.825,6.62509433895096));
#87030=CARTESIAN_POINT('',(0.3,-3.84557401594914,7.01509518736965));
#87031=CARTESIAN_POINT('',(9.,-3.84557401594914,7.01509518736965));
#87032=CARTESIAN_POINT('',(4.5,-3.84557401594914,7.01509518736965));
#87033=CARTESIAN_POINT('',(0.3,-3.825,6.62509433895096));
#87034=CARTESIAN_POINT('',(0.3,-3.85751288694036,7.2414083110324));
#87035=CARTESIAN_POINT('',(9.,-3.825,6.62509433895096));
#87036=CARTESIAN_POINT('',(0.3,-3.825,6.62509433895096));
#87037=CARTESIAN_POINT('',(9.,-3.85751288694036,7.2414083110324));
#87038=CARTESIAN_POINT('Origin',(9.,-3.9625,6.86325132499168));
#87039=CARTESIAN_POINT('',(9.,-4.1524636342535,6.83791238363012));
#87040=CARTESIAN_POINT('Origin',(9.,0.,0.));
#87041=CARTESIAN_POINT('',(9.,-3.825,6.62509433895096));
#87042=CARTESIAN_POINT('Origin',(0.3,-4.34248711305964,6.9614083110324));
#87043=CARTESIAN_POINT('',(0.3,-4.1524636342535,6.83791238363012));
#87044=CARTESIAN_POINT('',(4.5,-4.1524636342535,6.83791238363012));
#87045=CARTESIAN_POINT('',(0.3,-3.825,6.62509433895096));
#87046=CARTESIAN_POINT('Origin',(0.3,-3.9625,6.86325132499168));
#87047=CARTESIAN_POINT('Origin',(0.3,0.,0.));
#87048=CARTESIAN_POINT('Origin',(0.3,-2.61645409644137,7.1886485490122));
#87049=CARTESIAN_POINT('',(0.3,-2.56899261024221,7.57629704859313));
#87050=CARTESIAN_POINT('',(9.,-2.56899261024221,7.57629704859313));
#87051=CARTESIAN_POINT('',(4.5,-2.56899261024221,7.57629704859313));
#87052=CARTESIAN_POINT('',(0.3,-2.61645409644137,7.1886485490122));
#87053=CARTESIAN_POINT('',(0.3,-2.54145124145043,7.80124513057564));
#87054=CARTESIAN_POINT('',(9.,-2.61645409644137,7.1886485490122));
#87055=CARTESIAN_POINT('',(0.3,-2.61645409644137,7.1886485490122));
#87056=CARTESIAN_POINT('',(9.,-2.54145124145043,7.80124513057564));
#87057=CARTESIAN_POINT('Origin',(9.,-2.71050963585592,7.44706401972832));
#87058=CARTESIAN_POINT('',(9.,-2.90198735665059,7.45509687273345));
#87059=CARTESIAN_POINT('Origin',(9.,0.,0.));
#87060=CARTESIAN_POINT('',(9.,-2.61645409644137,7.1886485490122));
#87061=CARTESIAN_POINT('Origin',(0.3,-3.06767910909054,7.60971385031326));
#87062=CARTESIAN_POINT('',(0.3,-2.90198735665059,7.45509687273345));
#87063=CARTESIAN_POINT('',(4.5,-2.90198735665059,7.45509687273345));
#87064=CARTESIAN_POINT('',(0.3,-2.61645409644137,7.1886485490122));
#87065=CARTESIAN_POINT('Origin',(0.3,-2.71050963585592,7.44706401972832));
#87066=CARTESIAN_POINT('Origin',(0.3,0.,0.));
#87067=CARTESIAN_POINT('Origin',(0.3,-1.32840855915202,7.53377931054339));
#87068=CARTESIAN_POINT('',(0.3,-1.21435366404606,7.90729695778639));
#87069=CARTESIAN_POINT('',(9.,-1.21435366404606,7.90729695778639));
#87070=CARTESIAN_POINT('',(4.5,-1.21435366404606,7.90729695778639));
#87071=CARTESIAN_POINT('',(0.3,-1.32840855915202,7.53377931054339));
#87072=CARTESIAN_POINT('',(0.3,-1.14816888602541,8.12404506444685));
#87073=CARTESIAN_POINT('',(9.,-1.32840855915202,7.53377931054339));
#87074=CARTESIAN_POINT('',(0.3,-1.32840855915202,7.53377931054339));
#87075=CARTESIAN_POINT('',(9.,-1.14816888602541,8.12404506444685));
#87076=CARTESIAN_POINT('Origin',(9.,-1.37616180801042,7.80460144262175));
#87077=CARTESIAN_POINT('',(9.,-1.56333566169231,7.84576201581982));
#87078=CARTESIAN_POINT('Origin',(9.,0.,0.));
#87079=CARTESIAN_POINT('',(9.,-1.32840855915202,7.53377931054339));
#87080=CARTESIAN_POINT('Origin',(0.3,-1.69966122771225,8.02680208495337));
#87081=CARTESIAN_POINT('',(0.3,-1.56333566169231,7.84576201581982));
#87082=CARTESIAN_POINT('',(4.5,-1.56333566169231,7.84576201581982));
#87083=CARTESIAN_POINT('',(0.3,-1.32840855915202,7.53377931054339));
#87084=CARTESIAN_POINT('Origin',(0.3,-1.37616180801042,7.80460144262175));
#87085=CARTESIAN_POINT('Origin',(0.3,0.,0.));
#87086=CARTESIAN_POINT('Origin',(0.3,4.68427400673863E-16,7.65));
#87087=CARTESIAN_POINT('',(0.3,0.177182803739527,7.99803765020264));
#87088=CARTESIAN_POINT('',(9.,0.177182803739527,7.99803765020264));
#87089=CARTESIAN_POINT('',(4.5,0.177182803739527,7.99803765020264));
#87090=CARTESIAN_POINT('',(0.3,4.68427400673863E-16,7.65));
#87091=CARTESIAN_POINT('',(0.3,0.28,8.2));
#87092=CARTESIAN_POINT('',(9.,4.68427400673863E-16,7.65));
#87093=CARTESIAN_POINT('',(0.3,4.68427400673863E-16,7.65));
#87094=CARTESIAN_POINT('',(9.,0.28,8.2));
#87095=CARTESIAN_POINT('Origin',(9.,4.85266294162139E-16,7.925));
#87096=CARTESIAN_POINT('',(9.,-0.177182803739526,7.99803765020264));
#87097=CARTESIAN_POINT('Origin',(9.,0.,0.));
#87098=CARTESIAN_POINT('',(9.,4.68427400673863E-16,7.65));
#87099=CARTESIAN_POINT('Origin',(0.3,-0.279999999999999,8.2));
#87100=CARTESIAN_POINT('',(0.3,-0.177182803739526,7.99803765020264));
#87101=CARTESIAN_POINT('',(4.5,-0.177182803739526,7.99803765020264));
#87102=CARTESIAN_POINT('',(0.3,4.68427400673863E-16,7.65));
#87103=CARTESIAN_POINT('Origin',(0.3,4.85266294162139E-16,7.925));
#87104=CARTESIAN_POINT('Origin',(0.3,0.,0.));
#87105=CARTESIAN_POINT('Origin',(0.3,1.32840855915202,7.53377931054339));
#87106=CARTESIAN_POINT('',(0.3,1.56333566169231,7.84576201581982));
#87107=CARTESIAN_POINT('',(9.,1.56333566169231,7.84576201581982));
#87108=CARTESIAN_POINT('',(4.5,1.56333566169231,7.84576201581982));
#87109=CARTESIAN_POINT('',(0.3,1.32840855915202,7.53377931054339));
#87110=CARTESIAN_POINT('',(0.3,1.69966122771225,8.02680208495337));
#87111=CARTESIAN_POINT('',(9.,1.32840855915202,7.53377931054339));
#87112=CARTESIAN_POINT('',(0.3,1.32840855915202,7.53377931054339));
#87113=CARTESIAN_POINT('',(9.,1.69966122771225,8.02680208495337));
#87114=CARTESIAN_POINT('Origin',(9.,1.37616180801042,7.80460144262175));
#87115=CARTESIAN_POINT('',(9.,1.21435366404606,7.90729695778639));
#87116=CARTESIAN_POINT('Origin',(9.,0.,0.));
#87117=CARTESIAN_POINT('',(9.,1.32840855915202,7.53377931054339));
#87118=CARTESIAN_POINT('Origin',(0.3,1.14816888602541,8.12404506444685));
#87119=CARTESIAN_POINT('',(0.3,1.21435366404606,7.90729695778639));
#87120=CARTESIAN_POINT('',(4.5,1.21435366404606,7.90729695778639));
#87121=CARTESIAN_POINT('',(0.3,1.32840855915202,7.53377931054339));
#87122=CARTESIAN_POINT('Origin',(0.3,1.37616180801042,7.80460144262175));
#87123=CARTESIAN_POINT('Origin',(0.3,0.,0.));
#87124=CARTESIAN_POINT('Origin',(0.3,2.61645409644137,7.1886485490122));
#87125=CARTESIAN_POINT('',(0.3,2.90198735665059,7.45509687273345));
#87126=CARTESIAN_POINT('',(9.,2.90198735665059,7.45509687273345));
#87127=CARTESIAN_POINT('',(4.5,2.90198735665059,7.45509687273345));
#87128=CARTESIAN_POINT('',(0.3,2.61645409644137,7.1886485490122));
#87129=CARTESIAN_POINT('',(0.3,3.06767910909054,7.60971385031326));
#87130=CARTESIAN_POINT('',(9.,2.61645409644137,7.1886485490122));
#87131=CARTESIAN_POINT('',(0.3,2.61645409644137,7.1886485490122));
#87132=CARTESIAN_POINT('',(9.,3.06767910909054,7.60971385031326));
#87133=CARTESIAN_POINT('Origin',(9.,2.71050963585593,7.44706401972832));
#87134=CARTESIAN_POINT('',(9.,2.56899261024221,7.57629704859313));
#87135=CARTESIAN_POINT('Origin',(9.,0.,0.));
#87136=CARTESIAN_POINT('',(9.,2.61645409644137,7.1886485490122));
#87137=CARTESIAN_POINT('Origin',(0.3,2.54145124145043,7.80124513057564));
#87138=CARTESIAN_POINT('',(0.3,2.56899261024221,7.57629704859313));
#87139=CARTESIAN_POINT('',(4.5,2.56899261024221,7.57629704859313));
#87140=CARTESIAN_POINT('',(0.3,2.61645409644137,7.1886485490122));
#87141=CARTESIAN_POINT('Origin',(0.3,2.71050963585593,7.44706401972832));
#87142=CARTESIAN_POINT('Origin',(0.3,0.,0.));
#87143=CARTESIAN_POINT('Origin',(0.3,3.825,6.62509433895096));
#87144=CARTESIAN_POINT('',(0.3,4.15246363425351,6.83791238363012));
#87145=CARTESIAN_POINT('',(9.,4.15246363425351,6.83791238363012));
#87146=CARTESIAN_POINT('',(4.5,4.15246363425351,6.83791238363012));
#87147=CARTESIAN_POINT('',(0.3,3.825,6.62509433895096));
#87148=CARTESIAN_POINT('',(0.3,4.34248711305964,6.96140831103239));
#87149=CARTESIAN_POINT('',(9.,3.825,6.62509433895096));
#87150=CARTESIAN_POINT('',(0.3,3.825,6.62509433895096));
#87151=CARTESIAN_POINT('',(9.,4.34248711305964,6.96140831103239));
#87152=CARTESIAN_POINT('Origin',(9.,3.9625,6.86325132499168));
#87153=CARTESIAN_POINT('',(9.,3.84557401594914,7.01509518736965));
#87154=CARTESIAN_POINT('Origin',(9.,0.,0.));
#87155=CARTESIAN_POINT('',(9.,3.825,6.62509433895096));
#87156=CARTESIAN_POINT('Origin',(0.3,3.85751288694036,7.2414083110324));
#87157=CARTESIAN_POINT('',(0.3,3.84557401594914,7.01509518736965));
#87158=CARTESIAN_POINT('',(4.5,3.84557401594914,7.01509518736965));
#87159=CARTESIAN_POINT('',(0.3,3.825,6.62509433895096));
#87160=CARTESIAN_POINT('Origin',(0.3,3.9625,6.86325132499168));
#87161=CARTESIAN_POINT('Origin',(0.3,0.,0.));
#87162=CARTESIAN_POINT('Origin',(0.3,4.91732521410203,5.86023998986018));
#87163=CARTESIAN_POINT('',(0.3,5.27676940557761,6.01296138690081));
#87164=CARTESIAN_POINT('',(9.,5.27676940557761,6.01296138690081));
#87165=CARTESIAN_POINT('',(4.5,5.27676940557761,6.01296138690081));
#87166=CARTESIAN_POINT('',(0.3,4.91732521410203,5.86023998986018));
#87167=CARTESIAN_POINT('',(0.3,5.48535084350294,6.10158390286339));
#87168=CARTESIAN_POINT('',(9.,4.91732521410203,5.86023998986018));
#87169=CARTESIAN_POINT('',(0.3,4.91732521410203,5.86023998986018));
#87170=CARTESIAN_POINT('',(9.,5.48535084350294,6.10158390286339));
#87171=CARTESIAN_POINT('Origin',(9.,5.09409180676582,6.0709022117179));
#87172=CARTESIAN_POINT('',(9.,5.0053096011358,6.24074320868739));
#87173=CARTESIAN_POINT('Origin',(9.,0.,0.));
#87174=CARTESIAN_POINT('',(9.,4.91732521410203,5.86023998986018));
#87175=CARTESIAN_POINT('Origin',(0.3,5.05636595535631,6.46154496428785));
#87176=CARTESIAN_POINT('',(0.3,5.0053096011358,6.24074320868739));
#87177=CARTESIAN_POINT('',(4.5,5.0053096011358,6.24074320868739));
#87178=CARTESIAN_POINT('',(0.3,4.91732521410203,5.86023998986018));
#87179=CARTESIAN_POINT('Origin',(0.3,5.09409180676582,6.0709022117179));
#87180=CARTESIAN_POINT('Origin',(0.3,0.,0.));
#87181=CARTESIAN_POINT('Origin',(0.3,5.86023998986018,4.91732521410203));
#87182=CARTESIAN_POINT('',(0.3,6.24074320868739,5.0053096011358));
#87183=CARTESIAN_POINT('',(9.,6.24074320868739,5.0053096011358));
#87184=CARTESIAN_POINT('',(4.5,6.24074320868739,5.0053096011358));
#87185=CARTESIAN_POINT('',(0.3,5.86023998986018,4.91732521410203));
#87186=CARTESIAN_POINT('',(0.3,6.46154496428785,5.05636595535631));
#87187=CARTESIAN_POINT('',(9.,5.86023998986018,4.91732521410203));
#87188=CARTESIAN_POINT('',(0.3,5.86023998986018,4.91732521410203));
#87189=CARTESIAN_POINT('',(9.,6.46154496428785,5.05636595535631));
#87190=CARTESIAN_POINT('Origin',(9.,6.0709022117179,5.09409180676582));
#87191=CARTESIAN_POINT('',(9.,6.01296138690081,5.27676940557761));
#87192=CARTESIAN_POINT('Origin',(9.,0.,0.));
#87193=CARTESIAN_POINT('',(9.,5.86023998986018,4.91732521410203));
#87194=CARTESIAN_POINT('Origin',(0.3,6.10158390286339,5.48535084350294));
#87195=CARTESIAN_POINT('',(0.3,6.01296138690081,5.27676940557761));
#87196=CARTESIAN_POINT('',(4.5,6.01296138690081,5.27676940557761));
#87197=CARTESIAN_POINT('',(0.3,5.86023998986018,4.91732521410203));
#87198=CARTESIAN_POINT('Origin',(0.3,6.0709022117179,5.09409180676582));
#87199=CARTESIAN_POINT('Origin',(0.3,0.,0.));
#87200=CARTESIAN_POINT('Origin',(0.3,6.62509433895096,3.825));
#87201=CARTESIAN_POINT('',(0.3,7.01509518736965,3.84557401594914));
#87202=CARTESIAN_POINT('',(9.,7.01509518736965,3.84557401594914));
#87203=CARTESIAN_POINT('',(4.5,7.01509518736965,3.84557401594914));
#87204=CARTESIAN_POINT('',(0.3,6.62509433895096,3.825));
#87205=CARTESIAN_POINT('',(0.3,7.2414083110324,3.85751288694036));
#87206=CARTESIAN_POINT('',(9.,6.62509433895096,3.825));
#87207=CARTESIAN_POINT('',(0.3,6.62509433895096,3.825));
#87208=CARTESIAN_POINT('',(9.,7.2414083110324,3.85751288694036));
#87209=CARTESIAN_POINT('Origin',(9.,6.86325132499168,3.9625));
#87210=CARTESIAN_POINT('',(9.,6.83791238363012,4.1524636342535));
#87211=CARTESIAN_POINT('Origin',(9.,0.,0.));
#87212=CARTESIAN_POINT('',(9.,6.62509433895096,3.825));
#87213=CARTESIAN_POINT('Origin',(0.3,6.9614083110324,4.34248711305964));
#87214=CARTESIAN_POINT('',(0.3,6.83791238363012,4.1524636342535));
#87215=CARTESIAN_POINT('',(4.5,6.83791238363012,4.1524636342535));
#87216=CARTESIAN_POINT('',(0.3,6.62509433895096,3.825));
#87217=CARTESIAN_POINT('Origin',(0.3,6.86325132499168,3.9625));
#87218=CARTESIAN_POINT('Origin',(0.3,0.,0.));
#87219=CARTESIAN_POINT('Origin',(0.3,7.1886485490122,2.61645409644137));
#87220=CARTESIAN_POINT('',(0.3,7.57629704859313,2.56899261024221));
#87221=CARTESIAN_POINT('',(9.,7.57629704859313,2.56899261024221));
#87222=CARTESIAN_POINT('',(4.5,7.57629704859313,2.56899261024221));
#87223=CARTESIAN_POINT('',(0.3,7.1886485490122,2.61645409644137));
#87224=CARTESIAN_POINT('',(0.3,7.80124513057564,2.54145124145043));
#87225=CARTESIAN_POINT('',(9.,7.1886485490122,2.61645409644137));
#87226=CARTESIAN_POINT('',(0.3,7.1886485490122,2.61645409644137));
#87227=CARTESIAN_POINT('',(9.,7.80124513057564,2.54145124145043));
#87228=CARTESIAN_POINT('Origin',(9.,7.44706401972832,2.71050963585592));
#87229=CARTESIAN_POINT('',(9.,7.45509687273345,2.90198735665059));
#87230=CARTESIAN_POINT('Origin',(9.,0.,0.));
#87231=CARTESIAN_POINT('',(9.,7.1886485490122,2.61645409644137));
#87232=CARTESIAN_POINT('Origin',(0.3,7.60971385031326,3.06767910909054));
#87233=CARTESIAN_POINT('',(0.3,7.45509687273345,2.90198735665059));
#87234=CARTESIAN_POINT('',(4.5,7.45509687273345,2.90198735665059));
#87235=CARTESIAN_POINT('',(0.3,7.1886485490122,2.61645409644137));
#87236=CARTESIAN_POINT('Origin',(0.3,7.44706401972832,2.71050963585592));
#87237=CARTESIAN_POINT('Origin',(0.3,0.,0.));
#87238=CARTESIAN_POINT('Origin',(0.3,7.53377931054339,1.32840855915202));
#87239=CARTESIAN_POINT('',(0.3,7.90729695778639,1.21435366404606));
#87240=CARTESIAN_POINT('',(9.,7.90729695778639,1.21435366404606));
#87241=CARTESIAN_POINT('',(4.5,7.90729695778639,1.21435366404606));
#87242=CARTESIAN_POINT('',(0.3,7.53377931054339,1.32840855915202));
#87243=CARTESIAN_POINT('',(0.3,8.12404506444685,1.14816888602541));
#87244=CARTESIAN_POINT('',(9.,7.53377931054339,1.32840855915202));
#87245=CARTESIAN_POINT('',(0.3,7.53377931054339,1.32840855915202));
#87246=CARTESIAN_POINT('',(9.,8.12404506444685,1.14816888602541));
#87247=CARTESIAN_POINT('Origin',(9.,7.80460144262175,1.37616180801042));
#87248=CARTESIAN_POINT('',(9.,7.84576201581982,1.56333566169231));
#87249=CARTESIAN_POINT('Origin',(9.,0.,0.));
#87250=CARTESIAN_POINT('',(9.,7.53377931054339,1.32840855915202));
#87251=CARTESIAN_POINT('Origin',(0.3,8.02680208495337,1.69966122771225));
#87252=CARTESIAN_POINT('',(0.3,7.84576201581982,1.56333566169231));
#87253=CARTESIAN_POINT('',(4.5,7.84576201581982,1.56333566169232));
#87254=CARTESIAN_POINT('',(0.3,7.53377931054339,1.32840855915202));
#87255=CARTESIAN_POINT('Origin',(0.3,7.80460144262175,1.37616180801042));
#87256=CARTESIAN_POINT('Origin',(0.3,0.,0.));
#87257=CARTESIAN_POINT('Origin',(9.,7.925,0.));
#87258=CARTESIAN_POINT('',(9.,7.99803765020264,-0.177182803739528));
#87259=CARTESIAN_POINT('',(9.,7.99803765020264,0.177182803739527));
#87260=CARTESIAN_POINT('Origin',(9.,0.,0.));
#87261=CARTESIAN_POINT('',(9.,7.65,0.));
#87262=CARTESIAN_POINT('',(9.,8.2,-0.28));
#87263=CARTESIAN_POINT('',(9.,7.65,0.));
#87264=CARTESIAN_POINT('Origin',(0.3,7.65,0.));
#87265=CARTESIAN_POINT('',(0.3,7.99803765020264,-0.177182803739528));
#87266=CARTESIAN_POINT('',(4.5,7.99803765020264,-0.177182803739527));
#87267=CARTESIAN_POINT('',(0.3,7.65,0.));
#87268=CARTESIAN_POINT('',(0.3,8.2,-0.28));
#87269=CARTESIAN_POINT('',(0.3,7.65,0.));
#87270=CARTESIAN_POINT('Origin',(0.3,8.2,0.28));
#87271=CARTESIAN_POINT('',(0.3,7.99803765020264,0.177182803739527));
#87272=CARTESIAN_POINT('',(4.5,7.99803765020264,0.177182803739528));
#87273=CARTESIAN_POINT('',(0.3,7.65,0.));
#87274=CARTESIAN_POINT('Origin',(0.3,7.925,0.));
#87275=CARTESIAN_POINT('Origin',(0.3,0.,0.));
#87276=CARTESIAN_POINT('Origin',(3.80327876194488,0.,0.));
#87277=CARTESIAN_POINT('',(2.59655752388976,0.,0.));
#87278=CARTESIAN_POINT('',(5.,-3.98342616391485,4.87829010127814E-16));
#87279=CARTESIAN_POINT('',(3.80327876194488,-2.,-2.44929359829471E-16));
#87280=CARTESIAN_POINT('Origin',(5.,0.,0.));
#87281=CARTESIAN_POINT('Origin',(5.,2.82820063659975E-16,4.61880215351701));
#87282=CARTESIAN_POINT('',(10.,-4.,2.3094010767585));
#87283=CARTESIAN_POINT('',(10.,2.82820063659975E-16,4.61880215351701));
#87284=CARTESIAN_POINT('',(10.,-1.,4.04145188432738));
#87285=CARTESIAN_POINT('',(5.,-4.,2.3094010767585));
#87286=CARTESIAN_POINT('',(5.,-4.,2.3094010767585));
#87287=CARTESIAN_POINT('',(5.,2.82820063659975E-16,4.61880215351701));
#87288=CARTESIAN_POINT('',(5.,2.82820063659975E-16,4.61880215351701));
#87289=CARTESIAN_POINT('',(5.,2.82820063659975E-16,4.61880215351701));
#87290=CARTESIAN_POINT('Origin',(5.,4.,2.3094010767585));
#87291=CARTESIAN_POINT('',(10.,4.,2.3094010767585));
#87292=CARTESIAN_POINT('',(10.,3.,2.88675134594813));
#87293=CARTESIAN_POINT('',(5.,4.,2.3094010767585));
#87294=CARTESIAN_POINT('',(5.,4.,2.3094010767585));
#87295=CARTESIAN_POINT('',(5.,4.,2.3094010767585));
#87296=CARTESIAN_POINT('Origin',(5.,4.,-2.30940107675851));
#87297=CARTESIAN_POINT('',(10.,4.,-2.30940107675851));
#87298=CARTESIAN_POINT('',(10.,4.,-1.15470053837925));
#87299=CARTESIAN_POINT('',(5.,4.,-2.30940107675851));
#87300=CARTESIAN_POINT('',(5.,4.,-2.30940107675851));
#87301=CARTESIAN_POINT('',(5.,4.,-2.30940107675851));
#87302=CARTESIAN_POINT('Origin',(5.,-8.48460190979926E-16,-4.61880215351701));
#87303=CARTESIAN_POINT('',(10.,-8.48460190979926E-16,-4.61880215351701));
#87304=CARTESIAN_POINT('',(10.,0.999999999999999,-4.04145188432738));
#87305=CARTESIAN_POINT('',(5.,-8.48460190979926E-16,-4.61880215351701));
#87306=CARTESIAN_POINT('',(5.,-8.48460190979926E-16,-4.61880215351701));
#87307=CARTESIAN_POINT('',(5.,-8.48460190979926E-16,-4.61880215351701));
#87308=CARTESIAN_POINT('Origin',(5.,-4.,-2.3094010767585));
#87309=CARTESIAN_POINT('',(10.,-4.,-2.3094010767585));
#87310=CARTESIAN_POINT('',(10.,-3.,-2.88675134594813));
#87311=CARTESIAN_POINT('',(5.,-4.,-2.3094010767585));
#87312=CARTESIAN_POINT('',(5.,-4.,-2.3094010767585));
#87313=CARTESIAN_POINT('',(5.,-4.,-2.3094010767585));
#87314=CARTESIAN_POINT('Origin',(5.,-4.,2.3094010767585));
#87315=CARTESIAN_POINT('',(10.,-4.,1.15470053837925));
#87316=CARTESIAN_POINT('',(5.,-4.,2.3094010767585));
#87317=CARTESIAN_POINT('Origin',(5.,0.,0.));
#87318=CARTESIAN_POINT('Origin',(-25.,4.,0.));
#87319=CARTESIAN_POINT('',(-25.,-4.,-4.89858719658941E-16));
#87320=CARTESIAN_POINT('Origin',(-25.,0.,0.));
#87321=CARTESIAN_POINT('Origin',(-24.5,0.,0.));
#87322=CARTESIAN_POINT('',(-24.5,-4.5,-5.51091059616309E-16));
#87323=CARTESIAN_POINT('Origin',(4.5,0.,0.));
#87324=CARTESIAN_POINT('Origin',(9.,0.,0.));
#87325=CARTESIAN_POINT('Origin',(9.,0.,0.));
#87326=CARTESIAN_POINT('Origin',(9.,0.,0.));
#87327=CARTESIAN_POINT('Origin',(9.,0.,0.));
#87328=CARTESIAN_POINT('Origin',(9.,0.,0.));
#87329=CARTESIAN_POINT('Origin',(9.,0.,0.));
#87330=CARTESIAN_POINT('Origin',(9.,0.,0.));
#87331=CARTESIAN_POINT('Origin',(9.,0.,0.));
#87332=CARTESIAN_POINT('Origin',(9.,0.,0.));
#87333=CARTESIAN_POINT('Origin',(9.,0.,0.));
#87334=CARTESIAN_POINT('Origin',(9.,0.,0.));
#87335=CARTESIAN_POINT('Origin',(9.,0.,0.));
#87336=CARTESIAN_POINT('Origin',(9.,0.,0.));
#87337=CARTESIAN_POINT('Origin',(9.,0.,0.));
#87338=CARTESIAN_POINT('Origin',(9.,0.,0.));
#87339=CARTESIAN_POINT('Origin',(9.,0.,0.));
#87340=CARTESIAN_POINT('Origin',(9.,0.,0.));
#87341=CARTESIAN_POINT('',(4.5,-8.,-9.79717439317883E-16));
#87342=CARTESIAN_POINT('Origin',(9.,0.,0.));
#87343=CARTESIAN_POINT('Origin',(9.,0.,0.));
#87344=CARTESIAN_POINT('Origin',(9.,0.,0.));
#87345=CARTESIAN_POINT('Origin',(9.,0.,0.));
#87346=CARTESIAN_POINT('Origin',(9.,0.,0.));
#87347=CARTESIAN_POINT('Origin',(9.,0.,0.));
#87348=CARTESIAN_POINT('Origin',(9.,0.,0.));
#87349=CARTESIAN_POINT('Origin',(9.,0.,0.));
#87350=CARTESIAN_POINT('Origin',(9.,0.,0.));
#87351=CARTESIAN_POINT('Origin',(9.,0.,0.));
#87352=CARTESIAN_POINT('Origin',(9.,0.,0.));
#87353=CARTESIAN_POINT('Origin',(9.,0.,0.));
#87354=CARTESIAN_POINT('Origin',(9.,0.,0.));
#87355=CARTESIAN_POINT('Origin',(9.,0.,0.));
#87356=CARTESIAN_POINT('Origin',(9.,0.,0.));
#87357=CARTESIAN_POINT('Origin',(9.,0.,0.));
#87358=CARTESIAN_POINT('Origin',(9.,0.,0.));
#87359=CARTESIAN_POINT('Origin',(9.,0.,0.));
#87360=CARTESIAN_POINT('Origin',(9.,0.,0.));
#87361=CARTESIAN_POINT('Origin',(9.5,0.,0.));
#87362=CARTESIAN_POINT('',(10.,-7.,-8.57252759403147E-16));
#87363=CARTESIAN_POINT('Origin',(10.,0.,0.));
#87364=CARTESIAN_POINT('',(9.5,-7.5,-9.18485099360515E-16));
#87365=CARTESIAN_POINT('Origin',(10.,0.,0.));
#87366=CARTESIAN_POINT('',(0.,0.,0.));
#87367=CARTESIAN_POINT('Origin',(0.1,0.,0.));
#87368=CARTESIAN_POINT('',(0.2,-10.,-1.22464679914735E-15));
#87369=CARTESIAN_POINT('Origin',(0.2,0.,0.));
#87370=CARTESIAN_POINT('',(1.21430643318376E-16,-9.8,-1.20015386316441E-15));
#87371=CARTESIAN_POINT('',(0.1,-9.9,-1.21240033115588E-15));
#87372=CARTESIAN_POINT('Origin',(0.,0.,0.));
#87373=CARTESIAN_POINT('Origin',(1.,0.,0.));
#87374=CARTESIAN_POINT('',(1.8,-10.,-1.22464679914735E-15));
#87375=CARTESIAN_POINT('Origin',(1.8,0.,0.));
#87376=CARTESIAN_POINT('',(1.,-10.,-1.22464679914735E-15));
#87377=CARTESIAN_POINT('Origin',(1.9,0.,0.));
#87378=CARTESIAN_POINT('',(2.,-9.8,-1.20015386316441E-15));
#87379=CARTESIAN_POINT('Origin',(2.,0.,0.));
#87380=CARTESIAN_POINT('',(1.9,-9.9,-1.21240033115588E-15));
#87381=CARTESIAN_POINT('Origin',(2.,5.45,0.));
#87382=CARTESIAN_POINT('',(2.,-5.45,-6.67432505535308E-16));
#87383=CARTESIAN_POINT('Origin',(2.,0.,0.));
#87384=CARTESIAN_POINT('Origin',(1.9,0.,0.));
#87385=CARTESIAN_POINT('',(1.8,-5.25,-6.42939569552361E-16));
#87386=CARTESIAN_POINT('',(1.9,-5.35,-6.55186037543834E-16));
#87387=CARTESIAN_POINT('Origin',(1.8,0.,0.));
#87388=CARTESIAN_POINT('Origin',(1.,0.,0.));
#87389=CARTESIAN_POINT('',(0.2,-5.25,-6.42939569552361E-16));
#87390=CARTESIAN_POINT('',(1.,-5.25,-6.42939569552361E-16));
#87391=CARTESIAN_POINT('Origin',(0.2,0.,0.));
#87392=CARTESIAN_POINT('Origin',(0.1,0.,0.));
#87393=CARTESIAN_POINT('',(-8.67361737988404E-17,-5.45,-6.67432505535308E-16));
#87394=CARTESIAN_POINT('',(0.1,-5.35,-6.55186037543834E-16));
#87395=CARTESIAN_POINT('Origin',(0.,0.,0.));
#87396=CARTESIAN_POINT('Origin',(0.,9.8,0.));
#87397=CARTESIAN_POINT('',(0.,0.,0.));
#87398=CARTESIAN_POINT('Origin',(1.1,0.,0.));
#87399=CARTESIAN_POINT('',(1.7,-5.1,-6.2456986756515E-16));
#87400=CARTESIAN_POINT('',(0.499999999999998,-5.1,-6.2456986756515E-16));
#87401=CARTESIAN_POINT('',(1.1,-5.1,-6.2456986756515E-16));
#87402=CARTESIAN_POINT('',(1.7,1.28149545762236,4.93637208809195));
#87403=CARTESIAN_POINT('Origin',(1.7,0.,0.));
#87404=CARTESIAN_POINT('',(0.5,0.588675134594813,5.06591172306721));
#87405=CARTESIAN_POINT('Origin',(-0.519615242270663,0.,0.));
#87406=CARTESIAN_POINT('Origin',(0.5,0.,0.));
#87407=CARTESIAN_POINT('Origin',(1.1,0.,0.));
#87408=CARTESIAN_POINT('',(2.05,-9.05,-1.10830535322835E-15));
#87409=CARTESIAN_POINT('',(0.149999999999998,-9.05,-1.10830535322835E-15));
#87410=CARTESIAN_POINT('',(1.1,-9.05,-1.10830535322835E-15));
#87411=CARTESIAN_POINT('',(2.05,0.883568051838733,9.00676454104191));
#87412=CARTESIAN_POINT('Origin',(2.05,0.,0.));
#87413=CARTESIAN_POINT('',(0.15,-0.213397459621556,9.0474837122941));
#87414=CARTESIAN_POINT('Origin',(0.519615242270663,0.,0.));
#87415=CARTESIAN_POINT('Origin',(0.15,0.,0.));
#87416=CARTESIAN_POINT('Origin',(2.4,1.6856406460551,0.));
#87417=CARTESIAN_POINT('',(2.2,1.57017059221718,5.37536643507551));
#87418=CARTESIAN_POINT('Ctrl Pts',(2.2,1.57017059221718,5.37536643507551));
#87419=CARTESIAN_POINT('Ctrl Pts',(1.93935692691251,1.4196882438077,5.14778785676925));
#87420=CARTESIAN_POINT('Ctrl Pts',(1.7,1.28149545762236,4.93637208809195));
#87421=CARTESIAN_POINT('',(2.2,1.57017059221718,8.76039749733631));
#87422=CARTESIAN_POINT('',(2.2,1.57017059221718,0.));
#87423=CARTESIAN_POINT('',(2.05,1.48356805183873,8.92757110504103));
#87424=CARTESIAN_POINT('Ctrl Pts',(2.05,1.48356805183873,8.92757110504103));
#87425=CARTESIAN_POINT('Ctrl Pts',(2.12570884457451,1.52727857363386,8.84356028415378));
#87426=CARTESIAN_POINT('Ctrl Pts',(2.2,1.57017059221718,8.76039749733631));
#87427=CARTESIAN_POINT('',(0.15,0.386602540378444,9.04173868654547));
#87428=CARTESIAN_POINT('Origin',(-0.519615242270663,0.,0.));
#87429=CARTESIAN_POINT('',(0.,0.3,8.89494238317483));
#87430=CARTESIAN_POINT('Ctrl Pts',(0.,0.3,8.89494238317483));
#87431=CARTESIAN_POINT('Ctrl Pts',(0.0743861895232588,0.342946886545244,
8.96792239730301));
#87432=CARTESIAN_POINT('Ctrl Pts',(0.15,0.386602540378444,9.04173868654547));
#87433=CARTESIAN_POINT('',(0.,0.3,5.59195851200633));
#87434=CARTESIAN_POINT('',(5.55111512312578E-16,0.299999999999999,0.));
#87435=CARTESIAN_POINT('Ctrl Pts',(0.5,0.588675134594813,5.06591172306721));
#87436=CARTESIAN_POINT('Ctrl Pts',(0.262339397490468,0.451461721760166,
5.32111616952063));
#87437=CARTESIAN_POINT('Ctrl Pts',(0.,0.3,5.59195851200633));
#87438=CARTESIAN_POINT('Origin',(-0.2,-0.415470053837925,0.));
#87439=CARTESIAN_POINT('',(1.7,0.681495457622364,5.05426195811417));
#87440=CARTESIAN_POINT('',(2.2,0.970170592217176,5.51532129816541));
#87441=CARTESIAN_POINT('Ctrl Pts',(1.7,0.681495457622364,5.05426195811417));
#87442=CARTESIAN_POINT('Ctrl Pts',(1.93909466606049,0.819536827434189,5.2769073690057));
#87443=CARTESIAN_POINT('Ctrl Pts',(2.2,0.970170592217177,5.51532129816541));
#87444=CARTESIAN_POINT('',(0.5,-0.0113248654051871,5.0999874262025));
#87445=CARTESIAN_POINT('Origin',(0.519615242270663,0.,0.));
#87446=CARTESIAN_POINT('',(0.,-0.3,5.59195851200633));
#87447=CARTESIAN_POINT('Ctrl Pts',(0.,-0.3,5.59195851200633));
#87448=CARTESIAN_POINT('Ctrl Pts',(0.261503310263914,-0.149020993425151,
5.33817894042));
#87449=CARTESIAN_POINT('Ctrl Pts',(0.5,-0.0113248654051871,5.0999874262025));
#87450=CARTESIAN_POINT('',(0.,-0.3,8.89494238317483));
#87451=CARTESIAN_POINT('',(2.77555756156289E-16,-0.3,0.));
#87452=CARTESIAN_POINT('Ctrl Pts',(0.15,-0.213397459621556,9.0474837122941));
#87453=CARTESIAN_POINT('Ctrl Pts',(0.0743623716417539,-0.257066864715054,
8.97079504406147));
#87454=CARTESIAN_POINT('Ctrl Pts',(0.,-0.3,8.89494238317483));
#87455=CARTESIAN_POINT('',(2.2,0.970170592217176,8.84696383071599));
#87456=CARTESIAN_POINT('Ctrl Pts',(2.2,0.970170592217176,8.84696383071599));
#87457=CARTESIAN_POINT('Ctrl Pts',(2.12567129134184,0.927256892264872,8.92644410555483));
#87458=CARTESIAN_POINT('Ctrl Pts',(2.05,0.883568051838733,9.00676454104191));
#87459=CARTESIAN_POINT('',(2.2,0.970170592217176,0.));
#87460=CARTESIAN_POINT('Origin',(0.075,0.,0.));
#87461=CARTESIAN_POINT('Origin',(0.15,0.,0.));
#87462=CARTESIAN_POINT('Origin',(0.,0.,0.));
#87463=CARTESIAN_POINT('Origin',(1.1,0.,0.));
#87464=CARTESIAN_POINT('Origin',(2.05,0.,0.));
#87465=CARTESIAN_POINT('Origin',(2.125,0.,0.));
#87466=CARTESIAN_POINT('Origin',(2.2,0.,0.));
#87467=CARTESIAN_POINT('Origin',(2.2,5.1,0.));
#87468=CARTESIAN_POINT('Origin',(2.2,0.,0.));
#87469=CARTESIAN_POINT('Origin',(1.95,0.,0.));
#87470=CARTESIAN_POINT('Origin',(1.7,0.,0.));
#87471=CARTESIAN_POINT('Origin',(1.1,0.,0.));
#87472=CARTESIAN_POINT('Origin',(0.5,0.,0.));
#87473=CARTESIAN_POINT('Origin',(0.25,0.,0.));
#87474=CARTESIAN_POINT('Origin',(0.,0.,0.));
#87475=CARTESIAN_POINT('Origin',(0.,9.05,0.));
#87476=CARTESIAN_POINT('',(0.,0.,0.));
#87477=CARTESIAN_POINT('Origin',(-7.7,0.,0.));
#87478=CARTESIAN_POINT('',(-15.1358238829104,-2.94538307225005,0.00197110619363838));
#87479=CARTESIAN_POINT('',(-15.2801761170896,-2.94466557400741,0.00313752023776137));
#87480=CARTESIAN_POINT('',(-7.7,-2.942,-3.60291088309151E-16));
#87481=CARTESIAN_POINT('',(-15.458,1.29046914982061,2.6465053321022));
#87482=CARTESIAN_POINT('Ctrl Pts',(-15.1358238829104,-2.94538307225005,
0.00197110619363838));
#87483=CARTESIAN_POINT('Ctrl Pts',(-15.1415696469556,-2.9461379076381,0.107826186325021));
#87484=CARTESIAN_POINT('Ctrl Pts',(-15.1473154110008,-2.94092576030921,
0.213601568550446));
#87485=CARTESIAN_POINT('Ctrl Pts',(-15.153061175046,-2.92950004699259,0.31869564336318));
#87486=CARTESIAN_POINT('Ctrl Pts',(-15.2059089097093,-2.82440992130234,
1.28531796490334));
#87487=CARTESIAN_POINT('Ctrl Pts',(-15.2587566443725,-2.19366807307829,
2.19430342932105));
#87488=CARTESIAN_POINT('Ctrl Pts',(-15.3116043790358,-1.32498508042342,
2.63183072499184));
#87489=CARTESIAN_POINT('Ctrl Pts',(-15.3604029193572,-0.522860593656641,
3.03583467171792));
#87490=CARTESIAN_POINT('Ctrl Pts',(-15.4092014596786,0.48213979207355,3.03785896067201));
#87491=CARTESIAN_POINT('Ctrl Pts',(-15.458,1.29201644558801,2.64838508500723));
#87492=CARTESIAN_POINT('',(-15.458,-1.28892185405329,2.64462557919714));
#87493=CARTESIAN_POINT('Origin',(-15.458,0.,0.));
#87494=CARTESIAN_POINT('Ctrl Pts',(-15.458,-1.28892185405329,2.64462557919715));
#87495=CARTESIAN_POINT('Ctrl Pts',(-15.4051522653367,-2.16707535766418,
2.21663635799285));
#87496=CARTESIAN_POINT('Ctrl Pts',(-15.3523045306734,-2.80781137912627,
1.32067398609183));
#87497=CARTESIAN_POINT('Ctrl Pts',(-15.2994567960101,-2.92486432853091,
0.356906459573303));
#87498=CARTESIAN_POINT('Ctrl Pts',(-15.2930299030366,-2.93909931481463,
0.239701232447736));
#87499=CARTESIAN_POINT('Ctrl Pts',(-15.2866030100631,-2.94558936356448,
0.121493210473513));
#87500=CARTESIAN_POINT('Ctrl Pts',(-15.2801761170896,-2.94466557400741,
0.00313752023776137));
#87501=CARTESIAN_POINT('Origin',(-7.7,0.,0.));
#87502=CARTESIAN_POINT('',(-14.1358238829104,-2.93775688134926,0.00129066909678663));
#87503=CARTESIAN_POINT('',(-14.2801761170896,-2.93759521907236,0.00112342388299112));
#87504=CARTESIAN_POINT('',(-7.7,-2.942,-3.60291088309151E-16));
#87505=CARTESIAN_POINT('Ctrl Pts',(-14.1358238829104,-2.93775688134926,
0.00129066909678663));
#87506=CARTESIAN_POINT('Ctrl Pts',(-14.1578165723092,-2.93937115251897,
0.409195620159363));
#87507=CARTESIAN_POINT('Ctrl Pts',(-14.1798092617081,-2.86019584296587,
0.816500692953316));
#87508=CARTESIAN_POINT('Ctrl Pts',(-14.2018019511069,-2.69719296954668,
1.18691526487588));
#87509=CARTESIAN_POINT('Ctrl Pts',(-14.2546496857702,-2.30550223779513,
2.07700972569356));
#87510=CARTESIAN_POINT('Ctrl Pts',(-14.3074974204334,-1.42976965241086,
2.75408897290262));
#87511=CARTESIAN_POINT('Ctrl Pts',(-14.3603451550967,-0.469734389951471,
2.90911082424985));
#87512=CARTESIAN_POINT('Ctrl Pts',(-14.41319288976,0.490300872507907,3.06413267559709));
#87513=CARTESIAN_POINT('Ctrl Pts',(-14.4660406244233,1.53463881204239,2.6970971310825));
#87514=CARTESIAN_POINT('Ctrl Pts',(-14.5188883590866,2.18656529744424,1.97550114427565));
#87515=CARTESIAN_POINT('Ctrl Pts',(-14.5717360937499,2.83849178284608,1.25390515746879));
#87516=CARTESIAN_POINT('Ctrl Pts',(-14.6245838284131,3.09800681411528,0.177748728369656));
#87517=CARTESIAN_POINT('Ctrl Pts',(-14.6774315630764,2.84666544889829,-0.761656087067673));
#87518=CARTESIAN_POINT('Ctrl Pts',(-14.7302792977397,2.59532408368129,-1.701060902505));
#87519=CARTESIAN_POINT('Ctrl Pts',(-14.783127032403,1.83312632197811,-2.50371410428052));
#87520=CARTESIAN_POINT('Ctrl Pts',(-14.8359747670663,0.907961517914752,
-2.80338699340931));
#87521=CARTESIAN_POINT('Ctrl Pts',(-14.8888225017296,-0.0172032861486045,
-3.10305988253811));
#87522=CARTESIAN_POINT('Ctrl Pts',(-14.9416702363928,-1.10533513257213,
-2.89975245902016));
#87523=CARTESIAN_POINT('Ctrl Pts',(-14.9945179710561,-1.85968185420569,
-2.28596915792989));
#87524=CARTESIAN_POINT('Ctrl Pts',(-15.0416199416742,-2.53201374022922,
-1.73891821623806));
#87525=CARTESIAN_POINT('Ctrl Pts',(-15.0887219122923,-2.93919516860669,
-0.865795623332123));
#87526=CARTESIAN_POINT('Ctrl Pts',(-15.1358238829104,-2.94538307225005,
0.00197110619363838));
#87527=CARTESIAN_POINT('Ctrl Pts',(-15.2801761170896,-2.94466557400741,
0.00313752023776137));
#87528=CARTESIAN_POINT('Ctrl Pts',(-15.2337552753998,-2.93799312917907,
-0.851734465675268));
#87529=CARTESIAN_POINT('Ctrl Pts',(-15.1873344337101,-2.54453802420963,
-1.71431035888275));
#87530=CARTESIAN_POINT('Ctrl Pts',(-15.1409135920203,-1.88906561096285,
-2.26235996115331));
#87531=CARTESIAN_POINT('Ctrl Pts',(-15.088065857357,-1.14284406664301,-2.88628617422528));
#87532=CARTESIAN_POINT('Ctrl Pts',(-15.0352181226937,-0.0570311006561663,
-3.10256591923317));
#87533=CARTESIAN_POINT('Ctrl Pts',(-14.9823703880304,0.871996126213134,
-2.81455814367286));
#87534=CARTESIAN_POINT('Ctrl Pts',(-14.9295226533672,1.80102335308244,-2.52655036811256));
#87535=CARTESIAN_POINT('Ctrl Pts',(-14.8766749187039,2.5732648408342,-1.73425507198407));
#87536=CARTESIAN_POINT('Ctrl Pts',(-14.8238271840406,2.83659880862163,-0.798275641797322));
#87537=CARTESIAN_POINT('Ctrl Pts',(-14.7709794493773,3.09993277640907,0.137703788389426));
#87538=CARTESIAN_POINT('Ctrl Pts',(-14.718131714714,2.85435922423218,1.21736735263443));
#87539=CARTESIAN_POINT('Ctrl Pts',(-14.6652839800507,2.21177553304593,1.9473366320817));
#87540=CARTESIAN_POINT('Ctrl Pts',(-14.6124362453875,1.56919184185968,2.67730591152896));
#87541=CARTESIAN_POINT('Ctrl Pts',(-14.5595885107242,0.529598011664078,
3.05758090617849));
#87542=CARTESIAN_POINT('Ctrl Pts',(-14.5067407760609,-0.432361259668386,
2.9148644525704));
#87543=CARTESIAN_POINT('Ctrl Pts',(-14.4538930413976,-1.39432053100085,
2.7721479989623));
#87544=CARTESIAN_POINT('Ctrl Pts',(-14.4010453067343,-2.27864524347017,
2.10644009709658));
#87545=CARTESIAN_POINT('Ctrl Pts',(-14.348197572071,-2.68172448593006,1.22146505496284));
#87546=CARTESIAN_POINT('Ctrl Pts',(-14.3255237537439,-2.85466180430726,
0.841774923356542));
#87547=CARTESIAN_POINT('Ctrl Pts',(-14.3028499354168,-2.93901350293065,
0.421723028943609));
#87548=CARTESIAN_POINT('Ctrl Pts',(-14.2801761170896,-2.93759521907236,
0.00112342388299112));
#87549=CARTESIAN_POINT('Origin',(-7.7,0.,0.));
#87550=CARTESIAN_POINT('',(-13.1358238829104,-2.94074805441212,-0.00260717695666907));
#87551=CARTESIAN_POINT('',(-13.2801761170896,-2.94111110959967,-0.00264487064251058));
#87552=CARTESIAN_POINT('',(-7.7,-2.942,-3.60291088309151E-16));
#87553=CARTESIAN_POINT('Ctrl Pts',(-13.1358238829104,-2.94074805441212,
-0.00260717695666907));
#87554=CARTESIAN_POINT('Ctrl Pts',(-13.1740634976629,-2.93465880245723,
0.704816327991579));
#87555=CARTESIAN_POINT('Ctrl Pts',(-13.2123031124153,-2.6782697242631,1.41619979630778));
#87556=CARTESIAN_POINT('Ctrl Pts',(-13.2505427271678,-2.21386422561743,
1.94484407522698));
#87557=CARTESIAN_POINT('Ctrl Pts',(-13.3033904618311,-1.572048696683,2.67543858472817));
#87558=CARTESIAN_POINT('Ctrl Pts',(-13.3562381964943,-0.53292878682618,
3.05700737618249));
#87559=CARTESIAN_POINT('Ctrl Pts',(-13.4090859311576,0.429171271208409,
2.91537721181919));
#87560=CARTESIAN_POINT('Ctrl Pts',(-13.4619336658209,1.391271329243,2.77374704745589));
#87561=CARTESIAN_POINT('Ctrl Pts',(-13.5147814004842,2.27635153545535,2.10891792727497));
#87562=CARTESIAN_POINT('Ctrl Pts',(-13.5676291351475,2.680401504673,1.22436176363895));
#87563=CARTESIAN_POINT('Ctrl Pts',(-13.6204768698108,3.08445147389065,0.339805600002934));
#87564=CARTESIAN_POINT('Ctrl Pts',(-13.673324604474,3.00747120611361,-0.764477607088176));
#87565=CARTESIAN_POINT('Ctrl Pts',(-13.7261723391373,2.48459999269888,-1.58441694249922));
#87566=CARTESIAN_POINT('Ctrl Pts',(-13.7790200738006,1.96172877928415,-2.40435627791026));
#87567=CARTESIAN_POINT('Ctrl Pts',(-13.8318678084639,0.992966620231722,
-2.93995174164124));
#87568=CARTESIAN_POINT('Ctrl Pts',(-13.8847155431272,0.0205212209196415,
-2.94672469674374));
#87569=CARTESIAN_POINT('Ctrl Pts',(-13.9375632777905,-0.951924178392424,
-2.95349765184624));
#87570=CARTESIAN_POINT('Ctrl Pts',(-13.9904110124537,-1.92805281796414,
-2.43144809832029));
#87571=CARTESIAN_POINT('Ctrl Pts',(-14.043258747117,-2.46229269869059,-1.61886848434418));
#87572=CARTESIAN_POINT('Ctrl Pts',(-14.0741137923815,-2.77420759545808,
-1.14444548532719));
#87573=CARTESIAN_POINT('Ctrl Pts',(-14.1049688376459,-2.93549211012882,
-0.570987031933492));
#87574=CARTESIAN_POINT('Ctrl Pts',(-14.1358238829104,-2.93775688134926,
0.00129066909678663));
#87575=CARTESIAN_POINT('Ctrl Pts',(-14.2801761170896,-2.93759521907236,
0.00112342388299112));
#87576=CARTESIAN_POINT('Ctrl Pts',(-14.2500022007535,-2.93570779200279,
-0.558603090240103));
#87577=CARTESIAN_POINT('Ctrl Pts',(-14.2198282844173,-2.78192330778483,
-1.11929958981901));
#87578=CARTESIAN_POINT('Ctrl Pts',(-14.1896543680812,-2.48287763479889,
-1.58713267790547));
#87579=CARTESIAN_POINT('Ctrl Pts',(-14.1368066334179,-1.95911776875739,
-2.40651318623828));
#87580=CARTESIAN_POINT('Ctrl Pts',(-14.0839588987546,-0.98976426422395,
-2.94103202050213));
#87581=CARTESIAN_POINT('Ctrl Pts',(-14.0311111640913,-0.0173102695312365,
-2.9467397656718));
#87582=CARTESIAN_POINT('Ctrl Pts',(-13.9782634294281,0.95514372516147,-2.95244751084146));
#87583=CARTESIAN_POINT('Ctrl Pts',(-13.9254156947648,1.93069821001345,-2.42934416691693));
#87584=CARTESIAN_POINT('Ctrl Pts',(-13.8725679601015,2.4640522158048,-1.61618788323316));
#87585=CARTESIAN_POINT('Ctrl Pts',(-13.8197202254382,2.99740622159616,-0.803031599549377));
#87586=CARTESIAN_POINT('Ctrl Pts',(-13.7668724907749,3.08855974832689,0.30017762389366));
#87587=CARTESIAN_POINT('Ctrl Pts',(-13.7140247561116,2.69590010018066,1.1898495617677));
#87588=CARTESIAN_POINT('Ctrl Pts',(-13.6611770214484,2.30324045203443,2.07952149964175));
#87589=CARTESIAN_POINT('Ctrl Pts',(-13.6083292867851,1.42676762901126,2.7556561519468));
#87590=CARTESIAN_POINT('Ctrl Pts',(-13.5554815521218,0.466565002411474,
2.90962599796443));
#87591=CARTESIAN_POINT('Ctrl Pts',(-13.5026338174585,-0.493637624188301,
3.06359584398207));
#87592=CARTESIAN_POINT('Ctrl Pts',(-13.4497860827952,-1.53757005436468,
2.69540088371229));
#87593=CARTESIAN_POINT('Ctrl Pts',(-13.3969383481319,-2.18871233098836,
1.9731070214835));
#87594=CARTESIAN_POINT('Ctrl Pts',(-13.3580176044512,-2.6682587450335,1.44115963616757));
#87595=CARTESIAN_POINT('Ctrl Pts',(-13.3190968607704,-2.93476077004709,
0.717153505126285));
#87596=CARTESIAN_POINT('Ctrl Pts',(-13.2801761170896,-2.94111110959967,
-0.00264487064251058));
#87597=CARTESIAN_POINT('Origin',(-7.7,0.,0.));
#87598=CARTESIAN_POINT('',(-12.1358238829104,-2.94666731984368,0.000555183168313277));
#87599=CARTESIAN_POINT('',(-12.2801761170896,-2.9465427897585,0.000779102665135559));
#87600=CARTESIAN_POINT('',(-7.7,-2.942,-3.60291088309151E-16));
#87601=CARTESIAN_POINT('Ctrl Pts',(-12.1358238829104,-2.94666731984368,
0.000555183168313277));
#87602=CARTESIAN_POINT('Ctrl Pts',(-12.1374626883532,-2.94674572763455,
0.0307149631628695));
#87603=CARTESIAN_POINT('Ctrl Pts',(-12.139101493796,-2.94632262466987,0.0608724894688986));
#87604=CARTESIAN_POINT('Ctrl Pts',(-12.1407402992388,-2.94539122482773,
0.0910143091064779));
#87605=CARTESIAN_POINT('Ctrl Pts',(-12.1935880339021,-2.91535570600564,
1.06301918831248));
#87606=CARTESIAN_POINT('Ctrl Pts',(-12.2464357685654,-2.35673450139353,
2.01869046311919));
#87607=CARTESIAN_POINT('Ctrl Pts',(-12.2992835032287,-1.52451995638186,
2.52179538823306));
#87608=CARTESIAN_POINT('Ctrl Pts',(-12.352131237892,-0.692305411370191,
3.02490031334693));
#87609=CARTESIAN_POINT('Ctrl Pts',(-12.4049789725552,0.413502474041036,
3.07543888876795));
#87610=CARTESIAN_POINT('Ctrl Pts',(-12.4578267072185,1.28813849951715,2.65034191401869));
#87611=CARTESIAN_POINT('Ctrl Pts',(-12.5106744418818,2.16277452499326,2.22524493926943));
#87612=CARTESIAN_POINT('Ctrl Pts',(-12.5635221765451,2.80623869053425,1.32451241434988));
#87613=CARTESIAN_POINT('Ctrl Pts',(-12.6163699112084,2.9248106062348,0.359299315654169));
#87614=CARTESIAN_POINT('Ctrl Pts',(-12.6692176458717,3.04338252193535,-0.605913783041536));
#87615=CARTESIAN_POINT('Ctrl Pts',(-12.7220653805349,2.63706218779547,-1.63560745551341));
#87616=CARTESIAN_POINT('Ctrl Pts',(-12.7749131151982,1.89132157897925,-2.25976011876333));
#87617=CARTESIAN_POINT('Ctrl Pts',(-12.8277608498615,1.14558097016303,-2.88391278201326));
#87618=CARTESIAN_POINT('Ctrl Pts',(-12.8806085845248,0.0604200866704679,
-3.10252443604124));
#87619=CARTESIAN_POINT('Ctrl Pts',(-12.9334563191881,-0.868820564034781,
-2.81580606293874));
#87620=CARTESIAN_POINT('Ctrl Pts',(-12.9863040538514,-1.79806121474003,
-2.52908768983624));
#87621=CARTESIAN_POINT('Ctrl Pts',(-13.0391517885146,-2.57138163265797,
-1.73703928960327));
#87622=CARTESIAN_POINT('Ctrl Pts',(-13.0919995231779,-2.83578626761092,
-0.801204975712751));
#87623=CARTESIAN_POINT('Ctrl Pts',(-13.1066076430888,-2.90887274212077,
-0.542522556095674));
#87624=CARTESIAN_POINT('Ctrl Pts',(-13.1212157629996,-2.9430742421444,-0.272853816597777));
#87625=CARTESIAN_POINT('Ctrl Pts',(-13.1358238829104,-2.94074805441212,
-0.00260717695666907));
#87626=CARTESIAN_POINT('Ctrl Pts',(-13.2801761170896,-2.94111110959967,
-0.00264487064251058));
#87627=CARTESIAN_POINT('Ctrl Pts',(-13.2662491261071,-2.94338344854597,
-0.260209977074633));
#87628=CARTESIAN_POINT('Ctrl Pts',(-13.2523221351246,-2.91234545461203,
-0.517236314255438));
#87629=CARTESIAN_POINT('Ctrl Pts',(-13.2383951441421,-2.84583880363258,
-0.764731501724886));
#87630=CARTESIAN_POINT('Ctrl Pts',(-13.1855474094788,-2.59347087658213,
-1.70388339851668));
#87631=CARTESIAN_POINT('Ctrl Pts',(-13.1326996748155,-1.83038289941027,
-2.50579442791246));
#87632=CARTESIAN_POINT('Ctrl Pts',(-13.0798519401522,-0.904899930405956,
-2.80441922491318));
#87633=CARTESIAN_POINT('Ctrl Pts',(-13.027004205489,0.0205830385983635,
-3.10304402191389));
#87634=CARTESIAN_POINT('Ctrl Pts',(-12.9741564708257,1.10846099943515,-2.89838258651955));
#87635=CARTESIAN_POINT('Ctrl Pts',(-12.9213087361624,1.86215333580489,-2.28385574206214));
#87636=CARTESIAN_POINT('Ctrl Pts',(-12.8684610014991,2.61584567217464,-1.66932889760473));
#87637=CARTESIAN_POINT('Ctrl Pts',(-12.8156132668358,3.03535238407735,-0.64493664408427));
#87638=CARTESIAN_POINT('Ctrl Pts',(-12.7627655321725,2.92918226774181,0.321719163828909));
#87639=CARTESIAN_POINT('Ctrl Pts',(-12.7099177975092,2.82301215140626,1.28837497174208));
#87640=CARTESIAN_POINT('Ctrl Pts',(-12.657070062846,2.19116520683245,2.19729433404797));
#87641=CARTESIAN_POINT('Ctrl Pts',(-12.6042223281827,1.32205898240464,2.6335853531165));
#87642=CARTESIAN_POINT('Ctrl Pts',(-12.5513745935194,0.45295275797683,3.06987637218503));
#87643=CARTESIAN_POINT('Ctrl Pts',(-12.4985268588561,-0.653412746304991,
3.03353904801619));
#87644=CARTESIAN_POINT('Ctrl Pts',(-12.4456791241928,-1.49201781655651,
2.54116011967247));
#87645=CARTESIAN_POINT('Ctrl Pts',(-12.3928313895296,-2.33062288680803,
2.04878119132876));
#87646=CARTESIAN_POINT('Ctrl Pts',(-12.3399836548663,-2.90146752302926,
1.10036065881016));
#87647=CARTESIAN_POINT('Ctrl Pts',(-12.287135920203,-2.94397977118869,0.128821568406056));
#87648=CARTESIAN_POINT('Ctrl Pts',(-12.2848159858319,-2.94584599357887,
0.0861724947403499));
#87649=CARTESIAN_POINT('Ctrl Pts',(-12.2824960514607,-2.94669407976322,
0.0434788698766825));
#87650=CARTESIAN_POINT('Ctrl Pts',(-12.2801761170896,-2.9465427897585,0.000779102665135559));
#87651=CARTESIAN_POINT('Origin',(-7.7,0.,0.));
#87652=CARTESIAN_POINT('',(-11.1358238829104,-2.93916360235934,0.00220716881453697));
#87653=CARTESIAN_POINT('',(-11.2801761170896,-2.93887905319533,0.00208280935630314));
#87654=CARTESIAN_POINT('',(-7.7,-2.942,-3.60291088309151E-16));
#87655=CARTESIAN_POINT('Ctrl Pts',(-11.1358238829104,-2.93916360235934,
0.00220716881453697));
#87656=CARTESIAN_POINT('Ctrl Pts',(-11.1537096137068,-2.94148269897771,
0.333540081468947));
#87657=CARTESIAN_POINT('Ctrl Pts',(-11.1715953445033,-2.88977704335533,
0.664170570633947));
#87658=CARTESIAN_POINT('Ctrl Pts',(-11.1894810752997,-2.78090778079409,
0.974764066720982));
#87659=CARTESIAN_POINT('Ctrl Pts',(-11.242328809963,-2.45922710884912,1.89248796943232));
#87660=CARTESIAN_POINT('Ctrl Pts',(-11.2951765446263,-1.63847927291341,
2.63527880115994));
#87661=CARTESIAN_POINT('Ctrl Pts',(-11.3480242792896,-0.693308867908512,
2.86407679451984));
#87662=CARTESIAN_POINT('Ctrl Pts',(-11.4008720139528,0.251861537096377,
3.09287478787973));
#87663=CARTESIAN_POINT('Ctrl Pts',(-11.4537197486161,1.32145451117044,2.80767994287192));
#87664=CARTESIAN_POINT('Ctrl Pts',(-11.5065674832794,2.02723577709945,2.13867439663664));
#87665=CARTESIAN_POINT('Ctrl Pts',(-11.5594152179427,2.73301704302846,1.46966885040136));
#87666=CARTESIAN_POINT('Ctrl Pts',(-11.612262952606,3.07498660081242,0.416852602938626));
#87667=CARTESIAN_POINT('Ctrl Pts',(-11.6651106872693,2.89704651038734,-0.539198096916202));
#87668=CARTESIAN_POINT('Ctrl Pts',(-11.7179584219326,2.71910641996226,-1.49524879677103));
#87669=CARTESIAN_POINT('Ctrl Pts',(-11.7708061565958,2.02125668132815,-2.35453394901796));
#87670=CARTESIAN_POINT('Ctrl Pts',(-11.8236538912591,1.12204291994308,-2.72481793114896));
#87671=CARTESIAN_POINT('Ctrl Pts',(-11.8765016259224,0.22282915855803,-3.09510191327996));
#87672=CARTESIAN_POINT('Ctrl Pts',(-11.9293493605857,-0.877748625577962,
-2.97638472529505));
#87673=CARTESIAN_POINT('Ctrl Pts',(-11.982197095249,-1.67731260112992,-2.42285688949995));
#87674=CARTESIAN_POINT('Ctrl Pts',(-12.0334060244694,-2.45208214030059,
-1.88649392247026));
#87675=CARTESIAN_POINT('Ctrl Pts',(-12.0846149536899,-2.94421725535864,
-0.941869096557914));
#87676=CARTESIAN_POINT('Ctrl Pts',(-12.1358238829104,-2.94666731984368,
0.000555183168313277));
#87677=CARTESIAN_POINT('Ctrl Pts',(-12.2801761170896,-2.9465427897585,0.000779102665135559));
#87678=CARTESIAN_POINT('Ctrl Pts',(-12.2296483167974,-2.94324771760488,
-0.929215011409908));
#87679=CARTESIAN_POINT('Ctrl Pts',(-12.1791205165053,-2.46588711038851,
-1.86212281851241));
#87680=CARTESIAN_POINT('Ctrl Pts',(-12.1285927162131,-1.70828039271164,
-2.40112264659498));
#87681=CARTESIAN_POINT('Ctrl Pts',(-12.0757449815499,-0.915888905977512,
-2.96487012290226));
#87682=CARTESIAN_POINT('Ctrl Pts',(-12.0228972468866,0.183073927588378,
-3.0977074272272));
#87683=CARTESIAN_POINT('Ctrl Pts',(-11.9700495122233,1.08696745191729,-2.73899865737196));
#87684=CARTESIAN_POINT('Ctrl Pts',(-11.91720177756,1.9908609762462,-2.38028988751671));
#87685=CARTESIAN_POINT('Ctrl Pts',(-11.8643540428967,2.69968519133814,-1.53003504348128));
#87686=CARTESIAN_POINT('Ctrl Pts',(-11.8115063082334,2.88988497988314,-0.576347710895525));
#87687=CARTESIAN_POINT('Ctrl Pts',(-11.7586585735702,3.08008476842813,0.37733962169024));
#87688=CARTESIAN_POINT('Ctrl Pts',(-11.7058108389069,2.75166013042619,1.43445944282634));
#87689=CARTESIAN_POINT('Ctrl Pts',(-11.6529631042436,2.05452619305162,2.11247106489354));
#87690=CARTESIAN_POINT('Ctrl Pts',(-11.6001153695803,1.35739225567705,2.79048268696074));
#87691=CARTESIAN_POINT('Ctrl Pts',(-11.547267634917,0.291549018929873,3.08938610995905));
#87692=CARTESIAN_POINT('Ctrl Pts',(-11.4944199002537,-0.656480873097509,
2.87274167728717));
#87693=CARTESIAN_POINT('Ctrl Pts',(-11.4415721655904,-1.6045107651249,2.65609724461528));
#87694=CARTESIAN_POINT('Ctrl Pts',(-11.3887244309272,-2.43472731243248,
1.92390495627319));
#87695=CARTESIAN_POINT('Ctrl Pts',(-11.3358766962639,-2.76816376222187,
1.0103866911436));
#87696=CARTESIAN_POINT('Ctrl Pts',(-11.3173098365391,-2.88530913902571,
0.689442650822292));
#87697=CARTESIAN_POINT('Ctrl Pts',(-11.2987429768144,-2.94113646385435,
0.346117368328329));
#87698=CARTESIAN_POINT('Ctrl Pts',(-11.2801761170896,-2.93887905319533,
0.00208280935630314));
#87699=CARTESIAN_POINT('Origin',(-7.7,0.,0.));
#87700=CARTESIAN_POINT('',(-10.1358238829104,-2.93881981982172,-0.00205406958497051));
#87701=CARTESIAN_POINT('',(-10.2801761170896,-2.93909999412443,-0.00218120945484637));
#87702=CARTESIAN_POINT('',(-7.7,-2.942,-3.60291088309151E-16));
#87703=CARTESIAN_POINT('Ctrl Pts',(-10.1358238829104,-2.93881981982172,
-0.00205406958497051));
#87704=CARTESIAN_POINT('Ctrl Pts',(-10.1699565390605,-2.93473247363868,
0.63043906752137));
#87705=CARTESIAN_POINT('Ctrl Pts',(-10.2040891952105,-2.7344359265845,1.2652927625898));
#87706=CARTESIAN_POINT('Ctrl Pts',(-10.2382218513606,-2.35764221671594,
1.76780548958973));
#87707=CARTESIAN_POINT('Ctrl Pts',(-10.2910695860239,-1.77425093552235,
2.54584805225045));
#87708=CARTESIAN_POINT('Ctrl Pts',(-10.3439173206872,-0.7677525585416,3.00663677490463));
#87709=CARTESIAN_POINT('Ctrl Pts',(-10.3967650553505,0.202419260911082,
2.93983664748256));
#87710=CARTESIAN_POINT('Ctrl Pts',(-10.4496127900137,1.17259108036376,2.87303652006049));
#87711=CARTESIAN_POINT('Ctrl Pts',(-10.502460524677,2.10643634228836,2.27864754256218));
#87712=CARTESIAN_POINT('Ctrl Pts',(-10.5553082593403,2.57768516873133,1.42798888019613));
#87713=CARTESIAN_POINT('Ctrl Pts',(-10.6081559940036,3.0489339951743,0.577330217830078));
#87714=CARTESIAN_POINT('Ctrl Pts',(-10.6610037286669,3.05758638613563,-0.529598129403716));
#87715=CARTESIAN_POINT('Ctrl Pts',(-10.7138514633302,2.59969280758565,-1.38751950517789));
#87716=CARTESIAN_POINT('Ctrl Pts',(-10.7666991979934,2.14179922903567,-2.24544088095207));
#87717=CARTESIAN_POINT('Ctrl Pts',(-10.8195469326567,1.21735968097438,-2.85435528526663));
#87718=CARTESIAN_POINT('Ctrl Pts',(-10.87239466732,0.248350640016974,-2.93631316972379));
#87719=CARTESIAN_POINT('Ctrl Pts',(-10.9252424019833,-0.720658400940432,
-3.01827105418095));
#87720=CARTESIAN_POINT('Ctrl Pts',(-10.9780901366466,-1.73423693479395,
-2.5732724187807));
#87721=CARTESIAN_POINT('Ctrl Pts',(-11.0309378713099,-2.3297194477436,-1.80444461423305));
#87722=CARTESIAN_POINT('Ctrl Pts',(-11.0658998751767,-2.72366749590564,
-1.29581806956093));
#87723=CARTESIAN_POINT('Ctrl Pts',(-11.1008618790436,-2.93463036489413,
-0.645463463449812));
#87724=CARTESIAN_POINT('Ctrl Pts',(-11.1358238829104,-2.93916360235934,
0.00220716881453697));
#87725=CARTESIAN_POINT('Ctrl Pts',(-11.2801761170896,-2.93887905319533,
0.00208280935630314));
#87726=CARTESIAN_POINT('Ctrl Pts',(-11.2458952421511,-2.9347110886804,-0.633124536715663));
#87727=CARTESIAN_POINT('Ctrl Pts',(-11.2116143672126,-2.73253231482323,
-1.27074980564275));
#87728=CARTESIAN_POINT('Ctrl Pts',(-11.177333492274,-2.35269386222101,-1.77438537823672));
#87729=CARTESIAN_POINT('Ctrl Pts',(-11.1244857576107,-1.76713116015959,
-2.55079494057035));
#87730=CARTESIAN_POINT('Ctrl Pts',(-11.0716380229475,-0.759349403765581,
-3.00876982332051));
#87731=CARTESIAN_POINT('Ctrl Pts',(-11.0187902882842,0.210631932906051,
-2.93925944229535));
#87732=CARTESIAN_POINT('Ctrl Pts',(-10.9659425536209,1.18061326957769,-2.86974906127019));
#87733=CARTESIAN_POINT('Ctrl Pts',(-10.9130948189576,2.11279418652695,-2.27275341646971));
#87734=CARTESIAN_POINT('Ctrl Pts',(-10.8602470842943,2.58166452491497,-1.42078153172831));
#87735=CARTESIAN_POINT('Ctrl Pts',(-10.807399349631,3.05053486330299,-0.568809646986925));
#87736=CARTESIAN_POINT('Ctrl Pts',(-10.7545516149678,3.05609462312976,0.538138477695383));
#87737=CARTESIAN_POINT('Ctrl Pts',(-10.7017038803045,2.5958059555438,1.39477715827506));
#87738=CARTESIAN_POINT('Ctrl Pts',(-10.6488561456412,2.13551728795784,2.25141583885473));
#87739=CARTESIAN_POINT('Ctrl Pts',(-10.5960084109779,1.20938019295914,2.85774507533179));
#87740=CARTESIAN_POINT('Ctrl Pts',(-10.5431606763146,0.240146021913272,
2.93699536402476));
#87741=CARTESIAN_POINT('Ctrl Pts',(-10.4903129416513,-0.729088149132603,
3.01624565271774));
#87742=CARTESIAN_POINT('Ctrl Pts',(-10.437465206988,-1.74141939622565,2.56841699362663));
#87743=CARTESIAN_POINT('Ctrl Pts',(-10.3846174723248,-2.3347515512458,1.79792855088024));
#87744=CARTESIAN_POINT('Ctrl Pts',(-10.3498036872464,-2.72561292414242,
1.29036433413454));
#87745=CARTESIAN_POINT('Ctrl Pts',(-10.314989902168,-2.93464543616332,0.642778666215291));
#87746=CARTESIAN_POINT('Ctrl Pts',(-10.2801761170896,-2.93909999412443,
-0.00218120945484637));
#87747=CARTESIAN_POINT('Origin',(-7.7,0.,0.));
#87748=CARTESIAN_POINT('',(-9.1358238829104,-2.94651094858123,-0.000827005293144168));
#87749=CARTESIAN_POINT('',(-9.28017611708961,-2.94664335289425,-0.000604394974247732));
#87750=CARTESIAN_POINT('',(-7.7,-2.942,-3.60291088309151E-16));
#87751=CARTESIAN_POINT('Ctrl Pts',(-9.1358238829104,-2.94651094858123,-0.000827005293144167));
#87752=CARTESIAN_POINT('Ctrl Pts',(-9.18620346441409,-2.94304481294294,
0.926466056987759));
#87753=CARTESIAN_POINT('Ctrl Pts',(-9.23658304591779,-2.46886221095953,
1.85681365907283));
#87754=CARTESIAN_POINT('Ctrl Pts',(-9.2869626274215,-1.71498223198426,2.39634075520239));
#87755=CARTESIAN_POINT('Ctrl Pts',(-9.33981036208479,-0.924168812981929,
2.96229989914274));
#87756=CARTESIAN_POINT('Ctrl Pts',(-9.39265809674808,0.174418680626146,
3.09820703168757));
#87757=CARTESIAN_POINT('Ctrl Pts',(-9.44550583141136,1.07931091990927,2.74202498333447));
#87758=CARTESIAN_POINT('Ctrl Pts',(-9.49835356607464,1.98420315919241,2.38584293498135));
#87759=CARTESIAN_POINT('Ctrl Pts',(-9.55120130073791,2.69540014415059,1.53757170573029));
#87760=CARTESIAN_POINT('Ctrl Pts',(-9.6040490354012,2.88826366721313,0.584419421068629));
#87761=CARTESIAN_POINT('Ctrl Pts',(-9.65689677006448,3.08112719027567,-0.368732863593014));
#87762=CARTESIAN_POINT('Ctrl Pts',(-9.70974450472777,2.75565725144258,-1.42676620366524));
#87763=CARTESIAN_POINT('Ctrl Pts',(-9.76259223939106,2.06042025326562,-2.1067229174712));
#87764=CARTESIAN_POINT('Ctrl Pts',(-9.81543997405434,1.36518325508866,-2.78667963127716));
#87765=CARTESIAN_POINT('Ctrl Pts',(-9.86828770871762,0.300179197567841,
-3.08855971881685));
#87766=CARTESIAN_POINT('Ctrl Pts',(-9.9211354433809,-0.648452332654128,
-2.87456477459487));
#87767=CARTESIAN_POINT('Ctrl Pts',(-9.97398317804418,-1.59708386287611,
-2.66056983037287));
#87768=CARTESIAN_POINT('Ctrl Pts',(-10.0268309127075,-2.42934286579924,
-1.93069985438918));
#87769=CARTESIAN_POINT('Ctrl Pts',(-10.0796786473708,-2.76533027455759,
-1.0181166650637));
#87770=CARTESIAN_POINT('Ctrl Pts',(-10.098393725884,-2.88431419646887,-0.694941676639214));
#87771=CARTESIAN_POINT('Ctrl Pts',(-10.1171088043972,-2.94106092887547,
-0.348852709221223));
#87772=CARTESIAN_POINT('Ctrl Pts',(-10.1358238829104,-2.93881981982172,
-0.00205406958497051));
#87773=CARTESIAN_POINT('Ctrl Pts',(-10.2801761170896,-2.93909999412443,
-0.00218120945484637));
#87774=CARTESIAN_POINT('Ctrl Pts',(-10.2621421675047,-2.94140750747045,
-0.336278000594554));
#87775=CARTESIAN_POINT('Ctrl Pts',(-10.2441082179198,-2.88881935641474,
-0.669670196702219));
#87776=CARTESIAN_POINT('Ctrl Pts',(-10.2260742683349,-2.77817338772164,
-0.982529647323611));
#87777=CARTESIAN_POINT('Ctrl Pts',(-10.1732265336716,-2.45393000623006,
-1.89935117637941));
#87778=CARTESIAN_POINT('Ctrl Pts',(-10.1203787990084,-1.63111018029966,
-2.63984600808933));
#87779=CARTESIAN_POINT('Ctrl Pts',(-10.0675310643451,-0.685304300627017,
-2.86600242422521));
#87780=CARTESIAN_POINT('Ctrl Pts',(-10.0146833296818,0.260501579045617,
-3.09215884036109));
#87781=CARTESIAN_POINT('Ctrl Pts',(-9.96183559501851,1.32929351246048,-2.80397684092295));
#87782=CARTESIAN_POINT('Ctrl Pts',(-9.90898786035523,2.03320287127863,-2.13300210134507));
#87783=CARTESIAN_POINT('Ctrl Pts',(-9.85614012569194,2.73711223009679,-1.4620273617672));
#87784=CARTESIAN_POINT('Ctrl Pts',(-9.80329239102865,3.07613901431823,-0.408259882049594));
#87785=CARTESIAN_POINT('Ctrl Pts',(-9.75044465636537,2.89552856401662,0.547289882130422));
#87786=CARTESIAN_POINT('Ctrl Pts',(-9.69759692170208,2.71491811371502,1.50283964631043));
#87787=CARTESIAN_POINT('Ctrl Pts',(-9.6447491870388,2.01467042889038,2.36017169495285));
#87788=CARTESIAN_POINT('Ctrl Pts',(-9.59190145237552,1.11442571902731,2.72794193429589));
#87789=CARTESIAN_POINT('Ctrl Pts',(-9.53905371771224,0.214181009164244,
3.09571217363894));
#87790=CARTESIAN_POINT('Ctrl Pts',(-9.48620598304895,-0.88606072573725,
2.9739206036826));
#87791=CARTESIAN_POINT('Ctrl Pts',(-9.43335824838567,-1.6840750495964,2.41816110039132));
#87792=CARTESIAN_POINT('Ctrl Pts',(-9.38229753795365,-2.45510485003712,
1.88119437422596));
#87793=CARTESIAN_POINT('Ctrl Pts',(-9.33123682752163,-2.94400105383844,
0.939112395821627));
#87794=CARTESIAN_POINT('Ctrl Pts',(-9.28017611708961,-2.94664335289425,
-0.000604394974247732));
#87795=CARTESIAN_POINT('Origin',(-7.7,0.,0.));
#87796=CARTESIAN_POINT('',(-8.1358238829104,-2.94119143690723,0.00265091043401527));
#87797=CARTESIAN_POINT('',(-8.28017611708961,-2.94082616552171,0.00261679703180889));
#87798=CARTESIAN_POINT('',(-7.7,-2.942,-3.60291088309151E-16));
#87799=CARTESIAN_POINT('Ctrl Pts',(-8.1358238829104,-2.94119143690723,0.00265091043401527));
#87800=CARTESIAN_POINT('Ctrl Pts',(-8.14960265510445,-2.94344974034563,
0.257457099259614));
#87801=CARTESIAN_POINT('Ctrl Pts',(-8.16338142729849,-2.91307886267284,
0.511733420342749));
#87802=CARTESIAN_POINT('Ctrl Pts',(-8.17716019949254,-2.84796435061584,
0.756777463120442));
#87803=CARTESIAN_POINT('Ctrl Pts',(-8.23000793415583,-2.5982211654136,1.69663062065564));
#87804=CARTESIAN_POINT('Ctrl Pts',(-8.28285566881911,-1.83737671270331,
2.50067101054199));
#87805=CARTESIAN_POINT('Ctrl Pts',(-8.33570340348239,-0.912731648410138,
2.80188044160635));
#87806=CARTESIAN_POINT('Ctrl Pts',(-8.38855113814568,0.0119134158830346,
3.10308987267071));
#87807=CARTESIAN_POINT('Ctrl Pts',(-8.44139887280896,1.1003590917591,2.90146834491308));
#87808=CARTESIAN_POINT('Ctrl Pts',(-8.49424660747225,1.85576545901611,2.289049504093));
#87809=CARTESIAN_POINT('Ctrl Pts',(-8.54709434213553,2.61117182627314,1.67663066327292));
#87810=CARTESIAN_POINT('Ctrl Pts',(-8.59994207679881,3.0335388849111,0.653414509390389));
#87811=CARTESIAN_POINT('Ctrl Pts',(-8.6527898114621,2.93006986026258,-0.313534184813269));
#87812=CARTESIAN_POINT('Ctrl Pts',(-8.70563754612538,2.82660083561406,-1.28048287901691));
#87813=CARTESIAN_POINT('Ctrl Pts',(-8.75848528078866,2.19729572767907,-2.19116411354167));
#87814=CARTESIAN_POINT('Ctrl Pts',(-8.81133301545195,1.32941177541667,-2.62988163278296));
#87815=CARTESIAN_POINT('Ctrl Pts',(-8.86418075011523,0.461527823154263,
-3.06859915202426));
#87816=CARTESIAN_POINT('Ctrl Pts',(-8.91702848477852,-0.644934973435559,
-3.0353529559821));
#87817=CARTESIAN_POINT('Ctrl Pts',(-8.9698762194418,-1.48491246668953,-2.54531884787264));
#87818=CARTESIAN_POINT('Ctrl Pts',(-9.02272395410509,-2.3248899599435,-2.05528473976319));
#87819=CARTESIAN_POINT('Ctrl Pts',(-9.07557168876836,-2.89838214986163,
-1.10846271958645));
#87820=CARTESIAN_POINT('Ctrl Pts',(-9.12841942343164,-2.9436085726224,-0.137046131830142));
#87821=CARTESIAN_POINT('Ctrl Pts',(-9.13088757659123,-2.94572078687236,
-0.0916779635326883));
#87822=CARTESIAN_POINT('Ctrl Pts',(-9.13335572975081,-2.94668075851954,
-0.0462561500620593));
#87823=CARTESIAN_POINT('Ctrl Pts',(-9.1358238829104,-2.94651094858123,-0.000827005293144167));
#87824=CARTESIAN_POINT('Ctrl Pts',(-9.28017611708961,-2.94664335289425,
-0.000604394974247732));
#87825=CARTESIAN_POINT('Ctrl Pts',(-9.27838909285835,-2.94673582815359,
-0.033492630595535));
#87826=CARTESIAN_POINT('Ctrl Pts',(-9.27660206862708,-2.94623270946163,
-0.0663779691882953));
#87827=CARTESIAN_POINT('Ctrl Pts',(-9.27481504439582,-2.94512524663853,
-0.099242942979859));
#87828=CARTESIAN_POINT('Ctrl Pts',(-9.22196730973253,-2.9123742070047,-1.07116004643351));
#87829=CARTESIAN_POINT('Ctrl Pts',(-9.16911957506925,-2.35108521492026,
-2.02526681671459));
#87830=CARTESIAN_POINT('Ctrl Pts',(-9.11627184040597,-1.51746837275248,
-2.52604465871351));
#87831=CARTESIAN_POINT('Ctrl Pts',(-9.06342410574268,-0.683851530584683,
-3.02682250071243));
#87832=CARTESIAN_POINT('Ctrl Pts',(-9.0105763710794,0.422093161666457,-3.07427141442917));
#87833=CARTESIAN_POINT('Ctrl Pts',(-8.95772863641611,1.29553805405546,-2.64673251965762));
#87834=CARTESIAN_POINT('Ctrl Pts',(-8.90488090175283,2.16898294644444,-2.21919362488608));
#87835=CARTESIAN_POINT('Ctrl Pts',(-8.85203316708954,2.8099280389713,-1.31666692162628));
#87836=CARTESIAN_POINT('Ctrl Pts',(-8.79918543242626,2.92580281968231,-0.351126388153944));
#87837=CARTESIAN_POINT('Ctrl Pts',(-8.74633769776298,3.04167760039333,0.614414145318391));
#87838=CARTESIAN_POINT('Ctrl Pts',(-8.6934899630997,2.63248206928852,1.64296850900325));
#87839=CARTESIAN_POINT('Ctrl Pts',(-8.64064222843642,1.88500062868308,2.26503521164317));
#87840=CARTESIAN_POINT('Ctrl Pts',(-8.58779449377313,1.13751918807765,2.88710191428309));
#87841=CARTESIAN_POINT('Ctrl Pts',(-8.53494675910984,0.051751837971596,
3.10268095587807));
#87842=CARTESIAN_POINT('Ctrl Pts',(-8.48209902444656,-0.876684069716822,
2.81336754122595));
#87843=CARTESIAN_POINT('Ctrl Pts',(-8.42925128978327,-1.80511997740523,
2.52405412657384));
#87844=CARTESIAN_POINT('Ctrl Pts',(-8.37640355512,-2.57622444267601,1.72984825567463));
#87845=CARTESIAN_POINT('Ctrl Pts',(-8.32355582045671,-2.83801344879435,
0.793278982818404));
#87846=CARTESIAN_POINT('Ctrl Pts',(-8.30909591933435,-2.90964269018971,
0.537020144742652));
#87847=CARTESIAN_POINT('Ctrl Pts',(-8.29463601821198,-2.94314211175223,
0.270103293504598));
#87848=CARTESIAN_POINT('Ctrl Pts',(-8.28017611708961,-2.94082616552171,
0.00261679703180889));
#87849=CARTESIAN_POINT('Origin',(-7.7,0.,0.));
#87850=CARTESIAN_POINT('',(-7.1358238829104,-2.93757269053894,-0.0010613151321931));
#87851=CARTESIAN_POINT('',(-7.28017611708961,-2.93772161116193,-0.00124778266073289));
#87852=CARTESIAN_POINT('',(-7.7,-2.942,-3.60291088309151E-16));
#87853=CARTESIAN_POINT('Ctrl Pts',(-7.1358238829104,-2.93757269053894,-0.0010613151321931));
#87854=CARTESIAN_POINT('Ctrl Pts',(-7.16584958045808,-2.93576229085772,
0.555920429035681));
#87855=CARTESIAN_POINT('Ctrl Pts',(-7.19587527800575,-2.78357509105504,
1.11381923203582));
#87856=CARTESIAN_POINT('Ctrl Pts',(-7.22590097555343,-2.48729794486864,
1.58017783952249));
#87857=CARTESIAN_POINT('Ctrl Pts',(-7.27874871021672,-1.96582543008058,
2.40100792705857));
#87858=CARTESIAN_POINT('Ctrl Pts',(-7.33159644488001,-0.997977548263203,
2.93825620062515));
#87859=CARTESIAN_POINT('Ctrl Pts',(-7.3844441795433,-0.0255452633823754,
2.94668636108162));
#87860=CARTESIAN_POINT('Ctrl Pts',(-7.43729191420658,0.946887021498432,
2.95511652153809));
#87861=CARTESIAN_POINT('Ctrl Pts',(-7.49013964886985,1.92390370944269,2.43472856888446));
#87862=CARTESIAN_POINT('Ctrl Pts',(-7.54298738353314,2.45952857579088,1.62306261614694));
#87863=CARTESIAN_POINT('Ctrl Pts',(-7.59583511819642,2.99515344213909,0.811396663409416));
#87864=CARTESIAN_POINT('Ctrl Pts',(-7.64868285285971,3.08938648689121,-0.291547289412031));
#87865=CARTESIAN_POINT('Ctrl Pts',(-7.70153058752299,2.69921340122809,-1.18231133196649));
#87866=CARTESIAN_POINT('Ctrl Pts',(-7.75437832218628,2.30904031556496,-2.07307537452096));
#87867=CARTESIAN_POINT('Ctrl Pts',(-7.80722605684956,1.43446109948659,-2.75165950680844));
#87868=CARTESIAN_POINT('Ctrl Pts',(-7.86007379151284,0.474692615678287,
-2.90831222390001));
#87869=CARTESIAN_POINT('Ctrl Pts',(-7.91292152617613,-0.485075868130016,
-3.06496494099157));
#87870=CARTESIAN_POINT('Ctrl Pts',(-7.96576926083941,-1.53003361966824,
-2.69968624288721));
#87871=CARTESIAN_POINT('Ctrl Pts',(-8.0186169955027,-2.18319153659025,-1.979213931243));
#87872=CARTESIAN_POINT('Ctrl Pts',(-8.05768595797193,-2.66605428000392,
-1.44658739799432));
#87873=CARTESIAN_POINT('Ctrl Pts',(-8.09675492044117,-2.93478813978928,
-0.719838240845876));
#87874=CARTESIAN_POINT('Ctrl Pts',(-8.1358238829104,-2.94119143690723,0.00265091043401527));
#87875=CARTESIAN_POINT('Ctrl Pts',(-8.28017611708961,-2.94082616552171,
0.00261679703180889));
#87876=CARTESIAN_POINT('Ctrl Pts',(-8.24178828354869,-2.93467784143329,
-0.707500583034972));
#87877=CARTESIAN_POINT('Ctrl Pts',(-8.20340045000778,-2.67610823149551,
-1.4216327364097));
#87878=CARTESIAN_POINT('Ctrl Pts',(-8.16501261646686,-2.20842183533617,
-1.95102149586555));
#87879=CARTESIAN_POINT('Ctrl Pts',(-8.11216488180358,-1.56456766879375,
-2.67982002688002));
#87880=CARTESIAN_POINT('Ctrl Pts',(-8.0593171471403,-0.524385788743001,
-3.0584844140957));
#87881=CARTESIAN_POINT('Ctrl Pts',(-8.00646941247701,0.437314731902111,
-2.91416672573489));
#87882=CARTESIAN_POINT('Ctrl Pts',(-7.95362167781373,1.39901525254722,-2.76984903737408));
#87883=CARTESIAN_POINT('Ctrl Pts',(-7.90077394315044,2.2822344137867,-2.1025492734368));
#87884=CARTESIAN_POINT('Ctrl Pts',(-7.84792620848715,2.68381150000848,-1.21686799306303));
#87885=CARTESIAN_POINT('Ctrl Pts',(-7.79507847382387,3.08538858623026,-0.331186712689277));
#87886=CARTESIAN_POINT('Ctrl Pts',(-7.74223073916059,3.00532359743435,0.772876084120949));
#87887=CARTESIAN_POINT('Ctrl Pts',(-7.68938300449731,2.48016358739293,1.59135177125903));
#87888=CARTESIAN_POINT('Ctrl Pts',(-7.63653526983403,1.9550035773515,2.40982745839712));
#87889=CARTESIAN_POINT('Ctrl Pts',(-7.58368753517074,0.98474854606456,2.94271603586306));
#87890=CARTESIAN_POINT('Ctrl Pts',(-7.53083980050746,0.0122882426526789,
2.94677126346982));
#87891=CARTESIAN_POINT('Ctrl Pts',(-7.47799206584417,-0.960172060759209,
2.95082649107658));
#87892=CARTESIAN_POINT('Ctrl Pts',(-7.42514433118089,-1.93483763629604,
2.42604836882414));
#87893=CARTESIAN_POINT('Ctrl Pts',(-7.37229659651761,-2.46680546536339,
1.61198097884942));
#87894=CARTESIAN_POINT('Ctrl Pts',(-7.34158977004161,-2.77590185184169,
1.13897250946104));
#87895=CARTESIAN_POINT('Ctrl Pts',(-7.31088294356561,-2.93553842718574,
0.568296682012325));
#87896=CARTESIAN_POINT('Ctrl Pts',(-7.28017611708961,-2.93772161116193,
-0.00124778266073289));
#87897=CARTESIAN_POINT('Origin',(-7.7,0.,0.));
#87898=CARTESIAN_POINT('',(-6.1358238829104,-2.94505049637757,-0.00196725817694088));
#87899=CARTESIAN_POINT('',(-6.28017611708961,-2.94535604779933,-0.00180876985891124));
#87900=CARTESIAN_POINT('',(-7.7,-2.942,-3.60291088309151E-16));
#87901=CARTESIAN_POINT('Ctrl Pts',(-6.1358238829104,-2.94505049637757,-0.00196725817694088));
#87902=CARTESIAN_POINT('Ctrl Pts',(-6.18209650581171,-2.93847787371737,
0.850848357286048));
#87903=CARTESIAN_POINT('Ctrl Pts',(-6.22836912871302,-2.54719747420371,
1.70892155386477));
#87904=CARTESIAN_POINT('Ctrl Pts',(-6.27464175161433,-1.89517178337686,
2.25653206991563));
#87905=CARTESIAN_POINT('Ctrl Pts',(-6.32748948627761,-1.15049645395035,
2.88195534260979));
#87906=CARTESIAN_POINT('Ctrl Pts',(-6.3803372209409,-0.0657098796553496,
3.10241694474892));
#87907=CARTESIAN_POINT('Ctrl Pts',(-6.43318495560419,0.864018279731717,
2.81728335162707));
#87908=CARTESIAN_POINT('Ctrl Pts',(-6.48603269026747,1.79374643911876,2.53214975850523));
#87909=CARTESIAN_POINT('Ctrl Pts',(-6.53888042493076,2.56841618359787,1.74142097012241));
#87910=CARTESIAN_POINT('Ctrl Pts',(-6.59172815959404,2.83441606285926,0.806038866104609));
#87911=CARTESIAN_POINT('Ctrl Pts',(-6.64457589425732,3.10041594212064,-0.129343237913193));
#87912=CARTESIAN_POINT('Ctrl Pts',(-6.69742362892061,2.8577459561643,-1.20937865756599));
#87913=CARTESIAN_POINT('Ctrl Pts',(-6.75027136358389,2.2171770319462,-1.94106648007633));
#87914=CARTESIAN_POINT('Ctrl Pts',(-6.80311909824717,1.57660810772809,-2.67275430258668));
#87915=CARTESIAN_POINT('Ctrl Pts',(-6.85596683291045,0.53814024524822,-3.05609452795455));
#87916=CARTESIAN_POINT('Ctrl Pts',(-6.90881456757374,-0.424199875648816,
-2.91610485692219));
#87917=CARTESIAN_POINT('Ctrl Pts',(-6.96166230223702,-1.38653999654583,
-2.77611518588984));
#87918=CARTESIAN_POINT('Ctrl Pts',(-7.01451003690031,-2.27275237586001,
-2.11279561845726));
#87919=CARTESIAN_POINT('Ctrl Pts',(-7.06735777156359,-2.67830999163772,
-1.2289298839882));
#87920=CARTESIAN_POINT('Ctrl Pts',(-7.09017980867919,-2.85344807501569,
-0.847236766472653));
#87921=CARTESIAN_POINT('Ctrl Pts',(-7.1130018457948,-2.938948745455,-0.424413945589069));
#87922=CARTESIAN_POINT('Ctrl Pts',(-7.1358238829104,-2.93757269053894,-0.0010613151321931));
#87923=CARTESIAN_POINT('Ctrl Pts',(-7.28017611708961,-2.93772161116193,
-0.00124778266073289));
#87924=CARTESIAN_POINT('Ctrl Pts',(-7.25803520890233,-2.93929577826156,
-0.411913199705981));
#87925=CARTESIAN_POINT('Ctrl Pts',(-7.23589430071504,-2.85900970571129,
-0.821990419652761));
#87926=CARTESIAN_POINT('Ctrl Pts',(-7.21375339252776,-2.69386683455209,
-1.19444269758718));
#87927=CARTESIAN_POINT('Ctrl Pts',(-7.16090565786447,-2.29969029207556,
-2.08344232635207));
#87928=CARTESIAN_POINT('Ctrl Pts',(-7.10805792320119,-1.4220671245246,-2.75808492618488));
#87929=CARTESIAN_POINT('Ctrl Pts',(-7.0552101885379,-0.461603659066119,
-2.9104181730562));
#87930=CARTESIAN_POINT('Ctrl Pts',(-7.00236245387462,0.498859806392379,
-3.06275141992753));
#87931=CARTESIAN_POINT('Ctrl Pts',(-6.94951471921134,1.5421635697584,-2.69277531383738));
#87932=CARTESIAN_POINT('Ctrl Pts',(-6.89666698454805,2.19207352029423,-1.9693718698468));
#87933=CARTESIAN_POINT('Ctrl Pts',(-6.84381924988477,2.84198347083005,-1.24596842585625));
#87934=CARTESIAN_POINT('Ctrl Pts',(-6.79097151522149,3.09849960853568,-0.169137643965288));
#87935=CARTESIAN_POINT('Ctrl Pts',(-6.7381237805582,2.84453069017054,0.769582375575847));
#87936=CARTESIAN_POINT('Ctrl Pts',(-6.68527604589492,2.59056177180539,1.70830239511698));
#87937=CARTESIAN_POINT('Ctrl Pts',(-6.63242831123163,1.82610779736946,2.50891165230829));
#87938=CARTESIAN_POINT('Ctrl Pts',(-6.57958057656835,0.900117051627725,
2.80595815604724));
#87939=CARTESIAN_POINT('Ctrl Pts',(-6.52673284190507,-0.0258736941140224,
3.10300465978619));
#87940=CARTESIAN_POINT('Ctrl Pts',(-6.47388510724178,-1.11340121116158,
2.89648841007276));
#87941=CARTESIAN_POINT('Ctrl Pts',(-6.4210373725785,-1.86604468884618,2.28067733345775));
#87942=CARTESIAN_POINT('Ctrl Pts',(-6.37408362074887,-2.53474761987163,
1.7335462094929));
#87943=CARTESIAN_POINT('Ctrl Pts',(-6.32712986891924,-2.93909873492038,
0.863324648112405));
#87944=CARTESIAN_POINT('Ctrl Pts',(-6.28017611708961,-2.94535604779933,
-0.00180876985891124));
#87945=CARTESIAN_POINT('Origin',(-7.7,0.,0.));
#87946=CARTESIAN_POINT('',(-5.1358238829104,-2.94346675723798,0.0024934893022114));
#87947=CARTESIAN_POINT('',(-5.28017611708961,-2.94309162548594,0.00256319306684998));
#87948=CARTESIAN_POINT('',(-7.7,-2.942,-3.60291088309151E-16));
#87949=CARTESIAN_POINT('Ctrl Pts',(-5.1358238829104,-2.94346675723798,0.0024934893022114));
#87950=CARTESIAN_POINT('Ctrl Pts',(-5.14549569650206,-2.94507633932214,
0.18099679752495));
#87951=CARTESIAN_POINT('Ctrl Pts',(-5.15516751009372,-2.93022859135991,
0.359232954535137));
#87952=CARTESIAN_POINT('Ctrl Pts',(-5.16483932368538,-2.89796164657921,
0.534257771161184));
#87953=CARTESIAN_POINT('Ctrl Pts',(-5.21768705834866,-2.72165190694203,
1.49061047387653));
#87954=CARTESIAN_POINT('Ctrl Pts',(-5.27053479301194,-2.02526828700205,
2.35108422924666));
#87955=CARTESIAN_POINT('Ctrl Pts',(-5.32338252767523,-1.12668717677613,
2.72290085694465));
#87956=CARTESIAN_POINT('Ctrl Pts',(-5.37623026233851,-0.228106066550204,
3.09471748464264));
#87957=CARTESIAN_POINT('Ctrl Pts',(-5.4290779970018,0.872672533961652,2.97787698466847));
#87958=CARTESIAN_POINT('Ctrl Pts',(-5.48192573166508,1.67317912706062,2.42571323116108));
#87959=CARTESIAN_POINT('Ctrl Pts',(-5.53477346632837,2.47368572015958,1.87354947765369));
#87960=CARTESIAN_POINT('Ctrl Pts',(-5.58762120099164,2.97392030584565,0.886062470613057));
#87961=CARTESIAN_POINT('Ctrl Pts',(-5.64046893565493,2.94554212522987,-0.0859922064235157));
#87962=CARTESIAN_POINT('Ctrl Pts',(-5.69331667031821,2.9171639446141,-1.05804688346009));
#87963=CARTESIAN_POINT('Ctrl Pts',(-5.7461644049815,2.3601729976965,-2.01466923049262));
#87964=CARTESIAN_POINT('Ctrl Pts',(-5.79901213964479,1.52881746953169,-2.51919237374194));
#87965=CARTESIAN_POINT('Ctrl Pts',(-5.85185987430807,0.697461941366897,
-3.02371551699126));
#87966=CARTESIAN_POINT('Ctrl Pts',(-5.90470760897135,-0.408258168045107,
-3.07613945645739));
#87967=CARTESIAN_POINT('Ctrl Pts',(-5.95755534363463,-1.28361772349481,
-2.65253437508267));
#87968=CARTESIAN_POINT('Ctrl Pts',(-6.01040307829791,-2.15897727894452,
-2.22892929370794));
#87969=CARTESIAN_POINT('Ctrl Pts',(-6.0632508129612,-2.80397628043193,-1.32929519149237));
#87970=CARTESIAN_POINT('Ctrl Pts',(-6.11609854762449,-2.92419373889664,
-0.364285668760009));
#87971=CARTESIAN_POINT('Ctrl Pts',(-6.12267365938646,-2.93915073242118,
-0.244222897786757));
#87972=CARTESIAN_POINT('Ctrl Pts',(-6.12924877114843,-2.94598443367894,
-0.12314815591822));
#87973=CARTESIAN_POINT('Ctrl Pts',(-6.1358238829104,-2.94505049637757,-0.00196725817694088));
#87974=CARTESIAN_POINT('Ctrl Pts',(-6.28017611708961,-2.94535604779933,
-0.00180876985891124));
#87975=CARTESIAN_POINT('Ctrl Pts',(-6.27428213425596,-2.94614151207547,
-0.110406726691919));
#87976=CARTESIAN_POINT('Ctrl Pts',(-6.2683881514223,-2.94065416034498,-0.21892450898504));
#87977=CARTESIAN_POINT('Ctrl Pts',(-6.26249416858865,-2.92862945740852,
-0.326712995330997));
#87978=CARTESIAN_POINT('Ctrl Pts',(-6.20964643392537,-2.82081130996463,
-1.29318634398818));
#87979=CARTESIAN_POINT('Ctrl Pts',(-6.15679869926208,-2.18741557675519,
-2.20102713778601));
#87980=CARTESIAN_POINT('Ctrl Pts',(-6.1039509645988,-1.31756673364422,-2.63583568958937));
#87981=CARTESIAN_POINT('Ctrl Pts',(-6.05110322993552,-0.447717890533236,
-3.07064424139274));
#87982=CARTESIAN_POINT('Ctrl Pts',(-5.99825549527223,0.658584062479277,
-3.03242055120164));
#87983=CARTESIAN_POINT('Ctrl Pts',(-5.94540776060895,1.49634839757276,-2.5386124858277));
#87984=CARTESIAN_POINT('Ctrl Pts',(-5.89256002594566,2.33411273266621,-2.04480442045378));
#87985=CARTESIAN_POINT('Ctrl Pts',(-5.83971229128238,2.90333944984063,-1.09541197989705));
#87986=CARTESIAN_POINT('Ctrl Pts',(-5.7868645566191,2.94419513434113,-0.123801821640741));
#87987=CARTESIAN_POINT('Ctrl Pts',(-5.73401682195581,2.98505081884163,0.847808336615591));
#87988=CARTESIAN_POINT('Ctrl Pts',(-5.68116908729253,2.49753547066817,1.8416362125715));
#87989=CARTESIAN_POINT('Ctrl Pts',(-5.62832135262925,1.70418393198402,2.40403182301857));
#87990=CARTESIAN_POINT('Ctrl Pts',(-5.57547361796596,0.910832393299871,
2.96642743346563));
#87991=CARTESIAN_POINT('Ctrl Pts',(-5.52262588330268,-0.188355335894953,
3.09739077840386));
#87992=CARTESIAN_POINT('Ctrl Pts',(-5.4697781486394,-1.09163593871943,2.73714136599013));
#87993=CARTESIAN_POINT('Ctrl Pts',(-5.41693041397611,-1.99491654154391,
2.3768919535764));
#87994=CARTESIAN_POINT('Ctrl Pts',(-5.36408267931283,-2.70229001799803,
1.5254297838107));
#87995=CARTESIAN_POINT('Ctrl Pts',(-5.31123494464955,-2.89086346732779,
0.571419542361142));
#87996=CARTESIAN_POINT('Ctrl Pts',(-5.30088200212957,-2.92780526046507,
0.384527648959713));
#87997=CARTESIAN_POINT('Ctrl Pts',(-5.29052905960959,-2.94483688929665,
0.19370023348868));
#87998=CARTESIAN_POINT('Ctrl Pts',(-5.28017611708961,-2.94309162548594,
0.00256319306684998));
#87999=CARTESIAN_POINT('Origin',(-7.7,0.,0.));
#88000=CARTESIAN_POINT('',(-4.1358238829104,-2.93721437885968,0.000152849678604627));
#88001=CARTESIAN_POINT('',(-4.2801761170896,-2.93720779641154,-5.3281763612922E-5));
#88002=CARTESIAN_POINT('',(-7.7,-2.942,-3.60291088309151E-16));
#88003=CARTESIAN_POINT('Ctrl Pts',(-4.1358238829104,-2.93721437885968,0.000152849678604627));
#88004=CARTESIAN_POINT('Ctrl Pts',(-4.16174262185569,-2.93743789235776,
0.481096322078444));
#88005=CARTESIAN_POINT('Ctrl Pts',(-4.18766136080098,-2.82590721058178,
0.961942138436253));
#88006=CARTESIAN_POINT('Ctrl Pts',(-4.21358009974627,-2.60205478700782,
1.38308494226313));
#88007=CARTESIAN_POINT('Ctrl Pts',(-4.26642783440955,-2.14562465320618,
2.24178579182884));
#88008=CARTESIAN_POINT('Ctrl Pts',(-4.31927556907284,-1.22222466387983,
2.85227550533413));
#88009=CARTESIAN_POINT('Ctrl Pts',(-4.37212330373612,-0.25335677173094,
2.93588545711232));
#88010=CARTESIAN_POINT('Ctrl Pts',(-4.42497103839941,0.715511120417946,
3.01949540889051));
#88011=CARTESIAN_POINT('Ctrl Pts',(-4.47781877306269,1.72984691538937,2.57622559894159));
#88012=CARTESIAN_POINT('Ctrl Pts',(-4.53066650772597,2.32663943477293,1.80841422559673));
#88013=CARTESIAN_POINT('Ctrl Pts',(-4.58351424238926,2.9234319541565,1.04060285225185));
#88014=CARTESIAN_POINT('Ctrl Pts',(-4.63636197705254,3.1026811979522,-0.0517500844889977));
#88015=CARTESIAN_POINT('Ctrl Pts',(-4.68920971171582,2.78256573751978,-0.970021127403228));
#88016=CARTESIAN_POINT('Ctrl Pts',(-4.74205744637911,2.46245027708737,-1.88829217031744));
#88017=CARTESIAN_POINT('Ctrl Pts',(-4.7949051810424,1.64297011242686,-2.63248131940505));
#88018=CARTESIAN_POINT('Ctrl Pts',(-4.84775291570568,0.698191187988024,
-2.86289052114596));
#88019=CARTESIAN_POINT('Ctrl Pts',(-4.90060065036896,-0.246587736450821,
-3.09329972288687));
#88020=CARTESIAN_POINT('Ctrl Pts',(-4.95344838503224,-1.316665420668,-2.80992897728107));
#88021=CARTESIAN_POINT('Ctrl Pts',(-5.00629611969553,-2.02358633310939,
-2.14212777944788));
#88022=CARTESIAN_POINT('Ctrl Pts',(-5.04947204076715,-2.60113164728262,
-1.59654277012084));
#88023=CARTESIAN_POINT('Ctrl Pts',(-5.09264796183877,-2.93628142551449,
-0.794362723217666));
#88024=CARTESIAN_POINT('Ctrl Pts',(-5.1358238829104,-2.94346675723798,0.0024934893022114));
#88025=CARTESIAN_POINT('Ctrl Pts',(-5.28017611708961,-2.94309162548594,
0.00256319306684998));
#88026=CARTESIAN_POINT('Ctrl Pts',(-5.2376813249463,-2.93592799807001,-0.781979828198723));
#88027=CARTESIAN_POINT('Ctrl Pts',(-5.195186532803,-2.61241459108027,-1.57173935609301));
#88028=CARTESIAN_POINT('Ctrl Pts',(-5.15269174065969,-2.05092138691181,
-2.11597101700905));
#88029=CARTESIAN_POINT('Ctrl Pts',(-5.09984400599641,-1.35263243496063,
-2.79279302179629));
#88030=CARTESIAN_POINT('Ctrl Pts',(-5.04699627133313,-0.28628110885286,
-3.08987871823736));
#88031=CARTESIAN_POINT('Ctrl Pts',(-4.99414853666985,0.661378020646438,
-2.8716181838679));
#88032=CARTESIAN_POINT('Ctrl Pts',(-4.94130080200656,1.60903715014574,-2.65335764949843));
#88033=CARTESIAN_POINT('Ctrl Pts',(-4.88845306734327,2.43800408303655,-1.91975088431843));
#88034=CARTESIAN_POINT('Ctrl Pts',(-4.83560533267999,2.76988247494261,-1.0056654290317));
#88035=CARTESIAN_POINT('Ctrl Pts',(-4.78275759801671,3.10176086684867,-0.0915799737449764));
#88036=CARTESIAN_POINT('Ctrl Pts',(-4.72990986335342,2.93655071776997,1.0029841716485));
#88037=CARTESIAN_POINT('Ctrl Pts',(-4.67706212869014,2.34966506772764,1.7783942053389));
#88038=CARTESIAN_POINT('Ctrl Pts',(-4.62421439402686,1.7627794176853,2.55380423902931));
#88039=CARTESIAN_POINT('Ctrl Pts',(-4.57136665936357,0.754218266679339,
3.01006016101665));
#88040=CARTESIAN_POINT('Ctrl Pts',(-4.51851892470029,-0.215643143023527,
2.93889603677497));
#88041=CARTESIAN_POINT('Ctrl Pts',(-4.46567119003701,-1.18550455272636,
2.86773191253328));
#88042=CARTESIAN_POINT('Ctrl Pts',(-4.41282345537372,-2.11666622112609,
2.26914774206261));
#88043=CARTESIAN_POINT('Ctrl Pts',(-4.35997572071044,-2.58408324300676,
1.41637765920455));
#88044=CARTESIAN_POINT('Ctrl Pts',(-4.33337585283683,-2.81934840816703,
0.987152609632971));
#88045=CARTESIAN_POINT('Ctrl Pts',(-4.30677598496322,-2.93712784426376,
0.49353173908822));
#88046=CARTESIAN_POINT('Ctrl Pts',(-4.2801761170896,-2.93720779641154,-5.3281763612922E-5));
#88047=CARTESIAN_POINT('Origin',(-7.7,0.,0.));
#88048=CARTESIAN_POINT('',(-3.1358238829104,-2.94290902102838,-0.00259068251834249));
#88049=CARTESIAN_POINT('',(-3.2801761170896,-2.94328604584299,-0.00252931999075325));
#88050=CARTESIAN_POINT('',(-7.7,-2.942,-3.60291088309151E-16));
#88051=CARTESIAN_POINT('Ctrl Pts',(-3.1358238829104,-2.94290902102838,-0.00259068251834249));
#88052=CARTESIAN_POINT('Ctrl Pts',(-3.17798954720932,-2.93577329752197,
0.77600050829119));
#88053=CARTESIAN_POINT('Ctrl Pts',(-3.22015521150824,-2.61779276653383,
1.5597441706684));
#88054=CARTESIAN_POINT('Ctrl Pts',(-3.26232087580717,-2.06400928767338,
2.10320678247858));
#88055=CARTESIAN_POINT('Ctrl Pts',(-3.31516861047045,-1.36993265356056,
2.78434790490345));
#88056=CARTESIAN_POINT('Ctrl Pts',(-3.36801634513374,-0.305444837903283,
3.08804341587024));
#88057=CARTESIAN_POINT('Ctrl Pts',(-3.42086407979702,0.64355018528268,2.87566622534601));
#88058=CARTESIAN_POINT('Ctrl Pts',(-3.4737118144603,1.59254520846861,2.66328903482179));
#88059=CARTESIAN_POINT('Ctrl Pts',(-3.52655954912359,2.42604743918324,1.93483914280656));
#88060=CARTESIAN_POINT('Ctrl Pts',(-3.57940728378687,2.76359033593641,1.02283014731745));
#88061=CARTESIAN_POINT('Ctrl Pts',(-3.63225501845015,3.1011332326896,0.110821151828297));
#88062=CARTESIAN_POINT('Ctrl Pts',(-3.68510275311344,2.94271679548128,-0.984746947134762));
#88063=CARTESIAN_POINT('Ctrl Pts',(-3.73795048777672,2.36065294704176,-1.76378307655536));
#88064=CARTESIAN_POINT('Ctrl Pts',(-3.79079822244,1.77858909860226,-2.54281920597594));
#88065=CARTESIAN_POINT('Ctrl Pts',(-3.84364595710329,0.772877838931594,
-3.00532336585409));
#88066=CARTESIAN_POINT('Ctrl Pts',(-3.89649369176657,-0.197406467007782,
-2.94017750459693));
#88067=CARTESIAN_POINT('Ctrl Pts',(-3.94934142642986,-1.16769077294716,
-2.87503164333976));
#88068=CARTESIAN_POINT('Ctrl Pts',(-4.00218916109314,-2.10254812515524,
-2.28223576094729));
#88069=CARTESIAN_POINT('Ctrl Pts',(-4.05503689575642,-2.57524666212081,
-1.43238182693799));
#88070=CARTESIAN_POINT('Ctrl Pts',(-4.08196589147441,-2.81611407032574,
-0.999331799426508));
#88071=CARTESIAN_POINT('Ctrl Pts',(-4.1088948871924,-2.93698215328553,-0.499536766247084));
#88072=CARTESIAN_POINT('Ctrl Pts',(-4.1358238829104,-2.93721437885968,0.000152849678604627));
#88073=CARTESIAN_POINT('Ctrl Pts',(-4.2801761170896,-2.93720779641154,-5.3281763612922E-5));
#88074=CARTESIAN_POINT('Ctrl Pts',(-4.25392825029993,-2.93728669053742,
-0.487106598654287));
#88075=CARTESIAN_POINT('Ctrl Pts',(-4.22768038351026,-2.82276056857575,
-0.974125008385675));
#88076=CARTESIAN_POINT('Ctrl Pts',(-4.20143251672059,-2.59342404981643,
-1.39920104976605));
#88077=CARTESIAN_POINT('Ctrl Pts',(-4.14858478205731,-2.13167545938383,
-2.25505368063311));
#88078=CARTESIAN_POINT('Ctrl Pts',(-4.09573704739402,-1.20450590315705,
-2.85980294712179));
#88079=CARTESIAN_POINT('Ctrl Pts',(-4.04288931273074,-0.23513801698091,
-2.93740055033165));
#88080=CARTESIAN_POINT('Ctrl Pts',(-3.99004157806746,0.734229869195233,
-3.01499815354152));
#88081=CARTESIAN_POINT('Ctrl Pts',(-3.93719384340417,1.74579608532074,-2.56544409347258));
#88082=CARTESIAN_POINT('Ctrl Pts',(-3.88434610874089,2.33781367422211,-1.7939451234042));
#88083=CARTESIAN_POINT('Ctrl Pts',(-3.8314983740776,2.92983126312348,-1.02244615333581));
#88084=CARTESIAN_POINT('Ctrl Pts',(-3.77865063941432,3.10230022480071,0.0709977267320187));
#88085=CARTESIAN_POINT('Ctrl Pts',(-3.72580290475104,2.77649410964299,0.98726507943176));
#88086=CARTESIAN_POINT('Ctrl Pts',(-3.67295517008775,2.45068799448526,1.90353243213151));
#88087=CARTESIAN_POINT('Ctrl Pts',(-3.62010743542447,1.62660680249256,2.64262325746317));
#88088=CARTESIAN_POINT('Ctrl Pts',(-3.56725970076119,0.680416694159909,
2.86716672049554));
#88089=CARTESIAN_POINT('Ctrl Pts',(-3.5144119660979,-0.26577341417273,3.09171018352791));
#88090=CARTESIAN_POINT('Ctrl Pts',(-3.46156423143462,-1.33407243884532,
2.801706284261));
#88091=CARTESIAN_POINT('Ctrl Pts',(-3.40871649677134,-2.03683674323611,
2.12953233551788));
#88092=CARTESIAN_POINT('Ctrl Pts',(-3.36586970354409,-2.6066094502324,1.58456104435399));
#88093=CARTESIAN_POINT('Ctrl Pts',(-3.32302291031685,-2.93610497497431,
0.788377658866007));
#88094=CARTESIAN_POINT('Ctrl Pts',(-3.2801761170896,-2.94328604584299,-0.00252931999075325));
#88095=CARTESIAN_POINT('Origin',(-7.7,0.,0.));
#88096=CARTESIAN_POINT('',(-2.1358238829104,-2.94549590326081,0.00172726763101459));
#88097=CARTESIAN_POINT('',(-2.2801761170896,-2.94520044895666,0.00189243946321858));
#88098=CARTESIAN_POINT('',(-7.7,-2.942,-3.60291088309151E-16));
#88099=CARTESIAN_POINT('Ctrl Pts',(-2.1358238829104,-2.94549590326081,0.00172726763101459));
#88100=CARTESIAN_POINT('Ctrl Pts',(-2.14138873789967,-2.94621118435907,
0.104248158404311));
#88101=CARTESIAN_POINT('Ctrl Pts',(-2.14695359288894,-2.94132097000673,
0.206700038959149));
#88102=CARTESIAN_POINT('Ctrl Pts',(-2.15251844787821,-2.93059923639254,
0.308537962920288));
#88103=CARTESIAN_POINT('Ctrl Pts',(-2.20536618254149,-2.8287781944668,1.2756617414436));
#88104=CARTESIAN_POINT('Ctrl Pts',(-2.25821391720478,-2.20102858389113,
2.18741447546925));
#88105=CARTESIAN_POINT('Ctrl Pts',(-2.31106165186806,-1.33389435847118,
2.62761108458551));
#88106=CARTESIAN_POINT('Ctrl Pts',(-2.36390938653134,-0.466760133051231,
3.06780769370176));
#88107=CARTESIAN_POINT('Ctrl Pts',(-2.41675712119463,0.63975870721301,3.03644817790864));
#88108=CARTESIAN_POINT('Ctrl Pts',(-2.46960485585791,1.48057073115753,2.54784698609512));
#88109=CARTESIAN_POINT('Ctrl Pts',(-2.5224525905212,2.32138275510203,2.05924579428162));
#88110=CARTESIAN_POINT('Ctrl Pts',(-2.57530032518448,2.89648796272684,1.11340292644773));
#88111=CARTESIAN_POINT('Ctrl Pts',(-2.62814805984776,2.94337049059091,0.142064852598672));
#88112=CARTESIAN_POINT('Ctrl Pts',(-2.68099579451105,2.99025301845499,-0.829273221250395));
#88113=CARTESIAN_POINT('Ctrl Pts',(-2.73384352917433,2.50891286655834,-1.82610650111461));
#88114=CARTESIAN_POINT('Ctrl Pts',(-2.78669126383761,1.71906563566131,-2.39341317509171));
#88115=CARTESIAN_POINT('Ctrl Pts',(-2.8395389985009,0.929218404764276,-2.9607198490688));
#88116=CARTESIAN_POINT('Ctrl Pts',(-2.89238673316418,-0.169135905133138,
-3.09849991715875));
#88117=CARTESIAN_POINT('Ctrl Pts',(-2.94523446782747,-1.0746341620639,-2.74386125494763));
#88118=CARTESIAN_POINT('Ctrl Pts',(-2.99808220249075,-1.98013241899465,
-2.38922259273651));
#88119=CARTESIAN_POINT('Ctrl Pts',(-3.05092993715403,-2.69277462295876,
-1.54216520022432));
#88120=CARTESIAN_POINT('Ctrl Pts',(-3.10377767181732,-2.88726299865664,
-0.589343137026765));
#88121=CARTESIAN_POINT('Ctrl Pts',(-3.11445974218168,-2.92657477857477,
-0.396749975018218));
#88122=CARTESIAN_POINT('Ctrl Pts',(-3.12514181254604,-2.94471675492428,
-0.199835669015806));
#88123=CARTESIAN_POINT('Ctrl Pts',(-3.1358238829104,-2.94290902102838,-0.00259068251834249));
#88124=CARTESIAN_POINT('Ctrl Pts',(-3.2801761170896,-2.94328604584299,-0.00252931999075325));
#88125=CARTESIAN_POINT('Ctrl Pts',(-3.27017517565356,-2.94496219156584,
-0.187136236427897));
#88126=CARTESIAN_POINT('Ctrl Pts',(-3.26017423421752,-2.92907832148784,
-0.371455688921979));
#88127=CARTESIAN_POINT('Ctrl Pts',(-3.25017329278148,-2.89459120843848,
-0.552226040806602));
#88128=CARTESIAN_POINT('Ctrl Pts',(-3.1973255581182,-2.71235178514105,-1.50746647016865));
#88129=CARTESIAN_POINT('Ctrl Pts',(-3.14447782345492,-2.01064335443715,
-2.36360333067339));
#88130=CARTESIAN_POINT('Ctrl Pts',(-3.09163008879163,-1.10977289024573,
-2.72983809441704));
#88131=CARTESIAN_POINT('Ctrl Pts',(-3.03878235412835,-0.208902426054322,
-3.09607285816069));
#88132=CARTESIAN_POINT('Ctrl Pts',(-2.98593461946506,0.89113007162461,-2.97240552514326));
#88133=CARTESIAN_POINT('Ctrl Pts',(-2.93308688480178,1.68819564156411,-2.41528619309179));
#88134=CARTESIAN_POINT('Ctrl Pts',(-2.8802391501385,2.48526121150361,-1.85816686104031));
#88135=CARTESIAN_POINT('Ctrl Pts',(-2.82739141547522,2.97935985370367,-0.86759552995479));
#88136=CARTESIAN_POINT('Ctrl Pts',(-2.77454368081193,2.94495173425786,0.10426431795293));
#88137=CARTESIAN_POINT('Ctrl Pts',(-2.72169594614865,2.91054361481204,1.07612416586066));
#88138=CARTESIAN_POINT('Ctrl Pts',(-2.66884821148536,2.34762873372032,2.02927253059059));
#88139=CARTESIAN_POINT('Ctrl Pts',(-2.61600047682208,1.51315923045204,2.52862830825837));
#88140=CARTESIAN_POINT('Ctrl Pts',(-2.5631527421588,0.678689727183778,3.02798408592614));
#88141=CARTESIAN_POINT('Ctrl Pts',(-2.51030500749551,-0.427334398261043,
3.07354727653178));
#88142=CARTESIAN_POINT('Ctrl Pts',(-2.45745727283223,-1.30004899242779,
2.64451975108657));
#88143=CARTESIAN_POINT('Ctrl Pts',(-2.40460953816895,-2.17276358659452,
2.21549222564138));
#88144=CARTESIAN_POINT('Ctrl Pts',(-2.35176180350566,-2.81216864948318,
1.31187398414536));
#88145=CARTESIAN_POINT('Ctrl Pts',(-2.29891406884238,-2.92639711020017,
0.346137294326151));
#88146=CARTESIAN_POINT('Ctrl Pts',(-2.29266808492479,-2.93989757778153,
0.231998516729099));
#88147=CARTESIAN_POINT('Ctrl Pts',(-2.2864221010072,-2.94606212951774,0.116992039186075));
#88148=CARTESIAN_POINT('Ctrl Pts',(-2.2801761170896,-2.94520044895666,0.00189243946321858));
#88149=CARTESIAN_POINT('Origin',(-7.7,0.,0.));
#88150=CARTESIAN_POINT('',(-1.13582388291039,-2.93784718745393,0.00133151008673116));
#88151=CARTESIAN_POINT('',(-1.2801761170896,-2.93764836154578,0.0011528133628201));
#88152=CARTESIAN_POINT('',(-7.7,-2.942,-3.60291088309151E-16));
#88153=CARTESIAN_POINT('Ctrl Pts',(-1.13582388291039,-2.93784718745393,
0.00133151008673116));
#88154=CARTESIAN_POINT('Ctrl Pts',(-1.1576356632533,-2.93947473760419,0.405867522931662));
#88155=CARTESIAN_POINT('Ctrl Pts',(-1.1794474435962,-2.86160462622403,0.809791925226849));
#88156=CARTESIAN_POINT('Ctrl Pts',(-1.20125922393911,-2.70117913249261,
1.1777113598064));
#88157=CARTESIAN_POINT('Ctrl Pts',(-1.25410695860239,-2.31248440915232,
2.06914288673587));
#88158=CARTESIAN_POINT('Ctrl Pts',(-1.30695469326567,-1.43915341522439,
2.74920947561571));
#88159=CARTESIAN_POINT('Ctrl Pts',(-1.35980242792896,-0.479674863775861,
2.90749655167124));
#88160=CARTESIAN_POINT('Ctrl Pts',(-1.41265016259224,0.47980368767267,3.06578362772676));
#88161=CARTESIAN_POINT('Ctrl Pts',(-1.46549789725552,1.52542979664179,2.70229119095795));
#88162=CARTESIAN_POINT('Ctrl Pts',(-1.51834563191881,2.17982640754776,1.98293454354379));
#88163=CARTESIAN_POINT('Ctrl Pts',(-1.57119336658209,2.83422301845374,1.26357789612962));
#88164=CARTESIAN_POINT('Ctrl Pts',(-1.62404110124538,3.09739013129655,0.188357038070054));
#88165=CARTESIAN_POINT('Ctrl Pts',(-1.67688883590866,2.84924391347341,-0.751921077245129));
#88166=CARTESIAN_POINT('Ctrl Pts',(-1.72973657057194,2.60109769565026,-1.6921991925603));
#88167=CARTESIAN_POINT('Ctrl Pts',(-1.78258430523523,1.8416381471612,-2.49753456513111));
#88168=CARTESIAN_POINT('Ctrl Pts',(-1.83543203989851,0.917511068992977,
-2.80031983874035));
#88169=CARTESIAN_POINT('Ctrl Pts',(-1.88827977456179,-0.00661600917524305,
-3.10310511234959));
#88170=CARTESIAN_POINT('Ctrl Pts',(-1.94112750922508,-1.0954106170226,-2.90334028699726));
#88171=CARTESIAN_POINT('Ctrl Pts',(-1.99397524388836,-1.85186168430837,
-2.2922104628106));
#88172=CARTESIAN_POINT('Ctrl Pts',(-2.04125812356237,-2.52865861839909,
-1.74543247646309));
#88173=CARTESIAN_POINT('Ctrl Pts',(-2.08854100323638,-2.93941837740121,
-0.869361548133691));
#88174=CARTESIAN_POINT('Ctrl Pts',(-2.1358238829104,-2.94549590326081,0.00172726763101459));
#88175=CARTESIAN_POINT('Ctrl Pts',(-2.2801761170896,-2.94520044895666,0.00189243946321858));
#88176=CARTESIAN_POINT('Ctrl Pts',(-2.23357436634391,-2.93877138617659,
-0.856874238130207));
#88177=CARTESIAN_POINT('Ctrl Pts',(-2.18697261559822,-2.54120861453645,
-1.72082480689521));
#88178=CARTESIAN_POINT('Ctrl Pts',(-2.14037086485253,-1.88113620379347,
-2.26824587484884));
#88179=CARTESIAN_POINT('Ctrl Pts',(-2.08752313018924,-1.13259497812453,
-2.88903721606212));
#88180=CARTESIAN_POINT('Ctrl Pts',(-2.03467539552596,-0.0464606682413524,
-3.10276476034627));
#88181=CARTESIAN_POINT('Ctrl Pts',(-1.98182766086268,0.881480161163561,
-2.81186872231317));
#88182=CARTESIAN_POINT('Ctrl Pts',(-1.92897992619939,1.80942099056847,-2.52097268428006));
#88183=CARTESIAN_POINT('Ctrl Pts',(-1.87613219153611,2.57916833949514,-1.72545306392968));
#88184=CARTESIAN_POINT('Ctrl Pts',(-1.82328445687283,2.83936093304215,-0.788438863463607));
#88185=CARTESIAN_POINT('Ctrl Pts',(-1.77043672220954,3.09955352658915,0.148575337002482));
#88186=CARTESIAN_POINT('Ctrl Pts',(-1.71758898754626,2.8501913647565,1.22708411758425));
#88187=CARTESIAN_POINT('Ctrl Pts',(-1.66474125288298,2.20509390103984,1.95478393112635));
#88188=CARTESIAN_POINT('Ctrl Pts',(-1.61189351821969,1.55999643732318,2.68248374466846));
#88189=CARTESIAN_POINT('Ctrl Pts',(-1.55904578355641,0.519163671722485,
3.05937459117085));
#88190=CARTESIAN_POINT('Ctrl Pts',(-1.50619804889312,-0.442286305680839,
2.91341713798924));
#88191=CARTESIAN_POINT('Ctrl Pts',(-1.45335031422984,-1.40373628308415,
2.76745968480763));
#88192=CARTESIAN_POINT('Ctrl Pts',(-1.40050257956656,-2.28580347229011,
2.09865393194203));
#88193=CARTESIAN_POINT('Ctrl Pts',(-1.34765484490327,-2.68587574865743,
1.21228971570189));
#88194=CARTESIAN_POINT('Ctrl Pts',(-1.32516193563205,-2.8561534241642,0.835037785715198));
#88195=CARTESIAN_POINT('Ctrl Pts',(-1.30266902636083,-2.93911768646335,
0.418375124404466));
#88196=CARTESIAN_POINT('Ctrl Pts',(-1.2801761170896,-2.93764836154578,0.0011528133628201));
#88197=CARTESIAN_POINT('Origin',(-7.7,0.,0.));
#88198=CARTESIAN_POINT('',(-0.249999999999999,-2.942,-3.60291088309151E-16));
#88199=CARTESIAN_POINT('',(-0.2801761170896,-2.94174543957041,-0.0025773274983063));
#88200=CARTESIAN_POINT('',(-7.7,-2.942,-3.60291088309151E-16));
#88201=CARTESIAN_POINT('',(-0.250000000000001,-2.21686865784453,1.93412961144453));
#88202=CARTESIAN_POINT('Origin',(-0.25,0.,0.));
#88203=CARTESIAN_POINT('Ctrl Pts',(-0.250000000000001,-2.21686865784453,
1.93412961144453));
#88204=CARTESIAN_POINT('Ctrl Pts',(-0.302847734663285,-1.57463683943972,
2.67024552677286));
#88205=CARTESIAN_POINT('Ctrl Pts',(-0.355695469326569,-0.542559076580902,
3.05509500507822));
#88206=CARTESIAN_POINT('Ctrl Pts',(-0.408543203989852,0.418376638715716,
2.91670525910205));
#88207=CARTESIAN_POINT('Ctrl Pts',(-0.461390938653135,1.37931235401231,
2.77831551312588));
#88208=CARTESIAN_POINT('Ctrl Pts',(-0.514238673316417,2.2691060217467,2.1166865428682));
#88209=CARTESIAN_POINT('Ctrl Pts',(-0.5670864079797,2.67678709245509,1.23355235122458));
#88210=CARTESIAN_POINT('Ctrl Pts',(-0.619934142642985,3.08446816316349,
0.350418159580932));
#88211=CARTESIAN_POINT('Ctrl Pts',(-0.672781877306269,3.01003663684585,
-0.754221253448677));
#88212=CARTESIAN_POINT('Ctrl Pts',(-0.725629611969553,2.48967051684404,
-1.57596292656688));
#88213=CARTESIAN_POINT('Ctrl Pts',(-0.778477346632837,1.96930439684224,
-2.39770459968508));
#88214=CARTESIAN_POINT('Ctrl Pts',(-0.831325081296121,1.00300368315625,
-2.93654853289187));
#88215=CARTESIAN_POINT('Ctrl Pts',(-0.884172815959405,0.0307377045118488,
-2.94662393799235));
#88216=CARTESIAN_POINT('Ctrl Pts',(-0.93702055062269,-0.941528274132556,
-2.95669934309284));
#88217=CARTESIAN_POINT('Ctrl Pts',(-0.989868285285974,-1.91975951773539,
-2.43800622008702));
#88218=CARTESIAN_POINT('Ctrl Pts',(-1.04271601994926,-2.45684591316047,
-1.62726142609455));
#88219=CARTESIAN_POINT('Ctrl Pts',(-1.07375197426964,-2.77226130306725,
-1.15113433091906));
#88220=CARTESIAN_POINT('Ctrl Pts',(-1.10478792859001,-2.93553134842917,
-0.574282264590201));
#88221=CARTESIAN_POINT('Ctrl Pts',(-1.13582388291039,-2.93784718745393,
0.00133151008673116));
#88222=CARTESIAN_POINT('Ctrl Pts',(-1.2801761170896,-2.93764836154578,0.0011528133628201));
#88223=CARTESIAN_POINT('Ctrl Pts',(-1.24982129169754,-2.93566546547934,
-0.561900647113437));
#88224=CARTESIAN_POINT('Ctrl Pts',(-1.21946646630548,-2.77990979285944,
-1.12597335710706));
#88225=CARTESIAN_POINT('Ctrl Pts',(-1.18911164091342,-2.47745937646832,
-1.59557717601159));
#88226=CARTESIAN_POINT('Ctrl Pts',(-1.13626390625014,-1.95089336438317,
-2.41315717187029));
#88227=CARTESIAN_POINT('Ctrl Pts',(-1.08341617158686,-0.97968397668418,
-2.94439448397298));
#88228=CARTESIAN_POINT('Ctrl Pts',(-1.03056843692357,-0.00723965287597085,
-2.94678989518399));
#88229=CARTESIAN_POINT('Ctrl Pts',(-0.977720702260289,0.965204670932211,
-2.94918530639499));
#88230=CARTESIAN_POINT('Ctrl Pts',(-0.924872967597005,1.93888393084963,
-2.4227388167143));
#88231=CARTESIAN_POINT('Ctrl Pts',(-0.872025232933722,2.46950402838423,
-1.60776891670247));
#88232=CARTESIAN_POINT('Ctrl Pts',(-0.819177498270439,3.00012412591883,
-0.792799016690619));
#88233=CARTESIAN_POINT('Ctrl Pts',(-0.766329763607154,3.08768506107063,
0.310694293652399));
#88234=CARTESIAN_POINT('Ctrl Pts',(-0.71348202894387,2.69191482003378,1.19902692584877));
#88235=CARTESIAN_POINT('Ctrl Pts',(-0.660634294280585,2.29614457899693,
2.08735955804518));
#88236=CARTESIAN_POINT('Ctrl Pts',(-0.607786559617304,1.41704316177144,
2.76053151209489));
#88237=CARTESIAN_POINT('Ctrl Pts',(-0.554938824954019,0.456472030616278,
2.91121453806236));
#88238=CARTESIAN_POINT('Ctrl Pts',(-0.502091090290737,-0.504099100538845,
3.06189756402983));
#88239=CARTESIAN_POINT('Ctrl Pts',(-0.449243355627451,-1.54613994562364,
2.69009166191506));
#88240=CARTESIAN_POINT('Ctrl Pts',(-0.396395620964168,-2.19510946333902,
1.96560658123782));
#88241=CARTESIAN_POINT('Ctrl Pts',(-0.357655786339312,-2.67083414582638,
1.43452549720582));
#88242=CARTESIAN_POINT('Ctrl Pts',(-0.318915951714456,-2.93533926593172,
0.713929847825713));
#88243=CARTESIAN_POINT('Ctrl Pts',(-0.2801761170896,-2.94174543957041,-0.0025773274983063));
#88244=CARTESIAN_POINT('Origin',(-17.306589891905,0.,0.));
#88245=CARTESIAN_POINT('',(-0.806589891905004,-2.36840213013048,0.00107342251797217));
#88246=CARTESIAN_POINT('',(-0.609410108094966,-2.37154478120365,-0.00207776223488526));
#88247=CARTESIAN_POINT('',(-17.306589891905,-2.37175,-2.3095687792789E-13));
#88248=CARTESIAN_POINT('',(-0.25,2.22665730523966,0.827839780511538));
#88249=CARTESIAN_POINT('Ctrl Pts',(-0.806589891905004,-2.36840213013048,
0.00107342251797246));
#88250=CARTESIAN_POINT('Ctrl Pts',(-0.775553937584626,-2.3665351718684,
-0.462968715513973));
#88251=CARTESIAN_POINT('Ctrl Pts',(-0.691670248600965,-2.01078495654127,
-1.71987561692049));
#88252=CARTESIAN_POINT('Ctrl Pts',(-0.55493882495402,0.029588806200308,
-2.80175461640703));
#88253=CARTESIAN_POINT('Ctrl Pts',(-0.400444815306063,2.30690749425437,
-1.5318400425519));
#88254=CARTESIAN_POINT('Ctrl Pts',(-0.29879854032139,2.47529789451049,0.147370939433083));
#88255=CARTESIAN_POINT('Ctrl Pts',(-0.25,2.22665730523966,0.827839780511538));
#88256=CARTESIAN_POINT('',(-0.250000000000001,1.50502666328431,-1.8330555925294));
#88257=CARTESIAN_POINT('Origin',(-0.249999999999999,0.,0.));
#88258=CARTESIAN_POINT('Ctrl Pts',(-0.609410108094966,-2.37154478120365,
-0.00207776223488519));
#88259=CARTESIAN_POINT('Ctrl Pts',(-0.595302208056545,-2.37342552465464,
-0.21243206319483));
#88260=CARTESIAN_POINT('Ctrl Pts',(-0.52834657335484,-2.25138912390084,
-1.20869219511272));
#88261=CARTESIAN_POINT('Ctrl Pts',(-0.408543203989851,-0.847344309994932,
-2.66988130255231));
#88262=CARTESIAN_POINT('Ctrl Pts',(-0.302847734663285,0.896356686121819,
-2.33280287161008));
#88263=CARTESIAN_POINT('Ctrl Pts',(-0.250000000000001,1.50502666328431,
-1.8330555925294));
#88264=CARTESIAN_POINT('Origin',(-17.306589891905,0.,0.));
#88265=CARTESIAN_POINT('',(-1.80658989190501,-2.37456828978886,0.00139247008960864));
#88266=CARTESIAN_POINT('',(-1.60941010809497,-2.36824184279273,0.000929362709871234));
#88267=CARTESIAN_POINT('',(-17.306589891905,-2.37175,-2.3095687792789E-13));
#88268=CARTESIAN_POINT('Ctrl Pts',(-1.80658989190501,-2.37456828978886,
0.00139247008960867));
#88269=CARTESIAN_POINT('Ctrl Pts',(-1.759307012231,-2.36966877518737,-0.700852566888605));
#88270=CARTESIAN_POINT('Ctrl Pts',(-1.6591763978937,-1.66841196255505,-2.19649738938181));
#88271=CARTESIAN_POINT('Ctrl Pts',(-1.50619804889313,0.872419133718849,
-2.66267225518167));
#88272=CARTESIAN_POINT('Ctrl Pts',(-1.34765484490327,2.70917798905082,-0.714962360659344));
#88273=CARTESIAN_POINT('Ctrl Pts',(-1.18911164091343,2.07270626924971,1.88546769043105));
#88274=CARTESIAN_POINT('Ctrl Pts',(-1.03056843692357,-0.456148649799437,
2.76457699047157));
#88275=CARTESIAN_POINT('Ctrl Pts',(-0.903061187254099,-2.15483664022398,
1.44180137017275));
#88276=CARTESIAN_POINT('Ctrl Pts',(-0.82840167224791,-2.36971421105125,
0.327197925735182));
#88277=CARTESIAN_POINT('Ctrl Pts',(-0.806589891905004,-2.36840213013048,
0.00107342251797246));
#88278=CARTESIAN_POINT('Ctrl Pts',(-1.60941010809497,-2.36824184279273,
0.0009293627098712));
#88279=CARTESIAN_POINT('Ctrl Pts',(-1.57905528270292,-2.36664329291314,
-0.452987035959174));
#88280=CARTESIAN_POINT('Ctrl Pts',(-1.49585272264758,-2.02246849688374,
-1.69942388568812));
#88281=CARTESIAN_POINT('Ctrl Pts',(-1.35980242792896,-0.0068319532377577,
-2.80194755688051));
#88282=CARTESIAN_POINT('Ctrl Pts',(-1.20125922393911,2.34801894891291,-1.52873260592859));
#88283=CARTESIAN_POINT('Ctrl Pts',(-1.04271601994925,2.55978575511233,1.14007459203818));
#88284=CARTESIAN_POINT('Ctrl Pts',(-0.884172815959405,0.433672104903693,
2.76814622563851));
#88285=CARTESIAN_POINT('Ctrl Pts',(-0.739737512007974,-1.86225432289822,
1.94894705441156));
#88286=CARTESIAN_POINT('Ctrl Pts',(-0.648149942719829,-2.36638032086125,
0.575548306111478));
#88287=CARTESIAN_POINT('Ctrl Pts',(-0.609410108094966,-2.37154478120365,
-0.00207776223488519));
#88288=CARTESIAN_POINT('Origin',(-17.306589891905,0.,0.));
#88289=CARTESIAN_POINT('',(-2.80658989190501,-2.37248282482123,-0.00208852864143664));
#88290=CARTESIAN_POINT('',(-2.60941010809497,-2.3743301036074,0.00152562654522952));
#88291=CARTESIAN_POINT('',(-17.306589891905,-2.37175,-2.3095687792789E-13));
#88292=CARTESIAN_POINT('Ctrl Pts',(-2.80658989190501,-2.37248282482123,
-0.00208852864143679));
#88293=CARTESIAN_POINT('Ctrl Pts',(-2.79590782154065,-2.37394016434114,
-0.161101375930807));
#88294=CARTESIAN_POINT('Ctrl Pts',(-2.73237801651301,-2.28695745611499,
-1.10521789855147));
#88295=CARTESIAN_POINT('Ctrl Pts',(-2.61600047682208,-1.02181166468338,
-2.60898948164979));
#88296=CARTESIAN_POINT('Ctrl Pts',(-2.45745727283223,1.63456682052989,-2.27576730983566));
#88297=CARTESIAN_POINT('Ctrl Pts',(-2.29891406884238,2.79869174091825,0.135081770570203));
#88298=CARTESIAN_POINT('Ctrl Pts',(-2.14037086485253,1.40779530021379,2.42261014084723));
#88299=CARTESIAN_POINT('Ctrl Pts',(-1.98182766086268,-1.26832916552041,
2.49845337495562));
#88300=CARTESIAN_POINT('Ctrl Pts',(-1.87056733654684,-2.33376337820802,
0.951001110586071));
#88301=CARTESIAN_POINT('Ctrl Pts',(-1.81215474689428,-2.37514492743155,
0.0840416620310201));
#88302=CARTESIAN_POINT('Ctrl Pts',(-1.80658989190501,-2.37456828978886,
0.00139247008960867));
#88303=CARTESIAN_POINT('Ctrl Pts',(-2.60941010809497,-2.3743301036074,0.00152562654522945));
#88304=CARTESIAN_POINT('Ctrl Pts',(-2.56280835734929,-2.36914719074238,
-0.690785681266458));
#88305=CARTESIAN_POINT('Ctrl Pts',(-2.46335887194031,-1.68518474265676,
-2.17711636459373));
#88306=CARTESIAN_POINT('Ctrl Pts',(-2.31106165186806,0.838152943427643,
-2.67365418881957));
#88307=CARTESIAN_POINT('Ctrl Pts',(-2.15251844787821,2.69979292454605,-0.749683767780105));
#88308=CARTESIAN_POINT('Ctrl Pts',(-1.99397524388836,2.09670858668745,1.85869814963478));
#88309=CARTESIAN_POINT('Ctrl Pts',(-1.83543203989851,-0.420553593951653,
2.77021160836216));
#88310=CARTESIAN_POINT('Ctrl Pts',(-1.70724366130071,-2.14539904246319,
1.46238996746531));
#88311=CARTESIAN_POINT('Ctrl Pts',(-1.6319030173662,-2.36942636739278,0.337281169716417));
#88312=CARTESIAN_POINT('Ctrl Pts',(-1.60941010809497,-2.36824184279273,
0.0009293627098712));
#88313=CARTESIAN_POINT('Origin',(-17.306589891905,0.,0.));
#88314=CARTESIAN_POINT('',(-3.80658989190501,-2.36789197928635,0.000123222714106244));
#88315=CARTESIAN_POINT('',(-3.60941010809497,-2.37278677064178,-0.00203906005744159));
#88316=CARTESIAN_POINT('',(-17.306589891905,-2.37175,-2.3095687792789E-13));
#88317=CARTESIAN_POINT('Ctrl Pts',(-3.80658989190501,-2.36789197928635,
0.000123222714106461));
#88318=CARTESIAN_POINT('Ctrl Pts',(-3.77966089618702,-2.36770476616414,
-0.402711191484291));
#88319=CARTESIAN_POINT('Ctrl Pts',(-3.69988416580574,-2.07903988532791,
-1.59635363341212));
#88320=CARTESIAN_POINT('Ctrl Pts',(-3.56725970076119,-0.187703149434983,
-2.79565599393456));
#88321=CARTESIAN_POINT('Ctrl Pts',(-3.40871649677134,2.24461739453909,-1.67708606749907));
#88322=CARTESIAN_POINT('Ctrl Pts',(-3.25017329278149,2.6277487863971,0.972553944787357));
#88323=CARTESIAN_POINT('Ctrl Pts',(-3.09163008879163,0.611917125250802,
2.73431570350978));
#88324=CARTESIAN_POINT('Ctrl Pts',(-2.94376895516614,-1.78909631603478,
2.0493130260116));
#88325=CARTESIAN_POINT('Ctrl Pts',(-2.84875555620393,-2.36673022379259,
0.625587765309121));
#88326=CARTESIAN_POINT('Ctrl Pts',(-2.80658989190501,-2.37248282482123,
-0.00208852864143679));
#88327=CARTESIAN_POINT('Ctrl Pts',(-3.60941010809497,-2.37278677064178,
-0.0020390600574414));
#88328=CARTESIAN_POINT('Ctrl Pts',(-3.59940916665894,-2.37413802781993,
-0.15086348359909));
#88329=CARTESIAN_POINT('Ctrl Pts',(-3.53656049055962,-2.29366732089097,
-1.08466088751338));
#88330=CARTESIAN_POINT('Ctrl Pts',(-3.42086407979702,-1.05522311535154,
-2.59565560789489));
#88331=CARTESIAN_POINT('Ctrl Pts',(-3.26232087580717,1.60521408013114,-2.29656519618435));
#88332=CARTESIAN_POINT('Ctrl Pts',(-3.10377767181731,2.80019550906176,0.0991393121454807));
#88333=CARTESIAN_POINT('Ctrl Pts',(-2.94523446782747,1.43878146837926,2.40433608377855));
#88334=CARTESIAN_POINT('Ctrl Pts',(-2.78669126383761,-1.23614652569664,
2.51453101646264));
#88335=CARTESIAN_POINT('Ctrl Pts',(-2.67474981059345,-2.32800632564574,
0.971495952065517));
#88336=CARTESIAN_POINT('Ctrl Pts',(-2.61565609201257,-2.37502476399855,
0.0943153871308459));
#88337=CARTESIAN_POINT('Ctrl Pts',(-2.60941010809497,-2.3743301036074,0.00152562654522945));
#88338=CARTESIAN_POINT('Origin',(-17.306589891905,0.,0.));
#88339=CARTESIAN_POINT('',(-4.80658989190501,-2.37293245461563,0.00201017445689671));
#88340=CARTESIAN_POINT('',(-4.60941010809497,-2.36788667271892,-4.29541209298612E-5));
#88341=CARTESIAN_POINT('',(-17.306589891905,-2.37175,-2.3095687792789E-13));
#88342=CARTESIAN_POINT('Ctrl Pts',(-4.80658989190501,-2.37293245461563,
0.00201017445689676));
#88343=CARTESIAN_POINT('Ctrl Pts',(-4.76341397083339,-2.36713986096666,
-0.640390818759947));
#88344=CARTESIAN_POINT('Ctrl Pts',(-4.66739031509848,-1.76624041701385,
-2.07864193942938));
#88345=CARTESIAN_POINT('Ctrl Pts',(-4.51851892470029,0.663872292187274,
-2.72216797540702));
#88346=CARTESIAN_POINT('Ctrl Pts',(-4.35997572071044,2.64579147695974,-0.922340700408471));
#88347=CARTESIAN_POINT('Ctrl Pts',(-4.20143251672059,2.21227577950313,1.71952341690803));
#88348=CARTESIAN_POINT('Ctrl Pts',(-4.04288931273074,-0.24090327052083,
2.79157491766907));
#88349=CARTESIAN_POINT('Ctrl Pts',(-3.91127510445888,-2.09482974284144,
1.56588393431461));
#88350=CARTESIAN_POINT('Ctrl Pts',(-3.8325086308503,-2.36807216900053,0.387845072022191));
#88351=CARTESIAN_POINT('Ctrl Pts',(-3.80658989190501,-2.36789197928635,
0.000123222714106461));
#88352=CARTESIAN_POINT('Ctrl Pts',(-4.60941010809497,-2.36788667271892,
-4.29541209298265E-5));
#88353=CARTESIAN_POINT('Ctrl Pts',(-4.58316224130531,-2.36795027473895,
-0.392690372317799));
#88354=CARTESIAN_POINT('Ctrl Pts',(-4.50406663985236,-2.08972978198754,
-1.57581348531183));
#88355=CARTESIAN_POINT('Ctrl Pts',(-4.37212330373612,-0.223580041071285,
-2.79301553794379));
#88356=CARTESIAN_POINT('Ctrl Pts',(-4.21358009974628,2.22290076086175,-1.70576552913832));
#88357=CARTESIAN_POINT('Ctrl Pts',(-4.05503689575642,2.64001829300782,0.938737043143364));
#88358=CARTESIAN_POINT('Ctrl Pts',(-3.89649369176657,0.646971487662433,
2.7262339822803));
#88359=CARTESIAN_POINT('Ctrl Pts',(-3.74795142921276,-1.77373833013654,
2.06910028661809));
#88360=CARTESIAN_POINT('Ctrl Pts',(-3.65225690132222,-2.36699761196315,
0.63556584378477));
#88361=CARTESIAN_POINT('Ctrl Pts',(-3.60941010809497,-2.37278677064178,
-0.0020390600574414));
#88362=CARTESIAN_POINT('Origin',(-17.306589891905,0.,0.));
#88363=CARTESIAN_POINT('',(-5.80658989190502,-2.37420921644579,-0.00158594309364022));
#88364=CARTESIAN_POINT('',(-5.60941010809497,-2.37263003492395,0.00206636748989852));
#88365=CARTESIAN_POINT('',(-17.306589891905,-2.37175,-2.3095687792789E-13));
#88366=CARTESIAN_POINT('Ctrl Pts',(-5.80658989190502,-2.37420921644579,
-0.00158594309364031));
#88367=CARTESIAN_POINT('Ctrl Pts',(-5.80001478014305,-2.37496212800069,
-0.0992782592791646));
#88368=CARTESIAN_POINT('Ctrl Pts',(-5.74059193371779,-2.32517322677813,
-0.981403206808898));
#88369=CARTESIAN_POINT('Ctrl Pts',(-5.62832135262924,-1.2205227666753,-2.52215167718616));
#88370=CARTESIAN_POINT('Ctrl Pts',(-5.4697781486394,1.45366996224847,-2.39536396974682));
#88371=CARTESIAN_POINT('Ctrl Pts',(-5.31123494464955,2.8007569218186,-0.0817653447559351));
#88372=CARTESIAN_POINT('Ctrl Pts',(-5.15269174065969,1.59093566559739,2.30647970175859));
#88373=CARTESIAN_POINT('Ctrl Pts',(-4.99414853666984,-1.07130598541964,
2.58905936438303));
#88374=CARTESIAN_POINT('Ctrl Pts',(-4.87878125375162,-2.29685610505972,
1.07473064721425));
#88375=CARTESIAN_POINT('Ctrl Pts',(-4.81626170549667,-2.37423005023362,
0.145914056604193));
#88376=CARTESIAN_POINT('Ctrl Pts',(-4.80658989190501,-2.37293245461563,
0.00201017445689676));
#88377=CARTESIAN_POINT('Ctrl Pts',(-5.60941010809497,-2.37263003492395,
0.00206636748989856));
#88378=CARTESIAN_POINT('Ctrl Pts',(-5.56691531595168,-2.36685493862076,
-0.630408109289954));
#88379=CARTESIAN_POINT('Ctrl Pts',(-5.4715727891451,-1.78170188936919,-2.05888119862122));
#88380=CARTESIAN_POINT('Ctrl Pts',(-5.32338252767523,0.628868639624235,
-2.73046663851582));
#88381=CARTESIAN_POINT('Ctrl Pts',(-5.16483932368538,2.63373164752747,-0.956232941728888));
#88382=CARTESIAN_POINT('Ctrl Pts',(-5.00629611969553,2.23416961039886,1.6909790010008));
#88383=CARTESIAN_POINT('Ctrl Pts',(-4.84775291570567,-0.205043418049532,
2.79443751524972));
#88384=CARTESIAN_POINT('Ctrl Pts',(-4.71545757850549,-2.08422822423836,
1.58643001607205));
#88385=CARTESIAN_POINT('Ctrl Pts',(-4.63600997596859,-2.36782221775416,
0.397870123107349));
#88386=CARTESIAN_POINT('Ctrl Pts',(-4.60941010809497,-2.36788667271892,
-4.29541209298265E-5));
#88387=CARTESIAN_POINT('Origin',(-17.306589891905,0.,0.));
#88388=CARTESIAN_POINT('',(-6.80658989190501,-2.36818083915218,-0.0008555996482021));
#88389=CARTESIAN_POINT('',(-6.60941010809497,-2.37445554261321,-0.00145817468174603));
#88390=CARTESIAN_POINT('',(-17.306589891905,-2.37175,-2.3095687792789E-13));
#88391=CARTESIAN_POINT('Ctrl Pts',(-6.80658989190501,-2.36818083915218,
-0.00085559964820188));
#88392=CARTESIAN_POINT('Ctrl Pts',(-6.78376785478941,-2.36929017234292,
-0.342149481798462));
#88393=CARTESIAN_POINT('Ctrl Pts',(-6.70809808301052,-2.14074935415041,
-1.47234264798851));
#88394=CARTESIAN_POINT('Ctrl Pts',(-6.57958057656835,-0.403348751247113,
-2.77276661325373));
#88395=CARTESIAN_POINT('Ctrl Pts',(-6.42103737257851,2.10819389270592,-1.84565528132004));
#88396=CARTESIAN_POINT('Ctrl Pts',(-6.26249416858865,2.69509315088937,0.766418824623061));
#88397=CARTESIAN_POINT('Ctrl Pts',(-6.1039509645988,0.821548317644948,2.6788025810951));
#88398=CARTESIAN_POINT('Ctrl Pts',(-5.95198287237092,-1.69321188063458,
2.16772687694675));
#88399=CARTESIAN_POINT('Ctrl Pts',(-5.85286251480633,-2.36891057001675,
0.685927801289234));
#88400=CARTESIAN_POINT('Ctrl Pts',(-5.80658989190502,-2.37420921644579,
-0.00158594309364031));
#88401=CARTESIAN_POINT('Ctrl Pts',(-6.60941010809497,-2.37445554261321,
-0.00145817468174572));
#88402=CARTESIAN_POINT('Ctrl Pts',(-6.60351612526133,-2.37508875977735,
-0.0890065105479783));
#88403=CARTESIAN_POINT('Ctrl Pts',(-6.5447744077644,-2.33100010852313,-0.960902990558076));
#88404=CARTESIAN_POINT('Ctrl Pts',(-6.43318495560419,-1.2528030468829,-2.50627379902584));
#88405=CARTESIAN_POINT('Ctrl Pts',(-6.27464175161433,1.42279687533745,-2.41382950547303));
#88406=CARTESIAN_POINT('Ctrl Pts',(-6.11609854762448,2.79947614093066,-0.117716465815816));
#88407=CARTESIAN_POINT('Ctrl Pts',(-5.95755534363463,1.62041646007026,2.285864021742));
#88408=CARTESIAN_POINT('Ctrl Pts',(-5.79901213964478,-1.0379776562294,2.60259989532173));
#88409=CARTESIAN_POINT('Ctrl Pts',(-5.68296372779822,-2.2902184224173,1.09528349834256));
#88410=CARTESIAN_POINT('Ctrl Pts',(-5.61976305061496,-2.37403701298076,
0.156155176334485));
#88411=CARTESIAN_POINT('Ctrl Pts',(-5.60941010809497,-2.37263003492395,
0.00206636748989856));
#88412=CARTESIAN_POINT('Origin',(-17.306589891905,0.,0.));
#88413=CARTESIAN_POINT('',(-7.80658989190501,-2.37109816127964,0.00213708253619841));
#88414=CARTESIAN_POINT('',(-7.60941010809498,-2.36830089438249,-0.00100592404030236));
#88415=CARTESIAN_POINT('',(-17.306589891905,-2.37175,-2.3095687792789E-13));
#88416=CARTESIAN_POINT('Ctrl Pts',(-7.80658989190501,-2.37109816127964,
0.0021370825361984));
#88417=CARTESIAN_POINT('Ctrl Pts',(-7.76752092943578,-2.36593601989977,
-0.580311471015131));
#88418=CARTESIAN_POINT('Ctrl Pts',(-7.67560423230326,-1.85624009305816,
-1.9587052675019));
#88419=CARTESIAN_POINT('Ctrl Pts',(-7.53083980050746,0.451359570691226,
-2.76535701938333));
#88420=CARTESIAN_POINT('Ctrl Pts',(-7.37229659651761,2.56653624207177,-1.1241959904035));
#88421=CARTESIAN_POINT('Ctrl Pts',(-7.21375339252775,2.33863288664257,1.54328258210251));
#88422=CARTESIAN_POINT('Ctrl Pts',(-7.05521018853791,-0.0242896112824878,
2.80184491388995));
#88423=CARTESIAN_POINT('Ctrl Pts',(-6.91948902166366,-2.02809044884209,
1.68954352771679));
#88424=CARTESIAN_POINT('Ctrl Pts',(-6.83661558945269,-2.36672135055807,
0.448165967901147));
#88425=CARTESIAN_POINT('Ctrl Pts',(-6.80658989190501,-2.36818083915218,
-0.00085559964820188));
#88426=CARTESIAN_POINT('Ctrl Pts',(-7.60941010809498,-2.36830089438249,
-0.00100592404030229));
#88427=CARTESIAN_POINT('Ctrl Pts',(-7.5872691999077,-2.36956993952812,-0.332071764583063));
#88428=CARTESIAN_POINT('Ctrl Pts',(-7.51228055705713,-2.15035683272869,
-1.45174667900709));
#88429=CARTESIAN_POINT('Ctrl Pts',(-7.38444417954329,-0.438913988766854,
-2.76735945269628));
#88430=CARTESIAN_POINT('Ctrl Pts',(-7.22590097555344,2.08432431928549,-1.87256934771392));
#88431=CARTESIAN_POINT('Ctrl Pts',(-7.06735777156358,2.70471060372122,0.731754316748925));
#88432=CARTESIAN_POINT('Ctrl Pts',(-6.90881456757374,0.855872690191172,
2.66803406427797));
#88433=CARTESIAN_POINT('Ctrl Pts',(-6.75616534641753,-1.67654134756637,
2.18714080723266));
#88434=CARTESIAN_POINT('Ctrl Pts',(-6.65636385992461,-2.36941108924122,
0.695985803589395));
#88435=CARTESIAN_POINT('Ctrl Pts',(-6.60941010809497,-2.37445554261321,
-0.00145817468174572));
#88436=CARTESIAN_POINT('Origin',(-17.306589891905,0.,0.));
#88437=CARTESIAN_POINT('',(-8.80658989190501,-2.37538658813648,-0.000666706255725389));
#88438=CARTESIAN_POINT('',(-8.60941010809498,-2.37080369071248,0.00210958135937009));
#88439=CARTESIAN_POINT('',(-17.306589891905,-2.37175,-2.3095687792789E-13));
#88440=CARTESIAN_POINT('Ctrl Pts',(-8.80658989190501,-2.37538658813648,
-0.000666706255725148));
#88441=CARTESIAN_POINT('Ctrl Pts',(-8.80412173874543,-2.37552348369093,
-0.0372902868490661));
#88442=CARTESIAN_POINT('Ctrl Pts',(-8.74880585092257,-2.35817895798474,
-0.857960161496038));
#88443=CARTESIAN_POINT('Ctrl Pts',(-8.64064222843641,-1.41192306630101,
-2.42020622293936));
#88444=CARTESIAN_POINT('Ctrl Pts',(-8.48209902444656,1.26406585736851,-2.50061240797977));
#88445=CARTESIAN_POINT('Ctrl Pts',(-8.32355582045671,2.78604518069765,-0.298122722747819));
#88446=CARTESIAN_POINT('Ctrl Pts',(-8.16501261646686,1.76454714739586,2.17653354472756));
#88447=CARTESIAN_POINT('Ctrl Pts',(-8.00646941247701,-0.867867228973001,
2.66415678584837));
#88448=CARTESIAN_POINT('Ctrl Pts',(-7.88699517095639,-2.25452734930914,
1.19877087178493));
#88449=CARTESIAN_POINT('Ctrl Pts',(-7.82036866409906,-2.37291873611991,
0.207554002436673));
#88450=CARTESIAN_POINT('Ctrl Pts',(-7.80658989190501,-2.37109816127964,
0.0021370825361984));
#88451=CARTESIAN_POINT('Ctrl Pts',(-8.60941010809498,-2.37080369071248,
0.00210958135936995));
#88452=CARTESIAN_POINT('Ctrl Pts',(-8.57102227455407,-2.36584710075431,
-0.570365230392202));
#88453=CARTESIAN_POINT('Ctrl Pts',(-8.47978670634988,-1.87042622880759,
-1.93864657712568));
#88454=CARTESIAN_POINT('Ctrl Pts',(-8.33570340348239,0.415818959741428,
-2.77092374898376));
#88455=CARTESIAN_POINT('Ctrl Pts',(-8.17716019949255,2.55189140603955,-1.15705405307796));
#88456=CARTESIAN_POINT('Ctrl Pts',(-8.0186169955027,2.35825360470366,1.51313045236188));
#88457=CARTESIAN_POINT('Ctrl Pts',(-7.86007379151283,0.0116842262656824,
2.80192564298541));
#88458=CARTESIAN_POINT('Ctrl Pts',(-7.72367149571027,-2.01635883652552,
1.70998943732583));
#88459=CARTESIAN_POINT('Ctrl Pts',(-7.64011693457098,-2.36654087854452,
0.458143322760719));
#88460=CARTESIAN_POINT('Ctrl Pts',(-7.60941010809498,-2.36830089438249,
-0.00100592404030229));
#88461=CARTESIAN_POINT('Origin',(-17.306589891905,0.,0.));
#88462=CARTESIAN_POINT('',(-9.80658989190502,-2.36918623645893,-0.00165592778327176));
#88463=CARTESIAN_POINT('',(-9.60941010809498,-2.3754933284252,-0.000487244657051689));
#88464=CARTESIAN_POINT('',(-17.306589891905,-2.37175,-2.3095687792789E-13));
#88465=CARTESIAN_POINT('Ctrl Pts',(-9.80658989190502,-2.36918623645893,
-0.00165592778327162));
#88466=CARTESIAN_POINT('Ctrl Pts',(-9.7878748133918,-2.37099294971461,-0.281234334838761));
#88467=CARTESIAN_POINT('Ctrl Pts',(-9.7163120002153,-2.19606353177059,-1.34810002136817));
#88468=CARTESIAN_POINT('Ctrl Pts',(-9.59190145237552,-0.616578301017466,
-2.733268392497));
#88469=CARTESIAN_POINT('Ctrl Pts',(-9.43335824838566,1.95914233809709,-2.00316904074074));
#88470=CARTESIAN_POINT('Ctrl Pts',(-9.27481504439582,2.74629392962736,0.555692863728672));
#88471=CARTESIAN_POINT('Ctrl Pts',(-9.11627184040596,1.02625846150236,2.60724346329648));
#88472=CARTESIAN_POINT('Ctrl Pts',(-8.9601967895757,-1.58932149542791,2.28366798664447));
#88473=CARTESIAN_POINT('Ctrl Pts',(-8.85696947340871,-2.37259229609025,
0.746888467253723));
#88474=CARTESIAN_POINT('Ctrl Pts',(-8.80658989190501,-2.37538658813648,
-0.000666706255725148));
#88475=CARTESIAN_POINT('Ctrl Pts',(-9.60941010809498,-2.3754933284252,-0.000487244657051797));
#88476=CARTESIAN_POINT('Ctrl Pts',(-9.60762308386372,-2.37556787913775,
-0.0270007296449992));
#88477=CARTESIAN_POINT('Ctrl Pts',(-9.55298832496918,-2.36316749088712,
-0.837527098122419));
#88478=CARTESIAN_POINT('Ctrl Pts',(-9.44550583141135,-1.4428787190723,-2.40187943744293));
#88479=CARTESIAN_POINT('Ctrl Pts',(-9.2869626274215,1.23185716520365,-2.51663500621346));
#88480=CARTESIAN_POINT('Ctrl Pts',(-9.12841942343165,2.78198788226743,-0.333867118596373));
#88481=CARTESIAN_POINT('Ctrl Pts',(-8.96987621944179,1.79234529127704,2.15369965101908));
#88482=CARTESIAN_POINT('Ctrl Pts',(-8.81133301545195,-0.833591533278391,
2.67507924847269));
#88483=CARTESIAN_POINT('Ctrl Pts',(-8.691177645003,-2.24696283819461,1.21936495983762));
#88484=CARTESIAN_POINT('Ctrl Pts',(-8.62387000921735,-2.37267073540056,
0.217748975652233));
#88485=CARTESIAN_POINT('Ctrl Pts',(-8.60941010809498,-2.37080369071248,
0.00210958135936995));
#88486=CARTESIAN_POINT('Origin',(-17.306589891905,0.,0.));
#88487=CARTESIAN_POINT('',(-10.806589891905,-2.36946338337721,0.00177935167763374));
#88488=CARTESIAN_POINT('',(-10.609410108095,-2.36941210437275,-0.00175842403990767));
#88489=CARTESIAN_POINT('',(-17.306589891905,-2.37175,-2.3095687792789E-13));
#88490=CARTESIAN_POINT('Ctrl Pts',(-10.806589891905,-2.36946338337721,0.00177935167763384));
#88491=CARTESIAN_POINT('Ctrl Pts',(-10.7716278880382,-2.36580882662732,
-0.520352810821665));
#88492=CARTESIAN_POINT('Ctrl Pts',(-10.683818149508,-1.93866057672306,-1.837161940075));
#88493=CARTESIAN_POINT('Ctrl Pts',(-10.5431606763146,0.236143210481572,
-2.79198160648));
#88494=CARTESIAN_POINT('Ctrl Pts',(-10.3846174723248,2.47190748456146,-1.31931735926746));
#88495=CARTESIAN_POINT('Ctrl Pts',(-10.2260742683349,2.45098160937866,1.35779750227409));
#88496=CARTESIAN_POINT('Ctrl Pts',(-10.0675310643451,0.192469542788204,
2.79533189117441));
#88497=CARTESIAN_POINT('Ctrl Pts',(-9.92770293886843,-1.9544090201471,1.81246152264369));
#88498=CARTESIAN_POINT('Ctrl Pts',(-9.84072254805508,-2.36589114355968,
0.508240604484572));
#88499=CARTESIAN_POINT('Ctrl Pts',(-9.80658989190502,-2.36918623645893,
-0.00165592778327162));
#88500=CARTESIAN_POINT('Ctrl Pts',(-10.609410108095,-2.36941210437275,-0.00175842403990777));
#88501=CARTESIAN_POINT('Ctrl Pts',(-10.5913761585101,-2.3712723507284,-0.271096991132142));
#88502=CARTESIAN_POINT('Ctrl Pts',(-10.5204944742619,-2.2046407678535,-1.32748836904326));
#88503=CARTESIAN_POINT('Ctrl Pts',(-10.3967650553504,-0.651618847034371,
-2.72512691597345));
#88504=CARTESIAN_POINT('Ctrl Pts',(-10.2382218513606,1.93326279954282,-2.02815649737983));
#88505=CARTESIAN_POINT('Ctrl Pts',(-10.0796786473708,2.75320172762965,0.520388390472216));
#88506=CARTESIAN_POINT('Ctrl Pts',(-9.9211354433809,1.05964722747713,2.59385265257382));
#88507=CARTESIAN_POINT('Ctrl Pts',(-9.76437926362231,-1.57130311251203,
2.30261886074424));
#88508=CARTESIAN_POINT('Ctrl Pts',(-9.660470818527,-2.37336318811748,0.757083557032393));
#88509=CARTESIAN_POINT('Ctrl Pts',(-9.60941010809498,-2.3754933284252,-0.000487244657051797));
#88510=CARTESIAN_POINT('Origin',(-17.306589891905,0.,0.));
#88511=CARTESIAN_POINT('',(-11.806589891905,-2.37551264984338,0.00044757161090019));
#88512=CARTESIAN_POINT('',(-11.609410108095,-2.36923398858465,0.00167909690344512));
#88513=CARTESIAN_POINT('',(-17.306589891905,-2.37175,-2.3095687792789E-13));
#88514=CARTESIAN_POINT('Ctrl Pts',(-11.806589891905,-2.37551264984338,0.000447571610900214));
#88515=CARTESIAN_POINT('Ctrl Pts',(-11.7553809626845,-2.37353748313963,
-0.759305924460025));
#88516=CARTESIAN_POINT('Ctrl Pts',(-11.6513242988008,-1.56735232559126,
-2.30673160249233));
#88517=CARTESIAN_POINT('Ctrl Pts',(-11.4944199002537,1.06689001235037,-2.59088220714646));
#88518=CARTESIAN_POINT('Ctrl Pts',(-11.3358766962639,2.75464506089428,-0.512694348708331));
#88519=CARTESIAN_POINT('Ctrl Pts',(-11.177333492274,1.92758901194037,2.03354997649873));
#88520=CARTESIAN_POINT('Ctrl Pts',(-11.0187902882842,-0.659229957733515,
2.7232959387495));
#88521=CARTESIAN_POINT('Ctrl Pts',(-10.8952090881612,-2.20648540280323,
1.32300329267972));
#88522=CARTESIAN_POINT('Ctrl Pts',(-10.8244756227015,-2.37133296781115,
0.268889764861912));
#88523=CARTESIAN_POINT('Ctrl Pts',(-10.806589891905,-2.36946338337721,0.00177935167763384));
#88524=CARTESIAN_POINT('Ctrl Pts',(-11.609410108095,-2.36923398858465,0.00167909690344501));
#88525=CARTESIAN_POINT('Ctrl Pts',(-11.5751292331565,-2.36587390366334,
-0.510405547231816));
#88526=CARTESIAN_POINT('Ctrl Pts',(-11.4880006235547,-1.95161611255133,
-1.81687917165628));
#88527=CARTESIAN_POINT('Ctrl Pts',(-11.3480242792896,0.200278529009738,
-2.79478305799562));
#88528=CARTESIAN_POINT('Ctrl Pts',(-11.1894810752997,2.45476536426573,-1.35094442384648));
#88529=CARTESIAN_POINT('Ctrl Pts',(-11.0309378713099,2.46821168687189,1.3262182696089));
#88530=CARTESIAN_POINT('Ctrl Pts',(-10.87239466732,0.228341882252721,2.79263026819601));
#88531=CARTESIAN_POINT('Ctrl Pts',(-10.731885412915,-1.94149674627528,1.83275085496228));
#88532=CARTESIAN_POINT('Ctrl Pts',(-10.6442238931734,-2.36582097662153,
0.518188409787725));
#88533=CARTESIAN_POINT('Ctrl Pts',(-10.609410108095,-2.36941210437275,-0.00175842403990777));
#88534=CARTESIAN_POINT('Origin',(-17.306589891905,0.,0.));
#88535=CARTESIAN_POINT('',(-12.806589891905,-2.37074071993608,-0.00210182595080978));
#88536=CARTESIAN_POINT('',(-12.609410108095,-2.3754122575152,0.00062808862859861));
#88537=CARTESIAN_POINT('',(-17.306589891905,-2.37175,-2.3095687792789E-13));
#88538=CARTESIAN_POINT('Ctrl Pts',(-12.806589891905,-2.37074071993608,-0.00210182595080953));
#88539=CARTESIAN_POINT('Ctrl Pts',(-12.7919817719942,-2.37261602100814,
-0.219966362853848));
#88540=CARTESIAN_POINT('Ctrl Pts',(-12.7245259174201,-2.24529599511548,
-1.22384721227819));
#88541=CARTESIAN_POINT('Ctrl Pts',(-12.6042223281827,-0.826114542781323,
-2.67739786594892));
#88542=CARTESIAN_POINT('Ctrl Pts',(-12.4456791241928,1.79835553752813,-2.1486838716176));
#88543=CARTESIAN_POINT('Ctrl Pts',(-12.287135920203,2.78104444218098,0.341638325206172));
#88544=CARTESIAN_POINT('Ctrl Pts',(-12.1285927162131,1.22482132733881,2.52006697848072));
#88545=CARTESIAN_POINT('Ctrl Pts',(-11.9700495122233,-1.4495836885253,2.39783903872389));
#88546=CARTESIAN_POINT('Ctrl Pts',(-11.8627152374539,-2.36423530914187,
0.833082325119274));
#88547=CARTESIAN_POINT('Ctrl Pts',(-11.8082286973478,-2.37557585979512,
0.024761459511004));
#88548=CARTESIAN_POINT('Ctrl Pts',(-11.806589891905,-2.37551264984338,0.000447571610900214));
#88549=CARTESIAN_POINT('Ctrl Pts',(-12.609410108095,-2.3754122575152,0.000628088628598614));
#88550=CARTESIAN_POINT('Ctrl Pts',(-12.5588823078028,-2.37275587159386,
-0.749104589840911));
#88551=CARTESIAN_POINT('Ctrl Pts',(-12.4555067728474,-1.58541971420767,
-2.28779889543668));
#88552=CARTESIAN_POINT('Ctrl Pts',(-12.2992835032286,1.03353864319095,-2.60436589634899));
#88553=CARTESIAN_POINT('Ctrl Pts',(-12.1407402992388,2.74783554884452,-0.548017908917588));
#88554=CARTESIAN_POINT('Ctrl Pts',(-11.9821970952489,1.95353799427501,2.00863464286302));
#88555=CARTESIAN_POINT('Ctrl Pts',(-11.8236538912591,-0.624212206359067,
2.73153490815486));
#88556=CARTESIAN_POINT('Ctrl Pts',(-11.6993915622078,-2.19794407502757,
1.34361468192694));
#88557=CARTESIAN_POINT('Ctrl Pts',(-11.6279769678197,-2.37105384369362,
0.279029187060534));
#88558=CARTESIAN_POINT('Ctrl Pts',(-11.609410108095,-2.36923398858465,0.00167909690344501));
#88559=CARTESIAN_POINT('Origin',(-17.306589891905,0.,0.));
#88560=CARTESIAN_POINT('',(-13.806589891905,-2.36832932812376,0.00104049776686726));
#88561=CARTESIAN_POINT('',(-13.609410108095,-2.37103340387255,-0.00213221344230991));
#88562=CARTESIAN_POINT('',(-17.306589891905,-2.37175,-2.3095687792789E-13));
#88563=CARTESIAN_POINT('Ctrl Pts',(-13.806589891905,-2.36832932812376,0.00104049776686699));
#88564=CARTESIAN_POINT('Ctrl Pts',(-13.7757348466406,-2.36650353915635,
-0.460312200200009));
#88565=CARTESIAN_POINT('Ctrl Pts',(-13.6920320667128,-2.01378149179939,
-1.71444028663224));
#88566=CARTESIAN_POINT('Ctrl Pts',(-13.5554815521218,0.0195128928627424,
-2.80187936245463));
#88567=CARTESIAN_POINT('Ctrl Pts',(-13.3969383481319,2.36247174813047,-1.50653754623712));
#88568=CARTESIAN_POINT('Ctrl Pts',(-13.2383951441421,2.54864912756637,1.16418002319016));
#88569=CARTESIAN_POINT('Ctrl Pts',(-13.0798519401522,0.408075729452012,
2.77207444785609));
#88570=CARTESIAN_POINT('Ctrl Pts',(-12.9359168560732,-1.87348586078252,
1.93427633586112));
#88571=CARTESIAN_POINT('Ctrl Pts',(-12.8448295066575,-2.36583175211693,
0.568201266456078));
#88572=CARTESIAN_POINT('Ctrl Pts',(-12.806589891905,-2.37074071993608,-0.00210182595080953));
#88573=CARTESIAN_POINT('Ctrl Pts',(-13.609410108095,-2.37103340387255,-0.00213221344230973));
#88574=CARTESIAN_POINT('Ctrl Pts',(-13.5954831171125,-2.37286529370797,
-0.209773287942694));
#88575=CARTESIAN_POINT('Ctrl Pts',(-13.5287083914667,-2.25289472910887,
-1.2032522754709));
#88576=CARTESIAN_POINT('Ctrl Pts',(-13.4090859311576,-0.860420371114484,
-2.6665705025054));
#88577=CARTESIAN_POINT('Ctrl Pts',(-13.2505427271678,1.77062098199356,-2.17159522099969));
#88578=CARTESIAN_POINT('Ctrl Pts',(-13.0919995231779,2.78520124435443,0.305905452644607));
#88579=CARTESIAN_POINT('Ctrl Pts',(-12.9334563191881,1.25707446924262,2.50413403614118));
#88580=CARTESIAN_POINT('Ctrl Pts',(-12.7749131151982,-1.41867915221937,
2.41625193356046));
#88581=CARTESIAN_POINT('Ctrl Pts',(-12.6668977115005,-2.35927592169033,
0.853512735567485));
#88582=CARTESIAN_POINT('Ctrl Pts',(-12.6117300424661,-2.37553422286826,
0.0350513289019418));
#88583=CARTESIAN_POINT('Ctrl Pts',(-12.609410108095,-2.3754122575152,0.000628088628598614));
#88584=CARTESIAN_POINT('Origin',(-17.306589891905,0.,0.));
#88585=CARTESIAN_POINT('',(-14.806589891905,-2.37447732889499,0.00158904524625122));
#88586=CARTESIAN_POINT('',(-14.609410108095,-2.36819900096358,0.000905669814256771));
#88587=CARTESIAN_POINT('',(-17.306589891905,-2.37175,-2.3095687792789E-13));
#88588=CARTESIAN_POINT('Ctrl Pts',(-14.806589891905,-2.37447732889499,0.00158904524625127));
#88589=CARTESIAN_POINT('Ctrl Pts',(-14.7594879212869,-2.36948883111584,
-0.697977827885181));
#88590=CARTESIAN_POINT('Ctrl Pts',(-14.6595382160056,-1.67293185990106,
-2.19161085343155));
#88591=CARTESIAN_POINT('Ctrl Pts',(-14.5067407760609,0.863349698447385,
-2.66549172608374));
#88592=CARTESIAN_POINT('Ctrl Pts',(-14.348197572071,2.70673094384455,-0.724268682598567));
#88593=CARTESIAN_POINT('Ctrl Pts',(-14.1896543680812,2.07909181188049,1.87842405436525));
#88594=CARTESIAN_POINT('Ctrl Pts',(-14.0311111640913,-0.44664765932035,
2.76610238818825));
#88595=CARTESIAN_POINT('Ctrl Pts',(-13.9034230053659,-2.15242365769109,
1.44726882168644));
#88596=CARTESIAN_POINT('Ctrl Pts',(-13.8285825813038,-2.36963070393844,
0.329880935456426));
#88597=CARTESIAN_POINT('Ctrl Pts',(-13.806589891905,-2.36832932812376,0.00104049776686699));
#88598=CARTESIAN_POINT('Ctrl Pts',(-14.609410108095,-2.36819900096358,0.000905669814256944));
#88599=CARTESIAN_POINT('Ctrl Pts',(-14.5792361917588,-2.36667741525576,
-0.450328646933255));
#88600=CARTESIAN_POINT('Ctrl Pts',(-14.4962145407594,-2.02556427845193,
-1.69402330663087));
#88601=CARTESIAN_POINT('Ctrl Pts',(-14.3603451550967,-0.0164545272929353,
-2.80188230448376));
#88602=CARTESIAN_POINT('Ctrl Pts',(-14.2018019511069,2.34293162102215,-1.53675277767917));
#88603=CARTESIAN_POINT('Ctrl Pts',(-14.043258747117,2.56338713804141,1.13136735389903));
#88604=CARTESIAN_POINT('Ctrl Pts',(-13.8847155431272,0.443630763460945,
2.76660429639169));
#88605=CARTESIAN_POINT('Ctrl Pts',(-13.7400993301198,-1.8593443188828,1.95434500217413));
#88606=CARTESIAN_POINT('Ctrl Pts',(-13.6483308517758,-2.36591395525473,
0.578147119572609));
#88607=CARTESIAN_POINT('Ctrl Pts',(-13.609410108095,-2.37103340387255,-0.00213221344230973));
#88608=CARTESIAN_POINT('Origin',(-0.25,3.51939854619125E-16,0.));
#88609=CARTESIAN_POINT('Ctrl Pts',(-0.25,2.22665730523966,0.827839780511539));
#88610=CARTESIAN_POINT('Ctrl Pts',(-0.25,2.21253493697841,0.887066447970513));
#88611=CARTESIAN_POINT('Ctrl Pts',(-0.249999999999997,2.19601471711402,
0.945593270349512));
#88612=CARTESIAN_POINT('Ctrl Pts',(-0.249999999999997,2.17708701742544,
1.00327396853317));
#88613=CARTESIAN_POINT('Ctrl Pts',(-0.249999999999997,2.15165423815579,
1.08077839269253));
#88614=CARTESIAN_POINT('Ctrl Pts',(-0.250000000000005,2.12187728230406,
1.15675586863499));
#88615=CARTESIAN_POINT('Ctrl Pts',(-0.250000000000004,2.08808045010065,
1.23103089813193));
#88616=CARTESIAN_POINT('Ctrl Pts',(-0.250000000000003,2.06840578169053,
1.27426976051136));
#88617=CARTESIAN_POINT('Ctrl Pts',(-0.25,2.0473677896996,1.31693163959809));
#88618=CARTESIAN_POINT('Ctrl Pts',(-0.250000000000001,2.02502259951598,
1.35898078015481));
#88619=CARTESIAN_POINT('Ctrl Pts',(-0.250000000000001,2.01629265380112,
1.37540877702575));
#88620=CARTESIAN_POINT('Ctrl Pts',(-0.249999999999999,2.00736312468595,
1.39174323478388));
#88621=CARTESIAN_POINT('Ctrl Pts',(-0.249999999999999,1.99823713884684,
1.40798196099185));
#88622=CARTESIAN_POINT('Ctrl Pts',(-0.249999999999999,1.99115494736671,
1.42058397138565));
#88623=CARTESIAN_POINT('Ctrl Pts',(-0.250000000000001,1.98395548148856,
1.43312635989235));
#88624=CARTESIAN_POINT('Ctrl Pts',(-0.250000000000001,1.97664492917627,
1.4456004937163));
#88625=CARTESIAN_POINT('Ctrl Pts',(-0.250000000000002,1.93344420468633,
1.51931470784926));
#88626=CARTESIAN_POINT('Ctrl Pts',(-0.249999999999999,1.88632573736469,
1.59072308909904));
#88627=CARTESIAN_POINT('Ctrl Pts',(-0.249999999999999,1.83564389935666,
1.65963329088958));
#88628=CARTESIAN_POINT('Ctrl Pts',(-0.249999999999999,1.79139338401687,
1.71979906350653));
#88629=CARTESIAN_POINT('Ctrl Pts',(-0.249999999999997,1.74442536456685,
1.77806067486507));
#88630=CARTESIAN_POINT('Ctrl Pts',(-0.249999999999997,1.69494407121667,
1.8342821297957));
#88631=CARTESIAN_POINT('Ctrl Pts',(-0.249999999999997,1.67108524646734,
1.86139091676392));
#88632=CARTESIAN_POINT('Ctrl Pts',(-0.249999999999999,1.64664168508504,
1.88802522921354));
#88633=CARTESIAN_POINT('Ctrl Pts',(-0.25,1.62163414288635,1.91416882292567));
#88634=CARTESIAN_POINT('Ctrl Pts',(-0.25,1.606390797066,1.93010464887667));
#88635=CARTESIAN_POINT('Ctrl Pts',(-0.249999999999998,1.59093334989609,
1.94586244562507));
#88636=CARTESIAN_POINT('Ctrl Pts',(-0.249999999999998,1.57529127421572,
1.96141409772889));
#88637=CARTESIAN_POINT('Ctrl Pts',(-0.249999999999998,1.51243278415657,
2.02390921596938));
#88638=CARTESIAN_POINT('Ctrl Pts',(-0.249999999999999,1.44653991914015,
2.08313958788272));
#88639=CARTESIAN_POINT('Ctrl Pts',(-0.249999999999999,1.37797049065438,
2.13890775763005));
#88640=CARTESIAN_POINT('Ctrl Pts',(-0.249999999999998,1.30477974292812,
2.19843449036313));
#88641=CARTESIAN_POINT('Ctrl Pts',(-0.249999999999999,1.22853932099898,
2.25401777387017));
#88642=CARTESIAN_POINT('Ctrl Pts',(-0.249999999999998,1.14962650113067,
2.30539173571991));
#88643=CARTESIAN_POINT('Ctrl Pts',(-0.249999999999998,1.09044188622944,
2.34392220710722));
#88644=CARTESIAN_POINT('Ctrl Pts',(-0.25,1.02975273329805,2.38008449190169));
#88645=CARTESIAN_POINT('Ctrl Pts',(-0.25,0.967700507001693,2.41375165933649));
#88646=CARTESIAN_POINT('Ctrl Pts',(-0.250000000000001,0.921161337279424,
2.43900203491258));
#88647=CARTESIAN_POINT('Ctrl Pts',(-0.249999999999997,0.873855113607986,
2.46284866395087));
#88648=CARTESIAN_POINT('Ctrl Pts',(-0.249999999999997,0.825837112674175,
2.48523195686642));
#88649=CARTESIAN_POINT('Ctrl Pts',(-0.249999999999997,0.812484513410199,
2.4914561880859));
#88650=CARTESIAN_POINT('Ctrl Pts',(-0.249999999999995,0.799076856063629,
2.49756723169206));
#88651=CARTESIAN_POINT('Ctrl Pts',(-0.249999999999995,0.785615286660712,
2.50356372448443));
#88652=CARTESIAN_POINT('Ctrl Pts',(-0.249999999999995,0.772636490123328,
2.5093451647876));
#88653=CARTESIAN_POINT('Ctrl Pts',(-0.250000000000001,0.759614812827758,
2.51501686886279));
#88654=CARTESIAN_POINT('Ctrl Pts',(-0.250000000000001,0.746556237332744,
2.52057598998014));
#88655=CARTESIAN_POINT('Ctrl Pts',(-0.250000000000002,0.661371947117411,
2.55683950025228));
#88656=CARTESIAN_POINT('Ctrl Pts',(-0.249999999999992,0.574557887090518,
2.58834304940443));
#88657=CARTESIAN_POINT('Ctrl Pts',(-0.249999999999994,0.48646010071724,
2.61485457170675));
#88658=CARTESIAN_POINT('Ctrl Pts',(-0.249999999999995,0.450950611910523,
2.62554054513694));
#88659=CARTESIAN_POINT('Ctrl Pts',(-0.250000000000001,0.415232105718096,
2.6354151139179));
#88660=CARTESIAN_POINT('Ctrl Pts',(-0.250000000000001,0.379325561708904,
2.64446137371408));
#88661=CARTESIAN_POINT('Ctrl Pts',(-0.25,0.2933372621455,2.66612518232464));
#88662=CARTESIAN_POINT('Ctrl Pts',(-0.249999999999999,0.206272069189806,
2.68304215953505));
#88663=CARTESIAN_POINT('Ctrl Pts',(-0.249999999999998,0.11844610394434,
2.69538014091633));
#88664=CARTESIAN_POINT('Ctrl Pts',(-0.249999999999998,0.0288600713565845,
2.70796538036119));
#88665=CARTESIAN_POINT('Ctrl Pts',(-0.249999999999999,-0.0615182634234459,
2.71578635010443));
#88666=CARTESIAN_POINT('Ctrl Pts',(-0.249999999999998,-0.152370710138942,
2.71896997432629));
#88667=CARTESIAN_POINT('Ctrl Pts',(-0.249999999999998,-0.17073330596056,
2.71961343090833));
#88668=CARTESIAN_POINT('Ctrl Pts',(-0.249999999999995,-0.189115303514798,
2.7200672839337));
#88669=CARTESIAN_POINT('Ctrl Pts',(-0.249999999999995,-0.20751411631365,
2.72033232888479));
#88670=CARTESIAN_POINT('Ctrl Pts',(-0.249999999999994,-0.221324751245115,
2.72053127862683));
#88671=CARTESIAN_POINT('Ctrl Pts',(-0.25,-0.235143715204858,2.72062376322601));
#88672=CARTESIAN_POINT('Ctrl Pts',(-0.25,-0.248957210752076,2.72061034785803));
#88673=CARTESIAN_POINT('Ctrl Pts',(-0.250000000000001,-0.341482715415868,
2.72052048908994));
#88674=CARTESIAN_POINT('Ctrl Pts',(-0.249999999999998,-0.433912331818891,
2.71568618768959));
#88675=CARTESIAN_POINT('Ctrl Pts',(-0.249999999999999,-0.525897798319606,
2.70631418714313));
#88676=CARTESIAN_POINT('Ctrl Pts',(-0.249999999999999,-0.619674068827689,
2.69675972933713));
#88677=CARTESIAN_POINT('Ctrl Pts',(-0.25,-0.712989524571036,2.68248921578258));
#88678=CARTESIAN_POINT('Ctrl Pts',(-0.249999999999999,-0.805492806230512,
2.66366898531223));
#88679=CARTESIAN_POINT('Ctrl Pts',(-0.249999999999997,-0.898813914036067,
2.64468236424171));
#88680=CARTESIAN_POINT('Ctrl Pts',(-0.249999999999998,-0.991309340568736,
2.62106517248096));
#88681=CARTESIAN_POINT('Ctrl Pts',(-0.249999999999997,-1.08262302389016,
2.59293522572841));
#88682=CARTESIAN_POINT('Ctrl Pts',(-0.249999999999997,-1.1353317955791,
2.57669784610389));
#88683=CARTESIAN_POINT('Ctrl Pts',(-0.250000000000005,-1.18764683585401,
2.55895587944617));
#88684=CARTESIAN_POINT('Ctrl Pts',(-0.250000000000006,-1.23949850126476,
2.53972416718926));
#88685=CARTESIAN_POINT('Ctrl Pts',(-0.250000000000006,-1.25272255783918,
2.53481938257157));
#88686=CARTESIAN_POINT('Ctrl Pts',(-0.250000000000002,-1.26591860367828,
2.52981684034259));
#88687=CARTESIAN_POINT('Ctrl Pts',(-0.250000000000002,-1.27907848770803,
2.52471944034195));
#88688=CARTESIAN_POINT('Ctrl Pts',(-0.250000000000002,-1.37073515539029,
2.48921679481363));
#88689=CARTESIAN_POINT('Ctrl Pts',(-0.250000000000005,-1.46040274807117,
2.44920963606695));
#88690=CARTESIAN_POINT('Ctrl Pts',(-0.250000000000005,-1.54771241082929,
2.40488333309869));
#88691=CARTESIAN_POINT('Ctrl Pts',(-0.250000000000005,-1.63531255634976,
2.36040955473625));
#88692=CARTESIAN_POINT('Ctrl Pts',(-0.250000000000003,-1.72054002860748,
2.31158770014214));
#88693=CARTESIAN_POINT('Ctrl Pts',(-0.250000000000004,-1.80302121060508,
2.2585523933109));
#88694=CARTESIAN_POINT('Ctrl Pts',(-0.250000000000005,-1.88397085596804,
2.2065018628053));
#88695=CARTESIAN_POINT('Ctrl Pts',(-0.25,-1.96227614017533,2.15039259324176));
#88696=CARTESIAN_POINT('Ctrl Pts',(-0.250000000000001,-2.03756910697441,
2.09030490667818));
#88697=CARTESIAN_POINT('Ctrl Pts',(-0.250000000000001,-2.0994426421019,
2.04092662151587));
#88698=CARTESIAN_POINT('Ctrl Pts',(-0.250000000000001,-2.15928191063436,
1.98886079770323));
#88699=CARTESIAN_POINT('Ctrl Pts',(-0.250000000000001,-2.21686865784453,
1.93412961144453));
#88700=CARTESIAN_POINT('',(-0.25,-3.60291088309151E-16,2.942));
#88701=CARTESIAN_POINT('Origin',(-0.25,0.,0.));
#88702=CARTESIAN_POINT('',(-0.25,-2.89149574471101,-0.555476496098387));
#88703=CARTESIAN_POINT('Origin',(-0.25,0.,0.));
#88704=CARTESIAN_POINT('Ctrl Pts',(-0.25,-2.89371419577505,-0.556479620053392));
#88705=CARTESIAN_POINT('Ctrl Pts',(-0.25,-2.87319648930919,-0.628281513663384));
#88706=CARTESIAN_POINT('Ctrl Pts',(-0.250000000000005,-2.8497945550991,
-0.699127993612092));
#88707=CARTESIAN_POINT('Ctrl Pts',(-0.250000000000004,-2.82345497557192,
-0.768854229344188));
#88708=CARTESIAN_POINT('Ctrl Pts',(-0.250000000000004,-2.78891200574704,
-0.860296511268678));
#88709=CARTESIAN_POINT('Ctrl Pts',(-0.249999999999999,-2.74931759817973,
-0.949813518739235));
#88710=CARTESIAN_POINT('Ctrl Pts',(-0.25,-2.7049917476029,-1.03713570465333));
#88711=CARTESIAN_POINT('Ctrl Pts',(-0.250000000000001,-2.68151631903656,
-1.0833824367748));
#88712=CARTESIAN_POINT('Ctrl Pts',(-0.250000000000004,-2.65671306618578,
-1.12901301630281));
#88713=CARTESIAN_POINT('Ctrl Pts',(-0.250000000000004,-2.63062539793924,
-1.17398328280867));
#88714=CARTESIAN_POINT('Ctrl Pts',(-0.250000000000004,-2.61659733378916,
-1.19816504475953));
#88715=CARTESIAN_POINT('Ctrl Pts',(-0.250000000000005,-2.60219783598583,
-1.22215582354875));
#88716=CARTESIAN_POINT('Ctrl Pts',(-0.250000000000005,-2.58743338226914,
-1.24594836073162));
#88717=CARTESIAN_POINT('Ctrl Pts',(-0.250000000000006,-2.57841221178637,
-1.26048574479356));
#88718=CARTESIAN_POINT('Ctrl Pts',(-0.250000000000002,-2.5692556860291,
-1.27494753731645));
#88719=CARTESIAN_POINT('Ctrl Pts',(-0.250000000000002,-2.55997180439406,
-1.28932244956251));
#88720=CARTESIAN_POINT('Ctrl Pts',(-0.250000000000001,-2.50722268190062,
-1.37099776994114));
#88721=CARTESIAN_POINT('Ctrl Pts',(-0.249999999999998,-2.45031051886283,
-1.44996023242765));
#88722=CARTESIAN_POINT('Ctrl Pts',(-0.249999999999997,-2.38955315391405,
-1.52594513247122));
#88723=CARTESIAN_POINT('Ctrl Pts',(-0.249999999999997,-2.33964731266927,
-1.58835880629945));
#88724=CARTESIAN_POINT('Ctrl Pts',(-0.250000000000005,-2.28714614339243,
-1.64876308353032));
#88725=CARTESIAN_POINT('Ctrl Pts',(-0.250000000000005,-2.23221010314724,
-1.70699014883082));
#88726=CARTESIAN_POINT('Ctrl Pts',(-0.250000000000006,-2.2077967295152,
-1.73286604185723));
#88727=CARTESIAN_POINT('Ctrl Pts',(-0.250000000000001,-2.18290234415457,
-1.75831168687554));
#88728=CARTESIAN_POINT('Ctrl Pts',(-0.250000000000001,-2.15754040351483,
-1.7833109594478));
#88729=CARTESIAN_POINT('Ctrl Pts',(-0.250000000000001,-2.14235758353611,
-1.79827666970062));
#88730=CARTESIAN_POINT('Ctrl Pts',(-0.250000000000002,-2.12700719616793,
-1.81308239326784));
#88731=CARTESIAN_POINT('Ctrl Pts',(-0.250000000000002,-2.11149207982293,
-1.82772451114123));
#88732=CARTESIAN_POINT('Ctrl Pts',(-0.250000000000002,-2.10034093269375,
-1.83824820990432));
#88733=CARTESIAN_POINT('Ctrl Pts',(-0.250000000000001,-2.08910489602872,
-1.8486870996063));
#88734=CARTESIAN_POINT('Ctrl Pts',(-0.250000000000001,-2.07779536845615,
-1.85903064245993));
#88735=CARTESIAN_POINT('Ctrl Pts',(-0.250000000000001,-2.00763237329104,
-1.92320078065298));
#88736=CARTESIAN_POINT('Ctrl Pts',(-0.250000000000004,-1.93454403565031,
-1.98379921146077));
#88737=CARTESIAN_POINT('Ctrl Pts',(-0.250000000000003,-1.85882259425096,
-2.04057766488801));
#88738=CARTESIAN_POINT('Ctrl Pts',(-0.250000000000002,-1.78043266758531,
-2.0993570372573));
#88739=CARTESIAN_POINT('Ctrl Pts',(-0.249999999999999,-1.69921998861886,
-2.15404336229777));
#88740=CARTESIAN_POINT('Ctrl Pts',(-0.249999999999998,-1.61548348714018,
-2.20430748725186));
#88741=CARTESIAN_POINT('Ctrl Pts',(-0.249999999999998,-1.53798869174479,
-2.2508249319774));
#88742=CARTESIAN_POINT('Ctrl Pts',(-0.250000000000001,-1.45833145198356,
-2.29355469232131));
#88743=CARTESIAN_POINT('Ctrl Pts',(-0.250000000000001,-1.37673980248905,
-2.33218716905464));
#88744=CARTESIAN_POINT('Ctrl Pts',(-0.250000000000001,-1.32909704313918,
-2.35474533283119));
#88745=CARTESIAN_POINT('Ctrl Pts',(-0.250000000000003,-1.28079462304566,
-2.37590557784026));
#88746=CARTESIAN_POINT('Ctrl Pts',(-0.250000000000003,-1.23187796096567,
-2.39559798168754));
#88747=CARTESIAN_POINT('Ctrl Pts',(-0.250000000000003,-1.21499175511448,
-2.40239586958362));
#88748=CARTESIAN_POINT('Ctrl Pts',(-0.250000000000002,-1.19802860580916,
-2.40902009027204));
#88749=CARTESIAN_POINT('Ctrl Pts',(-0.250000000000002,-1.18101594114361,
-2.41545826461572));
#88750=CARTESIAN_POINT('Ctrl Pts',(-0.250000000000001,-1.09759886515225,
-2.44702614002095));
#88751=CARTESIAN_POINT('Ctrl Pts',(-0.250000000000005,-1.01287967862669,
-2.4741726092685));
#88752=CARTESIAN_POINT('Ctrl Pts',(-0.250000000000005,-0.927092223399418,
-2.49664604416005));
#88753=CARTESIAN_POINT('Ctrl Pts',(-0.250000000000004,-0.886487901330664,
-2.5072830141682));
#88754=CARTESIAN_POINT('Ctrl Pts',(-0.249999999999998,-0.84564411064597,
-2.51687238559944));
#88755=CARTESIAN_POINT('Ctrl Pts',(-0.249999999999998,-0.804585174478583,
-2.52538339335047));
#88756=CARTESIAN_POINT('Ctrl Pts',(-0.249999999999999,-0.716013041901021,
-2.54374329687598));
#88757=CARTESIAN_POINT('Ctrl Pts',(-0.25,-0.626439022336421,-2.55708831331885));
#88758=CARTESIAN_POINT('Ctrl Pts',(-0.250000000000001,-0.536235855388279,
-2.56552072220656));
#88759=CARTESIAN_POINT('Ctrl Pts',(-0.250000000000002,-0.443708985077977,
-2.57417035647057));
#88760=CARTESIAN_POINT('Ctrl Pts',(-0.25,-0.350519004198512,-2.57765081355158));
#88761=CARTESIAN_POINT('Ctrl Pts',(-0.25,-0.257086776744317,-2.57601949021612));
#88762=CARTESIAN_POINT('Ctrl Pts',(-0.25,-0.243661630645749,-2.57578508764744));
#88763=CARTESIAN_POINT('Ctrl Pts',(-0.250000000000003,-0.230231530774191,
-2.57544506120073));
#88764=CARTESIAN_POINT('Ctrl Pts',(-0.250000000000003,-0.21679777797424,
-2.57499949833529));
#88765=CARTESIAN_POINT('Ctrl Pts',(-0.250000000000003,-0.202668222536943,
-2.57453085749444));
#88766=CARTESIAN_POINT('Ctrl Pts',(-0.250000000000004,-0.188542730400431,
-2.57394570730987));
#88767=CARTESIAN_POINT('Ctrl Pts',(-0.250000000000004,-0.174427630795246,
-2.57324484391326));
#88768=CARTESIAN_POINT('Ctrl Pts',(-0.250000000000003,-0.0858016677984528,
-2.56884425906505));
#88769=CARTESIAN_POINT('Ctrl Pts',(-0.250000000000001,0.00247755739145698,
-2.55988411430444));
#88770=CARTESIAN_POINT('Ctrl Pts',(-0.250000000000002,0.0900618971462069,
-2.54649071805601));
#88771=CARTESIAN_POINT('Ctrl Pts',(-0.250000000000002,0.177515102319017,
-2.53311737490637));
#88772=CARTESIAN_POINT('Ctrl Pts',(-0.250000000000002,0.264276427722839,
-2.51532361020355));
#88773=CARTESIAN_POINT('Ctrl Pts',(-0.250000000000002,0.349981301201772,
-2.49318670047294));
#88774=CARTESIAN_POINT('Ctrl Pts',(-0.250000000000002,0.434317736638152,
-2.47140324776513));
#88775=CARTESIAN_POINT('Ctrl Pts',(-0.250000000000002,0.517631958865446,
-2.44541374332064));
#88776=CARTESIAN_POINT('Ctrl Pts',(-0.250000000000002,0.599546682957301,
-2.41525188469741));
#88777=CARTESIAN_POINT('Ctrl Pts',(-0.250000000000002,0.627537361614373,
-2.40494542390196));
#88778=CARTESIAN_POINT('Ctrl Pts',(-0.249999999999999,0.655364319587099,
-2.39415147439514));
#88779=CARTESIAN_POINT('Ctrl Pts',(-0.249999999999999,0.683011442265382,
-2.38287044100979));
#88780=CARTESIAN_POINT('Ctrl Pts',(-0.249999999999999,0.70026444827292,
-2.37583058593939));
#88781=CARTESIAN_POINT('Ctrl Pts',(-0.250000000000004,0.717447409397925,
-2.3686010365864));
#88782=CARTESIAN_POINT('Ctrl Pts',(-0.250000000000004,0.734556286227355,
-2.36118180434677));
#88783=CARTESIAN_POINT('Ctrl Pts',(-0.250000000000005,0.747119478010523,
-2.35573379987285));
#88784=CARTESIAN_POINT('Ctrl Pts',(-0.249999999999999,0.759634939071271,
-2.35018686706227));
#88785=CARTESIAN_POINT('Ctrl Pts',(-0.249999999999999,0.772097715167772,
-2.34454300922358));
#88786=CARTESIAN_POINT('Ctrl Pts',(-0.249999999999999,0.849775762223969,
-2.30936594663516));
#88787=CARTESIAN_POINT('Ctrl Pts',(-0.249999999999998,0.925455358875783,
-2.27040707536139));
#88788=CARTESIAN_POINT('Ctrl Pts',(-0.249999999999999,0.998809291101006,
-2.22774211242364));
#88789=CARTESIAN_POINT('Ctrl Pts',(-0.25,1.07101111120779,-2.18574725426885));
#88790=CARTESIAN_POINT('Ctrl Pts',(-0.25,1.14096041241647,-2.14016132509184));
#88791=CARTESIAN_POINT('Ctrl Pts',(-0.250000000000002,1.20831094189049,
-2.0910204724465));
#88792=CARTESIAN_POINT('Ctrl Pts',(-0.250000000000003,1.27356246615044,
-2.04341111341719));
#88793=CARTESIAN_POINT('Ctrl Pts',(-0.25,1.33637510283447,-1.99246448542687));
#88794=CARTESIAN_POINT('Ctrl Pts',(-0.250000000000001,1.39639388640012,
-1.93818640597136));
#88795=CARTESIAN_POINT('Ctrl Pts',(-0.250000000000001,1.43371761251259,
-1.90443263671525));
#88796=CARTESIAN_POINT('Ctrl Pts',(-0.250000000000001,1.4699600853265,-1.86939002404756));
#88797=CARTESIAN_POINT('Ctrl Pts',(-0.250000000000001,1.50502666328431,
-1.8330555925294));
#88798=CARTESIAN_POINT('Ctrl Pts',(-15.7872339910054,-1.03908919352511,
2.13201587949043));
#88799=CARTESIAN_POINT('Ctrl Pts',(-15.7343862563421,-1.74702956476549,
1.78698412034994));
#88800=CARTESIAN_POINT('Ctrl Pts',(-15.6286907870155,-2.78011294947163,
0.342389453078488));
#88801=CARTESIAN_POINT('Ctrl Pts',(-15.4701475830257,-1.79667481887822,
-2.15247714088935));
#88802=CARTESIAN_POINT('Ctrl Pts',(-15.3116043790358,0.829372328041529,
-2.67555139502504));
#88803=CARTESIAN_POINT('Ctrl Pts',(-15.153061175046,2.69704440340713,-0.759379027323357));
#88804=CARTESIAN_POINT('Ctrl Pts',(-14.9945179710561,2.10312284761966,1.85179574340887));
#88805=CARTESIAN_POINT('Ctrl Pts',(-14.8359747670663,-0.411142958056525,
2.77149379088676));
#88806=CARTESIAN_POINT('Ctrl Pts',(-14.6774315630764,-2.54988918864703,
1.1614740258459));
#88807=CARTESIAN_POINT('Ctrl Pts',(-14.5188883590866,-2.36084355622959,
-1.50914432504944));
#88808=CARTESIAN_POINT('Ctrl Pts',(-14.3603451550967,-0.0164545272929353,
-2.80188230448376));
#88809=CARTESIAN_POINT('Ctrl Pts',(-14.2018019511069,2.34293162102215,-1.53675277767917));
#88810=CARTESIAN_POINT('Ctrl Pts',(-14.043258747117,2.56338713804141,1.13136735389903));
#88811=CARTESIAN_POINT('Ctrl Pts',(-13.8847155431272,0.443630763460945,
2.76660429639169));
#88812=CARTESIAN_POINT('Ctrl Pts',(-13.7261723391373,-2.08112798018708,
1.87612190650057));
#88813=CARTESIAN_POINT('Ctrl Pts',(-13.5676291351475,-2.70595460958226,
-0.727142408722851));
#88814=CARTESIAN_POINT('Ctrl Pts',(-13.4090859311576,-0.860420371114484,
-2.6665705025054));
#88815=CARTESIAN_POINT('Ctrl Pts',(-13.2505427271678,1.77062098199356,-2.17159522099969));
#88816=CARTESIAN_POINT('Ctrl Pts',(-13.0919995231779,2.78520124435443,0.305905452644607));
#88817=CARTESIAN_POINT('Ctrl Pts',(-12.9334563191881,1.25707446924262,2.50413403614118));
#88818=CARTESIAN_POINT('Ctrl Pts',(-12.7749131151982,-1.41867915221937,
2.41625193356046));
#88819=CARTESIAN_POINT('Ctrl Pts',(-12.6163699112084,-2.79927136767585,
0.122489461091731));
#88820=CARTESIAN_POINT('Ctrl Pts',(-12.4578267072185,-1.6243115612719,-2.28309783734224));
#88821=CARTESIAN_POINT('Ctrl Pts',(-12.2992835032286,1.03353864319095,-2.60436589634899));
#88822=CARTESIAN_POINT('Ctrl Pts',(-12.1407402992388,2.74783554884452,-0.548017908917588));
#88823=CARTESIAN_POINT('Ctrl Pts',(-11.9821970952489,1.95353799427501,2.00863464286302));
#88824=CARTESIAN_POINT('Ctrl Pts',(-11.8236538912591,-0.624212206359067,
2.73153490815486));
#88825=CARTESIAN_POINT('Ctrl Pts',(-11.6651106872692,-2.63209741649849,
0.960722134658545));
#88826=CARTESIAN_POINT('Ctrl Pts',(-11.5065674832794,-2.23704952747652,
-1.68716722370331));
#88827=CARTESIAN_POINT('Ctrl Pts',(-11.3480242792896,0.200278529009738,
-2.79478305799562));
#88828=CARTESIAN_POINT('Ctrl Pts',(-11.1894810752997,2.45476536426573,-1.35094442384648));
#88829=CARTESIAN_POINT('Ctrl Pts',(-11.0309378713099,2.46821168687189,1.3262182696089));
#88830=CARTESIAN_POINT('Ctrl Pts',(-10.87239466732,0.228341882252721,2.79263026819601));
#88831=CARTESIAN_POINT('Ctrl Pts',(-10.7138514633301,-2.21998915305615,
1.70955315514429));
#88832=CARTESIAN_POINT('Ctrl Pts',(-10.5553082593403,-2.64161502869699,
-0.934234376434406));
#88833=CARTESIAN_POINT('Ctrl Pts',(-10.3967650553504,-0.651618847034371,
-2.72512691597345));
#88834=CARTESIAN_POINT('Ctrl Pts',(-10.2382218513606,1.93326279954282,-2.02815649737983));
#88835=CARTESIAN_POINT('Ctrl Pts',(-10.0796786473708,2.75320172762965,0.520388390472216));
#88836=CARTESIAN_POINT('Ctrl Pts',(-9.9211354433809,1.05964722747713,2.59385265257382));
#88837=CARTESIAN_POINT('Ctrl Pts',(-9.76259223939105,-1.60129600986408,
2.29929878849087));
#88838=CARTESIAN_POINT('Ctrl Pts',(-9.6040490354012,-2.80036053447984,-0.0943647544917269));
#88839=CARTESIAN_POINT('Ctrl Pts',(-9.44550583141135,-1.4428787190723,-2.40187943744293));
#88840=CARTESIAN_POINT('Ctrl Pts',(-9.2869626274215,1.23185716520365,-2.51663500621346));
#88841=CARTESIAN_POINT('Ctrl Pts',(-9.12841942343165,2.78198788226743,-0.333867118596373));
#88842=CARTESIAN_POINT('Ctrl Pts',(-8.96987621944179,1.79234529127704,2.15369965101908));
#88843=CARTESIAN_POINT('Ctrl Pts',(-8.81133301545195,-0.833591533278391,
2.67507924847269));
#88844=CARTESIAN_POINT('Ctrl Pts',(-8.65278981146209,-2.69851371088473,
0.754286140751512));
#88845=CARTESIAN_POINT('Ctrl Pts',(-8.49424660747226,-2.09986904910667,
-1.85512096817608));
#88846=CARTESIAN_POINT('Ctrl Pts',(-8.33570340348239,0.415818959741428,
-2.77092374898376));
#88847=CARTESIAN_POINT('Ctrl Pts',(-8.17716019949255,2.55189140603955,-1.15705405307796));
#88848=CARTESIAN_POINT('Ctrl Pts',(-8.0186169955027,2.35825360470366,1.51313045236188));
#88849=CARTESIAN_POINT('Ctrl Pts',(-7.86007379151283,0.0116842262656824,
2.80192564298541));
#88850=CARTESIAN_POINT('Ctrl Pts',(-7.701530587523,-2.34555208792137,1.53274565170167));
#88851=CARTESIAN_POINT('Ctrl Pts',(-7.54298738353314,-2.56145248058093,
-1.13573105077235));
#88852=CARTESIAN_POINT('Ctrl Pts',(-7.38444417954329,-0.438913988766854,
-2.76735945269628));
#88853=CARTESIAN_POINT('Ctrl Pts',(-7.22590097555344,2.08432431928549,-1.87256934771392));
#88854=CARTESIAN_POINT('Ctrl Pts',(-7.06735777156358,2.70471060372122,0.731754316748925));
#88855=CARTESIAN_POINT('Ctrl Pts',(-6.90881456757374,0.855872690191172,
2.66803406427797));
#88856=CARTESIAN_POINT('Ctrl Pts',(-6.75027136358388,-1.77432111187291,
2.16857289984097));
#88857=CARTESIAN_POINT('Ctrl Pts',(-6.59172815959403,-2.78467557941811,
-0.310653741898083));
#88858=CARTESIAN_POINT('Ctrl Pts',(-6.43318495560419,-1.2528030468829,-2.50627379902584));
#88859=CARTESIAN_POINT('Ctrl Pts',(-6.27464175161433,1.42279687533745,-2.41382950547303));
#88860=CARTESIAN_POINT('Ctrl Pts',(-6.11609854762448,2.79947614093066,-0.117716465815816));
#88861=CARTESIAN_POINT('Ctrl Pts',(-5.95755534363463,1.62041646007026,2.285864021742));
#88862=CARTESIAN_POINT('Ctrl Pts',(-5.79901213964478,-1.0379776562294,2.60259989532173));
#88863=CARTESIAN_POINT('Ctrl Pts',(-5.64046893565492,-2.74876593914578,
0.543331981173054));
#88864=CARTESIAN_POINT('Ctrl Pts',(-5.48192573166508,-1.95011037910057,
-2.01196255911331));
#88865=CARTESIAN_POINT('Ctrl Pts',(-5.32338252767523,0.628868639624235,
-2.73046663851582));
#88866=CARTESIAN_POINT('Ctrl Pts',(-5.16483932368538,2.63373164752747,-0.956232941728888));
#88867=CARTESIAN_POINT('Ctrl Pts',(-5.00629611969553,2.23416961039886,1.6909790010008));
#88868=CARTESIAN_POINT('Ctrl Pts',(-4.84775291570567,-0.205043418049532,
2.79443751524972));
#88869=CARTESIAN_POINT('Ctrl Pts',(-4.68920971171582,-2.45706519272027,
1.3467570193484));
#88870=CARTESIAN_POINT('Ctrl Pts',(-4.53066650772597,-2.46594686124215,
-1.33042470912548));
#88871=CARTESIAN_POINT('Ctrl Pts',(-4.37212330373612,-0.223580041071285,
-2.79301553794379));
#88872=CARTESIAN_POINT('Ctrl Pts',(-4.21358009974628,2.22290076086175,-1.70576552913832));
#88873=CARTESIAN_POINT('Ctrl Pts',(-4.05503689575642,2.64001829300782,0.938737043143364));
#88874=CARTESIAN_POINT('Ctrl Pts',(-3.89649369176657,0.646971487662433,
2.7262339822803));
#88875=CARTESIAN_POINT('Ctrl Pts',(-3.73795048777672,-1.93671805526808,
2.02485728470756));
#88876=CARTESIAN_POINT('Ctrl Pts',(-3.57940728378687,-2.75231044083283,
-0.525081917648047));
#88877=CARTESIAN_POINT('Ctrl Pts',(-3.42086407979702,-1.05522311535154,
-2.59565560789489));
#88878=CARTESIAN_POINT('Ctrl Pts',(-3.26232087580717,1.60521408013114,-2.29656519618435));
#88879=CARTESIAN_POINT('Ctrl Pts',(-3.10377767181731,2.80019550906176,0.0991393121454807));
#88880=CARTESIAN_POINT('Ctrl Pts',(-2.94523446782747,1.43878146837926,2.40433608377855));
#88881=CARTESIAN_POINT('Ctrl Pts',(-2.78669126383761,-1.23614652569664,
2.51453101646264));
#88882=CARTESIAN_POINT('Ctrl Pts',(-2.62814805984777,-2.78255266904079,
0.329123235087791));
#88883=CARTESIAN_POINT('Ctrl Pts',(-2.46960485585791,-1.7886713762176,-2.15675245208684));
#88884=CARTESIAN_POINT('Ctrl Pts',(-2.31106165186806,0.838152943427643,
-2.67365418881957));
#88885=CARTESIAN_POINT('Ctrl Pts',(-2.15251844787821,2.69979292454605,-0.749683767780105));
#88886=CARTESIAN_POINT('Ctrl Pts',(-1.99397524388836,2.09670858668745,1.85869814963478));
#88887=CARTESIAN_POINT('Ctrl Pts',(-1.83543203989851,-0.420553593951653,
2.77021160836216));
#88888=CARTESIAN_POINT('Ctrl Pts',(-1.67688883590866,-2.55383998688081,
1.15269966645968));
#88889=CARTESIAN_POINT('Ctrl Pts',(-1.51834563191881,-2.35570945011923,
-1.51714596444729));
#88890=CARTESIAN_POINT('Ctrl Pts',(-1.35980242792896,-0.0068319532377577,
-2.80194755688051));
#88891=CARTESIAN_POINT('Ctrl Pts',(-1.20125922393911,2.34801894891291,-1.52873260592859));
#88892=CARTESIAN_POINT('Ctrl Pts',(-1.04271601994925,2.55978575511233,1.14007459203818));
#88893=CARTESIAN_POINT('Ctrl Pts',(-0.884172815959405,0.433672104903693,
2.76814622563851));
#88894=CARTESIAN_POINT('Ctrl Pts',(-0.725629611969553,-2.08651182541223,
1.86893074466561));
#88895=CARTESIAN_POINT('Ctrl Pts',(-0.567086407979702,-2.70540359932766,
-0.73619943737228));
#88896=CARTESIAN_POINT('Ctrl Pts',(-0.408543203989851,-0.847344309994932,
-2.66988130255231));
#88897=CARTESIAN_POINT('Ctrl Pts',(-0.302847734663285,0.896356686121819,
-2.33280287161008));
#88898=CARTESIAN_POINT('Ctrl Pts',(-0.250000000000001,1.50502666328431,
-1.8330555925294));
#88899=CARTESIAN_POINT('Ctrl Pts',(-15.6774893273369,-1.12236674703449,
2.30288577939267));
#88900=CARTESIAN_POINT('Ctrl Pts',(-15.6246415926736,-1.88704482906504,
1.93020153289759));
#88901=CARTESIAN_POINT('Ctrl Pts',(-15.5189461233471,-3.00292443317721,
0.369830173449262));
#88902=CARTESIAN_POINT('Ctrl Pts',(-15.3604029193572,-1.94066889012877,
-2.32498690366536));
#88903=CARTESIAN_POINT('Ctrl Pts',(-15.2018597153673,0.895842173804579,
-2.88998281809704));
#88904=CARTESIAN_POINT('Ctrl Pts',(-15.0433165113775,2.91319837846674,-0.820239276834098));
#88905=CARTESIAN_POINT('Ctrl Pts',(-14.8847733073877,2.27167712243153,2.00020746789906));
#88906=CARTESIAN_POINT('Ctrl Pts',(-14.7262301033978,-0.444093911548188,
2.99361449420052));
#88907=CARTESIAN_POINT('Ctrl Pts',(-14.567686899408,-2.75424944441119,1.25456008230755));
#88908=CARTESIAN_POINT('Ctrl Pts',(-14.4091436954181,-2.55005279525,-1.63009433402444));
#88909=CARTESIAN_POINT('Ctrl Pts',(-14.2506004914283,-0.0177732714254624,
-3.02643848791117));
#88910=CARTESIAN_POINT('Ctrl Pts',(-14.0920572874384,2.53070531230325,-1.65991545945025));
#88911=CARTESIAN_POINT('Ctrl Pts',(-13.9335140834486,2.76882918371348,1.22204051837825));
#88912=CARTESIAN_POINT('Ctrl Pts',(-13.7749708794587,0.479185444303327,
2.98833313234507));
#88913=CARTESIAN_POINT('Ctrl Pts',(-13.6164276754689,-2.24791948163841,
2.02648324548122));
#88914=CARTESIAN_POINT('Ctrl Pts',(-13.457884471479,-2.92282269097284,-0.785419062188865));
#88915=CARTESIAN_POINT('Ctrl Pts',(-13.2993412674892,-0.92937855482246,
-2.88028215410634));
#88916=CARTESIAN_POINT('Ctrl Pts',(-13.1407980634993,1.91252697475302,-2.34563719770819));
#88917=CARTESIAN_POINT('Ctrl Pts',(-12.9822548595095,3.00842052822964,0.330422171575135));
#88918=CARTESIAN_POINT('Ctrl Pts',(-12.8237116555196,1.35782240024796,2.70482725621207));
#88919=CARTESIAN_POINT('Ctrl Pts',(-12.6651684515298,-1.53237885167518,
2.60990186365609));
#88920=CARTESIAN_POINT('Ctrl Pts',(-12.5066252475399,-3.02361829820073,
0.132306349491674));
#88921=CARTESIAN_POINT('Ctrl Pts',(-12.3480820435501,-1.75449162069573,
-2.4660761644206));
#88922=CARTESIAN_POINT('Ctrl Pts',(-12.1895388395602,1.11637134917872,-2.81309217475004));
#88923=CARTESIAN_POINT('Ctrl Pts',(-12.0309956355704,2.96806016803971,-0.591938672427007));
#88924=CARTESIAN_POINT('Ctrl Pts',(-11.8724524315805,2.11010382699142,2.16961618322949));
#88925=CARTESIAN_POINT('Ctrl Pts',(-11.7139092275907,-0.674239543511815,
2.95045311642237));
#88926=CARTESIAN_POINT('Ctrl Pts',(-11.5553660236008,-2.84304623091236,
1.03771897908273));
#88927=CARTESIAN_POINT('Ctrl Pts',(-11.396822819611,-2.41633732383554,-1.8223848350756));
#88928=CARTESIAN_POINT('Ctrl Pts',(-11.2382796156211,0.216329803549303,
-3.01877027402064));
#88929=CARTESIAN_POINT('Ctrl Pts',(-11.0797364116313,2.65150194400256,-1.45921553978739));
#88930=CARTESIAN_POINT('Ctrl Pts',(-10.9211932076414,2.66602591890011,1.43250771386515));
#88931=CARTESIAN_POINT('Ctrl Pts',(-10.7626500036516,0.246642287488625,
3.01644494940029));
#88932=CARTESIAN_POINT('Ctrl Pts',(-10.6041067996617,-2.39790964981033,
1.84656488160804));
#88933=CARTESIAN_POINT('Ctrl Pts',(-10.4455635956719,-2.85332662985148,
-1.00910836584611));
#88934=CARTESIAN_POINT('Ctrl Pts',(-10.287020391682,-0.703842682812667,
-2.94353155724871));
#88935=CARTESIAN_POINT('Ctrl Pts',(-10.1284771876922,2.08820368165366,-2.19070261208149));
#88936=CARTESIAN_POINT('Ctrl Pts',(-9.96993398370229,2.973856417933,0.562094792870815));
#88937=CARTESIAN_POINT('Ctrl Pts',(-9.81139077971244,1.14457239967333,2.80173634958097));
#88938=CARTESIAN_POINT('Ctrl Pts',(-9.65284757572259,-1.72963149345564,
2.48357553690266));
#88939=CARTESIAN_POINT('Ctrl Pts',(-9.49430437173273,-3.02479475601628,
-0.101927595045291));
#88940=CARTESIAN_POINT('Ctrl Pts',(-9.3357611677429,-1.55851788699347,-2.59437748729385));
#88941=CARTESIAN_POINT('Ctrl Pts',(-9.17721796375303,1.33058406144162,-2.71833011352428));
#88942=CARTESIAN_POINT('Ctrl Pts',(-9.01867475976319,3.004949632011,-0.360624818519741));
#88943=CARTESIAN_POINT('Ctrl Pts',(-8.86013155577333,1.93599237357926,2.32630739157542));
#88944=CARTESIAN_POINT('Ctrl Pts',(-8.70158835178349,-0.900399526230412,
2.88947283147281));
#88945=CARTESIAN_POINT('Ctrl Pts',(-8.54304514779364,-2.91478544323875,
0.814738222092814));
#88946=CARTESIAN_POINT('Ctrl Pts',(-8.38450194380378,-2.26816254901928,
-2.0037991920055));
#88947=CARTESIAN_POINT('Ctrl Pts',(-8.22595873981394,0.449144670263532,
-2.9929987664263));
#88948=CARTESIAN_POINT('Ctrl Pts',(-8.06741553582408,2.75641212903509,-1.24978587188514));
#88949=CARTESIAN_POINT('Ctrl Pts',(-7.90887233183423,2.54725527268193,1.63439992855164));
#88950=CARTESIAN_POINT('Ctrl Pts',(-7.75032912784439,0.0126206557696573,
3.02648529976662));
#88951=CARTESIAN_POINT('Ctrl Pts',(-7.59178592385452,-2.53353579589187,
1.65558718332501));
#88952=CARTESIAN_POINT('Ctrl Pts',(-7.43324271986469,-2.76673947359612,
-1.226753942688));
#88953=CARTESIAN_POINT('Ctrl Pts',(-7.27469951587482,-0.474090644835783,
-2.98914881047008));
#88954=CARTESIAN_POINT('Ctrl Pts',(-7.11615631188499,2.25137199056513,-2.02264596772502));
#88955=CARTESIAN_POINT('Ctrl Pts',(-6.95761310789512,2.92147898456125,0.790400590474505));
#88956=CARTESIAN_POINT('Ctrl Pts',(-6.79906990390528,0.924466401105285,
2.88186301268518));
#88957=CARTESIAN_POINT('Ctrl Pts',(-6.64052669991542,-1.91652365065164,
2.34237265334709));
#88958=CARTESIAN_POINT('Ctrl Pts',(-6.48198349592558,-3.00785273400343,
-0.335551011328845));
#88959=CARTESIAN_POINT('Ctrl Pts',(-6.32344029193572,-1.35320864577052,
-2.70713850987851));
#88960=CARTESIAN_POINT('Ctrl Pts',(-6.16489708794587,1.53682658872223,-2.6072852906522));
#88961=CARTESIAN_POINT('Ctrl Pts',(-6.00635388395602,3.02383948295879,-0.1271508236573));
#88962=CARTESIAN_POINT('Ctrl Pts',(-5.84781067996617,1.75028434754508,2.4690640440038));
#88963=CARTESIAN_POINT('Ctrl Pts',(-5.68926747597632,-1.12116612584954,
2.81118463799518));
#88964=CARTESIAN_POINT('Ctrl Pts',(-5.53072427198646,-2.96906512424789,
0.586877192130376));
#88965=CARTESIAN_POINT('Ctrl Pts',(-5.37218106799662,-2.10640150642318,
-2.17321081452728));
#88966=CARTESIAN_POINT('Ctrl Pts',(-5.21363786400676,0.679269165501129,
-2.94929923057003));
#88967=CARTESIAN_POINT('Ctrl Pts',(-5.05509466001692,2.8448114369941,-1.0328700008654));
#88968=CARTESIAN_POINT('Ctrl Pts',(-4.89655145602706,2.41322659649633,1.82650210634784));
#88969=CARTESIAN_POINT('Ctrl Pts',(-4.73800825203721,-0.221476573475216,
3.01839703783448));
#88970=CARTESIAN_POINT('Ctrl Pts',(-4.57946504804736,-2.65398609165546,
1.45469253676291));
#88971=CARTESIAN_POINT('Ctrl Pts',(-4.42092184405751,-2.66357957936498,
-1.43705127746513));
#88972=CARTESIAN_POINT('Ctrl Pts',(-4.26237864006766,-0.241498809690948,
-3.01686109649935));
#88973=CARTESIAN_POINT('Ctrl Pts',(-4.10383543607781,2.40105460772325,-1.84247369722676));
#88974=CARTESIAN_POINT('Ctrl Pts',(-3.94529223208796,2.85160192416453,1.01397189769554));
#88975=CARTESIAN_POINT('Ctrl Pts',(-3.78674902809811,0.698822861941575,
2.94472734911847));
#88976=CARTESIAN_POINT('Ctrl Pts',(-3.62820582410825,-2.09193585801802,
2.18713898480308));
#88977=CARTESIAN_POINT('Ctrl Pts',(-3.46966262011841,-2.97289369917019,
-0.567164481653337));
#88978=CARTESIAN_POINT('Ctrl Pts',(-3.31111941612855,-1.13979371814545,
-2.80368380232263));
#88979=CARTESIAN_POINT('Ctrl Pts',(-3.15257621213871,1.73386357652194,-2.48062286149818));
#88980=CARTESIAN_POINT('Ctrl Pts',(-2.99403300814886,3.02461650467576,0.107084808473903));
#88981=CARTESIAN_POINT('Ctrl Pts',(-2.835489804159,1.55409226312905,2.5970310209592));
#88982=CARTESIAN_POINT('Ctrl Pts',(-2.67694660016915,-1.33521719169972,
2.7160575000209));
#88983=CARTESIAN_POINT('Ctrl Pts',(-2.5184033961793,-3.00555968348449,0.355500737608286));
#88984=CARTESIAN_POINT('Ctrl Pts',(-2.35986019218945,-1.93202401348097,
-2.32960485865055));
#88985=CARTESIAN_POINT('Ctrl Pts',(-2.2013169881996,0.905326509499033,-2.88793356075652));
#88986=CARTESIAN_POINT('Ctrl Pts',(-2.04277378420975,2.91616717917131,-0.809766993046504));
#88987=CARTESIAN_POINT('Ctrl Pts',(-1.8842305802199,2.26474879209958,2.00766306581188));
#88988=CARTESIAN_POINT('Ctrl Pts',(-1.72568737623005,-0.454258760593834,
2.99222955146585));
#88989=CARTESIAN_POINT('Ctrl Pts',(-1.5671441722402,-2.75851687841923,1.24508250399859));
#88990=CARTESIAN_POINT('Ctrl Pts',(-1.40860096825035,-2.5445072174402,-1.63873726288739));
#88991=CARTESIAN_POINT('Ctrl Pts',(-1.25005776426049,-0.00737949848690254,
-3.02650896994557));
#88992=CARTESIAN_POINT('Ctrl Pts',(-1.09151456027065,2.53620036286428,-1.6512525129636));
#88993=CARTESIAN_POINT('Ctrl Pts',(-0.932971356280792,2.7649391688157,1.23144559602393));
#88994=CARTESIAN_POINT('Ctrl Pts',(-0.774428152290943,0.468428651451106,
2.98999863914054));
#88995=CARTESIAN_POINT('Ctrl Pts',(-0.615884948301092,-2.25373481384429,
2.01871574971051));
#88996=CARTESIAN_POINT('Ctrl Pts',(-0.457341744311241,-2.9222275201339,
-0.795201964221146));
#88997=CARTESIAN_POINT('Ctrl Pts',(-0.298798540321389,-0.915254515929336,
-2.88385829742676));
#88998=CARTESIAN_POINT('Ctrl Pts',(-0.193103070994823,0.968194977153174,
-2.51976479670557));
#88999=CARTESIAN_POINT('Ctrl Pts',(-0.14025533633154,1.62564666324746,-1.97996539213447));
#89000=CARTESIAN_POINT('Ctrl Pts',(-15.5677446636685,-1.20564430054386,
2.47375567929492));
#89001=CARTESIAN_POINT('Ctrl Pts',(-15.5148969290052,-2.0270600933646,2.07341894544524));
#89002=CARTESIAN_POINT('Ctrl Pts',(-15.4092014596786,-3.2257359168828,0.397270893820039));
#89003=CARTESIAN_POINT('Ctrl Pts',(-15.2506582556888,-2.08466296137931,
-2.49749666644138));
#89004=CARTESIAN_POINT('Ctrl Pts',(-15.0921150516989,0.962312019567628,
-3.10441424116905));
#89005=CARTESIAN_POINT('Ctrl Pts',(-14.9335718477091,3.12935235352635,-0.881099526344837));
#89006=CARTESIAN_POINT('Ctrl Pts',(-14.7750286437192,2.44023139724341,2.14861919238924));
#89007=CARTESIAN_POINT('Ctrl Pts',(-14.6164854397294,-0.477044865039856,
3.21573519751427));
#89008=CARTESIAN_POINT('Ctrl Pts',(-14.4579422357395,-2.95860970017535,
1.3476461387692));
#89009=CARTESIAN_POINT('Ctrl Pts',(-14.2993990317497,-2.73926203427042,
-1.75104434299943));
#89010=CARTESIAN_POINT('Ctrl Pts',(-14.1408558277598,-0.0190920155579868,
-3.25099467133857));
#89011=CARTESIAN_POINT('Ctrl Pts',(-13.98231262377,2.71847900358434,-1.78307814122133));
#89012=CARTESIAN_POINT('Ctrl Pts',(-13.8237694197801,2.97427122938555,1.31271368285747));
#89013=CARTESIAN_POINT('Ctrl Pts',(-13.6652262157903,0.514740125145709,
3.21006196829846));
#89014=CARTESIAN_POINT('Ctrl Pts',(-13.5066830118004,-2.41471098308974,
2.17684458446186));
#89015=CARTESIAN_POINT('Ctrl Pts',(-13.3481398078105,-3.13969077236341,
-0.843695715654877));
#89016=CARTESIAN_POINT('Ctrl Pts',(-13.1895966038207,-0.998336738530438,
-3.0939938057073));
#89017=CARTESIAN_POINT('Ctrl Pts',(-13.0310533998308,2.05443296751247,-2.51967917441669));
#89018=CARTESIAN_POINT('Ctrl Pts',(-12.872510195841,3.23163981210485,0.354938890505661));
#89019=CARTESIAN_POINT('Ctrl Pts',(-12.7139669918511,1.4585703312533,2.90552047628297));
#89020=CARTESIAN_POINT('Ctrl Pts',(-12.5554237878613,-1.64607855113099,
2.80355179375173));
#89021=CARTESIAN_POINT('Ctrl Pts',(-12.3968805838714,-3.24796522872561,
0.14212323789162));
#89022=CARTESIAN_POINT('Ctrl Pts',(-12.2383373798816,-1.88467168011957,
-2.64905449149896));
#89023=CARTESIAN_POINT('Ctrl Pts',(-12.0797941758917,1.19920405516649,-3.02181845315109));
#89024=CARTESIAN_POINT('Ctrl Pts',(-11.9212509719019,3.18828478723489,-0.635859435936428));
#89025=CARTESIAN_POINT('Ctrl Pts',(-11.7627077679121,2.26666965970783,2.33059772359595));
#89026=CARTESIAN_POINT('Ctrl Pts',(-11.6041645639222,-0.724266880664566,
3.16937132468987));
#89027=CARTESIAN_POINT('Ctrl Pts',(-11.4456213599323,-3.05399504532621,
1.11471582350691));
#89028=CARTESIAN_POINT('Ctrl Pts',(-11.2870781559425,-2.59562512019457,
-1.95760244644789));
#89029=CARTESIAN_POINT('Ctrl Pts',(-11.1285349519526,0.232381078088869,
-3.24275749004566));
#89030=CARTESIAN_POINT('Ctrl Pts',(-10.9699917479628,2.84823852373938,-1.5674866557283));
#89031=CARTESIAN_POINT('Ctrl Pts',(-10.8114485439729,2.86384015092833,1.53879715812141));
#89032=CARTESIAN_POINT('Ctrl Pts',(-10.6529053399831,0.26494269272453,3.24025963060457));
#89033=CARTESIAN_POINT('Ctrl Pts',(-10.4943621359932,-2.57583014656451,
1.98357660807178));
#89034=CARTESIAN_POINT('Ctrl Pts',(-10.3358189320034,-3.06503823100597,
-1.0839823552578));
#89035=CARTESIAN_POINT('Ctrl Pts',(-10.1772757280135,-0.756066518590962,
-3.16193619852398));
#89036=CARTESIAN_POINT('Ctrl Pts',(-10.0187325240237,2.24314456376451,-2.35324872678314));
#89037=CARTESIAN_POINT('Ctrl Pts',(-9.86018932003384,3.19451110823633,0.603801195269414));
#89038=CARTESIAN_POINT('Ctrl Pts',(-9.70164611604398,1.22949757186952,3.00962004658812));
#89039=CARTESIAN_POINT('Ctrl Pts',(-9.54310291205413,-1.85796697704721,
2.66785228531445));
#89040=CARTESIAN_POINT('Ctrl Pts',(-9.38455970806428,-3.24922897755272,
-0.109490435598857));
#89041=CARTESIAN_POINT('Ctrl Pts',(-9.22601650407443,-1.67415705491464,
-2.78687553714476));
#89042=CARTESIAN_POINT('Ctrl Pts',(-9.06747330008458,1.4293109576796,-2.9200252208351));
#89043=CARTESIAN_POINT('Ctrl Pts',(-8.90893009609472,3.22791138175458,-0.387382518443105));
#89044=CARTESIAN_POINT('Ctrl Pts',(-8.75038689210488,2.07963945588148,2.49891513213177));
#89045=CARTESIAN_POINT('Ctrl Pts',(-8.59184368811503,-0.96720751918243,
3.10386641447293));
#89046=CARTESIAN_POINT('Ctrl Pts',(-8.43330048412516,-3.13105717559277,
0.875190303434115));
#89047=CARTESIAN_POINT('Ctrl Pts',(-8.27475728013534,-2.43645604893188,
-2.15247741583492));
#89048=CARTESIAN_POINT('Ctrl Pts',(-8.11621407614546,0.482470380785634,
-3.21507378386883));
#89049=CARTESIAN_POINT('Ctrl Pts',(-7.95767087215563,2.96093285203063,-1.34251769069233));
#89050=CARTESIAN_POINT('Ctrl Pts',(-7.79912766816575,2.73625694066019,1.75566940474141));
#89051=CARTESIAN_POINT('Ctrl Pts',(-7.64058446417593,0.0135570852736332,
3.25104495654781));
#89052=CARTESIAN_POINT('Ctrl Pts',(-7.48204126018606,-2.72151950386236,
1.77842871494836));
#89053=CARTESIAN_POINT('Ctrl Pts',(-7.32349805619623,-2.97202646661131,
-1.31777683460364));
#89054=CARTESIAN_POINT('Ctrl Pts',(-7.16495485220635,-0.509267300904713,
-3.21093816824387));
#89055=CARTESIAN_POINT('Ctrl Pts',(-7.00641164821653,2.41841966184476,-2.17272258773612));
#89056=CARTESIAN_POINT('Ctrl Pts',(-6.84786844422665,3.13824736540129,0.849046864200083));
#89057=CARTESIAN_POINT('Ctrl Pts',(-6.68932524023682,0.993060112019402,
3.0956919610924));
#89058=CARTESIAN_POINT('Ctrl Pts',(-6.53078203624696,-2.05872618943038,
2.51617240685321));
#89059=CARTESIAN_POINT('Ctrl Pts',(-6.37223883225711,-3.23102988858874,
-0.360448280759603));
#89060=CARTESIAN_POINT('Ctrl Pts',(-6.21369562826727,-1.45361424465813,
-2.90800322073118));
#89061=CARTESIAN_POINT('Ctrl Pts',(-6.0551524242774,1.65085630210701,-2.80074107583137));
#89062=CARTESIAN_POINT('Ctrl Pts',(-5.89660922028756,3.24820282498693,-0.136585181498785));
#89063=CARTESIAN_POINT('Ctrl Pts',(-5.73806601629771,1.88015223501989,2.6522640662656));
#89064=CARTESIAN_POINT('Ctrl Pts',(-5.57952281230785,-1.20435459546967,
3.01976938066863));
#89065=CARTESIAN_POINT('Ctrl Pts',(-5.42097960831801,-3.18936430935001,
0.630422403087696));
#89066=CARTESIAN_POINT('Ctrl Pts',(-5.26243640432815,-2.26269263374579,
-2.33445906994125));
#89067=CARTESIAN_POINT('Ctrl Pts',(-5.10389320033831,0.729669691378021,
-3.16813182262423));
#89068=CARTESIAN_POINT('Ctrl Pts',(-4.94534999634845,3.05589122646074,-1.1095070600019));
#89069=CARTESIAN_POINT('Ctrl Pts',(-4.78680679235861,2.5922835825938,1.96202521169489));
#89070=CARTESIAN_POINT('Ctrl Pts',(-4.62826358836875,-0.237909728900899,
3.24235656041923));
#89071=CARTESIAN_POINT('Ctrl Pts',(-4.46972038437891,-2.85090699059066,
1.56262805417741));
#89072=CARTESIAN_POINT('Ctrl Pts',(-4.31117718038905,-2.8612122974878,-1.54367784580477));
#89073=CARTESIAN_POINT('Ctrl Pts',(-4.1526339763992,-0.259417578310609,
-3.24070665505491));
#89074=CARTESIAN_POINT('Ctrl Pts',(-3.99409077240935,2.57920845458475,-1.9791818653152));
#89075=CARTESIAN_POINT('Ctrl Pts',(-3.8355475684195,3.06318555532124,1.08920675224771));
#89076=CARTESIAN_POINT('Ctrl Pts',(-3.67700436442965,0.750674236220715,
3.16322071595664));
#89077=CARTESIAN_POINT('Ctrl Pts',(-3.5184611604398,-2.24715366076796,2.34942068489859));
#89078=CARTESIAN_POINT('Ctrl Pts',(-3.35991795644995,-3.19347695750756,
-0.609247045658628));
#89079=CARTESIAN_POINT('Ctrl Pts',(-3.2013747524601,-1.22436432093936,-3.01171199675037));
#89080=CARTESIAN_POINT('Ctrl Pts',(-3.04283154847024,1.86251307291274,-2.66468052681201));
#89081=CARTESIAN_POINT('Ctrl Pts',(-2.88428834448039,3.24903750028975,0.115030304802324));
#89082=CARTESIAN_POINT('Ctrl Pts',(-2.72574514049054,1.66940305787883,2.78972595813986));
#89083=CARTESIAN_POINT('Ctrl Pts',(-2.56720193650069,-1.43428785770279,
2.91758398357915));
#89084=CARTESIAN_POINT('Ctrl Pts',(-2.40865873251084,-3.22856669792818,
0.381878240128784));
#89085=CARTESIAN_POINT('Ctrl Pts',(-2.25011552852099,-2.07537665074434,
-2.50245726521425));
#89086=CARTESIAN_POINT('Ctrl Pts',(-2.09157232453114,0.972500075570423,
-3.10221293269348));
#89087=CARTESIAN_POINT('Ctrl Pts',(-1.93302912054129,3.13254143379656,-0.869850218312904));
#89088=CARTESIAN_POINT('Ctrl Pts',(-1.77448591655143,2.43278899751171,2.15662798198898));
#89089=CARTESIAN_POINT('Ctrl Pts',(-1.61594271256159,-0.487963927236016,
3.21424749456954));
#89090=CARTESIAN_POINT('Ctrl Pts',(-1.45739950857173,-2.96319376995764,
1.33746534153751));
#89091=CARTESIAN_POINT('Ctrl Pts',(-1.29885630458188,-2.73330498476118,
-1.7603285613275));
#89092=CARTESIAN_POINT('Ctrl Pts',(-1.14031310059203,-0.00792704373605107,
-3.25107038301062));
#89093=CARTESIAN_POINT('Ctrl Pts',(-0.981769896602184,2.72438177681566,
-1.77377241999862));
#89094=CARTESIAN_POINT('Ctrl Pts',(-0.823226692612331,2.97009258251906,
1.32281660000969));
#89095=CARTESIAN_POINT('Ctrl Pts',(-0.664683488622481,0.50318519799852,
3.21185105264258));
#89096=CARTESIAN_POINT('Ctrl Pts',(-0.506140284632631,-2.42095780227635,
2.1685007547554));
#89097=CARTESIAN_POINT('Ctrl Pts',(-0.347597080642779,-3.13905144094015,
-0.854204491070011));
#89098=CARTESIAN_POINT('Ctrl Pts',(-0.189053876652928,-0.983164721863736,
-3.09783529230121));
#89099=CARTESIAN_POINT('Ctrl Pts',(-0.0833584073263618,1.04003326818453,
-2.70672672180107));
#89100=CARTESIAN_POINT('Ctrl Pts',(-0.0305106726630785,1.7462666632106,
-2.12687519173954));
#89101=CARTESIAN_POINT('Ctrl Pts',(-15.458,-1.28892185405323,2.64462557919717));
#89102=CARTESIAN_POINT('Ctrl Pts',(-15.4051522653367,-2.16707535766416,
2.21663635799288));
#89103=CARTESIAN_POINT('Ctrl Pts',(-15.2994567960101,-3.44854740058839,
0.424711614190816));
#89104=CARTESIAN_POINT('Ctrl Pts',(-15.1409135920203,-2.22865703262986,
-2.6700064292174));
#89105=CARTESIAN_POINT('Ctrl Pts',(-14.9823703880304,1.02878186533068,-3.31884566424105));
#89106=CARTESIAN_POINT('Ctrl Pts',(-14.8238271840406,3.34550632858596,-0.941959775855578));
#89107=CARTESIAN_POINT('Ctrl Pts',(-14.6652839800507,2.60878567205529,2.29703091687943));
#89108=CARTESIAN_POINT('Ctrl Pts',(-14.5067407760609,-0.509995818531524,
3.43785590082803));
#89109=CARTESIAN_POINT('Ctrl Pts',(-14.348197572071,-3.1629699559395,1.44073219523085));
#89110=CARTESIAN_POINT('Ctrl Pts',(-14.1896543680812,-2.92847127329083,
-1.87199435197442));
#89111=CARTESIAN_POINT('Ctrl Pts',(-14.0311111640913,-0.0204107596905135,
-3.47555085476599));
#89112=CARTESIAN_POINT('Ctrl Pts',(-13.8725679601015,2.90625269486543,-1.90624082299241));
#89113=CARTESIAN_POINT('Ctrl Pts',(-13.7140247561117,3.17971327505761,1.40338684733669));
#89114=CARTESIAN_POINT('Ctrl Pts',(-13.5554815521218,0.550294805988092,
3.43179080425185));
#89115=CARTESIAN_POINT('Ctrl Pts',(-13.3969383481319,-2.58150248454107,
2.32720592344252));
#89116=CARTESIAN_POINT('Ctrl Pts',(-13.2383951441421,-3.35655885375399,
-0.901972369120892));
#89117=CARTESIAN_POINT('Ctrl Pts',(-13.0798519401522,-1.06729492223842,
-3.30770545730824));
#89118=CARTESIAN_POINT('Ctrl Pts',(-12.9213087361624,2.19633896027193,-2.6937211511252));
#89119=CARTESIAN_POINT('Ctrl Pts',(-12.7627655321725,3.45485909598007,0.379455609436187));
#89120=CARTESIAN_POINT('Ctrl Pts',(-12.6042223281827,1.55931826225864,3.10621369635386));
#89121=CARTESIAN_POINT('Ctrl Pts',(-12.4456791241928,-1.7597782505868,2.99720172384735));
#89122=CARTESIAN_POINT('Ctrl Pts',(-12.287135920203,-3.47231215925049,0.151940126291566));
#89123=CARTESIAN_POINT('Ctrl Pts',(-12.1285927162131,-2.0148517395434,-2.83203281857732));
#89124=CARTESIAN_POINT('Ctrl Pts',(-11.9700495122233,1.28203676115426,-3.23054473155214));
#89125=CARTESIAN_POINT('Ctrl Pts',(-11.8115063082334,3.40850940643008,-0.679780199445849));
#89126=CARTESIAN_POINT('Ctrl Pts',(-11.6529631042436,2.42323549242424,2.49157926396243));
#89127=CARTESIAN_POINT('Ctrl Pts',(-11.4944199002537,-0.774294217817315,
3.38828953295737));
#89128=CARTESIAN_POINT('Ctrl Pts',(-11.3358766962639,-3.26494385974007,
1.1917126679311));
#89129=CARTESIAN_POINT('Ctrl Pts',(-11.177333492274,-2.7749129165536,-2.09282005782018));
#89130=CARTESIAN_POINT('Ctrl Pts',(-11.0187902882842,0.248432352628435,
-3.46674470607068));
#89131=CARTESIAN_POINT('Ctrl Pts',(-10.8602470842943,3.04497510347621,-1.67575777166922));
#89132=CARTESIAN_POINT('Ctrl Pts',(-10.7017038803045,3.06165438295654,1.64508660237767));
#89133=CARTESIAN_POINT('Ctrl Pts',(-10.5431606763146,0.283243097960434,
3.46407431180885));
#89134=CARTESIAN_POINT('Ctrl Pts',(-10.3846174723248,-2.75375064331868,
2.12058833453552));
#89135=CARTESIAN_POINT('Ctrl Pts',(-10.2260742683349,-3.27674983216047,
-1.15885634466949));
#89136=CARTESIAN_POINT('Ctrl Pts',(-10.0675310643451,-0.808290354369253,
-3.38034083979924));
#89137=CARTESIAN_POINT('Ctrl Pts',(-9.90898786035523,2.39808544587535,-2.51579484148479));
#89138=CARTESIAN_POINT('Ctrl Pts',(-9.75044465636536,3.41516579853967,0.645507597668011));
#89139=CARTESIAN_POINT('Ctrl Pts',(-9.59190145237552,1.31442274406572,3.21750374359528));
#89140=CARTESIAN_POINT('Ctrl Pts',(-9.43335824838566,-1.98630246063877,
2.85212903372624));
#89141=CARTESIAN_POINT('Ctrl Pts',(-9.27481504439582,-3.47366319908915,
-0.11705327615242));
#89142=CARTESIAN_POINT('Ctrl Pts',(-9.11627184040597,-1.78979622283581,
-2.97937358699568));
#89143=CARTESIAN_POINT('Ctrl Pts',(-8.95772863641611,1.52803785391757,-3.12172032814591));
#89144=CARTESIAN_POINT('Ctrl Pts',(-8.79918543242626,3.45087313149815,-0.414140218366475));
#89145=CARTESIAN_POINT('Ctrl Pts',(-8.64064222843643,2.22328653818369,2.67152287268811));
#89146=CARTESIAN_POINT('Ctrl Pts',(-8.48209902444655,-1.03401551213445,
3.31825999747305));
#89147=CARTESIAN_POINT('Ctrl Pts',(-8.32355582045672,-3.3473289079468,0.935642384775419));
#89148=CARTESIAN_POINT('Ctrl Pts',(-8.16501261646686,-2.60474954884449,
-2.30115563966434));
#89149=CARTESIAN_POINT('Ctrl Pts',(-8.00646941247702,0.515796091307738,
-3.43714880131137));
#89150=CARTESIAN_POINT('Ctrl Pts',(-7.84792620848715,3.16545357502616,-1.43524950949952));
#89151=CARTESIAN_POINT('Ctrl Pts',(-7.68938300449731,2.92525860863845,1.87693888093117));
#89152=CARTESIAN_POINT('Ctrl Pts',(-7.53083980050746,0.0144935147776107,
3.47560461332901));
#89153=CARTESIAN_POINT('Ctrl Pts',(-7.37229659651761,-2.90950321183286,
1.9012702465717));
#89154=CARTESIAN_POINT('Ctrl Pts',(-7.21375339252776,-3.1773134596265,-1.40879972651929));
#89155=CARTESIAN_POINT('Ctrl Pts',(-7.0552101885379,-0.544443956973644,
-3.43272752601767));
#89156=CARTESIAN_POINT('Ctrl Pts',(-6.89666698454805,2.5854673331244,-2.32279920774723));
#89157=CARTESIAN_POINT('Ctrl Pts',(-6.7381237805582,3.35501574624132,0.907693137925664));
#89158=CARTESIAN_POINT('Ctrl Pts',(-6.57958057656835,1.06165382293352,3.30952090949962));
#89159=CARTESIAN_POINT('Ctrl Pts',(-6.42103737257851,-2.20092872820912,
2.68997216035933));
#89160=CARTESIAN_POINT('Ctrl Pts',(-6.26249416858865,-3.45420704317407,
-0.385345550190368));
#89161=CARTESIAN_POINT('Ctrl Pts',(-6.1039509645988,-1.55401984354575,-3.10886793158384));
#89162=CARTESIAN_POINT('Ctrl Pts',(-5.94540776060894,1.76488601549179,-2.99419686101054));
#89163=CARTESIAN_POINT('Ctrl Pts',(-5.7868645566191,3.47256616701507,-0.146019539340268));
#89164=CARTESIAN_POINT('Ctrl Pts',(-5.62832135262924,2.01002012249471,2.8354640885274));
#89165=CARTESIAN_POINT('Ctrl Pts',(-5.4697781486394,-1.2875430650898,3.22835412334209));
#89166=CARTESIAN_POINT('Ctrl Pts',(-5.31123494464955,-3.40966349445213,
0.673967614045017));
#89167=CARTESIAN_POINT('Ctrl Pts',(-5.15269174065969,-2.4189837610684,-2.49570732535522));
#89168=CARTESIAN_POINT('Ctrl Pts',(-4.99414853666985,0.780070217254916,
-3.38696441467844));
#89169=CARTESIAN_POINT('Ctrl Pts',(-4.83560533267999,3.26697101592738,-1.18614411913841));
#89170=CARTESIAN_POINT('Ctrl Pts',(-4.67706212869014,2.77134056869127,2.09754831704194));
#89171=CARTESIAN_POINT('Ctrl Pts',(-4.51851892470029,-0.254342884326582,
3.46631608300398));
#89172=CARTESIAN_POINT('Ctrl Pts',(-4.35997572071044,-3.04782788952586,
1.67056357159192));
#89173=CARTESIAN_POINT('Ctrl Pts',(-4.20143251672059,-3.05884501561062,
-1.65030441414442));
#89174=CARTESIAN_POINT('Ctrl Pts',(-4.04288931273074,-0.277336346930273,
-3.46455221361046));
#89175=CARTESIAN_POINT('Ctrl Pts',(-3.88434610874088,2.75736230144626,-2.11589003340364));
#89176=CARTESIAN_POINT('Ctrl Pts',(-3.72580290475104,3.27476918647795,1.16444160679989));
#89177=CARTESIAN_POINT('Ctrl Pts',(-3.56725970076118,0.802525610499856,
3.38171408279482));
#89178=CARTESIAN_POINT('Ctrl Pts',(-3.40871649677134,-2.4023714635179,2.5117023849941));
#89179=CARTESIAN_POINT('Ctrl Pts',(-3.25017329278148,-3.41406021584493,
-0.651329609663918));
#89180=CARTESIAN_POINT('Ctrl Pts',(-3.09163008879163,-1.30893492373327,
-3.21974019117812));
#89181=CARTESIAN_POINT('Ctrl Pts',(-2.93308688480178,1.99116256930354,-2.84873819212584));
#89182=CARTESIAN_POINT('Ctrl Pts',(-2.77454368081193,3.47345849590375,0.122975801130747));
#89183=CARTESIAN_POINT('Ctrl Pts',(-2.61600047682208,1.78471385262861,2.98242089532051));
#89184=CARTESIAN_POINT('Ctrl Pts',(-2.45745727283223,-1.53335852370586,
3.11911046713741));
#89185=CARTESIAN_POINT('Ctrl Pts',(-2.29891406884238,-3.45157371237187,
0.408255742649282));
#89186=CARTESIAN_POINT('Ctrl Pts',(-2.14037086485253,-2.21872928800771,
-2.67530967177796));
#89187=CARTESIAN_POINT('Ctrl Pts',(-1.98182766086268,1.03967364164181,-3.31649230463043));
#89188=CARTESIAN_POINT('Ctrl Pts',(-1.82328445687283,3.34891568842182,-0.929933443579305));
#89189=CARTESIAN_POINT('Ctrl Pts',(-1.66474125288297,2.60082920292383,2.30559289816608));
#89190=CARTESIAN_POINT('Ctrl Pts',(-1.50619804889312,-0.521669093878197,
3.43626543767323));
#89191=CARTESIAN_POINT('Ctrl Pts',(-1.34765484490327,-3.16787066149606,
1.42984817907643));
#89192=CARTESIAN_POINT('Ctrl Pts',(-1.18911164091342,-2.92210275208215,
-1.8819198597676));
#89193=CARTESIAN_POINT('Ctrl Pts',(-1.03056843692357,-0.00847458898519691,
-3.47563179607567));
#89194=CARTESIAN_POINT('Ctrl Pts',(-0.872025232933723,2.91256319076703,
-1.89629232703364));
#89195=CARTESIAN_POINT('Ctrl Pts',(-0.713482028943869,3.17524599622243,
1.41418760399544));
#89196=CARTESIAN_POINT('Ctrl Pts',(-0.554938824954021,0.537941744545933,
3.43370346614461));
#89197=CARTESIAN_POINT('Ctrl Pts',(-0.396395620964168,-2.58818079070841,
2.3182857598003));
#89198=CARTESIAN_POINT('Ctrl Pts',(-0.237852416974318,-3.35587536174639,
-0.913207017918879));
#89199=CARTESIAN_POINT('Ctrl Pts',(-0.0793092129844665,-1.05107492779814,
-3.31181228717566));
#89200=CARTESIAN_POINT('Ctrl Pts',(0.0263862563420996,1.11187155921588,
-2.89368864689656));
#89201=CARTESIAN_POINT('Ctrl Pts',(0.079233991005383,1.86688666317375,-2.27378499134461));
#89202=CARTESIAN_POINT('Ctrl Pts',(-0.2801761170896,-2.94174543957041,-0.0025773274983063));
#89203=CARTESIAN_POINT('Ctrl Pts',(-0.270117411393067,-2.94340878728205,
-0.188616707269291));
#89204=CARTESIAN_POINT('Ctrl Pts',(-0.260058705696534,-2.92767190815943,
-0.374380454857518));
#89205=CARTESIAN_POINT('Ctrl Pts',(-0.25,-2.89371419577505,-0.556479620053392));
#89206=CARTESIAN_POINT('',(-15.458,-1.37702479013096,-1.93106208855769));
#89207=CARTESIAN_POINT('Ctrl Pts',(-15.458,-1.37998566170037,-1.93363955138647));
#89208=CARTESIAN_POINT('Ctrl Pts',(-15.458,-1.43347830229574,-1.9045572974682));
#89209=CARTESIAN_POINT('Ctrl Pts',(-15.458,-1.48566986876101,-1.8733427436734));
#89210=CARTESIAN_POINT('Ctrl Pts',(-15.458,-1.53641663480976,-1.84002474984019));
#89211=CARTESIAN_POINT('Ctrl Pts',(-15.458,-1.60460402297775,-1.79525604524328));
#89212=CARTESIAN_POINT('Ctrl Pts',(-15.458,-1.67018419084743,-1.74669183548175));
#89213=CARTESIAN_POINT('Ctrl Pts',(-15.458,-1.73307230563806,-1.69469097346931));
#89214=CARTESIAN_POINT('Ctrl Pts',(-15.458,-1.76968235674676,-1.66441889070279));
#89215=CARTESIAN_POINT('Ctrl Pts',(-15.458,-1.80537978873803,-1.63298117771037));
#89216=CARTESIAN_POINT('Ctrl Pts',(-15.458,-1.84014472377397,-1.60044134393351));
#89217=CARTESIAN_POINT('Ctrl Pts',(-15.458,-1.85372686908611,-1.58772851273353));
#89218=CARTESIAN_POINT('Ctrl Pts',(-15.458,-1.86716665434422,-1.57484740618035));
#89219=CARTESIAN_POINT('Ctrl Pts',(-15.458,-1.88046277856858,-1.56180161460873));
#89220=CARTESIAN_POINT('Ctrl Pts',(-15.458,-1.89078117069646,-1.55167749191079));
#89221=CARTESIAN_POINT('Ctrl Pts',(-15.458,-1.90101141569677,-1.54145570679727));
#89222=CARTESIAN_POINT('Ctrl Pts',(-15.458,-1.91114679361931,-1.53114448488591));
#89223=CARTESIAN_POINT('Ctrl Pts',(-15.458,-1.97104061151735,-1.47021153771948));
#89224=CARTESIAN_POINT('Ctrl Pts',(-15.458,-2.02768651729067,-1.40609792454873));
#89225=CARTESIAN_POINT('Ctrl Pts',(-15.458,-2.08099125696457,-1.33919592441725));
#89226=CARTESIAN_POINT('Ctrl Pts',(-15.458,-2.12753187286875,-1.28078347722422));
#89227=CARTESIAN_POINT('Ctrl Pts',(-15.458,-2.17152540896558,-1.22024428012911));
#89228=CARTESIAN_POINT('Ctrl Pts',(-15.458,-2.21289384890174,-1.15781096868051));
#89229=CARTESIAN_POINT('Ctrl Pts',(-15.458,-2.23284077791439,-1.12770703356929));
#89230=CARTESIAN_POINT('Ctrl Pts',(-15.458,-2.25217713735731,-1.09716236855975));
#89231=CARTESIAN_POINT('Ctrl Pts',(-15.458,-2.27089265932552,-1.06620124816656));
#89232=CARTESIAN_POINT('Ctrl Pts',(-15.458,-2.28230086503392,-1.04732863371274));
#89233=CARTESIAN_POINT('Ctrl Pts',(-15.458,-2.2934813528384,-1.02829576315832));
#89234=CARTESIAN_POINT('Ctrl Pts',(-15.458,-2.3044146678338,-1.00913842369171));
#89235=CARTESIAN_POINT('Ctrl Pts',(-15.458,-2.34835022708968,-0.932154597315731));
#89236=CARTESIAN_POINT('Ctrl Pts',(-15.458,-2.38834257191954,-0.853093023880235));
#89237=CARTESIAN_POINT('Ctrl Pts',(-15.458,-2.4242944129843,-0.772350635534902));
#89238=CARTESIAN_POINT('Ctrl Pts',(-15.458,-2.46266928377817,-0.686166489505774));
#89239=CARTESIAN_POINT('Ctrl Pts',(-15.458,-2.49644173827623,-0.598066862910968));
#89240=CARTESIAN_POINT('Ctrl Pts',(-15.458,-2.52545351592011,-0.508485325700583));
#89241=CARTESIAN_POINT('Ctrl Pts',(-15.458,-2.54721234915301,-0.441299172792795));
#89242=CARTESIAN_POINT('Ctrl Pts',(-15.458,-2.5662925310425,-0.373278292061055));
#89243=CARTESIAN_POINT('Ctrl Pts',(-15.458,-2.58260842417879,-0.304592361318692));
#89244=CARTESIAN_POINT('Ctrl Pts',(-15.458,-2.59484534403102,-0.25307791326192));
#89245=CARTESIAN_POINT('Ctrl Pts',(-15.458,-2.60552703202891,-0.20118912404049));
#89246=CARTESIAN_POINT('Ctrl Pts',(-15.458,-2.61461037966331,-0.148994900882582));
#89247=CARTESIAN_POINT('Ctrl Pts',(-15.458,-2.6171362359893,-0.134480966807842));
#89248=CARTESIAN_POINT('Ctrl Pts',(-15.458,-2.6195384609721,-0.119943404900011));
#89249=CARTESIAN_POINT('Ctrl Pts',(-15.458,-2.62181603752144,-0.105383677115885));
#89250=CARTESIAN_POINT('Ctrl Pts',(-15.458,-2.62401192290557,-0.0913461715719244));
#89251=CARTESIAN_POINT('Ctrl Pts',(-15.458,-2.626090686319,-0.0772958939545234));
#89252=CARTESIAN_POINT('Ctrl Pts',(-15.458,-2.62805114010171,-0.0632393621128043));
#89253=CARTESIAN_POINT('Ctrl Pts',(-15.458,-2.64083969310654,0.0284550731791334));
#89254=CARTESIAN_POINT('Ctrl Pts',(-15.458,-2.64860794987797,0.120481249385476));
#89255=CARTESIAN_POINT('Ctrl Pts',(-15.458,-2.65122213956709,0.212444566688069));
#89256=CARTESIAN_POINT('Ctrl Pts',(-15.458,-2.65227583835989,0.24951212793885));
#89257=CARTESIAN_POINT('Ctrl Pts',(-15.458,-2.65249170062149,0.286569819973956));
#89258=CARTESIAN_POINT('Ctrl Pts',(-15.458,-2.6518588794726,0.323592979930078));
#89259=CARTESIAN_POINT('Ctrl Pts',(-15.458,-2.65034341185433,0.412255313889691));
#89260=CARTESIAN_POINT('Ctrl Pts',(-15.458,-2.64396453755206,0.500719073352961));
#89261=CARTESIAN_POINT('Ctrl Pts',(-15.458,-2.63296674054628,0.588722862793259));
#89262=CARTESIAN_POINT('Ctrl Pts',(-15.458,-2.62174854388975,0.67849027857141));
#89263=CARTESIAN_POINT('Ctrl Pts',(-15.458,-2.60572434059568,0.767779835098673));
#89264=CARTESIAN_POINT('Ctrl Pts',(-15.458,-2.58509965927721,0.85631746801127));
#89265=CARTESIAN_POINT('Ctrl Pts',(-15.458,-2.58093104674581,0.874212488077799));
#89266=CARTESIAN_POINT('Ctrl Pts',(-15.458,-2.57657432765316,0.892076780351709));
#89267=CARTESIAN_POINT('Ctrl Pts',(-15.458,-2.5720309446835,0.909908055300652));
#89268=CARTESIAN_POINT('Ctrl Pts',(-15.458,-2.56862062286144,0.923292440125721));
#89269=CARTESIAN_POINT('Ctrl Pts',(-15.458,-2.56510534954551,0.936657094581119));
#89270=CARTESIAN_POINT('Ctrl Pts',(-15.458,-2.56148926917185,0.949988846813725));
#89271=CARTESIAN_POINT('Ctrl Pts',(-15.458,-2.53726799609416,1.03928775006344));
#89272=CARTESIAN_POINT('Ctrl Pts',(-15.458,-2.50849153567128,1.12725652713466));
#89273=CARTESIAN_POINT('Ctrl Pts',(-15.458,-2.47545031643021,1.21361290371913));
#89274=CARTESIAN_POINT('Ctrl Pts',(-15.458,-2.44176584027502,1.30165049357576));
#89275=CARTESIAN_POINT('Ctrl Pts',(-15.458,-2.40364877016699,1.38801307200986));
#89276=CARTESIAN_POINT('Ctrl Pts',(-15.458,-2.36135133676212,1.4724048350925));
#89277=CARTESIAN_POINT('Ctrl Pts',(-15.458,-2.31867994269378,1.55754272381856));
#89278=CARTESIAN_POINT('Ctrl Pts',(-15.458,-2.27175365245138,1.64067566687927));
#89279=CARTESIAN_POINT('Ctrl Pts',(-15.458,-2.22077908013504,1.72149066351755));
#89280=CARTESIAN_POINT('Ctrl Pts',(-15.458,-2.19135516133176,1.76813929225768));
#89281=CARTESIAN_POINT('Ctrl Pts',(-15.458,-2.16058144437314,1.81401536176244));
#89282=CARTESIAN_POINT('Ctrl Pts',(-15.458,-2.12849042302997,1.859055511539));
#89283=CARTESIAN_POINT('Ctrl Pts',(-15.458,-2.12030608087635,1.87054233810272));
#89284=CARTESIAN_POINT('Ctrl Pts',(-15.458,-2.11203467242689,1.88197662493571));
#89285=CARTESIAN_POINT('Ctrl Pts',(-15.458,-2.10368112338145,1.89335125942451));
#89286=CARTESIAN_POINT('Ctrl Pts',(-15.458,-2.04549963217281,1.97257425708832));
#89287=CARTESIAN_POINT('Ctrl Pts',(-15.458,-1.983488402854,2.04870207909741));
#89288=CARTESIAN_POINT('Ctrl Pts',(-15.458,-1.91792260118989,2.12142699555156));
#89289=CARTESIAN_POINT('Ctrl Pts',(-15.458,-1.85213864268311,2.1943938893438));
#89290=CARTESIAN_POINT('Ctrl Pts',(-15.458,-1.78277602527643,2.26393609626659));
#89291=CARTESIAN_POINT('Ctrl Pts',(-15.458,-1.71006216878643,2.32972805253332));
#89292=CARTESIAN_POINT('Ctrl Pts',(-15.458,-1.63869844345376,2.3942984016079));
#89293=CARTESIAN_POINT('Ctrl Pts',(-15.458,-1.5641062449556,2.4552572514107));
#89294=CARTESIAN_POINT('Ctrl Pts',(-15.458,-1.48645909468778,2.51227033795963));
#89295=CARTESIAN_POINT('Ctrl Pts',(-15.458,-1.42265110390908,2.55912190286874));
#89296=CARTESIAN_POINT('Ctrl Pts',(-15.458,-1.35677924409571,2.60330862048415));
#89297=CARTESIAN_POINT('Ctrl Pts',(-15.458,-1.28892185405323,2.64462557919717));
#89298=CARTESIAN_POINT('Ctrl Pts',(-15.458,-1.37998566170039,-1.93363955138645));
#89299=CARTESIAN_POINT('Ctrl Pts',(-15.4092014596786,-0.787929274296016,
-2.35116721332258));
#89300=CARTESIAN_POINT('Ctrl Pts',(-15.3075551846939,0.877072683589833,
-2.62661234173148));
#89301=CARTESIAN_POINT('Ctrl Pts',(-15.153061175046,2.69704440340713,-0.759379027323357));
#89302=CARTESIAN_POINT('Ctrl Pts',(-14.9945179710561,2.10312284761966,1.85179574340887));
#89303=CARTESIAN_POINT('Ctrl Pts',(-14.8359747670663,-0.411142958056525,
2.77149379088676));
#89304=CARTESIAN_POINT('Ctrl Pts',(-14.7076054794126,-2.14284336011571,
1.46789272098577));
#89305=CARTESIAN_POINT('Ctrl Pts',(-14.6320839264221,-2.36934237783001,
0.339980147483457));
#89306=CARTESIAN_POINT('Ctrl Pts',(-14.609410108095,-2.36819900096358,0.000905669814256944));
#89307=CARTESIAN_POINT('Origin',(-15.458,-3.51939854619125E-16,0.));
#89308=CARTESIAN_POINT('',(-15.458,-2.942,-3.60291088309151E-16));
#89309=CARTESIAN_POINT('Origin',(-15.458,0.,0.));
#89310=CARTESIAN_POINT('Origin',(-15.458,0.,0.));
#89311=CARTESIAN_POINT('',(-15.458,1.37702479013102,-1.93106208855765));
#89312=CARTESIAN_POINT('Ctrl Pts',(-15.458,1.29201644558798,2.64838508500724));
#89313=CARTESIAN_POINT('Ctrl Pts',(-15.458,1.35598079841149,2.60984876276284));
#89314=CARTESIAN_POINT('Ctrl Pts',(-15.458,1.41827048161202,2.56877727889907));
#89315=CARTESIAN_POINT('Ctrl Pts',(-15.458,1.478712436698,2.52516206076636));
#89316=CARTESIAN_POINT('Ctrl Pts',(-15.458,1.55797887552663,2.46796300068971));
#89317=CARTESIAN_POINT('Ctrl Pts',(-15.458,1.6340690562504,2.40638958112882));
#89318=CARTESIAN_POINT('Ctrl Pts',(-15.458,1.7068062328737,2.34082102500523));
#89319=CARTESIAN_POINT('Ctrl Pts',(-15.458,1.74532859254324,2.30609524076032));
#89320=CARTESIAN_POINT('Ctrl Pts',(-15.458,1.78290977621518,2.27024832065862));
#89321=CARTESIAN_POINT('Ctrl Pts',(-15.458,1.81951847534658,2.23333368924381));
#89322=CARTESIAN_POINT('Ctrl Pts',(-15.458,1.83920400820175,2.21348364794776));
#89323=CARTESIAN_POINT('Ctrl Pts',(-15.458,1.85860828312012,2.19332484796848));
#89324=CARTESIAN_POINT('Ctrl Pts',(-15.458,1.87772598262537,2.17286543604939));
#89325=CARTESIAN_POINT('Ctrl Pts',(-15.458,1.88940700821849,2.16036461636752));
#89326=CARTESIAN_POINT('Ctrl Pts',(-15.458,1.90097975254709,2.14775284477581));
#89327=CARTESIAN_POINT('Ctrl Pts',(-15.458,1.91243540428845,2.13504078826461));
#89328=CARTESIAN_POINT('Ctrl Pts',(-15.458,1.97752404706709,2.06281351356038));
#89329=CARTESIAN_POINT('Ctrl Pts',(-15.458,2.0389078481352,1.98727494961689));
#89330=CARTESIAN_POINT('Ctrl Pts',(-15.458,2.09641417399276,1.90880097474144));
#89331=CARTESIAN_POINT('Ctrl Pts',(-15.458,2.14364962250154,1.84434278958995));
#89332=CARTESIAN_POINT('Ctrl Pts',(-15.458,2.18826826557574,1.77790325975163));
#89333=CARTESIAN_POINT('Ctrl Pts',(-15.458,2.23014995231654,1.70968105891695));
#89334=CARTESIAN_POINT('Ctrl Pts',(-15.458,2.24876201198549,1.67936337661968));
#89335=CARTESIAN_POINT('Ctrl Pts',(-15.458,2.26683325063596,1.64869356154499));
#89336=CARTESIAN_POINT('Ctrl Pts',(-15.458,2.28435161214332,1.61768881004261));
#89337=CARTESIAN_POINT('Ctrl Pts',(-15.458,2.29483893867365,1.59912788738667));
#89338=CARTESIAN_POINT('Ctrl Pts',(-15.458,2.30512810739652,1.58044692881486));
#89339=CARTESIAN_POINT('Ctrl Pts',(-15.458,2.31521636496224,1.56164961846106));
#89340=CARTESIAN_POINT('Ctrl Pts',(-15.458,2.32246704729265,1.54813952267358));
#89341=CARTESIAN_POINT('Ctrl Pts',(-15.458,2.32961371405895,1.53456959807542));
#89342=CARTESIAN_POINT('Ctrl Pts',(-15.458,2.33664916559811,1.52095359722892));
#89343=CARTESIAN_POINT('Ctrl Pts',(-15.458,2.38029635675402,1.43648137985685));
#89344=CARTESIAN_POINT('Ctrl Pts',(-15.458,2.41973243650582,1.35011673909372));
#89345=CARTESIAN_POINT('Ctrl Pts',(-15.458,2.4547939593135,1.26220655296561));
#89346=CARTESIAN_POINT('Ctrl Pts',(-15.458,2.49109107187097,1.17119835750465));
#89347=CARTESIAN_POINT('Ctrl Pts',(-15.458,2.52270054445843,1.0785327617823));
#89348=CARTESIAN_POINT('Ctrl Pts',(-15.458,2.54938259447905,0.98458420023318));
#89349=CARTESIAN_POINT('Ctrl Pts',(-15.458,2.57407579027275,0.897638473683871));
#89350=CARTESIAN_POINT('Ctrl Pts',(-15.458,2.59454836746826,0.809593140210348));
#89351=CARTESIAN_POINT('Ctrl Pts',(-15.458,2.61056092669808,0.720749094404554));
#89352=CARTESIAN_POINT('Ctrl Pts',(-15.458,2.61991094011146,0.668871502068452));
#89353=CARTESIAN_POINT('Ctrl Pts',(-15.458,2.62773935904613,0.61672171671261));
#89354=CARTESIAN_POINT('Ctrl Pts',(-15.458,2.63399052891176,0.564361823102604));
#89355=CARTESIAN_POINT('Ctrl Pts',(-15.458,2.63614843132954,0.546287199720975));
#89356=CARTESIAN_POINT('Ctrl Pts',(-15.458,2.63811861239107,0.528183596397594));
#89357=CARTESIAN_POINT('Ctrl Pts',(-15.458,2.63989627603494,0.510080720039946));
#89358=CARTESIAN_POINT('Ctrl Pts',(-15.458,2.64861266483537,0.421317185226454));
#89359=CARTESIAN_POINT('Ctrl Pts',(-15.458,2.65272106695796,0.332449891189197));
#89360=CARTESIAN_POINT('Ctrl Pts',(-15.458,2.65203956213944,0.24377021736768));
#89361=CARTESIAN_POINT('Ctrl Pts',(-15.458,2.65171699761295,0.201797048259159));
#89362=CARTESIAN_POINT('Ctrl Pts',(-15.458,2.65032064204942,0.159865954417084));
#89363=CARTESIAN_POINT('Ctrl Pts',(-15.458,2.64782714013714,0.118008441338152));
#89364=CARTESIAN_POINT('Ctrl Pts',(-15.458,2.64244816134619,0.02771347345198));
#89365=CARTESIAN_POINT('Ctrl Pts',(-15.458,2.63196657542956,-0.0622406233293999));
#89366=CARTESIAN_POINT('Ctrl Pts',(-15.458,2.6165783453312,-0.151520688076739));
#89367=CARTESIAN_POINT('Ctrl Pts',(-15.458,2.60079370843378,-0.243100642054985));
#89368=CARTESIAN_POINT('Ctrl Pts',(-15.458,2.57984588485276,-0.333972428620849));
#89369=CARTESIAN_POINT('Ctrl Pts',(-15.458,2.55390006101663,-0.423744721287635));
#89370=CARTESIAN_POINT('Ctrl Pts',(-15.458,2.55017192951763,-0.436644019230246));
#89371=CARTESIAN_POINT('Ctrl Pts',(-15.458,2.54634053796955,-0.449520548422734));
#89372=CARTESIAN_POINT('Ctrl Pts',(-15.458,2.54240631011605,-0.46237307584355));
#89373=CARTESIAN_POINT('Ctrl Pts',(-15.458,2.53826834072496,-0.475891196055698));
#89374=CARTESIAN_POINT('Ctrl Pts',(-15.458,2.53401895642664,-0.489375003499241));
#89375=CARTESIAN_POINT('Ctrl Pts',(-15.458,2.52966057660384,-0.50281859601556));
#89376=CARTESIAN_POINT('Ctrl Pts',(-15.458,2.50229503013095,-0.587228691217232));
#89377=CARTESIAN_POINT('Ctrl Pts',(-15.458,2.47061821529643,-0.67011473702423));
#89378=CARTESIAN_POINT('Ctrl Pts',(-15.458,2.43484287744197,-0.751173581138594));
#89379=CARTESIAN_POINT('Ctrl Pts',(-15.458,2.39912112064777,-0.832111022659138));
#89380=CARTESIAN_POINT('Ctrl Pts',(-15.458,2.35931244647116,-0.911227512394363));
#89381=CARTESIAN_POINT('Ctrl Pts',(-15.458,2.31558654972163,-0.988191253045081));
#89382=CARTESIAN_POINT('Ctrl Pts',(-15.458,2.27255883690487,-1.06392609157778));
#89383=CARTESIAN_POINT('Ctrl Pts',(-15.458,2.22573732113999,-1.13757699578186));
#89384=CARTESIAN_POINT('Ctrl Pts',(-15.458,2.17525294284896,-1.20878852905993));
#89385=CARTESIAN_POINT('Ctrl Pts',(-15.458,2.15800223012227,-1.23312179303172));
#89386=CARTESIAN_POINT('Ctrl Pts',(-15.458,2.14032361321456,-1.25716984887907));
#89387=CARTESIAN_POINT('Ctrl Pts',(-15.458,2.12222168617203,-1.28091724550889));
#89388=CARTESIAN_POINT('Ctrl Pts',(-15.458,2.11092470998078,-1.29573742314528));
#89389=CARTESIAN_POINT('Ctrl Pts',(-15.458,2.09946286113177,-1.31044048926918));
#89390=CARTESIAN_POINT('Ctrl Pts',(-15.458,2.08783720440675,-1.3250225466833));
#89391=CARTESIAN_POINT('Ctrl Pts',(-15.458,2.07930116483031,-1.33572929832211));
#89392=CARTESIAN_POINT('Ctrl Pts',(-15.458,2.07068208018384,-1.34636417148749));
#89393=CARTESIAN_POINT('Ctrl Pts',(-15.458,2.06198317460606,-1.35692290862301));
#89394=CARTESIAN_POINT('Ctrl Pts',(-15.458,2.00776228997665,-1.42273625294983));
#89395=CARTESIAN_POINT('Ctrl Pts',(-15.458,1.95041179714208,-1.48563387608283));
#89396=CARTESIAN_POINT('Ctrl Pts',(-15.458,1.8900901408264,-1.54531963924066));
#89397=CARTESIAN_POINT('Ctrl Pts',(-15.458,1.83071592658384,-1.60406794798104));
#89398=CARTESIAN_POINT('Ctrl Pts',(-15.458,1.7684625100101,-1.65970501421417));
#89399=CARTESIAN_POINT('Ctrl Pts',(-15.458,1.70345510229972,-1.7119059984751));
#89400=CARTESIAN_POINT('Ctrl Pts',(-15.458,1.64047369118742,-1.76248010634987));
#89401=CARTESIAN_POINT('Ctrl Pts',(-15.458,1.57490670552085,-1.80982925665588));
#89402=CARTESIAN_POINT('Ctrl Pts',(-15.458,1.50685234912452,-1.8536122879539));
#89403=CARTESIAN_POINT('Ctrl Pts',(-15.458,1.46453142187118,-1.88083961887897));
#89404=CARTESIAN_POINT('Ctrl Pts',(-15.458,1.42124829763283,-1.90668693330214));
#89405=CARTESIAN_POINT('Ctrl Pts',(-15.458,1.37702479013106,-1.93106208855762));
#89406=CARTESIAN_POINT('Origin',(-15.458,0.,0.));
#89407=CARTESIAN_POINT('Origin',(-17.306589891905,0.,0.));
#89408=CARTESIAN_POINT('Ctrl Pts',(-15.458,1.37702479013101,-1.93106208855765));
#89409=CARTESIAN_POINT('Ctrl Pts',(-15.4051522653367,2.01823803108889,-1.47381810153559));
#89410=CARTESIAN_POINT('Ctrl Pts',(-15.2994567960102,2.79847537909562,0.121597510273868));
#89411=CARTESIAN_POINT('Ctrl Pts',(-15.1409135920203,1.4163960290961,2.41971406834469));
#89412=CARTESIAN_POINT('Ctrl Pts',(-14.9823703880305,-1.25998309782399,
2.5017761501444));
#89413=CARTESIAN_POINT('Ctrl Pts',(-14.8709291546587,-2.33223647147471,
0.956512055862881));
#89414=CARTESIAN_POINT('Ctrl Pts',(-14.8123356559502,-2.37508585399071,
0.0869261581971881));
#89415=CARTESIAN_POINT('Ctrl Pts',(-14.806589891905,-2.37447732889499,0.00158904524625127));
#89416=CARTESIAN_POINT('Ctrl Pts',(-15.7872339910054,1.70810875200393,-2.39535560853239));
#89417=CARTESIAN_POINT('Ctrl Pts',(-15.7343862563421,2.50349163590743,-1.82817449339847));
#89418=CARTESIAN_POINT('Ctrl Pts',(-15.6286907870155,3.4713247877303,0.150833719922236));
#89419=CARTESIAN_POINT('Ctrl Pts',(-15.4701475830257,1.75694618640281,3.00149627451039));
#89420=CARTESIAN_POINT('Ctrl Pts',(-15.3116043790358,-1.56292622485423,
3.10328889373875));
#89421=CARTESIAN_POINT('Ctrl Pts',(-15.153061175046,-3.45515176952641,0.376332500485629));
#89422=CARTESIAN_POINT('Ctrl Pts',(-14.9945179710561,-2.19346697899567,
-2.69644503550222));
#89423=CARTESIAN_POINT('Ctrl Pts',(-14.8359747670663,1.07092856027493,-3.30636730605605));
#89424=CARTESIAN_POINT('Ctrl Pts',(-14.6774315630764,3.35752184538448,-0.898407700729471));
#89425=CARTESIAN_POINT('Ctrl Pts',(-14.5188883590866,2.57897675157689,2.33006158656791));
#89426=CARTESIAN_POINT('Ctrl Pts',(-14.3603451550967,-0.554037067026588,
3.43116822011167));
#89427=CARTESIAN_POINT('Ctrl Pts',(-14.2018019511069,-3.1812348231794,1.39993047848449));
#89428=CARTESIAN_POINT('Ctrl Pts',(-14.043258747117,-2.90418145753586,-1.90939854479434));
#89429=CARTESIAN_POINT('Ctrl Pts',(-13.8847155431272,0.0242044611793096,
-3.4755472053722));
#89430=CARTESIAN_POINT('Ctrl Pts',(-13.7261723391373,2.93049093833658,-1.86876081417929));
#89431=CARTESIAN_POINT('Ctrl Pts',(-13.5676291351475,3.16143174166768,1.44408880709405));
#89432=CARTESIAN_POINT('Ctrl Pts',(-13.4090859311576,0.506191123030663,
3.43857616763681));
#89433=CARTESIAN_POINT('Ctrl Pts',(-13.2505427271678,-2.61116860653983,
2.29386979327385));
#89434=CARTESIAN_POINT('Ctrl Pts',(-13.0919995231779,-3.3447020505759,-0.944990889370293));
#89435=CARTESIAN_POINT('Ctrl Pts',(-12.9334563191881,-1.02474079682209,
-3.32113609006922));
#89436=CARTESIAN_POINT('Ctrl Pts',(-12.7749131151982,2.23074185365558,-2.66530112798528));
#89437=CARTESIAN_POINT('Ctrl Pts',(-12.6163699112084,3.44970285607524,0.42377988943034));
#89438=CARTESIAN_POINT('Ctrl Pts',(-12.4578267072185,1.51931035945226,3.12597746418898));
#89439=CARTESIAN_POINT('Ctrl Pts',(-12.2992835032287,-1.79811329678141,
2.9743617379259));
#89440=CARTESIAN_POINT('Ctrl Pts',(-12.1407402992388,-3.47397691061775,
0.10734791350577));
#89441=CARTESIAN_POINT('Ctrl Pts',(-11.982197095249,-1.97832640971397,-2.85766753731015));
#89442=CARTESIAN_POINT('Ctrl Pts',(-11.8236538912591,1.32340694269406,-3.21381910126486));
#89443=CARTESIAN_POINT('Ctrl Pts',(-11.6651106872693,3.41695615859637,-0.63596364452411));
#89444=CARTESIAN_POINT('Ctrl Pts',(-11.5065674832794,2.39104748524451,2.52248509786409));
#89445=CARTESIAN_POINT('Ctrl Pts',(-11.3480242792896,-0.817731436977695,
3.37806963288756));
#89446=CARTESIAN_POINT('Ctrl Pts',(-11.1894810752997,-3.27997494478484,
1.1496971377047));
#89447=CARTESIAN_POINT('Ctrl Pts',(-11.0309378713099,-2.74781546864746,
-2.12827378338047));
#89448=CARTESIAN_POINT('Ctrl Pts',(-10.87239466732,0.292920132913095,-3.46326968958119));
#89449=CARTESIAN_POINT('Ctrl Pts',(-10.7138514633302,3.06623877709696,-1.63652647663751));
#89450=CARTESIAN_POINT('Ctrl Pts',(-10.5553082593403,3.04028160421297,1.68425856506386));
#89451=CARTESIAN_POINT('Ctrl Pts',(-10.3967650553505,0.238745818439147,
3.46742549755881));
#89452=CARTESIAN_POINT('Ctrl Pts',(-10.2382218513606,-2.7807493125031,2.08505932959628));
#89453=CARTESIAN_POINT('Ctrl Pts',(-10.0796786473708,-3.26160186872235,
-1.20082987840549));
#89454=CARTESIAN_POINT('Ctrl Pts',(-9.92113544338089,-0.764824859953005,
-3.39043980635655));
#89455=CARTESIAN_POINT('Ctrl Pts',(-9.76259223939106,2.43018731260948,-2.48479954373748));
#89456=CARTESIAN_POINT('Ctrl Pts',(-9.60404903540119,3.40659712910876,0.689300476479223));
#89457=CARTESIAN_POINT('Ctrl Pts',(-9.44550583141137,1.27300617423425,3.2341141642324));
#89458=CARTESIAN_POINT('Ctrl Pts',(-9.2869626274215,-2.02275630659,2.82639276659792));
#89459=CARTESIAN_POINT('Ctrl Pts',(-9.12841942343164,-3.47187433977975,
-0.161640699409721));
#89460=CARTESIAN_POINT('Ctrl Pts',(-8.96987621944181,-1.75139777002538,
-3.00210675993993));
#89461=CARTESIAN_POINT('Ctrl Pts',(-8.81133301545194,1.56799061974407,-3.10184534806643));
#89462=CARTESIAN_POINT('Ctrl Pts',(-8.6527898114621,3.45590594354905,-0.369801644492143));
#89463=CARTESIAN_POINT('Ctrl Pts',(-8.49424660747225,2.18880476763518,2.69984681715543));
#89464=CARTESIAN_POINT('Ctrl Pts',(-8.3357034034824,-1.07653225999301,3.30471140042836));
#89465=CARTESIAN_POINT('Ctrl Pts',(-8.17716019949254,-3.35906561812389,
0.892590230769289));
#89466=CARTESIAN_POINT('Ctrl Pts',(-8.0186169955027,-2.57499137120645,-2.33440754478286));
#89467=CARTESIAN_POINT('Ctrl Pts',(-7.86007379151284,0.559881883408217,
-3.43024363909593));
#89468=CARTESIAN_POINT('Ctrl Pts',(-7.701530587523,3.18361953164334,-1.39449124223347));
#89469=CARTESIAN_POINT('Ctrl Pts',(-7.54298738353313,2.90092039738697,1.91434061623083));
#89470=CARTESIAN_POINT('Ctrl Pts',(-7.38444417954331,-0.0301296664458408,
3.47550447419172));
#89471=CARTESIAN_POINT('Ctrl Pts',(-7.22590097555343,-2.93367331189794,
1.86375965349199));
#89472=CARTESIAN_POINT('Ctrl Pts',(-7.0673577715636,-3.15896475517418,-1.44947605102469));
#89473=CARTESIAN_POINT('Ctrl Pts',(-6.90881456757374,-0.50032761723165,
-3.43943475332242));
#89474=CARTESIAN_POINT('Ctrl Pts',(-6.75027136358389,2.61507597020796,-2.2894140772188));
#89475=CARTESIAN_POINT('Ctrl Pts',(-6.59172815959404,3.34308592807698,0.950692181739598));
#89476=CARTESIAN_POINT('Ctrl Pts',(-6.43318495560419,1.01907669463965,3.32287854688806));
#89477=CARTESIAN_POINT('Ctrl Pts',(-6.27464175161433,-2.23528302824535,
2.66149374047064));
#89478=CARTESIAN_POINT('Ctrl Pts',(-6.11609854762449,-3.44897528191934,
-0.429661089276792));
#89479=CARTESIAN_POINT('Ctrl Pts',(-5.95755534363462,-1.5139782774571,-3.12856339592352));
#89480=CARTESIAN_POINT('Ctrl Pts',(-5.79901213964479,1.8031820507789,-2.97129157752513));
#89481=CARTESIAN_POINT('Ctrl Pts',(-5.64046893565492,3.4741548915317,-0.10142453642758));
#89482=CARTESIAN_POINT('Ctrl Pts',(-5.48192573166509,1.97345113447355,2.86103648469429));
#89483=CARTESIAN_POINT('Ctrl Pts',(-5.32338252767522,-1.32888466706206,
3.21155798461682));
#89484=CARTESIAN_POINT('Ctrl Pts',(-5.16483932368538,-3.41803552688201,
0.630136718506388));
#89485=CARTESIAN_POINT('Ctrl Pts',(-5.00629611969552,-2.38674310488516,
-2.52655823167527));
#89486=CARTESIAN_POINT('Ctrl Pts',(-4.84775291570568,0.823489947766338,
-3.37667046849267));
#89487=CARTESIAN_POINT('Ctrl Pts',(-4.68920971171582,3.28193044174787,-1.14410302122984));
#89488=CARTESIAN_POINT('Ctrl Pts',(-4.53066650772598,2.74418271036083,2.13295578899264));
#89489=CARTESIAN_POINT('Ctrl Pts',(-4.37212330373612,-0.298824674553444,
3.46276521883943));
#89490=CARTESIAN_POINT('Ctrl Pts',(-4.21358009974627,-3.06902464253253,
1.63129607832356));
#89491=CARTESIAN_POINT('Ctrl Pts',(-4.05503689575642,-3.03740547736332,
-1.68943987855481));
#89492=CARTESIAN_POINT('Ctrl Pts',(-3.89649369176657,-0.232833420739063,
-3.46782752573225));
#89493=CARTESIAN_POINT('Ctrl Pts',(-3.73795048777672,2.78430035827296,-2.08031504609778));
#89494=CARTESIAN_POINT('Ctrl Pts',(-3.57940728378687,3.2595496698979,1.2063892507913));
#89495=CARTESIAN_POINT('Ctrl Pts',(-3.42086407979702,0.759042977753982,
3.39173892683704));
#89496=CARTESIAN_POINT('Ctrl Pts',(-3.26232087580717,-2.43442046921783,
2.48065239393666));
#89497=CARTESIAN_POINT('Ctrl Pts',(-3.10377767181732,-3.40541682692287,
-0.695107807712134));
#89498=CARTESIAN_POINT('Ctrl Pts',(-2.94523446782747,-1.26749021503053,
-3.2362799852487));
#89499=CARTESIAN_POINT('Ctrl Pts',(-2.78669126383761,2.02757271466167,-2.82293978097886));
#89500=CARTESIAN_POINT('Ctrl Pts',(-2.62814805984777,3.47159317035164,0.167560058613843));
#89501=CARTESIAN_POINT('Ctrl Pts',(-2.46960485585791,1.74627754747723,3.00508866211552));
#89502=CARTESIAN_POINT('Ctrl Pts',(-2.31106165186806,-1.57327897331545,
3.09916720949489));
#89503=CARTESIAN_POINT('Ctrl Pts',(-2.15251844787821,-3.45652780504244,
0.363909007418006));
#89504=CARTESIAN_POINT('Ctrl Pts',(-1.99397524388836,-2.18420522486996,
-2.70357546164494));
#89505=CARTESIAN_POINT('Ctrl Pts',(-1.83543203989851,1.08217859867216,-3.30286993770192));
#89506=CARTESIAN_POINT('Ctrl Pts',(-1.67688883590866,3.36055724413934,-0.886863819989433));
#89507=CARTESIAN_POINT('Ctrl Pts',(-1.51834563191881,2.57105590561094,2.33879875418911));
#89508=CARTESIAN_POINT('Ctrl Pts',(-1.35980242792896,-0.565822421296421,
3.42927606449558));
#89509=CARTESIAN_POINT('Ctrl Pts',(-1.20125922393911,-3.18581540308026,
1.38907629785603));
#89510=CARTESIAN_POINT('Ctrl Pts',(-1.04271601994926,-2.89799076133817,
-1.91931309708123));
#89511=CARTESIAN_POINT('Ctrl Pts',(-0.884172815959405,0.0367029694702862,
-3.47539246609865));
#89512=CARTESIAN_POINT('Ctrl Pts',(-0.725629611969554,2.9356051105282,-1.85886066647829));
#89513=CARTESIAN_POINT('Ctrl Pts',(-0.567086407979703,3.15889968948113,
1.45505757261049));
#89514=CARTESIAN_POINT('Ctrl Pts',(-0.408543203989852,0.489518686277904,
3.43994448338358));
#89515=CARTESIAN_POINT('Ctrl Pts',(-0.302847734663285,-1.57463683943972,
2.67024552677286));
#89516=CARTESIAN_POINT('Ctrl Pts',(-0.250000000000001,-2.21686865784453,
1.93412961144453));
#89517=CARTESIAN_POINT('Ctrl Pts',(-15.6774893273369,1.59774743137963,-2.24059110187414));
#89518=CARTESIAN_POINT('Ctrl Pts',(-15.6246415926736,2.34174043430125,-1.71005569611084));
#89519=CARTESIAN_POINT('Ctrl Pts',(-15.5189461233471,3.24704165151874,0.141088316706114));
#89520=CARTESIAN_POINT('Ctrl Pts',(-15.3604029193572,1.64342946730058,2.80756887245516));
#89521=CARTESIAN_POINT('Ctrl Pts',(-15.2018597153674,-1.46194518251082,
2.90278464587397));
#89522=CARTESIAN_POINT('Ctrl Pts',(-15.0433165113775,-3.2319135759424,0.352017566381606));
#89523=CARTESIAN_POINT('Ctrl Pts',(-14.8847733073876,-2.0517465456428,-2.52222706796369));
#89524=CARTESIAN_POINT('Ctrl Pts',(-14.7262301033978,1.00173560633241,-3.09274211273195));
#89525=CARTESIAN_POINT('Ctrl Pts',(-14.567686899408,3.14059154487117,-0.840361361352499));
#89526=CARTESIAN_POINT('Ctrl Pts',(-14.4091436954181,2.41234843834475,2.17951574250036));
#89527=CARTESIAN_POINT('Ctrl Pts',(-14.2506004914283,-0.518240597791176,
3.20947960947053));
#89528=CARTESIAN_POINT('Ctrl Pts',(-14.0920572874384,-2.97569446991427,
1.30948063083483));
#89529=CARTESIAN_POINT('Ctrl Pts',(-13.9335140834486,-2.71654158940082,
-1.78603184185203));
#89530=CARTESIAN_POINT('Ctrl Pts',(-13.7749708794587,0.0226406050737881,
-3.25099125773301));
#89531=CARTESIAN_POINT('Ctrl Pts',(-13.6164276754689,2.74115120826787,-1.74801972486523));
#89532=CARTESIAN_POINT('Ctrl Pts',(-13.457884471479,2.95717087030058,1.35078587912609));
#89533=CARTESIAN_POINT('Ctrl Pts',(-13.2993412674892,0.473485991837778,
3.2164089277099));
#89534=CARTESIAN_POINT('Ctrl Pts',(-13.1407980634993,-2.44246036975315,
2.14566230974626));
#89535=CARTESIAN_POINT('Ctrl Pts',(-12.9822548595095,-3.12860004011352,
-0.883934798880462));
#89536=CARTESIAN_POINT('Ctrl Pts',(-12.8237116555196,-0.95853204547517,
-3.10655668202912));
#89537=CARTESIAN_POINT('Ctrl Pts',(-12.6651684515298,2.0866130816131,-2.49309537586272));
#89538=CARTESIAN_POINT('Ctrl Pts',(-12.5066252475399,3.22681671811049,0.396399368022285));
#89539=CARTESIAN_POINT('Ctrl Pts',(-12.3480820435501,1.42114734874778,2.92400730228622));
#89540=CARTESIAN_POINT('Ctrl Pts',(-12.1895388395602,-1.68193676069604,
2.78218750485857));
#89541=CARTESIAN_POINT('Ctrl Pts',(-12.0309956355704,-3.24952242010339,
0.100412138785985));
#89542=CARTESIAN_POINT('Ctrl Pts',(-11.8724524315805,-1.85050626070654,
-2.67303294483893));
#89543=CARTESIAN_POINT('Ctrl Pts',(-11.7139092275906,1.23790129924616,-3.00617346989206));
#89544=CARTESIAN_POINT('Ctrl Pts',(-11.5553660236008,3.19618579269568,-0.594873879252186));
#89545=CARTESIAN_POINT('Ctrl Pts',(-11.3968228196109,2.23656132747646,2.35950672407564));
#89546=CARTESIAN_POINT('Ctrl Pts',(-11.2382796156211,-0.764897610562968,
3.15981173484154));
#89547=CARTESIAN_POINT('Ctrl Pts',(-11.0797364116312,-3.06805496832172,
1.07541492687576));
#89548=CARTESIAN_POINT('Ctrl Pts',(-10.9211932076414,-2.57027844496784,
-1.99076549820343));
#89549=CARTESIAN_POINT('Ctrl Pts',(-10.7626500036515,0.273994492102586,
-3.23950699521412));
#89550=CARTESIAN_POINT('Ctrl Pts',(-10.6041067996617,2.8681283462518,-1.53079010418083));
#89551=CARTESIAN_POINT('Ctrl Pts',(-10.4455635956718,2.84384827260153,1.57543821080061));
#89552=CARTESIAN_POINT('Ctrl Pts',(-10.287020391682,0.223320393222169,3.24339429543067));
#89553=CARTESIAN_POINT('Ctrl Pts',(-10.1284771876921,-2.60108442518668,
1.95034314075622));
#89554=CARTESIAN_POINT('Ctrl Pts',(-9.9699339837023,-3.05086898115845,-1.12324396880199));
#89555=CARTESIAN_POINT('Ctrl Pts',(-9.81139077971244,-0.715409340307828,
-3.17138266840337));
#89556=CARTESIAN_POINT('Ctrl Pts',(-9.65284757572259,2.27317232110535,-2.32425604273857));
#89557=CARTESIAN_POINT('Ctrl Pts',(-9.49430437173274,3.18649606261496,0.644764605562371));
#89558=CARTESIAN_POINT('Ctrl Pts',(-9.33576116774289,1.19075693665695,3.02515726392043));
#89559=CARTESIAN_POINT('Ctrl Pts',(-9.17721796375304,-1.89206553117273,
2.64377884464544));
#89560=CARTESIAN_POINT('Ctrl Pts',(-9.01867475976319,-3.24755569687704,
-0.151197054628592));
#89561=CARTESIAN_POINT('Ctrl Pts',(-8.86013155577334,-1.63823953545058,
-2.80813991427307));
#89562=CARTESIAN_POINT('Ctrl Pts',(-8.70158835178349,1.46668236561888,-2.90143436803755));
#89563=CARTESIAN_POINT('Ctrl Pts',(-8.54304514779364,3.23261902259859,-0.345908670577368));
#89564=CARTESIAN_POINT('Ctrl Pts',(-8.38450194380379,2.04738556088874,2.52540905967947));
#89565=CARTESIAN_POINT('Ctrl Pts',(-8.22595873981393,-1.00697724965301,
3.09119319556836));
#89566=CARTESIAN_POINT('Ctrl Pts',(-8.06741553582409,-3.14203557407958,
0.834919759536982));
#89567=CARTESIAN_POINT('Ctrl Pts',(-7.90887233183423,-2.40862055436636,
-2.18358090730129));
#89568=CARTESIAN_POINT('Ctrl Pts',(-7.75032912784438,0.52370777916922,-3.20861476585839));
#89569=CARTESIAN_POINT('Ctrl Pts',(-7.59178592385453,2.97792510178615,-1.30439282495681));
#89570=CARTESIAN_POINT('Ctrl Pts',(-7.43324271986468,2.71349122713884,1.79065460485472));
#89571=CARTESIAN_POINT('Ctrl Pts',(-7.27469951587483,-0.0281829813913912,
3.25095128742446));
#89572=CARTESIAN_POINT('Ctrl Pts',(-7.11615631188498,-2.74412796790182,
1.74334169038255));
#89573=CARTESIAN_POINT('Ctrl Pts',(-6.95761310789512,-2.95486327640258,
-1.35582505192015));
#89574=CARTESIAN_POINT('Ctrl Pts',(-6.79906990390528,-0.468001328570138,
-3.21721203996619));
#89575=CARTESIAN_POINT('Ctrl Pts',(-6.64052669991542,2.44611527770728,-2.14149447858588));
#89576=CARTESIAN_POINT('Ctrl Pts',(-6.48198349592558,3.12708833568111,0.889267729367418));
#89577=CARTESIAN_POINT('Ctrl Pts',(-6.32344029193572,0.953233902308082,
3.10818655829041));
#89578=CARTESIAN_POINT('Ctrl Pts',(-6.16489708794588,-2.09086084981154,
2.48953398457857));
#89579=CARTESIAN_POINT('Ctrl Pts',(-6.00635388395601,-3.22613615269721,
-0.40190058212067));
#89580=CARTESIAN_POINT('Ctrl Pts',(-5.84781067996618,-1.41615977386316,
-2.9264261563444));
#89581=CARTESIAN_POINT('Ctrl Pts',(-5.68926747597632,1.68667802126876,-2.77931570826569));
#89582=CARTESIAN_POINT('Ctrl Pts',(-5.53072427198647,3.24968890162733,-0.0948714725370323));
#89583=CARTESIAN_POINT('Ctrl Pts',(-5.37218106799661,1.8459459781815,2.67618422371572));
#89584=CARTESIAN_POINT('Ctrl Pts',(-5.21363786400677,-1.24302510651458,
3.00405844453889));
#89585=CARTESIAN_POINT('Ctrl Pts',(-5.05509466001691,-3.19719542273467,
0.589423432337293));
#89586=CARTESIAN_POINT('Ctrl Pts',(-4.89655145602707,-2.23253505417579,
-2.36331669172368));
#89587=CARTESIAN_POINT('Ctrl Pts',(-4.73800825203721,0.770284062573315,
-3.15850297079745));
#89588=CARTESIAN_POINT('Ctrl Pts',(-4.57946504804737,3.06988412015183,-1.07018224762271));
#89589=CARTESIAN_POINT('Ctrl Pts',(-4.42092184405751,2.56688040007493,1.99514499829777));
#89590=CARTESIAN_POINT('Ctrl Pts',(-4.26237864006767,-0.279517539875905,
3.23903511844931));
#89591=CARTESIAN_POINT('Ctrl Pts',(-4.10383543607781,-2.87073421624609,
1.52589764317013));
#89592=CARTESIAN_POINT('Ctrl Pts',(-3.94529223208797,-2.841157973005,-1.58028475837061));
#89593=CARTESIAN_POINT('Ctrl Pts',(-3.78674902809811,-0.217789996971037,
-3.24377034846635));
#89594=CARTESIAN_POINT('Ctrl Pts',(-3.62820582410826,2.60440603702834,-1.94590538656487));
#89595=CARTESIAN_POINT('Ctrl Pts',(-3.46966262011841,3.04894937539763,1.12844414878998));
#89596=CARTESIAN_POINT('Ctrl Pts',(-3.31111941612856,0.710001026919591,
3.17259785239462));
#89597=CARTESIAN_POINT('Ctrl Pts',(-3.1525762121387,-2.27713197243884,2.32037684129191));
#89598=CARTESIAN_POINT('Ctrl Pts',(-2.99403300814886,-3.18539202003948,
-0.650196723716245));
#89599=CARTESIAN_POINT('Ctrl Pts',(-2.835489804159,-1.18559736491481,-3.02718315071573));
#89600=CARTESIAN_POINT('Ctrl Pts',(-2.67694660016915,1.89657074995108,-2.64054895726446));
#89601=CARTESIAN_POINT('Ctrl Pts',(-2.5184033961793,3.24729269387384,0.156733962599296));
#89602=CARTESIAN_POINT('Ctrl Pts',(-2.35986019218945,1.63345013172275,2.81092915502609));
#89603=CARTESIAN_POINT('Ctrl Pts',(-2.2013169881996,-1.47162903738377,2.89892926464846));
#89604=CARTESIAN_POINT('Ctrl Pts',(-2.04277378420975,-3.2332007054701,0.340396758213354));
#89605=CARTESIAN_POINT('Ctrl Pts',(-1.8842305802199,-2.04308319569681,-2.52889679554445));
#89606=CARTESIAN_POINT('Ctrl Pts',(-1.72568737623005,1.01225877702106,-3.08947071019517));
#89607=CARTESIAN_POINT('Ctrl Pts',(-1.5671441722402,3.1434308257765,-0.829563333546072));
#89608=CARTESIAN_POINT('Ctrl Pts',(-1.40860096825035,2.4049393601572,2.18768839960309));
#89609=CARTESIAN_POINT('Ctrl Pts',(-1.2500577642605,-0.529264497464093,
3.20770970648758));
#89610=CARTESIAN_POINT('Ctrl Pts',(-1.09151456027064,-2.97997909743711,
1.29932774144854));
#89611=CARTESIAN_POINT('Ctrl Pts',(-0.932971356280794,-2.71075087558549,
-1.79530581251172));
#89612=CARTESIAN_POINT('Ctrl Pts',(-0.774428152290943,0.0343315817136276,
-3.25084651620144));
#89613=CARTESIAN_POINT('Ctrl Pts',(-0.615884948301093,2.74593495255419,
-1.73875922810764));
#89614=CARTESIAN_POINT('Ctrl Pts',(-0.457341744311242,2.95480241461973,
1.36104595004296));
#89615=CARTESIAN_POINT('Ctrl Pts',(-0.29879854032139,0.457890765266106,
3.21768883624451));
#89616=CARTESIAN_POINT('Ctrl Pts',(-0.193103070994824,-1.47289917144852,
2.4977203158458));
#89617=CARTESIAN_POINT('Ctrl Pts',(-0.14025533633154,-2.07363623634716,
1.8091650282895));
#89618=CARTESIAN_POINT('Ctrl Pts',(-15.5677446636685,1.48738611075532,-2.0858265952159));
#89619=CARTESIAN_POINT('Ctrl Pts',(-15.5148969290052,2.17998923269507,-1.59193689882322));
#89620=CARTESIAN_POINT('Ctrl Pts',(-15.4092014596786,3.02275851530718,0.131342913489991));
#89621=CARTESIAN_POINT('Ctrl Pts',(-15.2506582556888,1.52991274819834,2.61364147039993));
#89622=CARTESIAN_POINT('Ctrl Pts',(-15.0921150516989,-1.3609641401674,2.70228039800918));
#89623=CARTESIAN_POINT('Ctrl Pts',(-14.9335718477091,-3.0086753823584,0.327702632277589));
#89624=CARTESIAN_POINT('Ctrl Pts',(-14.7750286437192,-1.91002611228993,
-2.34800910042517));
#89625=CARTESIAN_POINT('Ctrl Pts',(-14.6164854397294,0.932542652389897,
-2.87911691940785));
#89626=CARTESIAN_POINT('Ctrl Pts',(-14.4579422357395,2.92366124435786,-0.782315021975532));
#89627=CARTESIAN_POINT('Ctrl Pts',(-14.2993990317497,2.24572012511262,2.0289698984328));
#89628=CARTESIAN_POINT('Ctrl Pts',(-14.1408558277598,-0.482444128555762,
2.98779099882939));
#89629=CARTESIAN_POINT('Ctrl Pts',(-13.98231262377,-2.77015411664915,1.21903078318517));
#89630=CARTESIAN_POINT('Ctrl Pts',(-13.8237694197801,-2.52890172126577,
-1.66266513890972));
#89631=CARTESIAN_POINT('Ctrl Pts',(-13.6652262157903,0.0210767489682646,
-3.02643531009382));
#89632=CARTESIAN_POINT('Ctrl Pts',(-13.5066830118004,2.55181147819917,-1.62727863555117));
#89633=CARTESIAN_POINT('Ctrl Pts',(-13.3481398078105,2.75290999893348,1.25748295115812));
#89634=CARTESIAN_POINT('Ctrl Pts',(-13.1895966038207,0.440780860644896,
2.994241687783));
#89635=CARTESIAN_POINT('Ctrl Pts',(-13.0310533998308,-2.27375213296647,
1.99745482621866));
#89636=CARTESIAN_POINT('Ctrl Pts',(-12.872510195841,-2.91249802965114,-0.822878708390627));
#89637=CARTESIAN_POINT('Ctrl Pts',(-12.7139669918512,-0.892323294128247,
-2.89197727398902));
#89638=CARTESIAN_POINT('Ctrl Pts',(-12.5554237878613,1.94248430957061,-2.32088962374017));
#89639=CARTESIAN_POINT('Ctrl Pts',(-12.3968805838714,3.00393058014573,0.36901884661423));
#89640=CARTESIAN_POINT('Ctrl Pts',(-12.2383373798816,1.32298433804329,2.72203714038347));
#89641=CARTESIAN_POINT('Ctrl Pts',(-12.0797941758917,-1.56576022461067,
2.59001327179123));
#89642=CARTESIAN_POINT('Ctrl Pts',(-11.9212509719019,-3.02506792958903,
0.0934763640662002));
#89643=CARTESIAN_POINT('Ctrl Pts',(-11.7627077679121,-1.72268611169912,
-2.4883983523677));
#89644=CARTESIAN_POINT('Ctrl Pts',(-11.6041645639222,1.15239565579826,-2.79852783851926));
#89645=CARTESIAN_POINT('Ctrl Pts',(-11.4456213599324,2.97541542679498,-0.55378411398026));
#89646=CARTESIAN_POINT('Ctrl Pts',(-11.2870781559425,2.08207516970842,2.19652835028719));
#89647=CARTESIAN_POINT('Ctrl Pts',(-11.1285349519526,-0.712063784148243,
2.94155383679551));
#89648=CARTESIAN_POINT('Ctrl Pts',(-10.9699917479628,-2.8561349918586,1.00113271604682));
#89649=CARTESIAN_POINT('Ctrl Pts',(-10.811448543973,-2.39274142128822,-1.85325721302638));
#89650=CARTESIAN_POINT('Ctrl Pts',(-10.6529053399831,0.25506885129208,-3.01574430084707));
#89651=CARTESIAN_POINT('Ctrl Pts',(-10.4943621359933,2.67001791540662,-1.42505373172415));
#89652=CARTESIAN_POINT('Ctrl Pts',(-10.3358189320034,2.6474149409901,1.46661785653735));
#89653=CARTESIAN_POINT('Ctrl Pts',(-10.1772757280135,0.207894968005185,
3.01936309330255));
#89654=CARTESIAN_POINT('Ctrl Pts',(-10.0187325240237,-2.42141953787024,
1.81562695191615));
#89655=CARTESIAN_POINT('Ctrl Pts',(-9.86018932003382,-2.84013609359455,
-1.04565805919847));
#89656=CARTESIAN_POINT('Ctrl Pts',(-9.70164611604399,-0.665993820662647,
-2.95232553045019));
#89657=CARTESIAN_POINT('Ctrl Pts',(-9.54310291205412,2.11615732960122,-2.16371254173965));
#89658=CARTESIAN_POINT('Ctrl Pts',(-9.38455970806428,2.96639499612116,0.600228734645521));
#89659=CARTESIAN_POINT('Ctrl Pts',(-9.22601650407443,1.10850769907965,2.81620036360846));
#89660=CARTESIAN_POINT('Ctrl Pts',(-9.06747330008458,-1.76137475575546,
2.46116492269297));
#89661=CARTESIAN_POINT('Ctrl Pts',(-8.90893009609472,-3.02323705397431,
-0.140753409847466));
#89662=CARTESIAN_POINT('Ctrl Pts',(-8.75038689210489,-1.52508130087579,
-2.61417306860622));
#89663=CARTESIAN_POINT('Ctrl Pts',(-8.59184368811502,1.36537411149369,-2.70102338800866));
#89664=CARTESIAN_POINT('Ctrl Pts',(-8.43330048412517,3.00933210164812,-0.322015696662593));
#89665=CARTESIAN_POINT('Ctrl Pts',(-8.27475728013533,1.9059663541423,2.35097130220351));
#89666=CARTESIAN_POINT('Ctrl Pts',(-8.11621407614547,-0.937422239313005,
2.87767499070837));
#89667=CARTESIAN_POINT('Ctrl Pts',(-7.95767087215562,-2.92500553003527,
0.777249288304674));
#89668=CARTESIAN_POINT('Ctrl Pts',(-7.79912766816577,-2.24224973752628,
-2.03275426981972));
#89669=CARTESIAN_POINT('Ctrl Pts',(-7.64058446417592,0.487533674930223,
-2.98698589262086));
#89670=CARTESIAN_POINT('Ctrl Pts',(-7.48204126018606,2.77223067192896,-1.21429440768016));
#89671=CARTESIAN_POINT('Ctrl Pts',(-7.32349805619622,2.5260620568907,1.66696859347862));
#89672=CARTESIAN_POINT('Ctrl Pts',(-7.16495485220636,-0.0262362963369388,
3.0263981006572));
#89673=CARTESIAN_POINT('Ctrl Pts',(-7.00641164821652,-2.55458262390571,
1.62292372727311));
#89674=CARTESIAN_POINT('Ctrl Pts',(-6.84786844422666,-2.75076179763098,
-1.26217405281561));
#89675=CARTESIAN_POINT('Ctrl Pts',(-6.68932524023683,-0.435675039908627,
-2.99498932660997));
#89676=CARTESIAN_POINT('Ctrl Pts',(-6.53078203624695,2.27715458520661,-1.99357487995296));
#89677=CARTESIAN_POINT('Ctrl Pts',(-6.37223883225713,2.91109074328524,0.827843276995237));
#89678=CARTESIAN_POINT('Ctrl Pts',(-6.21369562826725,0.887391109976515,
2.89349456969276));
#89679=CARTESIAN_POINT('Ctrl Pts',(-6.05515242427742,-1.94643867137773,
2.31757422868649));
#89680=CARTESIAN_POINT('Ctrl Pts',(-5.89660922028755,-3.00329702347508,
-0.374140074964546));
#89681=CARTESIAN_POINT('Ctrl Pts',(-5.73806601629772,-1.31834127026923,
-2.72428891676528));
#89682=CARTESIAN_POINT('Ctrl Pts',(-5.57952281230786,1.57017399175861,-2.58733983900626));
#89683=CARTESIAN_POINT('Ctrl Pts',(-5.42097960831801,3.02522291172297,-0.0883184086464839));
#89684=CARTESIAN_POINT('Ctrl Pts',(-5.26243640432816,1.71844082188944,2.49133196273716));
#89685=CARTESIAN_POINT('Ctrl Pts',(-5.10389320033831,-1.15716554596711,
2.79655890446096));
#89686=CARTESIAN_POINT('Ctrl Pts',(-4.94534999634845,-2.97635531858733,
0.548710146168202));
#89687=CARTESIAN_POINT('Ctrl Pts',(-4.78680679235861,-2.07832700346642,
-2.20007515177209));
#89688=CARTESIAN_POINT('Ctrl Pts',(-4.62826358836875,0.717078177380293,
-2.94033547310223));
#89689=CARTESIAN_POINT('Ctrl Pts',(-4.4697203843789,2.85783779855579,-0.996261474015594));
#89690=CARTESIAN_POINT('Ctrl Pts',(-4.31117718038905,2.38957808978902,1.8573342076029));
#89691=CARTESIAN_POINT('Ctrl Pts',(-4.1526339763992,-0.260210405198368,
3.01530501805919));
#89692=CARTESIAN_POINT('Ctrl Pts',(-3.99409077240935,-2.67244378995965,
1.42049920801671));
#89693=CARTESIAN_POINT('Ctrl Pts',(-3.8355475684195,-2.64491046864669,-1.47112963818641));
#89694=CARTESIAN_POINT('Ctrl Pts',(-3.67700436442965,-0.202746573203009,
-3.01971317120046));
#89695=CARTESIAN_POINT('Ctrl Pts',(-3.5184611604398,2.42451171578371,-1.81149572703197));
#89696=CARTESIAN_POINT('Ctrl Pts',(-3.35991795644994,2.83834908089737,1.05049904678867));
#89697=CARTESIAN_POINT('Ctrl Pts',(-3.2013747524601,0.660959076085197,2.9534567779522));
#89698=CARTESIAN_POINT('Ctrl Pts',(-3.04283154847024,-2.11984347565985,
2.16010128864717));
#89699=CARTESIAN_POINT('Ctrl Pts',(-2.8842883444804,-2.96536721315609,-0.605285639720359));
#89700=CARTESIAN_POINT('Ctrl Pts',(-2.72574514049054,-1.1037045147991,-2.81808631618276));
#89701=CARTESIAN_POINT('Ctrl Pts',(-2.56720193650069,1.76556878524048,-2.45815813355006));
#89702=CARTESIAN_POINT('Ctrl Pts',(-2.40865873251084,3.02299221739605,0.145907866584748));
#89703=CARTESIAN_POINT('Ctrl Pts',(-2.25011552852099,1.52062271596827,2.61676964793666));
#89704=CARTESIAN_POINT('Ctrl Pts',(-2.09157232453114,-1.36997910145209,
2.69869131980204));
#89705=CARTESIAN_POINT('Ctrl Pts',(-1.93302912054129,-3.00987360589777,
0.316884509008699));
#89706=CARTESIAN_POINT('Ctrl Pts',(-1.77448591655144,-1.90196116652366,
-2.35421812944396));
#89707=CARTESIAN_POINT('Ctrl Pts',(-1.61594271256159,0.942338955369951,
-2.87607148268842));
#89708=CARTESIAN_POINT('Ctrl Pts',(-1.45739950857174,2.92630440741367,-0.772262847102708));
#89709=CARTESIAN_POINT('Ctrl Pts',(-1.29885630458189,2.23882281470346,2.03657804501707));
#89710=CARTESIAN_POINT('Ctrl Pts',(-1.14031310059203,-0.492706573631765,
2.98614334847957));
#89711=CARTESIAN_POINT('Ctrl Pts',(-0.981769896602184,-2.77414279179396,
1.20957918504104));
#89712=CARTESIAN_POINT('Ctrl Pts',(-0.823226692612332,-2.52351098983281,
-1.67129852794222));
#89713=CARTESIAN_POINT('Ctrl Pts',(-0.664683488622482,0.031960193956968,
-3.02630056630424));
#89714=CARTESIAN_POINT('Ctrl Pts',(-0.506140284632631,2.55626479458018,
-1.61865778973699));
#89715=CARTESIAN_POINT('Ctrl Pts',(-0.34759708064278,2.75070513975834,1.26703432747543));
#89716=CARTESIAN_POINT('Ctrl Pts',(-0.189053876652929,0.426262844254307,
2.99543318910543));
#89717=CARTESIAN_POINT('Ctrl Pts',(-0.0833584073263626,-1.37116150345731,
2.32519510491873));
#89718=CARTESIAN_POINT('Ctrl Pts',(-0.0305106726630785,-1.9304038148498,
1.68420044513446));
#89719=CARTESIAN_POINT('Ctrl Pts',(-15.458,1.37702479013101,-1.93106208855765));
#89720=CARTESIAN_POINT('Ctrl Pts',(-15.4051522653367,2.01823803108889,-1.47381810153559));
#89721=CARTESIAN_POINT('Ctrl Pts',(-15.2994567960102,2.79847537909562,0.121597510273868));
#89722=CARTESIAN_POINT('Ctrl Pts',(-15.1409135920203,1.4163960290961,2.41971406834469));
#89723=CARTESIAN_POINT('Ctrl Pts',(-14.9823703880305,-1.25998309782399,
2.5017761501444));
#89724=CARTESIAN_POINT('Ctrl Pts',(-14.8238271840406,-2.78543718877439,
0.30338769817357));
#89725=CARTESIAN_POINT('Ctrl Pts',(-14.6652839800508,-1.76830567893707,
-2.17379113288664));
#89726=CARTESIAN_POINT('Ctrl Pts',(-14.5067407760609,0.863349698447385,
-2.66549172608374));
#89727=CARTESIAN_POINT('Ctrl Pts',(-14.348197572071,2.70673094384455,-0.724268682598567));
#89728=CARTESIAN_POINT('Ctrl Pts',(-14.1896543680812,2.07909181188049,1.87842405436525));
#89729=CARTESIAN_POINT('Ctrl Pts',(-14.0311111640913,-0.44664765932035,
2.76610238818825));
#89730=CARTESIAN_POINT('Ctrl Pts',(-13.8725679601015,-2.56461376338402,
1.12858093553551));
#89731=CARTESIAN_POINT('Ctrl Pts',(-13.7140247561116,-2.34126185313073,
-1.53929843596741));
#89732=CARTESIAN_POINT('Ctrl Pts',(-13.5554815521218,0.0195128928627424,
-2.80187936245463));
#89733=CARTESIAN_POINT('Ctrl Pts',(-13.3969383481319,2.36247174813047,-1.50653754623712));
#89734=CARTESIAN_POINT('Ctrl Pts',(-13.2383951441421,2.54864912756637,1.16418002319016));
#89735=CARTESIAN_POINT('Ctrl Pts',(-13.0798519401522,0.408075729452012,
2.77207444785609));
#89736=CARTESIAN_POINT('Ctrl Pts',(-12.9213087361624,-2.10504389617979,
1.84924734269107));
#89737=CARTESIAN_POINT('Ctrl Pts',(-12.7627655321725,-2.69639601918876,
-0.761822617900794));
#89738=CARTESIAN_POINT('Ctrl Pts',(-12.6042223281827,-0.826114542781323,
-2.67739786594892));
#89739=CARTESIAN_POINT('Ctrl Pts',(-12.4456791241928,1.79835553752813,-2.1486838716176));
#89740=CARTESIAN_POINT('Ctrl Pts',(-12.287135920203,2.78104444218098,0.341638325206172));
#89741=CARTESIAN_POINT('Ctrl Pts',(-12.1285927162131,1.22482132733881,2.52006697848072));
#89742=CARTESIAN_POINT('Ctrl Pts',(-11.9700495122233,-1.4495836885253,2.39783903872389));
#89743=CARTESIAN_POINT('Ctrl Pts',(-11.8115063082334,-2.80061343907466,
0.0865405893464179));
#89744=CARTESIAN_POINT('Ctrl Pts',(-11.6529631042436,-1.5948659626917,-2.30376375989648));
#89745=CARTESIAN_POINT('Ctrl Pts',(-11.4944199002537,1.06689001235037,-2.59088220714646));
#89746=CARTESIAN_POINT('Ctrl Pts',(-11.3358766962639,2.75464506089428,-0.512694348708331));
#89747=CARTESIAN_POINT('Ctrl Pts',(-11.177333492274,1.92758901194037,2.03354997649873));
#89748=CARTESIAN_POINT('Ctrl Pts',(-11.0187902882842,-0.659229957733515,
2.7232959387495));
#89749=CARTESIAN_POINT('Ctrl Pts',(-10.8602470842943,-2.64421501539548,
0.926850505217873));
#89750=CARTESIAN_POINT('Ctrl Pts',(-10.7017038803045,-2.2152043976086,-1.71574892784934));
#89751=CARTESIAN_POINT('Ctrl Pts',(-10.5431606763146,0.236143210481572,
-2.79198160648));
#89752=CARTESIAN_POINT('Ctrl Pts',(-10.3846174723248,2.47190748456146,-1.31931735926746));
#89753=CARTESIAN_POINT('Ctrl Pts',(-10.2260742683349,2.45098160937866,1.35779750227409));
#89754=CARTESIAN_POINT('Ctrl Pts',(-10.0675310643451,0.192469542788204,
2.79533189117441));
#89755=CARTESIAN_POINT('Ctrl Pts',(-9.90898786035522,-2.24175465055382,
1.68091076307609));
#89756=CARTESIAN_POINT('Ctrl Pts',(-9.75044465636537,-2.62940320603065,
-0.968072149594963));
#89757=CARTESIAN_POINT('Ctrl Pts',(-9.59190145237552,-0.616578301017466,
-2.733268392497));
#89758=CARTESIAN_POINT('Ctrl Pts',(-9.43335824838566,1.95914233809709,-2.00316904074074));
#89759=CARTESIAN_POINT('Ctrl Pts',(-9.27481504439582,2.74629392962736,0.555692863728672));
#89760=CARTESIAN_POINT('Ctrl Pts',(-9.11627184040596,1.02625846150236,2.60724346329648));
#89761=CARTESIAN_POINT('Ctrl Pts',(-8.95772863641611,-1.63068398033819,
2.27855100074049));
#89762=CARTESIAN_POINT('Ctrl Pts',(-8.79918543242627,-2.79891841107159,
-0.130309765066336));
#89763=CARTESIAN_POINT('Ctrl Pts',(-8.64064222843641,-1.41192306630101,
-2.42020622293936));
#89764=CARTESIAN_POINT('Ctrl Pts',(-8.48209902444656,1.26406585736851,-2.50061240797977));
#89765=CARTESIAN_POINT('Ctrl Pts',(-8.32355582045671,2.78604518069765,-0.298122722747819));
#89766=CARTESIAN_POINT('Ctrl Pts',(-8.16501261646686,1.76454714739586,2.17653354472756));
#89767=CARTESIAN_POINT('Ctrl Pts',(-8.00646941247701,-0.867867228973001,
2.66415678584837));
#89768=CARTESIAN_POINT('Ctrl Pts',(-7.84792620848716,-2.70797548599095,
0.719578817072367));
#89769=CARTESIAN_POINT('Ctrl Pts',(-7.68938300449731,-2.0758789206862,-1.88192763233816));
#89770=CARTESIAN_POINT('Ctrl Pts',(-7.53083980050746,0.451359570691226,
-2.76535701938333));
#89771=CARTESIAN_POINT('Ctrl Pts',(-7.37229659651761,2.56653624207177,-1.1241959904035));
#89772=CARTESIAN_POINT('Ctrl Pts',(-7.21375339252775,2.33863288664257,1.54328258210251));
#89773=CARTESIAN_POINT('Ctrl Pts',(-7.05521018853791,-0.0242896112824878,
2.80184491388995));
#89774=CARTESIAN_POINT('Ctrl Pts',(-6.89666698454806,-2.36503727990959,
1.50250576416366));
#89775=CARTESIAN_POINT('Ctrl Pts',(-6.7381237805582,-2.54666031885938,-1.16852305371107));
#89776=CARTESIAN_POINT('Ctrl Pts',(-6.57958057656835,-0.403348751247113,
-2.77276661325373));
#89777=CARTESIAN_POINT('Ctrl Pts',(-6.42103737257851,2.10819389270592,-1.84565528132004));
#89778=CARTESIAN_POINT('Ctrl Pts',(-6.26249416858865,2.69509315088937,0.766418824623061));
#89779=CARTESIAN_POINT('Ctrl Pts',(-6.1039509645988,0.821548317644948,2.6788025810951));
#89780=CARTESIAN_POINT('Ctrl Pts',(-5.94540776060894,-1.80201649294392,
2.14561447279441));
#89781=CARTESIAN_POINT('Ctrl Pts',(-5.78686455661911,-2.78045789425295,
-0.346379567808426));
#89782=CARTESIAN_POINT('Ctrl Pts',(-5.62832135262924,-1.2205227666753,-2.52215167718616));
#89783=CARTESIAN_POINT('Ctrl Pts',(-5.4697781486394,1.45366996224847,-2.39536396974682));
#89784=CARTESIAN_POINT('Ctrl Pts',(-5.31123494464955,2.8007569218186,-0.0817653447559351));
#89785=CARTESIAN_POINT('Ctrl Pts',(-5.15269174065969,1.59093566559739,2.30647970175859));
#89786=CARTESIAN_POINT('Ctrl Pts',(-4.99414853666984,-1.07130598541964,
2.58905936438303));
#89787=CARTESIAN_POINT('Ctrl Pts',(-4.83560533268,-2.75551521443999,0.507996859999107));
#89788=CARTESIAN_POINT('Ctrl Pts',(-4.67706212869014,-1.92411895275705,
-2.0368336118205));
#89789=CARTESIAN_POINT('Ctrl Pts',(-4.51851892470029,0.663872292187274,
-2.72216797540702));
#89790=CARTESIAN_POINT('Ctrl Pts',(-4.35997572071044,2.64579147695974,-0.922340700408471));
#89791=CARTESIAN_POINT('Ctrl Pts',(-4.20143251672059,2.21227577950313,1.71952341690803));
#89792=CARTESIAN_POINT('Ctrl Pts',(-4.04288931273074,-0.24090327052083,
2.79157491766907));
#89793=CARTESIAN_POINT('Ctrl Pts',(-3.88434610874089,-2.47415336367322,
1.31510077286328));
#89794=CARTESIAN_POINT('Ctrl Pts',(-3.72580290475104,-2.44866296428837,
-1.36197451800221));
#89795=CARTESIAN_POINT('Ctrl Pts',(-3.56725970076119,-0.187703149434983,
-2.79565599393456));
#89796=CARTESIAN_POINT('Ctrl Pts',(-3.40871649677134,2.24461739453909,-1.67708606749907));
#89797=CARTESIAN_POINT('Ctrl Pts',(-3.25017329278149,2.6277487863971,0.972553944787357));
#89798=CARTESIAN_POINT('Ctrl Pts',(-3.09163008879163,0.611917125250802,
2.73431570350978));
#89799=CARTESIAN_POINT('Ctrl Pts',(-2.93308688480178,-1.96255497888086,
1.99982573600243));
#89800=CARTESIAN_POINT('Ctrl Pts',(-2.77454368081194,-2.7453424062727,-0.560374555724473));
#89801=CARTESIAN_POINT('Ctrl Pts',(-2.61600047682208,-1.02181166468338,
-2.60898948164979));
#89802=CARTESIAN_POINT('Ctrl Pts',(-2.45745727283223,1.63456682052989,-2.27576730983566));
#89803=CARTESIAN_POINT('Ctrl Pts',(-2.29891406884238,2.79869174091825,0.135081770570203));
#89804=CARTESIAN_POINT('Ctrl Pts',(-2.14037086485253,1.40779530021379,2.42261014084723));
#89805=CARTESIAN_POINT('Ctrl Pts',(-1.98182766086268,-1.26832916552041,
2.49845337495562));
#89806=CARTESIAN_POINT('Ctrl Pts',(-1.82328445687283,-2.78654650632543,
0.293372259804046));
#89807=CARTESIAN_POINT('Ctrl Pts',(-1.66474125288298,-1.76083913735052,
-2.17953946334347));
#89808=CARTESIAN_POINT('Ctrl Pts',(-1.50619804889313,0.872419133718849,
-2.66267225518167));
#89809=CARTESIAN_POINT('Ctrl Pts',(-1.34765484490327,2.70917798905082,-0.714962360659344));
#89810=CARTESIAN_POINT('Ctrl Pts',(-1.18911164091343,2.07270626924971,1.88546769043105));
#89811=CARTESIAN_POINT('Ctrl Pts',(-1.03056843692357,-0.456148649799437,
2.76457699047157));
#89812=CARTESIAN_POINT('Ctrl Pts',(-0.872025232933722,-2.56830648615081,
1.11983062863355));
#89813=CARTESIAN_POINT('Ctrl Pts',(-0.713482028943871,-2.33627110408012,
-1.54729124337272));
#89814=CARTESIAN_POINT('Ctrl Pts',(-0.55493882495402,0.029588806200308,
-2.80175461640703));
#89815=CARTESIAN_POINT('Ctrl Pts',(-0.396395620964169,2.36659463660617,
-1.49855635136634));
#89816=CARTESIAN_POINT('Ctrl Pts',(-0.237852416974319,2.54660786489694,
1.17302270490791));
#89817=CARTESIAN_POINT('Ctrl Pts',(-0.0793092129844672,0.394634923242509,
2.77317754196636));
#89818=CARTESIAN_POINT('Ctrl Pts',(0.0263862563420988,-1.26942383546611,
2.15266989399166));
#89819=CARTESIAN_POINT('Ctrl Pts',(0.079233991005383,-1.78717139335243,
1.55923586197943));
#89820=CARTESIAN_POINT('Origin',(-0.25,0.,0.));
#89821=CARTESIAN_POINT('Origin',(-0.25,0.,0.));
#89822=CARTESIAN_POINT('',(0.,-3.90907258287835E-16,3.192));
#89823=CARTESIAN_POINT('Origin',(-0.25,-3.90907258287835E-16,3.192));
#89824=CARTESIAN_POINT('Origin',(0.,0.,0.));
#89825=CARTESIAN_POINT('Origin',(-7.7,0.,0.));
#89826=CARTESIAN_POINT('Origin',(0.,5.,0.));
#89827=CARTESIAN_POINT('',(0.,-5.,-6.12323399573677E-16));
#89828=CARTESIAN_POINT('Origin',(0.,0.,0.));
#89829=CARTESIAN_POINT('Origin',(0.3,4.70738105939836,-0.830038289247927));
#89830=CARTESIAN_POINT('',(0.3,4.90726077320404,-0.958536229765423));
#89831=CARTESIAN_POINT('',(5.4,4.90726077320404,-0.958536229765423));
#89832=CARTESIAN_POINT('',(2.7,4.90726077320404,-0.958536229765423));
#89833=CARTESIAN_POINT('',(0.3,4.70738105939836,-0.830038289247927));
#89834=CARTESIAN_POINT('',(0.3,5.0904382363941,-1.07629668839819));
#89835=CARTESIAN_POINT('',(5.4,4.70738105939836,-0.830038289247927));
#89836=CARTESIAN_POINT('',(0.3,4.70738105939836,-0.830038289247927));
#89837=CARTESIAN_POINT('',(5.4,5.0904382363941,-1.07629668839819));
#89838=CARTESIAN_POINT('Origin',(5.4,4.91419068753092,-0.866504406557983));
#89839=CARTESIAN_POINT('',(5.4,4.9391554355392,-0.777652611121163));
#89840=CARTESIAN_POINT('Origin',(5.4,0.,0.));
#89841=CARTESIAN_POINT('',(5.4,4.70738105939836,-0.830038289247927));
#89842=CARTESIAN_POINT('Origin',(0.3,5.15156239493286,-0.72964435933789));
#89843=CARTESIAN_POINT('',(0.3,4.9391554355392,-0.777652611121163));
#89844=CARTESIAN_POINT('',(2.7,4.9391554355392,-0.777652611121163));
#89845=CARTESIAN_POINT('',(0.3,4.70738105939836,-0.830038289247927));
#89846=CARTESIAN_POINT('Origin',(0.3,4.91419068753092,-0.866504406557983));
#89847=CARTESIAN_POINT('Origin',(0.3,0.,0.));
#89848=CARTESIAN_POINT('Origin',(0.3,4.49173072735664,-1.6348562850967));
#89849=CARTESIAN_POINT('',(0.3,4.66626038597752,-1.79611080121938));
#89850=CARTESIAN_POINT('',(5.4,4.66626038597752,-1.79611080121938));
#89851=CARTESIAN_POINT('',(2.7,4.66626038597752,-1.79611080121938));
#89852=CARTESIAN_POINT('',(0.3,4.49173072735664,-1.6348562850967));
#89853=CARTESIAN_POINT('',(0.3,4.8262060828614,-1.9438906465518));
#89854=CARTESIAN_POINT('',(5.4,4.49173072735664,-1.6348562850967));
#89855=CARTESIAN_POINT('',(0.3,4.49173072735664,-1.6348562850967));
#89856=CARTESIAN_POINT('',(5.4,4.8262060828614,-1.9438906465518));
#89857=CARTESIAN_POINT('Origin',(5.4,4.68906617772168,-1.70668051519509));
#89858=CARTESIAN_POINT('',(5.4,4.72908060747227,-1.62351366117741));
#89859=CARTESIAN_POINT('Origin',(5.4,0.,0.));
#89860=CARTESIAN_POINT('',(5.4,4.49173072735664,-1.6348562850967));
#89861=CARTESIAN_POINT('Origin',(0.3,4.94659717331204,-1.61311884403516));
#89862=CARTESIAN_POINT('',(0.3,4.72908060747227,-1.62351366117741));
#89863=CARTESIAN_POINT('',(2.7,4.72908060747227,-1.62351366117741));
#89864=CARTESIAN_POINT('',(0.3,4.49173072735664,-1.6348562850967));
#89865=CARTESIAN_POINT('Origin',(0.3,4.68906617772168,-1.70668051519509));
#89866=CARTESIAN_POINT('Origin',(0.3,0.,0.));
#89867=CARTESIAN_POINT('Origin',(0.3,4.13960143008962,-2.39));
#89868=CARTESIAN_POINT('',(0.3,4.28347803816477,-2.57911145485419));
#89869=CARTESIAN_POINT('',(5.4,4.28347803816477,-2.57911145485419));
#89870=CARTESIAN_POINT('',(2.7,4.28347803816477,-2.57911145485419));
#89871=CARTESIAN_POINT('',(0.3,4.13960143008962,-2.39));
#89872=CARTESIAN_POINT('',(0.3,4.41533209967908,-2.75242047106606));
#89873=CARTESIAN_POINT('',(5.4,4.13960143008962,-2.39));
#89874=CARTESIAN_POINT('',(0.3,4.13960143008962,-2.39));
#89875=CARTESIAN_POINT('',(5.4,4.41533209967908,-2.75242047106606));
#89876=CARTESIAN_POINT('Origin',(5.4,4.32146676488435,-2.495));
#89877=CARTESIAN_POINT('',(5.4,4.37531505817755,-2.42004507017633));
#89878=CARTESIAN_POINT('Origin',(5.4,0.,0.));
#89879=CARTESIAN_POINT('',(5.4,4.13960143008962,-2.39));
#89880=CARTESIAN_POINT('Origin',(0.3,4.59133209967908,-2.44757952893394));
#89881=CARTESIAN_POINT('',(0.3,4.37531505817755,-2.42004507017633));
#89882=CARTESIAN_POINT('',(2.7,4.37531505817755,-2.42004507017633));
#89883=CARTESIAN_POINT('',(0.3,4.13960143008962,-2.39));
#89884=CARTESIAN_POINT('Origin',(0.3,4.32146676488435,-2.495));
#89885=CARTESIAN_POINT('Origin',(0.3,0.,0.));
#89886=CARTESIAN_POINT('Origin',(0.3,3.66169243810871,-3.07252477430166));
#89887=CARTESIAN_POINT('',(0.3,3.77054437770685,-3.28374711202663));
#89888=CARTESIAN_POINT('',(5.4,3.77054437770685,-3.28374711202663));
#89889=CARTESIAN_POINT('',(2.7,3.77054437770685,-3.28374711202663));
#89890=CARTESIAN_POINT('',(0.3,3.66169243810871,-3.07252477430166));
#89891=CARTESIAN_POINT('',(0.3,3.87030048491385,-3.47731939235895));
#89892=CARTESIAN_POINT('',(5.4,3.66169243810871,-3.07252477430166));
#89893=CARTESIAN_POINT('',(0.3,3.66169243810871,-3.07252477430166));
#89894=CARTESIAN_POINT('',(5.4,3.87030048491385,-3.47731939235895));
#89895=CARTESIAN_POINT('Origin',(5.4,3.8225617711637,-3.20751017233583));
#89896=CARTESIAN_POINT('',(5.4,3.88860777485636,-3.14304463431983));
#89897=CARTESIAN_POINT('Origin',(5.4,0.,0.));
#89898=CARTESIAN_POINT('',(5.4,3.66169243810871,-3.07252477430166));
#89899=CARTESIAN_POINT('Origin',(0.3,4.09656172352352,-3.20767174838107));
#89900=CARTESIAN_POINT('',(0.3,3.88860777485636,-3.14304463431983));
#89901=CARTESIAN_POINT('',(2.7,3.88860777485636,-3.14304463431983));
#89902=CARTESIAN_POINT('',(0.3,3.66169243810871,-3.07252477430166));
#89903=CARTESIAN_POINT('Origin',(0.3,3.8225617711637,-3.20751017233583));
#89904=CARTESIAN_POINT('Origin',(0.3,0.,0.));
#89905=CARTESIAN_POINT('Origin',(0.3,3.07252477430166,-3.66169243810872));
#89906=CARTESIAN_POINT('',(0.3,3.14304463431983,-3.88860777485636));
#89907=CARTESIAN_POINT('',(5.4,3.14304463431983,-3.88860777485636));
#89908=CARTESIAN_POINT('',(2.7,3.14304463431983,-3.88860777485636));
#89909=CARTESIAN_POINT('',(0.3,3.07252477430166,-3.66169243810872));
#89910=CARTESIAN_POINT('',(0.3,3.20767174838106,-4.09656172352352));
#89911=CARTESIAN_POINT('',(5.4,3.07252477430166,-3.66169243810872));
#89912=CARTESIAN_POINT('',(0.3,3.07252477430166,-3.66169243810872));
#89913=CARTESIAN_POINT('',(5.4,3.20767174838106,-4.09656172352352));
#89914=CARTESIAN_POINT('Origin',(5.4,3.20751017233583,-3.8225617711637));
#89915=CARTESIAN_POINT('',(5.4,3.28374711202663,-3.77054437770685));
#89916=CARTESIAN_POINT('Origin',(5.4,0.,0.));
#89917=CARTESIAN_POINT('',(5.4,3.07252477430166,-3.66169243810872));
#89918=CARTESIAN_POINT('Origin',(0.3,3.47731939235894,-3.87030048491386));
#89919=CARTESIAN_POINT('',(0.3,3.28374711202663,-3.77054437770685));
#89920=CARTESIAN_POINT('',(2.7,3.28374711202663,-3.77054437770685));
#89921=CARTESIAN_POINT('',(0.3,3.07252477430166,-3.66169243810872));
#89922=CARTESIAN_POINT('Origin',(0.3,3.20751017233583,-3.8225617711637));
#89923=CARTESIAN_POINT('Origin',(0.3,0.,0.));
#89924=CARTESIAN_POINT('Origin',(0.3,2.39,-4.13960143008962));
#89925=CARTESIAN_POINT('',(0.3,2.42004507017632,-4.37531505817756));
#89926=CARTESIAN_POINT('',(5.4,2.42004507017632,-4.37531505817756));
#89927=CARTESIAN_POINT('',(2.7,2.42004507017632,-4.37531505817756));
#89928=CARTESIAN_POINT('',(0.3,2.39,-4.13960143008962));
#89929=CARTESIAN_POINT('',(0.3,2.44757952893394,-4.59133209967908));
#89930=CARTESIAN_POINT('',(5.4,2.39,-4.13960143008962));
#89931=CARTESIAN_POINT('',(0.3,2.39,-4.13960143008962));
#89932=CARTESIAN_POINT('',(5.4,2.44757952893394,-4.59133209967908));
#89933=CARTESIAN_POINT('Origin',(5.4,2.495,-4.32146676488435));
#89934=CARTESIAN_POINT('',(5.4,2.57911145485419,-4.28347803816477));
#89935=CARTESIAN_POINT('Origin',(5.4,0.,0.));
#89936=CARTESIAN_POINT('',(5.4,2.39,-4.13960143008962));
#89937=CARTESIAN_POINT('Origin',(0.3,2.75242047106606,-4.41533209967908));
#89938=CARTESIAN_POINT('',(0.3,2.57911145485419,-4.28347803816477));
#89939=CARTESIAN_POINT('',(2.7,2.57911145485419,-4.28347803816477));
#89940=CARTESIAN_POINT('',(0.3,2.39,-4.13960143008962));
#89941=CARTESIAN_POINT('Origin',(0.3,2.495,-4.32146676488435));
#89942=CARTESIAN_POINT('Origin',(0.3,0.,0.));
#89943=CARTESIAN_POINT('Origin',(0.3,1.63485628509669,-4.49173072735664));
#89944=CARTESIAN_POINT('',(0.3,1.6235136611774,-4.72908060747227));
#89945=CARTESIAN_POINT('',(5.4,1.6235136611774,-4.72908060747227));
#89946=CARTESIAN_POINT('',(2.7,1.6235136611774,-4.72908060747228));
#89947=CARTESIAN_POINT('',(0.3,1.63485628509669,-4.49173072735664));
#89948=CARTESIAN_POINT('',(0.3,1.61311884403515,-4.94659717331204));
#89949=CARTESIAN_POINT('',(5.4,1.63485628509669,-4.49173072735664));
#89950=CARTESIAN_POINT('',(0.3,1.63485628509669,-4.49173072735664));
#89951=CARTESIAN_POINT('',(5.4,1.61311884403515,-4.94659717331204));
#89952=CARTESIAN_POINT('Origin',(5.4,1.70668051519508,-4.68906617772168));
#89953=CARTESIAN_POINT('',(5.4,1.79611080121937,-4.66626038597752));
#89954=CARTESIAN_POINT('Origin',(5.4,0.,0.));
#89955=CARTESIAN_POINT('',(5.4,1.63485628509669,-4.49173072735664));
#89956=CARTESIAN_POINT('Origin',(0.3,1.94389064655179,-4.82620608286141));
#89957=CARTESIAN_POINT('',(0.3,1.79611080121937,-4.66626038597752));
#89958=CARTESIAN_POINT('',(2.7,1.79611080121937,-4.66626038597752));
#89959=CARTESIAN_POINT('',(0.3,1.63485628509669,-4.49173072735664));
#89960=CARTESIAN_POINT('Origin',(0.3,1.70668051519508,-4.68906617772168));
#89961=CARTESIAN_POINT('Origin',(0.3,0.,0.));
#89962=CARTESIAN_POINT('Origin',(0.3,0.830038289247925,-4.70738105939836));
#89963=CARTESIAN_POINT('',(0.3,0.777652611121161,-4.9391554355392));
#89964=CARTESIAN_POINT('',(5.4,0.777652611121161,-4.9391554355392));
#89965=CARTESIAN_POINT('',(2.7,0.777652611121161,-4.9391554355392));
#89966=CARTESIAN_POINT('',(0.3,0.830038289247925,-4.70738105939836));
#89967=CARTESIAN_POINT('',(0.3,0.729644359337887,-5.15156239493286));
#89968=CARTESIAN_POINT('',(5.4,0.830038289247925,-4.70738105939836));
#89969=CARTESIAN_POINT('',(0.3,0.830038289247925,-4.70738105939836));
#89970=CARTESIAN_POINT('',(5.4,0.729644359337887,-5.15156239493286));
#89971=CARTESIAN_POINT('Origin',(5.4,0.866504406557981,-4.91419068753092));
#89972=CARTESIAN_POINT('',(5.4,0.958536229765421,-4.90726077320404));
#89973=CARTESIAN_POINT('Origin',(5.4,0.,0.));
#89974=CARTESIAN_POINT('',(5.4,0.830038289247925,-4.70738105939836));
#89975=CARTESIAN_POINT('Origin',(0.3,1.07629668839818,-5.0904382363941));
#89976=CARTESIAN_POINT('',(0.3,0.958536229765421,-4.90726077320404));
#89977=CARTESIAN_POINT('',(2.7,0.958536229765421,-4.90726077320404));
#89978=CARTESIAN_POINT('',(0.3,0.830038289247925,-4.70738105939836));
#89979=CARTESIAN_POINT('Origin',(0.3,0.866504406557981,-4.91419068753092));
#89980=CARTESIAN_POINT('Origin',(0.3,0.,0.));
#89981=CARTESIAN_POINT('Origin',(0.3,-8.78071754988652E-16,-4.78));
#89982=CARTESIAN_POINT('',(0.3,-0.0918370200127877,-4.99915652503051));
#89983=CARTESIAN_POINT('',(5.4,-0.0918370200127877,-4.99915652503051));
#89984=CARTESIAN_POINT('',(2.7,-0.0918370200127877,-4.99915652503051));
#89985=CARTESIAN_POINT('',(0.3,-8.78071754988652E-16,-4.78));
#89986=CARTESIAN_POINT('',(0.3,-0.176000000000001,-5.2));
#89987=CARTESIAN_POINT('',(5.4,-8.78071754988652E-16,-4.78));
#89988=CARTESIAN_POINT('',(0.3,-8.78071754988652E-16,-4.78));
#89989=CARTESIAN_POINT('',(5.4,-0.176000000000001,-5.2));
#89990=CARTESIAN_POINT('Origin',(5.4,-9.16648129161794E-16,-4.99));
#89991=CARTESIAN_POINT('',(5.4,0.091837020012786,-4.99915652503051));
#89992=CARTESIAN_POINT('Origin',(5.4,0.,0.));
#89993=CARTESIAN_POINT('',(5.4,-8.78071754988652E-16,-4.78));
#89994=CARTESIAN_POINT('Origin',(0.3,0.175999999999999,-5.2));
#89995=CARTESIAN_POINT('',(0.3,0.091837020012786,-4.99915652503051));
#89996=CARTESIAN_POINT('',(2.7,0.0918370200127863,-4.99915652503051));
#89997=CARTESIAN_POINT('',(0.3,-8.78071754988652E-16,-4.78));
#89998=CARTESIAN_POINT('Origin',(0.3,-9.16648129161794E-16,-4.99));
#89999=CARTESIAN_POINT('Origin',(0.3,0.,0.));
#90000=CARTESIAN_POINT('Origin',(0.3,-0.830038289247927,-4.70738105939836));
#90001=CARTESIAN_POINT('',(0.3,-0.958536229765423,-4.90726077320404));
#90002=CARTESIAN_POINT('',(5.4,-0.958536229765423,-4.90726077320404));
#90003=CARTESIAN_POINT('',(2.7,-0.958536229765423,-4.90726077320404));
#90004=CARTESIAN_POINT('',(0.3,-0.830038289247927,-4.70738105939836));
#90005=CARTESIAN_POINT('',(0.3,-1.07629668839819,-5.0904382363941));
#90006=CARTESIAN_POINT('',(5.4,-0.830038289247927,-4.70738105939836));
#90007=CARTESIAN_POINT('',(0.3,-0.830038289247927,-4.70738105939836));
#90008=CARTESIAN_POINT('',(5.4,-1.07629668839819,-5.0904382363941));
#90009=CARTESIAN_POINT('Origin',(5.4,-0.866504406557982,-4.91419068753092));
#90010=CARTESIAN_POINT('',(5.4,-0.777652611121163,-4.9391554355392));
#90011=CARTESIAN_POINT('Origin',(5.4,0.,0.));
#90012=CARTESIAN_POINT('',(5.4,-0.830038289247927,-4.70738105939836));
#90013=CARTESIAN_POINT('Origin',(0.3,-0.729644359337889,-5.15156239493286));
#90014=CARTESIAN_POINT('',(0.3,-0.777652611121163,-4.9391554355392));
#90015=CARTESIAN_POINT('',(2.7,-0.777652611121163,-4.9391554355392));
#90016=CARTESIAN_POINT('',(0.3,-0.830038289247927,-4.70738105939836));
#90017=CARTESIAN_POINT('Origin',(0.3,-0.866504406557982,-4.91419068753092));
#90018=CARTESIAN_POINT('Origin',(0.3,0.,0.));
#90019=CARTESIAN_POINT('Origin',(0.3,-1.6348562850967,-4.49173072735664));
#90020=CARTESIAN_POINT('',(0.3,-1.79611080121938,-4.66626038597752));
#90021=CARTESIAN_POINT('',(5.4,-1.79611080121938,-4.66626038597752));
#90022=CARTESIAN_POINT('',(2.7,-1.79611080121938,-4.66626038597752));
#90023=CARTESIAN_POINT('',(0.3,-1.6348562850967,-4.49173072735664));
#90024=CARTESIAN_POINT('',(0.3,-1.9438906465518,-4.8262060828614));
#90025=CARTESIAN_POINT('',(5.4,-1.6348562850967,-4.49173072735664));
#90026=CARTESIAN_POINT('',(0.3,-1.6348562850967,-4.49173072735664));
#90027=CARTESIAN_POINT('',(5.4,-1.9438906465518,-4.8262060828614));
#90028=CARTESIAN_POINT('Origin',(5.4,-1.70668051519509,-4.68906617772168));
#90029=CARTESIAN_POINT('',(5.4,-1.62351366117741,-4.72908060747227));
#90030=CARTESIAN_POINT('Origin',(5.4,0.,0.));
#90031=CARTESIAN_POINT('',(5.4,-1.6348562850967,-4.49173072735664));
#90032=CARTESIAN_POINT('Origin',(0.3,-1.61311884403516,-4.94659717331204));
#90033=CARTESIAN_POINT('',(0.3,-1.62351366117741,-4.72908060747227));
#90034=CARTESIAN_POINT('',(2.7,-1.62351366117741,-4.72908060747227));
#90035=CARTESIAN_POINT('',(0.3,-1.6348562850967,-4.49173072735664));
#90036=CARTESIAN_POINT('Origin',(0.3,-1.70668051519509,-4.68906617772168));
#90037=CARTESIAN_POINT('Origin',(0.3,0.,0.));
#90038=CARTESIAN_POINT('Origin',(0.3,-2.39,-4.13960143008962));
#90039=CARTESIAN_POINT('',(0.3,-2.57911145485419,-4.28347803816477));
#90040=CARTESIAN_POINT('',(5.4,-2.57911145485419,-4.28347803816477));
#90041=CARTESIAN_POINT('',(2.7,-2.57911145485419,-4.28347803816477));
#90042=CARTESIAN_POINT('',(0.3,-2.39,-4.13960143008962));
#90043=CARTESIAN_POINT('',(0.3,-2.75242047106606,-4.41533209967908));
#90044=CARTESIAN_POINT('',(5.4,-2.39,-4.13960143008962));
#90045=CARTESIAN_POINT('',(0.3,-2.39,-4.13960143008962));
#90046=CARTESIAN_POINT('',(5.4,-2.75242047106606,-4.41533209967908));
#90047=CARTESIAN_POINT('Origin',(5.4,-2.495,-4.32146676488435));
#90048=CARTESIAN_POINT('',(5.4,-2.42004507017633,-4.37531505817755));
#90049=CARTESIAN_POINT('Origin',(5.4,0.,0.));
#90050=CARTESIAN_POINT('',(5.4,-2.39,-4.13960143008962));
#90051=CARTESIAN_POINT('Origin',(0.3,-2.44757952893394,-4.59133209967908));
#90052=CARTESIAN_POINT('',(0.3,-2.42004507017633,-4.37531505817755));
#90053=CARTESIAN_POINT('',(2.7,-2.42004507017633,-4.37531505817755));
#90054=CARTESIAN_POINT('',(0.3,-2.39,-4.13960143008962));
#90055=CARTESIAN_POINT('Origin',(0.3,-2.495,-4.32146676488435));
#90056=CARTESIAN_POINT('Origin',(0.3,0.,0.));
#90057=CARTESIAN_POINT('Origin',(0.3,-3.07252477430166,-3.66169243810871));
#90058=CARTESIAN_POINT('',(0.3,-3.28374711202663,-3.77054437770685));
#90059=CARTESIAN_POINT('',(5.4,-3.28374711202663,-3.77054437770685));
#90060=CARTESIAN_POINT('',(2.7,-3.28374711202663,-3.77054437770685));
#90061=CARTESIAN_POINT('',(0.3,-3.07252477430166,-3.66169243810871));
#90062=CARTESIAN_POINT('',(0.3,-3.47731939235895,-3.87030048491385));
#90063=CARTESIAN_POINT('',(5.4,-3.07252477430166,-3.66169243810871));
#90064=CARTESIAN_POINT('',(0.3,-3.07252477430166,-3.66169243810871));
#90065=CARTESIAN_POINT('',(5.4,-3.47731939235895,-3.87030048491385));
#90066=CARTESIAN_POINT('Origin',(5.4,-3.20751017233583,-3.8225617711637));
#90067=CARTESIAN_POINT('',(5.4,-3.14304463431983,-3.88860777485636));
#90068=CARTESIAN_POINT('Origin',(5.4,0.,0.));
#90069=CARTESIAN_POINT('',(5.4,-3.07252477430166,-3.66169243810871));
#90070=CARTESIAN_POINT('Origin',(0.3,-3.20767174838107,-4.09656172352352));
#90071=CARTESIAN_POINT('',(0.3,-3.14304463431983,-3.88860777485636));
#90072=CARTESIAN_POINT('',(2.7,-3.14304463431983,-3.88860777485636));
#90073=CARTESIAN_POINT('',(0.3,-3.07252477430166,-3.66169243810871));
#90074=CARTESIAN_POINT('Origin',(0.3,-3.20751017233583,-3.8225617711637));
#90075=CARTESIAN_POINT('Origin',(0.3,0.,0.));
#90076=CARTESIAN_POINT('Origin',(0.3,-3.66169243810872,-3.07252477430166));
#90077=CARTESIAN_POINT('',(0.3,-3.88860777485636,-3.14304463431983));
#90078=CARTESIAN_POINT('',(5.4,-3.88860777485636,-3.14304463431983));
#90079=CARTESIAN_POINT('',(2.7,-3.88860777485636,-3.14304463431983));
#90080=CARTESIAN_POINT('',(0.3,-3.66169243810872,-3.07252477430166));
#90081=CARTESIAN_POINT('',(0.3,-4.09656172352352,-3.20767174838106));
#90082=CARTESIAN_POINT('',(5.4,-3.66169243810872,-3.07252477430166));
#90083=CARTESIAN_POINT('',(0.3,-3.66169243810872,-3.07252477430166));
#90084=CARTESIAN_POINT('',(5.4,-4.09656172352352,-3.20767174838106));
#90085=CARTESIAN_POINT('Origin',(5.4,-3.8225617711637,-3.20751017233583));
#90086=CARTESIAN_POINT('',(5.4,-3.77054437770685,-3.28374711202663));
#90087=CARTESIAN_POINT('Origin',(5.4,0.,0.));
#90088=CARTESIAN_POINT('',(5.4,-3.66169243810872,-3.07252477430166));
#90089=CARTESIAN_POINT('Origin',(0.3,-3.87030048491386,-3.47731939235894));
#90090=CARTESIAN_POINT('',(0.3,-3.77054437770685,-3.28374711202663));
#90091=CARTESIAN_POINT('',(2.7,-3.77054437770685,-3.28374711202663));
#90092=CARTESIAN_POINT('',(0.3,-3.66169243810872,-3.07252477430166));
#90093=CARTESIAN_POINT('Origin',(0.3,-3.8225617711637,-3.20751017233583));
#90094=CARTESIAN_POINT('Origin',(0.3,0.,0.));
#90095=CARTESIAN_POINT('Origin',(0.3,-4.13960143008962,-2.39));
#90096=CARTESIAN_POINT('',(0.3,-4.37531505817756,-2.42004507017632));
#90097=CARTESIAN_POINT('',(5.4,-4.37531505817756,-2.42004507017632));
#90098=CARTESIAN_POINT('',(2.7,-4.37531505817756,-2.42004507017632));
#90099=CARTESIAN_POINT('',(0.3,-4.13960143008962,-2.39));
#90100=CARTESIAN_POINT('',(0.3,-4.59133209967908,-2.44757952893394));
#90101=CARTESIAN_POINT('',(5.4,-4.13960143008962,-2.39));
#90102=CARTESIAN_POINT('',(0.3,-4.13960143008962,-2.39));
#90103=CARTESIAN_POINT('',(5.4,-4.59133209967908,-2.44757952893394));
#90104=CARTESIAN_POINT('Origin',(5.4,-4.32146676488435,-2.495));
#90105=CARTESIAN_POINT('',(5.4,-4.28347803816477,-2.57911145485419));
#90106=CARTESIAN_POINT('Origin',(5.4,0.,0.));
#90107=CARTESIAN_POINT('',(5.4,-4.13960143008962,-2.39));
#90108=CARTESIAN_POINT('Origin',(0.3,-4.41533209967908,-2.75242047106606));
#90109=CARTESIAN_POINT('',(0.3,-4.28347803816477,-2.57911145485419));
#90110=CARTESIAN_POINT('',(2.7,-4.28347803816477,-2.57911145485419));
#90111=CARTESIAN_POINT('',(0.3,-4.13960143008962,-2.39));
#90112=CARTESIAN_POINT('Origin',(0.3,-4.32146676488435,-2.495));
#90113=CARTESIAN_POINT('Origin',(0.3,0.,0.));
#90114=CARTESIAN_POINT('Origin',(0.3,-4.49173072735664,-1.6348562850967));
#90115=CARTESIAN_POINT('',(0.3,-4.72908060747227,-1.6235136611774));
#90116=CARTESIAN_POINT('',(5.4,-4.72908060747227,-1.6235136611774));
#90117=CARTESIAN_POINT('',(2.7,-4.72908060747227,-1.6235136611774));
#90118=CARTESIAN_POINT('',(0.3,-4.49173072735664,-1.6348562850967));
#90119=CARTESIAN_POINT('',(0.3,-4.94659717331204,-1.61311884403516));
#90120=CARTESIAN_POINT('',(5.4,-4.49173072735664,-1.6348562850967));
#90121=CARTESIAN_POINT('',(0.3,-4.49173072735664,-1.6348562850967));
#90122=CARTESIAN_POINT('',(5.4,-4.94659717331204,-1.61311884403516));
#90123=CARTESIAN_POINT('Origin',(5.4,-4.68906617772168,-1.70668051519509));
#90124=CARTESIAN_POINT('',(5.4,-4.66626038597752,-1.79611080121937));
#90125=CARTESIAN_POINT('Origin',(5.4,0.,0.));
#90126=CARTESIAN_POINT('',(5.4,-4.49173072735664,-1.6348562850967));
#90127=CARTESIAN_POINT('Origin',(0.3,-4.82620608286141,-1.9438906465518));
#90128=CARTESIAN_POINT('',(0.3,-4.66626038597752,-1.79611080121937));
#90129=CARTESIAN_POINT('',(2.7,-4.66626038597752,-1.79611080121937));
#90130=CARTESIAN_POINT('',(0.3,-4.49173072735664,-1.6348562850967));
#90131=CARTESIAN_POINT('Origin',(0.3,-4.68906617772168,-1.70668051519509));
#90132=CARTESIAN_POINT('Origin',(0.3,0.,0.));
#90133=CARTESIAN_POINT('Origin',(0.3,-4.70738105939836,-0.830038289247926));
#90134=CARTESIAN_POINT('',(0.3,-4.9391554355392,-0.777652611121161));
#90135=CARTESIAN_POINT('',(5.4,-4.9391554355392,-0.777652611121161));
#90136=CARTESIAN_POINT('',(2.7,-4.9391554355392,-0.777652611121161));
#90137=CARTESIAN_POINT('',(0.3,-4.70738105939836,-0.830038289247926));
#90138=CARTESIAN_POINT('',(0.3,-5.15156239493286,-0.729644359337888));
#90139=CARTESIAN_POINT('',(5.4,-4.70738105939836,-0.830038289247926));
#90140=CARTESIAN_POINT('',(0.3,-4.70738105939836,-0.830038289247926));
#90141=CARTESIAN_POINT('',(5.4,-5.15156239493286,-0.729644359337888));
#90142=CARTESIAN_POINT('Origin',(5.4,-4.91419068753092,-0.866504406557981));
#90143=CARTESIAN_POINT('',(5.4,-4.90726077320404,-0.958536229765421));
#90144=CARTESIAN_POINT('Origin',(5.4,0.,0.));
#90145=CARTESIAN_POINT('',(5.4,-4.70738105939836,-0.830038289247926));
#90146=CARTESIAN_POINT('Origin',(0.3,-5.0904382363941,-1.07629668839818));
#90147=CARTESIAN_POINT('',(0.3,-4.90726077320404,-0.958536229765421));
#90148=CARTESIAN_POINT('',(2.7,-4.90726077320404,-0.958536229765421));
#90149=CARTESIAN_POINT('',(0.3,-4.70738105939836,-0.830038289247926));
#90150=CARTESIAN_POINT('Origin',(0.3,-4.91419068753092,-0.866504406557981));
#90151=CARTESIAN_POINT('Origin',(0.3,0.,0.));
#90152=CARTESIAN_POINT('Origin',(0.3,-4.78,5.85381169992435E-16));
#90153=CARTESIAN_POINT('',(0.3,-4.99915652503051,0.0918370200127872));
#90154=CARTESIAN_POINT('',(5.4,-4.99915652503051,0.0918370200127872));
#90155=CARTESIAN_POINT('',(2.7,-4.99915652503051,0.0918370200127877));
#90156=CARTESIAN_POINT('',(0.3,-4.78,5.85381169992435E-16));
#90157=CARTESIAN_POINT('',(0.3,-5.2,0.176000000000001));
#90158=CARTESIAN_POINT('',(5.4,-4.78,5.85381169992435E-16));
#90159=CARTESIAN_POINT('',(0.3,-4.78,5.85381169992435E-16));
#90160=CARTESIAN_POINT('',(5.4,-5.2,0.176000000000001));
#90161=CARTESIAN_POINT('Origin',(5.4,-4.99,6.11098752774529E-16));
#90162=CARTESIAN_POINT('',(5.4,-5.,-6.12323399573677E-16));
#90163=CARTESIAN_POINT('Origin',(5.4,0.,0.));
#90164=CARTESIAN_POINT('',(5.4,-4.99915652503051,-0.0918370200127866));
#90165=CARTESIAN_POINT('',(5.4,-4.78,5.85381169992435E-16));
#90166=CARTESIAN_POINT('Origin',(5.4,0.,0.));
#90167=CARTESIAN_POINT('Origin',(0.3,-5.2,-0.175999999999999));
#90168=CARTESIAN_POINT('',(0.3,-4.99915652503051,-0.0918370200127866));
#90169=CARTESIAN_POINT('',(2.7,-4.99915652503051,-0.091837020012786));
#90170=CARTESIAN_POINT('',(0.3,-4.78,5.85381169992435E-16));
#90171=CARTESIAN_POINT('Origin',(0.3,-4.99,6.11098752774529E-16));
#90172=CARTESIAN_POINT('',(0.3,-5.,-6.12323399573677E-16));
#90173=CARTESIAN_POINT('Origin',(0.3,0.,0.));
#90174=CARTESIAN_POINT('Origin',(0.3,0.,0.));
#90175=CARTESIAN_POINT('Origin',(0.3,-4.70738105939835,0.830038289247929));
#90176=CARTESIAN_POINT('',(0.3,-4.90726077320404,0.958536229765424));
#90177=CARTESIAN_POINT('',(5.4,-4.90726077320404,0.958536229765424));
#90178=CARTESIAN_POINT('',(2.7,-4.90726077320404,0.958536229765425));
#90179=CARTESIAN_POINT('',(0.3,-4.70738105939835,0.830038289247929));
#90180=CARTESIAN_POINT('',(0.3,-5.0904382363941,1.07629668839819));
#90181=CARTESIAN_POINT('',(5.4,-4.70738105939835,0.830038289247929));
#90182=CARTESIAN_POINT('',(0.3,-4.70738105939835,0.830038289247929));
#90183=CARTESIAN_POINT('',(5.4,-5.0904382363941,1.07629668839819));
#90184=CARTESIAN_POINT('Origin',(5.4,-4.91419068753092,0.866504406557984));
#90185=CARTESIAN_POINT('',(5.4,-4.9391554355392,0.777652611121165));
#90186=CARTESIAN_POINT('Origin',(5.4,0.,0.));
#90187=CARTESIAN_POINT('',(5.4,-4.70738105939835,0.830038289247929));
#90188=CARTESIAN_POINT('Origin',(0.3,-5.15156239493286,0.729644359337891));
#90189=CARTESIAN_POINT('',(0.3,-4.9391554355392,0.777652611121165));
#90190=CARTESIAN_POINT('',(2.7,-4.9391554355392,0.777652611121165));
#90191=CARTESIAN_POINT('',(0.3,-4.70738105939835,0.830038289247929));
#90192=CARTESIAN_POINT('Origin',(0.3,-4.91419068753092,0.866504406557984));
#90193=CARTESIAN_POINT('Origin',(0.3,0.,0.));
#90194=CARTESIAN_POINT('Origin',(0.3,-4.49173072735664,1.6348562850967));
#90195=CARTESIAN_POINT('',(0.3,-4.66626038597752,1.79611080121937));
#90196=CARTESIAN_POINT('',(5.4,-4.66626038597752,1.79611080121937));
#90197=CARTESIAN_POINT('',(2.7,-4.66626038597752,1.79611080121937));
#90198=CARTESIAN_POINT('',(0.3,-4.49173072735664,1.6348562850967));
#90199=CARTESIAN_POINT('',(0.3,-4.82620608286141,1.9438906465518));
#90200=CARTESIAN_POINT('',(5.4,-4.49173072735664,1.6348562850967));
#90201=CARTESIAN_POINT('',(0.3,-4.49173072735664,1.6348562850967));
#90202=CARTESIAN_POINT('',(5.4,-4.82620608286141,1.9438906465518));
#90203=CARTESIAN_POINT('Origin',(5.4,-4.68906617772168,1.70668051519509));
#90204=CARTESIAN_POINT('',(5.4,-4.72908060747227,1.62351366117741));
#90205=CARTESIAN_POINT('Origin',(5.4,0.,0.));
#90206=CARTESIAN_POINT('',(5.4,-4.49173072735664,1.6348562850967));
#90207=CARTESIAN_POINT('Origin',(0.3,-4.94659717331204,1.61311884403516));
#90208=CARTESIAN_POINT('',(0.3,-4.72908060747227,1.62351366117741));
#90209=CARTESIAN_POINT('',(2.7,-4.72908060747227,1.62351366117741));
#90210=CARTESIAN_POINT('',(0.3,-4.49173072735664,1.6348562850967));
#90211=CARTESIAN_POINT('Origin',(0.3,-4.68906617772168,1.70668051519509));
#90212=CARTESIAN_POINT('Origin',(0.3,0.,0.));
#90213=CARTESIAN_POINT('Origin',(0.3,-4.13960143008962,2.39));
#90214=CARTESIAN_POINT('',(0.3,-4.28347803816477,2.57911145485419));
#90215=CARTESIAN_POINT('',(5.4,-4.28347803816477,2.57911145485419));
#90216=CARTESIAN_POINT('',(2.7,-4.28347803816477,2.57911145485419));
#90217=CARTESIAN_POINT('',(0.3,-4.13960143008962,2.39));
#90218=CARTESIAN_POINT('',(0.3,-4.41533209967908,2.75242047106606));
#90219=CARTESIAN_POINT('',(5.4,-4.13960143008962,2.39));
#90220=CARTESIAN_POINT('',(0.3,-4.13960143008962,2.39));
#90221=CARTESIAN_POINT('',(5.4,-4.41533209967908,2.75242047106606));
#90222=CARTESIAN_POINT('Origin',(5.4,-4.32146676488435,2.495));
#90223=CARTESIAN_POINT('',(5.4,-4.37531505817756,2.42004507017632));
#90224=CARTESIAN_POINT('Origin',(5.4,0.,0.));
#90225=CARTESIAN_POINT('',(5.4,-4.13960143008962,2.39));
#90226=CARTESIAN_POINT('Origin',(0.3,-4.59133209967908,2.44757952893394));
#90227=CARTESIAN_POINT('',(0.3,-4.37531505817756,2.42004507017632));
#90228=CARTESIAN_POINT('',(2.7,-4.37531505817756,2.42004507017632));
#90229=CARTESIAN_POINT('',(0.3,-4.13960143008962,2.39));
#90230=CARTESIAN_POINT('Origin',(0.3,-4.32146676488435,2.495));
#90231=CARTESIAN_POINT('Origin',(0.3,0.,0.));
#90232=CARTESIAN_POINT('Origin',(0.3,-3.66169243810871,3.07252477430166));
#90233=CARTESIAN_POINT('',(0.3,-3.77054437770685,3.28374711202663));
#90234=CARTESIAN_POINT('',(5.4,-3.77054437770685,3.28374711202663));
#90235=CARTESIAN_POINT('',(2.7,-3.77054437770685,3.28374711202663));
#90236=CARTESIAN_POINT('',(0.3,-3.66169243810871,3.07252477430166));
#90237=CARTESIAN_POINT('',(0.3,-3.87030048491385,3.47731939235895));
#90238=CARTESIAN_POINT('',(5.4,-3.66169243810871,3.07252477430166));
#90239=CARTESIAN_POINT('',(0.3,-3.66169243810871,3.07252477430166));
#90240=CARTESIAN_POINT('',(5.4,-3.87030048491385,3.47731939235895));
#90241=CARTESIAN_POINT('Origin',(5.4,-3.8225617711637,3.20751017233583));
#90242=CARTESIAN_POINT('',(5.4,-3.88860777485636,3.14304463431983));
#90243=CARTESIAN_POINT('Origin',(5.4,0.,0.));
#90244=CARTESIAN_POINT('',(5.4,-3.66169243810871,3.07252477430166));
#90245=CARTESIAN_POINT('Origin',(0.3,-4.09656172352352,3.20767174838107));
#90246=CARTESIAN_POINT('',(0.3,-3.88860777485636,3.14304463431983));
#90247=CARTESIAN_POINT('',(2.7,-3.88860777485636,3.14304463431983));
#90248=CARTESIAN_POINT('',(0.3,-3.66169243810871,3.07252477430166));
#90249=CARTESIAN_POINT('Origin',(0.3,-3.8225617711637,3.20751017233583));
#90250=CARTESIAN_POINT('Origin',(0.3,0.,0.));
#90251=CARTESIAN_POINT('Origin',(0.3,-3.07252477430166,3.66169243810872));
#90252=CARTESIAN_POINT('',(0.3,-3.14304463431983,3.88860777485636));
#90253=CARTESIAN_POINT('',(5.4,-3.14304463431983,3.88860777485636));
#90254=CARTESIAN_POINT('',(2.7,-3.14304463431983,3.88860777485636));
#90255=CARTESIAN_POINT('',(0.3,-3.07252477430166,3.66169243810872));
#90256=CARTESIAN_POINT('',(0.3,-3.20767174838106,4.09656172352352));
#90257=CARTESIAN_POINT('',(5.4,-3.07252477430166,3.66169243810872));
#90258=CARTESIAN_POINT('',(0.3,-3.07252477430166,3.66169243810872));
#90259=CARTESIAN_POINT('',(5.4,-3.20767174838106,4.09656172352352));
#90260=CARTESIAN_POINT('Origin',(5.4,-3.20751017233583,3.8225617711637));
#90261=CARTESIAN_POINT('',(5.4,-3.28374711202663,3.77054437770685));
#90262=CARTESIAN_POINT('Origin',(5.4,0.,0.));
#90263=CARTESIAN_POINT('',(5.4,-3.07252477430166,3.66169243810872));
#90264=CARTESIAN_POINT('Origin',(0.3,-3.47731939235894,3.87030048491386));
#90265=CARTESIAN_POINT('',(0.3,-3.28374711202663,3.77054437770685));
#90266=CARTESIAN_POINT('',(2.7,-3.28374711202663,3.77054437770685));
#90267=CARTESIAN_POINT('',(0.3,-3.07252477430166,3.66169243810872));
#90268=CARTESIAN_POINT('Origin',(0.3,-3.20751017233583,3.8225617711637));
#90269=CARTESIAN_POINT('Origin',(0.3,0.,0.));
#90270=CARTESIAN_POINT('Origin',(0.3,-2.39,4.13960143008962));
#90271=CARTESIAN_POINT('',(0.3,-2.42004507017632,4.37531505817756));
#90272=CARTESIAN_POINT('',(5.4,-2.42004507017632,4.37531505817756));
#90273=CARTESIAN_POINT('',(2.7,-2.42004507017632,4.37531505817756));
#90274=CARTESIAN_POINT('',(0.3,-2.39,4.13960143008962));
#90275=CARTESIAN_POINT('',(0.3,-2.44757952893394,4.59133209967908));
#90276=CARTESIAN_POINT('',(5.4,-2.39,4.13960143008962));
#90277=CARTESIAN_POINT('',(0.3,-2.39,4.13960143008962));
#90278=CARTESIAN_POINT('',(5.4,-2.44757952893394,4.59133209967908));
#90279=CARTESIAN_POINT('Origin',(5.4,-2.495,4.32146676488435));
#90280=CARTESIAN_POINT('',(5.4,-2.57911145485419,4.28347803816477));
#90281=CARTESIAN_POINT('Origin',(5.4,0.,0.));
#90282=CARTESIAN_POINT('',(5.4,-2.39,4.13960143008962));
#90283=CARTESIAN_POINT('Origin',(0.3,-2.75242047106606,4.41533209967908));
#90284=CARTESIAN_POINT('',(0.3,-2.57911145485419,4.28347803816477));
#90285=CARTESIAN_POINT('',(2.7,-2.57911145485419,4.28347803816477));
#90286=CARTESIAN_POINT('',(0.3,-2.39,4.13960143008962));
#90287=CARTESIAN_POINT('Origin',(0.3,-2.495,4.32146676488435));
#90288=CARTESIAN_POINT('Origin',(0.3,0.,0.));
#90289=CARTESIAN_POINT('Origin',(0.3,-1.6348562850967,4.49173072735664));
#90290=CARTESIAN_POINT('',(0.3,-1.6235136611774,4.72908060747227));
#90291=CARTESIAN_POINT('',(5.4,-1.6235136611774,4.72908060747227));
#90292=CARTESIAN_POINT('',(2.7,-1.6235136611774,4.72908060747227));
#90293=CARTESIAN_POINT('',(0.3,-1.6348562850967,4.49173072735664));
#90294=CARTESIAN_POINT('',(0.3,-1.61311884403516,4.94659717331204));
#90295=CARTESIAN_POINT('',(5.4,-1.6348562850967,4.49173072735664));
#90296=CARTESIAN_POINT('',(0.3,-1.6348562850967,4.49173072735664));
#90297=CARTESIAN_POINT('',(5.4,-1.61311884403516,4.94659717331204));
#90298=CARTESIAN_POINT('Origin',(5.4,-1.70668051519509,4.68906617772168));
#90299=CARTESIAN_POINT('',(5.4,-1.79611080121937,4.66626038597752));
#90300=CARTESIAN_POINT('Origin',(5.4,0.,0.));
#90301=CARTESIAN_POINT('',(5.4,-1.6348562850967,4.49173072735664));
#90302=CARTESIAN_POINT('Origin',(0.3,-1.9438906465518,4.82620608286141));
#90303=CARTESIAN_POINT('',(0.3,-1.79611080121937,4.66626038597752));
#90304=CARTESIAN_POINT('',(2.7,-1.79611080121937,4.66626038597752));
#90305=CARTESIAN_POINT('',(0.3,-1.6348562850967,4.49173072735664));
#90306=CARTESIAN_POINT('Origin',(0.3,-1.70668051519509,4.68906617772168));
#90307=CARTESIAN_POINT('Origin',(0.3,0.,0.));
#90308=CARTESIAN_POINT('Origin',(0.3,-0.830038289247927,4.70738105939836));
#90309=CARTESIAN_POINT('',(0.3,-0.777652611121163,4.9391554355392));
#90310=CARTESIAN_POINT('',(5.4,-0.777652611121163,4.9391554355392));
#90311=CARTESIAN_POINT('',(2.7,-0.777652611121163,4.9391554355392));
#90312=CARTESIAN_POINT('',(0.3,-0.830038289247927,4.70738105939836));
#90313=CARTESIAN_POINT('',(0.3,-0.729644359337889,5.15156239493286));
#90314=CARTESIAN_POINT('',(5.4,-0.830038289247927,4.70738105939836));
#90315=CARTESIAN_POINT('',(0.3,-0.830038289247927,4.70738105939836));
#90316=CARTESIAN_POINT('',(5.4,-0.729644359337889,5.15156239493286));
#90317=CARTESIAN_POINT('Origin',(5.4,-0.866504406557982,4.91419068753092));
#90318=CARTESIAN_POINT('',(5.4,-0.958536229765423,4.90726077320404));
#90319=CARTESIAN_POINT('Origin',(5.4,0.,0.));
#90320=CARTESIAN_POINT('',(5.4,-0.830038289247927,4.70738105939836));
#90321=CARTESIAN_POINT('Origin',(0.3,-1.07629668839819,5.0904382363941));
#90322=CARTESIAN_POINT('',(0.3,-0.958536229765423,4.90726077320404));
#90323=CARTESIAN_POINT('',(2.7,-0.958536229765423,4.90726077320404));
#90324=CARTESIAN_POINT('',(0.3,-0.830038289247927,4.70738105939836));
#90325=CARTESIAN_POINT('Origin',(0.3,-0.866504406557982,4.91419068753092));
#90326=CARTESIAN_POINT('Origin',(0.3,0.,0.));
#90327=CARTESIAN_POINT('Origin',(0.3,2.92690584996217E-16,4.78));
#90328=CARTESIAN_POINT('',(0.3,0.0918370200127869,4.99915652503051));
#90329=CARTESIAN_POINT('',(5.4,0.0918370200127869,4.99915652503051));
#90330=CARTESIAN_POINT('',(2.7,0.0918370200127874,4.99915652503051));
#90331=CARTESIAN_POINT('',(0.3,2.92690584996217E-16,4.78));
#90332=CARTESIAN_POINT('',(0.3,0.176,5.2));
#90333=CARTESIAN_POINT('',(5.4,2.92690584996217E-16,4.78));
#90334=CARTESIAN_POINT('',(0.3,2.92690584996217E-16,4.78));
#90335=CARTESIAN_POINT('',(5.4,0.176,5.2));
#90336=CARTESIAN_POINT('Origin',(5.4,3.05549376387265E-16,4.99));
#90337=CARTESIAN_POINT('',(5.4,-0.0918370200127869,4.99915652503051));
#90338=CARTESIAN_POINT('Origin',(5.4,0.,0.));
#90339=CARTESIAN_POINT('',(5.4,2.92690584996217E-16,4.78));
#90340=CARTESIAN_POINT('Origin',(0.3,-0.176,5.2));
#90341=CARTESIAN_POINT('',(0.3,-0.0918370200127869,4.99915652503051));
#90342=CARTESIAN_POINT('',(2.7,-0.0918370200127863,4.99915652503051));
#90343=CARTESIAN_POINT('',(0.3,2.92690584996217E-16,4.78));
#90344=CARTESIAN_POINT('Origin',(0.3,3.05549376387265E-16,4.99));
#90345=CARTESIAN_POINT('Origin',(0.3,0.,0.));
#90346=CARTESIAN_POINT('Origin',(0.3,0.830038289247928,4.70738105939836));
#90347=CARTESIAN_POINT('',(0.3,0.958536229765423,4.90726077320404));
#90348=CARTESIAN_POINT('',(5.4,0.958536229765423,4.90726077320404));
#90349=CARTESIAN_POINT('',(2.7,0.958536229765423,4.90726077320404));
#90350=CARTESIAN_POINT('',(0.3,0.830038289247928,4.70738105939836));
#90351=CARTESIAN_POINT('',(0.3,1.07629668839819,5.0904382363941));
#90352=CARTESIAN_POINT('',(5.4,0.830038289247928,4.70738105939836));
#90353=CARTESIAN_POINT('',(0.3,0.830038289247928,4.70738105939836));
#90354=CARTESIAN_POINT('',(5.4,1.07629668839819,5.0904382363941));
#90355=CARTESIAN_POINT('Origin',(5.4,0.866504406557983,4.91419068753092));
#90356=CARTESIAN_POINT('',(5.4,0.777652611121164,4.9391554355392));
#90357=CARTESIAN_POINT('Origin',(5.4,0.,0.));
#90358=CARTESIAN_POINT('',(5.4,0.830038289247928,4.70738105939836));
#90359=CARTESIAN_POINT('Origin',(0.3,0.72964435933789,5.15156239493286));
#90360=CARTESIAN_POINT('',(0.3,0.777652611121164,4.9391554355392));
#90361=CARTESIAN_POINT('',(2.7,0.777652611121163,4.9391554355392));
#90362=CARTESIAN_POINT('',(0.3,0.830038289247928,4.70738105939836));
#90363=CARTESIAN_POINT('Origin',(0.3,0.866504406557983,4.91419068753092));
#90364=CARTESIAN_POINT('Origin',(0.3,0.,0.));
#90365=CARTESIAN_POINT('Origin',(0.3,1.6348562850967,4.49173072735664));
#90366=CARTESIAN_POINT('',(0.3,1.79611080121937,4.66626038597752));
#90367=CARTESIAN_POINT('',(5.4,1.79611080121937,4.66626038597752));
#90368=CARTESIAN_POINT('',(2.7,1.79611080121937,4.66626038597752));
#90369=CARTESIAN_POINT('',(0.3,1.6348562850967,4.49173072735664));
#90370=CARTESIAN_POINT('',(0.3,1.9438906465518,4.82620608286141));
#90371=CARTESIAN_POINT('',(5.4,1.6348562850967,4.49173072735664));
#90372=CARTESIAN_POINT('',(0.3,1.6348562850967,4.49173072735664));
#90373=CARTESIAN_POINT('',(5.4,1.9438906465518,4.82620608286141));
#90374=CARTESIAN_POINT('Origin',(5.4,1.70668051519509,4.68906617772168));
#90375=CARTESIAN_POINT('',(5.4,1.62351366117741,4.72908060747227));
#90376=CARTESIAN_POINT('Origin',(5.4,0.,0.));
#90377=CARTESIAN_POINT('',(5.4,1.6348562850967,4.49173072735664));
#90378=CARTESIAN_POINT('Origin',(0.3,1.61311884403516,4.94659717331204));
#90379=CARTESIAN_POINT('',(0.3,1.62351366117741,4.72908060747227));
#90380=CARTESIAN_POINT('',(2.7,1.62351366117741,4.72908060747227));
#90381=CARTESIAN_POINT('',(0.3,1.6348562850967,4.49173072735664));
#90382=CARTESIAN_POINT('Origin',(0.3,1.70668051519509,4.68906617772168));
#90383=CARTESIAN_POINT('Origin',(0.3,0.,0.));
#90384=CARTESIAN_POINT('Origin',(0.3,2.39,4.13960143008962));
#90385=CARTESIAN_POINT('',(0.3,2.57911145485419,4.28347803816477));
#90386=CARTESIAN_POINT('',(5.4,2.57911145485419,4.28347803816477));
#90387=CARTESIAN_POINT('',(2.7,2.57911145485419,4.28347803816477));
#90388=CARTESIAN_POINT('',(0.3,2.39,4.13960143008962));
#90389=CARTESIAN_POINT('',(0.3,2.75242047106606,4.41533209967908));
#90390=CARTESIAN_POINT('',(5.4,2.39,4.13960143008962));
#90391=CARTESIAN_POINT('',(0.3,2.39,4.13960143008962));
#90392=CARTESIAN_POINT('',(5.4,2.75242047106606,4.41533209967908));
#90393=CARTESIAN_POINT('Origin',(5.4,2.495,4.32146676488435));
#90394=CARTESIAN_POINT('',(5.4,2.42004507017632,4.37531505817756));
#90395=CARTESIAN_POINT('Origin',(5.4,0.,0.));
#90396=CARTESIAN_POINT('',(5.4,2.39,4.13960143008962));
#90397=CARTESIAN_POINT('Origin',(0.3,2.44757952893394,4.59133209967908));
#90398=CARTESIAN_POINT('',(0.3,2.42004507017632,4.37531505817756));
#90399=CARTESIAN_POINT('',(2.7,2.42004507017632,4.37531505817756));
#90400=CARTESIAN_POINT('',(0.3,2.39,4.13960143008962));
#90401=CARTESIAN_POINT('Origin',(0.3,2.495,4.32146676488435));
#90402=CARTESIAN_POINT('Origin',(0.3,0.,0.));
#90403=CARTESIAN_POINT('Origin',(0.3,3.07252477430166,3.66169243810872));
#90404=CARTESIAN_POINT('',(0.3,3.28374711202663,3.77054437770685));
#90405=CARTESIAN_POINT('',(5.4,3.28374711202663,3.77054437770685));
#90406=CARTESIAN_POINT('',(2.7,3.28374711202663,3.77054437770685));
#90407=CARTESIAN_POINT('',(0.3,3.07252477430166,3.66169243810872));
#90408=CARTESIAN_POINT('',(0.3,3.47731939235894,3.87030048491386));
#90409=CARTESIAN_POINT('',(5.4,3.07252477430166,3.66169243810872));
#90410=CARTESIAN_POINT('',(0.3,3.07252477430166,3.66169243810872));
#90411=CARTESIAN_POINT('',(5.4,3.47731939235894,3.87030048491386));
#90412=CARTESIAN_POINT('Origin',(5.4,3.20751017233583,3.8225617711637));
#90413=CARTESIAN_POINT('',(5.4,3.14304463431983,3.88860777485636));
#90414=CARTESIAN_POINT('Origin',(5.4,0.,0.));
#90415=CARTESIAN_POINT('',(5.4,3.07252477430166,3.66169243810872));
#90416=CARTESIAN_POINT('Origin',(0.3,3.20767174838106,4.09656172352352));
#90417=CARTESIAN_POINT('',(0.3,3.14304463431983,3.88860777485636));
#90418=CARTESIAN_POINT('',(2.7,3.14304463431983,3.88860777485636));
#90419=CARTESIAN_POINT('',(0.3,3.07252477430166,3.66169243810872));
#90420=CARTESIAN_POINT('Origin',(0.3,3.20751017233583,3.8225617711637));
#90421=CARTESIAN_POINT('Origin',(0.3,0.,0.));
#90422=CARTESIAN_POINT('Origin',(0.3,3.66169243810872,3.07252477430166));
#90423=CARTESIAN_POINT('',(0.3,3.88860777485636,3.14304463431983));
#90424=CARTESIAN_POINT('',(5.4,3.88860777485636,3.14304463431983));
#90425=CARTESIAN_POINT('',(2.7,3.88860777485636,3.14304463431983));
#90426=CARTESIAN_POINT('',(0.3,3.66169243810872,3.07252477430166));
#90427=CARTESIAN_POINT('',(0.3,4.09656172352352,3.20767174838106));
#90428=CARTESIAN_POINT('',(5.4,3.66169243810872,3.07252477430166));
#90429=CARTESIAN_POINT('',(0.3,3.66169243810872,3.07252477430166));
#90430=CARTESIAN_POINT('',(5.4,4.09656172352352,3.20767174838106));
#90431=CARTESIAN_POINT('Origin',(5.4,3.8225617711637,3.20751017233583));
#90432=CARTESIAN_POINT('',(5.4,3.77054437770685,3.28374711202663));
#90433=CARTESIAN_POINT('Origin',(5.4,0.,0.));
#90434=CARTESIAN_POINT('',(5.4,3.66169243810872,3.07252477430166));
#90435=CARTESIAN_POINT('Origin',(0.3,3.87030048491386,3.47731939235894));
#90436=CARTESIAN_POINT('',(0.3,3.77054437770685,3.28374711202663));
#90437=CARTESIAN_POINT('',(2.7,3.77054437770685,3.28374711202663));
#90438=CARTESIAN_POINT('',(0.3,3.66169243810872,3.07252477430166));
#90439=CARTESIAN_POINT('Origin',(0.3,3.8225617711637,3.20751017233583));
#90440=CARTESIAN_POINT('Origin',(0.3,0.,0.));
#90441=CARTESIAN_POINT('Origin',(0.3,4.13960143008962,2.39));
#90442=CARTESIAN_POINT('',(0.3,4.37531505817756,2.42004507017632));
#90443=CARTESIAN_POINT('',(5.4,4.37531505817756,2.42004507017632));
#90444=CARTESIAN_POINT('',(2.7,4.37531505817756,2.42004507017632));
#90445=CARTESIAN_POINT('',(0.3,4.13960143008962,2.39));
#90446=CARTESIAN_POINT('',(0.3,4.59133209967908,2.44757952893394));
#90447=CARTESIAN_POINT('',(5.4,4.13960143008962,2.39));
#90448=CARTESIAN_POINT('',(0.3,4.13960143008962,2.39));
#90449=CARTESIAN_POINT('',(5.4,4.59133209967908,2.44757952893394));
#90450=CARTESIAN_POINT('Origin',(5.4,4.32146676488435,2.495));
#90451=CARTESIAN_POINT('',(5.4,4.28347803816477,2.57911145485419));
#90452=CARTESIAN_POINT('Origin',(5.4,0.,0.));
#90453=CARTESIAN_POINT('',(5.4,4.13960143008962,2.39));
#90454=CARTESIAN_POINT('Origin',(0.3,4.41533209967908,2.75242047106606));
#90455=CARTESIAN_POINT('',(0.3,4.28347803816477,2.57911145485419));
#90456=CARTESIAN_POINT('',(2.7,4.28347803816477,2.57911145485419));
#90457=CARTESIAN_POINT('',(0.3,4.13960143008962,2.39));
#90458=CARTESIAN_POINT('Origin',(0.3,4.32146676488435,2.495));
#90459=CARTESIAN_POINT('Origin',(0.3,0.,0.));
#90460=CARTESIAN_POINT('Origin',(0.3,4.49173072735664,1.6348562850967));
#90461=CARTESIAN_POINT('',(0.3,4.72908060747227,1.6235136611774));
#90462=CARTESIAN_POINT('',(5.4,4.72908060747227,1.6235136611774));
#90463=CARTESIAN_POINT('',(2.7,4.72908060747227,1.6235136611774));
#90464=CARTESIAN_POINT('',(0.3,4.49173072735664,1.6348562850967));
#90465=CARTESIAN_POINT('',(0.3,4.94659717331204,1.61311884403516));
#90466=CARTESIAN_POINT('',(5.4,4.49173072735664,1.6348562850967));
#90467=CARTESIAN_POINT('',(0.3,4.49173072735664,1.6348562850967));
#90468=CARTESIAN_POINT('',(5.4,4.94659717331204,1.61311884403516));
#90469=CARTESIAN_POINT('Origin',(5.4,4.68906617772168,1.70668051519509));
#90470=CARTESIAN_POINT('',(5.4,4.66626038597752,1.79611080121937));
#90471=CARTESIAN_POINT('Origin',(5.4,0.,0.));
#90472=CARTESIAN_POINT('',(5.4,4.49173072735664,1.6348562850967));
#90473=CARTESIAN_POINT('Origin',(0.3,4.82620608286141,1.9438906465518));
#90474=CARTESIAN_POINT('',(0.3,4.66626038597752,1.79611080121937));
#90475=CARTESIAN_POINT('',(2.7,4.66626038597752,1.79611080121937));
#90476=CARTESIAN_POINT('',(0.3,4.49173072735664,1.6348562850967));
#90477=CARTESIAN_POINT('Origin',(0.3,4.68906617772168,1.70668051519509));
#90478=CARTESIAN_POINT('Origin',(0.3,0.,0.));
#90479=CARTESIAN_POINT('Origin',(0.3,4.70738105939836,0.830038289247927));
#90480=CARTESIAN_POINT('',(0.3,4.9391554355392,0.777652611121163));
#90481=CARTESIAN_POINT('',(5.4,4.9391554355392,0.777652611121163));
#90482=CARTESIAN_POINT('',(2.7,4.9391554355392,0.777652611121163));
#90483=CARTESIAN_POINT('',(0.3,4.70738105939836,0.830038289247927));
#90484=CARTESIAN_POINT('',(0.3,5.15156239493286,0.729644359337889));
#90485=CARTESIAN_POINT('',(5.4,4.70738105939836,0.830038289247927));
#90486=CARTESIAN_POINT('',(0.3,4.70738105939836,0.830038289247927));
#90487=CARTESIAN_POINT('',(5.4,5.15156239493286,0.729644359337889));
#90488=CARTESIAN_POINT('Origin',(5.4,4.91419068753092,0.866504406557982));
#90489=CARTESIAN_POINT('',(5.4,4.90726077320404,0.958536229765423));
#90490=CARTESIAN_POINT('Origin',(5.4,0.,0.));
#90491=CARTESIAN_POINT('',(5.4,4.70738105939836,0.830038289247927));
#90492=CARTESIAN_POINT('Origin',(0.3,5.0904382363941,1.07629668839819));
#90493=CARTESIAN_POINT('',(0.3,4.90726077320404,0.958536229765423));
#90494=CARTESIAN_POINT('',(2.7,4.90726077320404,0.958536229765423));
#90495=CARTESIAN_POINT('',(0.3,4.70738105939836,0.830038289247927));
#90496=CARTESIAN_POINT('Origin',(0.3,4.91419068753092,0.866504406557982));
#90497=CARTESIAN_POINT('Origin',(0.3,0.,0.));
#90498=CARTESIAN_POINT('Origin',(5.4,4.99,0.));
#90499=CARTESIAN_POINT('',(5.4,4.99915652503051,-0.0918370200127866));
#90500=CARTESIAN_POINT('',(5.4,4.99915652503051,0.0918370200127872));
#90501=CARTESIAN_POINT('Origin',(5.4,0.,0.));
#90502=CARTESIAN_POINT('',(5.4,4.78,0.));
#90503=CARTESIAN_POINT('',(5.4,5.2,-0.176));
#90504=CARTESIAN_POINT('',(5.4,4.78,0.));
#90505=CARTESIAN_POINT('Origin',(0.3,4.78,0.));
#90506=CARTESIAN_POINT('',(0.3,4.99915652503051,-0.0918370200127866));
#90507=CARTESIAN_POINT('',(2.7,4.99915652503051,-0.0918370200127872));
#90508=CARTESIAN_POINT('',(0.3,4.78,0.));
#90509=CARTESIAN_POINT('',(0.3,5.2,-0.176));
#90510=CARTESIAN_POINT('',(0.3,4.78,0.));
#90511=CARTESIAN_POINT('Origin',(0.3,5.2,0.176));
#90512=CARTESIAN_POINT('',(0.3,4.99915652503051,0.0918370200127872));
#90513=CARTESIAN_POINT('',(2.7,4.99915652503051,0.0918370200127866));
#90514=CARTESIAN_POINT('',(0.3,4.78,0.));
#90515=CARTESIAN_POINT('Origin',(0.3,4.99,0.));
#90516=CARTESIAN_POINT('Origin',(0.3,0.,0.));
#90517=CARTESIAN_POINT('Origin',(2.25392422621555,0.,0.));
#90518=CARTESIAN_POINT('',(1.4978484524311,0.,0.));
#90519=CARTESIAN_POINT('',(3.,-2.48346726553949,3.04137023753017E-16));
#90520=CARTESIAN_POINT('',(2.25392422621555,-1.25,-1.53080849893419E-16));
#90521=CARTESIAN_POINT('Origin',(3.,0.,0.));
#90522=CARTESIAN_POINT('Origin',(3.,1.76762539787484E-16,2.88675134594813));
#90523=CARTESIAN_POINT('',(6.,-2.5,1.44337567297406));
#90524=CARTESIAN_POINT('',(6.,1.76762539787484E-16,2.88675134594813));
#90525=CARTESIAN_POINT('',(6.,-0.625,2.52590742770461));
#90526=CARTESIAN_POINT('',(3.,-2.5,1.44337567297406));
#90527=CARTESIAN_POINT('',(3.,-2.5,1.44337567297406));
#90528=CARTESIAN_POINT('',(3.,1.76762539787484E-16,2.88675134594813));
#90529=CARTESIAN_POINT('',(3.,1.76762539787484E-16,2.88675134594813));
#90530=CARTESIAN_POINT('',(3.,1.76762539787484E-16,2.88675134594813));
#90531=CARTESIAN_POINT('Origin',(3.,2.5,1.44337567297406));
#90532=CARTESIAN_POINT('',(6.,2.5,1.44337567297406));
#90533=CARTESIAN_POINT('',(6.,1.875,1.80421959121758));
#90534=CARTESIAN_POINT('',(3.,2.5,1.44337567297406));
#90535=CARTESIAN_POINT('',(3.,2.5,1.44337567297406));
#90536=CARTESIAN_POINT('',(3.,2.5,1.44337567297406));
#90537=CARTESIAN_POINT('Origin',(3.,2.5,-1.44337567297407));
#90538=CARTESIAN_POINT('',(6.,2.5,-1.44337567297407));
#90539=CARTESIAN_POINT('',(6.,2.5,-0.721687836487033));
#90540=CARTESIAN_POINT('',(3.,2.5,-1.44337567297407));
#90541=CARTESIAN_POINT('',(3.,2.5,-1.44337567297407));
#90542=CARTESIAN_POINT('',(3.,2.5,-1.44337567297407));
#90543=CARTESIAN_POINT('Origin',(3.,-5.30287619362453E-16,-2.88675134594813));
#90544=CARTESIAN_POINT('',(6.,-5.30287619362453E-16,-2.88675134594813));
#90545=CARTESIAN_POINT('',(6.,0.625,-2.52590742770461));
#90546=CARTESIAN_POINT('',(3.,-5.30287619362453E-16,-2.88675134594813));
#90547=CARTESIAN_POINT('',(3.,-5.30287619362453E-16,-2.88675134594813));
#90548=CARTESIAN_POINT('',(3.,-5.30287619362453E-16,-2.88675134594813));
#90549=CARTESIAN_POINT('Origin',(3.,-2.5,-1.44337567297406));
#90550=CARTESIAN_POINT('',(6.,-2.5,-1.44337567297406));
#90551=CARTESIAN_POINT('',(6.,-1.875,-1.80421959121758));
#90552=CARTESIAN_POINT('',(3.,-2.5,-1.44337567297406));
#90553=CARTESIAN_POINT('',(3.,-2.5,-1.44337567297406));
#90554=CARTESIAN_POINT('',(3.,-2.5,-1.44337567297406));
#90555=CARTESIAN_POINT('Origin',(3.,-2.5,1.44337567297406));
#90556=CARTESIAN_POINT('',(6.,-2.5,0.721687836487032));
#90557=CARTESIAN_POINT('',(3.,-2.5,1.44337567297406));
#90558=CARTESIAN_POINT('Origin',(3.,0.,0.));
#90559=CARTESIAN_POINT('Origin',(-16.,2.4,0.));
#90560=CARTESIAN_POINT('',(-16.,-2.4,-2.93915231795365E-16));
#90561=CARTESIAN_POINT('Origin',(-16.,0.,0.));
#90562=CARTESIAN_POINT('Origin',(-15.7,0.,0.));
#90563=CARTESIAN_POINT('',(-15.7,-2.7,-3.30654635769785E-16));
#90564=CARTESIAN_POINT('Origin',(2.7,0.,0.));
#90565=CARTESIAN_POINT('Origin',(5.4,0.,0.));
#90566=CARTESIAN_POINT('Origin',(5.4,0.,0.));
#90567=CARTESIAN_POINT('Origin',(5.4,0.,0.));
#90568=CARTESIAN_POINT('Origin',(5.4,0.,0.));
#90569=CARTESIAN_POINT('Origin',(5.4,0.,0.));
#90570=CARTESIAN_POINT('Origin',(5.4,0.,0.));
#90571=CARTESIAN_POINT('Origin',(5.4,0.,0.));
#90572=CARTESIAN_POINT('Origin',(5.4,0.,0.));
#90573=CARTESIAN_POINT('Origin',(5.4,0.,0.));
#90574=CARTESIAN_POINT('Origin',(5.4,0.,0.));
#90575=CARTESIAN_POINT('Origin',(5.4,0.,0.));
#90576=CARTESIAN_POINT('Origin',(5.4,0.,0.));
#90577=CARTESIAN_POINT('Origin',(5.4,0.,0.));
#90578=CARTESIAN_POINT('Origin',(5.4,0.,0.));
#90579=CARTESIAN_POINT('Origin',(5.4,0.,0.));
#90580=CARTESIAN_POINT('Origin',(5.4,0.,0.));
#90581=CARTESIAN_POINT('Origin',(5.4,0.,0.));
#90582=CARTESIAN_POINT('',(2.7,-5.,-6.12323399573677E-16));
#90583=CARTESIAN_POINT('Origin',(5.4,0.,0.));
#90584=CARTESIAN_POINT('Origin',(5.4,0.,0.));
#90585=CARTESIAN_POINT('Origin',(5.4,0.,0.));
#90586=CARTESIAN_POINT('Origin',(5.4,0.,0.));
#90587=CARTESIAN_POINT('Origin',(5.4,0.,0.));
#90588=CARTESIAN_POINT('Origin',(5.4,0.,0.));
#90589=CARTESIAN_POINT('Origin',(5.4,0.,0.));
#90590=CARTESIAN_POINT('Origin',(5.4,0.,0.));
#90591=CARTESIAN_POINT('Origin',(5.4,0.,0.));
#90592=CARTESIAN_POINT('Origin',(5.4,0.,0.));
#90593=CARTESIAN_POINT('Origin',(5.4,0.,0.));
#90594=CARTESIAN_POINT('Origin',(5.4,0.,0.));
#90595=CARTESIAN_POINT('Origin',(5.4,0.,0.));
#90596=CARTESIAN_POINT('Origin',(5.4,0.,0.));
#90597=CARTESIAN_POINT('Origin',(5.4,0.,0.));
#90598=CARTESIAN_POINT('Origin',(5.4,0.,0.));
#90599=CARTESIAN_POINT('Origin',(5.4,0.,0.));
#90600=CARTESIAN_POINT('Origin',(5.4,0.,0.));
#90601=CARTESIAN_POINT('Origin',(5.4,0.,0.));
#90602=CARTESIAN_POINT('Origin',(5.7,0.,0.));
#90603=CARTESIAN_POINT('',(6.,-4.4,-5.38844591624836E-16));
#90604=CARTESIAN_POINT('Origin',(6.,0.,0.));
#90605=CARTESIAN_POINT('',(5.7,-4.7,-5.75583995599256E-16));
#90606=CARTESIAN_POINT('Origin',(6.,0.,0.));
#90607=CARTESIAN_POINT('',(0.,0.,0.));
#90608=CARTESIAN_POINT('Origin',(19.2,0.,0.));
#90609=CARTESIAN_POINT('',(20.,-2.53334006729474E-16,2.06862915010152));
#90610=CARTESIAN_POINT('Origin',(20.,0.,0.));
#90611=CARTESIAN_POINT('',(19.7656854249492,-3.22610491228314E-16,2.63431457505076));
#90612=CARTESIAN_POINT('Origin',(19.2,-2.53334006729474E-16,2.06862915010152));
#90613=CARTESIAN_POINT('',(19.7656854249492,-2.63431457505076,-3.22610491228314E-16));
#90614=CARTESIAN_POINT('Origin',(19.7656854249492,0.,-4.03263114035392E-16));
#90615=CARTESIAN_POINT('Origin',(19.7656854249492,0.,-4.03263114035392E-16));
#90616=CARTESIAN_POINT('Origin',(19.7,0.,0.));
#90617=CARTESIAN_POINT('',(19.4,-3.,-3.67394039744206E-16));
#90618=CARTESIAN_POINT('',(19.7,-2.7,-3.30654635769785E-16));
#90619=CARTESIAN_POINT('Origin',(19.4,0.,0.));
#90620=CARTESIAN_POINT('Origin',(20.,0.,0.));
#90621=CARTESIAN_POINT('Origin',(0.,2.4,0.));
#90622=CARTESIAN_POINT('',(-6.93889390390723E-17,-2.4,-2.93915231795365E-16));
#90623=CARTESIAN_POINT('Origin',(0.,0.,0.));
#90624=CARTESIAN_POINT('Origin',(0.3,0.,0.));
#90625=CARTESIAN_POINT('',(0.6,-3.,-3.67394039744206E-16));
#90626=CARTESIAN_POINT('Origin',(0.600000000000001,0.,0.));
#90627=CARTESIAN_POINT('',(0.3,-2.7,-3.30654635769785E-16));
#90628=CARTESIAN_POINT('Origin',(10.,0.,0.));
#90629=CARTESIAN_POINT('',(10.,-3.,-3.67394039744206E-16));
#90630=CARTESIAN_POINT('',(0.,0.,0.));
#90631=CARTESIAN_POINT('Origin',(-14.6,0.,0.));
#90632=CARTESIAN_POINT('',(-28.862836477965,-3.93726360443606,0.0027323502637925));
#90633=CARTESIAN_POINT('',(-29.046163522035,-3.93671054810784,0.00404045690675457));
#90634=CARTESIAN_POINT('',(-14.6,-3.933,-4.81653586104654E-16));
#90635=CARTESIAN_POINT('',(-29.267,1.75074643530109,3.52538993219839));
#90636=CARTESIAN_POINT('Ctrl Pts',(-28.862836477965,-3.93726360443606,0.0027323502637925));
#90637=CARTESIAN_POINT('Ctrl Pts',(-28.8704880036245,-3.93837525323034,
0.153518646252777));
#90638=CARTESIAN_POINT('Ctrl Pts',(-28.878139529284,-3.93046040114638,0.304180408115829));
#90639=CARTESIAN_POINT('Ctrl Pts',(-28.8857910549435,-3.91312829588934,
0.453742202611319));
#90640=CARTESIAN_POINT('Ctrl Pts',(-28.9517303860892,-3.76376364903901,
1.74263609552425));
#90641=CARTESIAN_POINT('Ctrl Pts',(-29.0176697172349,-2.91501250501241,
2.94983925441235));
#90642=CARTESIAN_POINT('Ctrl Pts',(-29.0836090483806,-1.75273691390075,
3.52758749070468));
#90643=CARTESIAN_POINT('Ctrl Pts',(-29.1447393655871,-0.675227113126593,
4.06320003539346));
#90644=CARTESIAN_POINT('Ctrl Pts',(-29.2058696827935,0.671743512076998,
4.0578230529153));
#90645=CARTESIAN_POINT('Ctrl Pts',(-29.267,1.75279839527107,3.52791786994589));
#90646=CARTESIAN_POINT('',(-29.267,-1.74869447533113,3.52286199445087));
#90647=CARTESIAN_POINT('Origin',(-29.267,0.,0.));
#90648=CARTESIAN_POINT('Ctrl Pts',(-29.267,-1.74869447533113,3.52286199445087));
#90649=CARTESIAN_POINT('Ctrl Pts',(-29.2010606688543,-2.91633732258385,
2.94326205571725));
#90650=CARTESIAN_POINT('Ctrl Pts',(-29.1351213377086,-3.76336534893867,
1.7427628349399));
#90651=CARTESIAN_POINT('Ctrl Pts',(-29.0691820065629,-3.91257791995379,
0.455813760205835));
#90652=CARTESIAN_POINT('Ctrl Pts',(-29.0615091783869,-3.92994058346889,
0.306061875403748));
#90653=CARTESIAN_POINT('Ctrl Pts',(-29.053836350211,-3.9378547559674,0.15513945093785));
#90654=CARTESIAN_POINT('Ctrl Pts',(-29.046163522035,-3.93671054810784,0.00404045690675457));
#90655=CARTESIAN_POINT('Origin',(-14.6,0.,0.));
#90656=CARTESIAN_POINT('',(-27.612836477965,-3.92708773793745,0.00134795691750567));
#90657=CARTESIAN_POINT('',(-27.796163522035,-3.92707419464339,0.00136457270431441));
#90658=CARTESIAN_POINT('',(-14.6,-3.933,-4.81653586104654E-16));
#90659=CARTESIAN_POINT('Ctrl Pts',(-27.612836477965,-3.92708773793745,0.00134795691750567));
#90660=CARTESIAN_POINT('Ctrl Pts',(-27.641518683417,-3.92884446881095,0.570375667339846));
#90661=CARTESIAN_POINT('Ctrl Pts',(-27.6702008888689,-3.81320567258203,
1.13872220665575));
#90662=CARTESIAN_POINT('Ctrl Pts',(-27.6988830943208,-3.57659994969859,
1.65121917528487));
#90663=CARTESIAN_POINT('Ctrl Pts',(-27.7648224254665,-3.03265213026327,
2.82943078046378));
#90664=CARTESIAN_POINT('Ctrl Pts',(-27.8307617566123,-1.84936613535815,
3.71246449188963));
#90665=CARTESIAN_POINT('Ctrl Pts',(-27.896701087758,-0.56506653815142,3.89861757445132));
#90666=CARTESIAN_POINT('Ctrl Pts',(-27.9626404189037,0.719233059055312,
4.08477065701301));
#90667=CARTESIAN_POINT('Ctrl Pts',(-28.0285797500494,2.10454625856366,3.57404311071053));
#90668=CARTESIAN_POINT('Ctrl Pts',(-28.0945190811951,2.960621034551,2.59873220565746));
#90669=CARTESIAN_POINT('Ctrl Pts',(-28.1604584123408,3.81669581053835,1.62342130060439));
#90670=CARTESIAN_POINT('Ctrl Pts',(-28.2263977434865,4.1435321630047,0.183527036800713));
#90671=CARTESIAN_POINT('Ctrl Pts',(-28.2923370746322,3.79245785029125,-1.06577113364283));
#90672=CARTESIAN_POINT('Ctrl Pts',(-28.3582764057779,3.4413835375778,-2.31506930408637));
#90673=CARTESIAN_POINT('Ctrl Pts',(-28.4242157369236,2.41239855968456,-3.37377138116979));
#90674=CARTESIAN_POINT('Ctrl Pts',(-28.4901550680693,1.17359560009141,-3.76043033403215));
#90675=CARTESIAN_POINT('Ctrl Pts',(-28.556094399215,-0.0652073595017287,
-4.14708928689451));
#90676=CARTESIAN_POINT('Ctrl Pts',(-28.6220337303607,-1.51382830079477,
-3.86170511553583));
#90677=CARTESIAN_POINT('Ctrl Pts',(-28.6879730615064,-2.51314969660425,
-3.0337207163876));
#90678=CARTESIAN_POINT('Ctrl Pts',(-28.7462608669926,-3.39651096407671,
-2.30181469361449));
#90679=CARTESIAN_POINT('Ctrl Pts',(-28.8045486724788,-3.92879528431619,
-1.14592775776201));
#90680=CARTESIAN_POINT('Ctrl Pts',(-28.862836477965,-3.93726360443606,0.0027323502637925));
#90681=CARTESIAN_POINT('Ctrl Pts',(-29.046163522035,-3.93671054810784,0.00404045690675457));
#90682=CARTESIAN_POINT('Ctrl Pts',(-28.9878970190653,-3.9280215759169,-1.14338651298282));
#90683=CARTESIAN_POINT('Ctrl Pts',(-28.9296305160955,-3.3969634616774,-2.30099571067004));
#90684=CARTESIAN_POINT('Ctrl Pts',(-28.8713640131258,-2.51437175851888,
-3.0335120984736));
#90685=CARTESIAN_POINT('Ctrl Pts',(-28.8054246819801,-1.51555591039341,
-3.86248995372817));
#90686=CARTESIAN_POINT('Ctrl Pts',(-28.7394853508344,-0.0665270984670233,
-4.14704673554652));
#90687=CARTESIAN_POINT('Ctrl Pts',(-28.6735460196887,1.17251990448456,-3.7604723075278));
#90688=CARTESIAN_POINT('Ctrl Pts',(-28.607606688543,2.41156690743614,-3.37389787950909));
#90689=CARTESIAN_POINT('Ctrl Pts',(-28.5416673573973,3.44063210141293,-2.31619224165332));
#90690=CARTESIAN_POINT('Ctrl Pts',(-28.4757280262516,3.79204558724253,-1.06716650818582));
#90691=CARTESIAN_POINT('Ctrl Pts',(-28.4097886951059,4.14345907307213,0.18185922528169));
#90692=CARTESIAN_POINT('Ctrl Pts',(-28.3438493639602,3.81722085075455,1.62220505436093));
#90693=CARTESIAN_POINT('Ctrl Pts',(-28.2779100328145,2.9614918507157,2.59787371676636));
#90694=CARTESIAN_POINT('Ctrl Pts',(-28.2119707016688,2.10576285067685,3.57354237917179));
#90695=CARTESIAN_POINT('Ctrl Pts',(-28.146031370523,0.720543072916747,4.08453387490342));
#90696=CARTESIAN_POINT('Ctrl Pts',(-28.0800920393773,-0.563833091052422,
3.89875014065244));
#90697=CARTESIAN_POINT('Ctrl Pts',(-28.0141527082316,-1.84820925502159,
3.71296640640145));
#90698=CARTESIAN_POINT('Ctrl Pts',(-27.9482133770859,-3.03174180519982,
2.83040744216786));
#90699=CARTESIAN_POINT('Ctrl Pts',(-27.8822740459403,-3.57605921681971,
1.65239327736364));
#90700=CARTESIAN_POINT('Ctrl Pts',(-27.8535705379718,-3.81300155290831,
1.13960161904887));
#90701=CARTESIAN_POINT('Ctrl Pts',(-27.8248670300034,-3.92882052327039,
0.570824853129742));
#90702=CARTESIAN_POINT('Ctrl Pts',(-27.796163522035,-3.92707419464339,0.00136457270431441));
#90703=CARTESIAN_POINT('Origin',(-14.6,0.,0.));
#90704=CARTESIAN_POINT('',(-26.362836477965,-3.9324910341208,-0.00353437058449479));
#90705=CARTESIAN_POINT('',(-26.546163522035,-3.93250329400039,-0.00353456554338567));
#90706=CARTESIAN_POINT('',(-14.6,-3.933,-4.81653586104654E-16));
#90707=CARTESIAN_POINT('Ctrl Pts',(-26.362836477965,-3.9324910341208,-0.0035343705844948));
#90708=CARTESIAN_POINT('Ctrl Pts',(-26.4125493632094,-3.92366140675108,
0.979300462816973));
#90709=CARTESIAN_POINT('Ctrl Pts',(-26.4622622484538,-3.5499695151475,1.96812479991632));
#90710=CARTESIAN_POINT('Ctrl Pts',(-26.5119751336982,-2.88332081962348,
2.68422145640243));
#90711=CARTESIAN_POINT('Ctrl Pts',(-26.5779144648439,-1.99907584217135,
3.63405436857873));
#90712=CARTESIAN_POINT('Ctrl Pts',(-26.6438537959896,-0.599418628171099,
4.10406506139591));
#90713=CARTESIAN_POINT('Ctrl Pts',(-26.7097931271353,0.678883795085354,
3.8804250807624));
#90714=CARTESIAN_POINT('Ctrl Pts',(-26.775732458281,1.95718621834181,3.65678510012889));
#90715=CARTESIAN_POINT('Ctrl Pts',(-26.8416717894267,3.11413385085448,2.7394944460447));
#90716=CARTESIAN_POINT('Ctrl Pts',(-26.9076111205724,3.62337886308066,1.54586884290443));
#90717=CARTESIAN_POINT('Ctrl Pts',(-26.9735504517181,4.13262387530683,0.352243239764167));
#90718=CARTESIAN_POINT('Ctrl Pts',(-27.0394897828638,3.99416626724652,-1.11771731243217));
#90719=CARTESIAN_POINT('Ctrl Pts',(-27.1054291140095,3.27099705696224,-2.19525935283343));
#90720=CARTESIAN_POINT('Ctrl Pts',(-27.1713684451552,2.54782784667795,-3.27280139323469));
#90721=CARTESIAN_POINT('Ctrl Pts',(-27.2373077763009,1.23994703416969,-3.95792492184086));
#90722=CARTESIAN_POINT('Ctrl Pts',(-27.3032471074466,-0.0576322518721723,
-3.93894051569577));
#90723=CARTESIAN_POINT('Ctrl Pts',(-27.3691864385923,-1.35521153791403,
-3.91995610955068));
#90724=CARTESIAN_POINT('Ctrl Pts',(-27.4351257697381,-2.64248929748948,
-3.19686376865435));
#90725=CARTESIAN_POINT('Ctrl Pts',(-27.5010651008838,-3.33382335529445,
-2.0986228487402));
#90726=CARTESIAN_POINT('Ctrl Pts',(-27.5383222265775,-3.72444181381511,
-1.47809335163534));
#90727=CARTESIAN_POINT('Ctrl Pts',(-27.5755793522713,-3.92480580940606,
-0.737798025631152));
#90728=CARTESIAN_POINT('Ctrl Pts',(-27.612836477965,-3.92708773793745,0.00134795691750567));
#90729=CARTESIAN_POINT('Ctrl Pts',(-27.796163522035,-3.92707419464339,0.00136457270431441));
#90730=CARTESIAN_POINT('Ctrl Pts',(-27.7589276988577,-3.92480875781817,
-0.737371693668906));
#90731=CARTESIAN_POINT('Ctrl Pts',(-27.7216918756804,-3.72469557009487,
-1.4772582297981));
#90732=CARTESIAN_POINT('Ctrl Pts',(-27.6844560525031,-3.33450232419475,
-2.0975649274865));
#90733=CARTESIAN_POINT('Ctrl Pts',(-27.6185167213574,-2.64352574688834,
-3.19603960215757));
#90734=CARTESIAN_POINT('Ctrl Pts',(-27.5525773902117,-1.35647031921396,
-3.91951958612487));
#90735=CARTESIAN_POINT('Ctrl Pts',(-27.486638059066,-0.0588948626118422,
-3.93891465672187));
#90736=CARTESIAN_POINT('Ctrl Pts',(-27.4206987279203,1.23868059399027,-3.95830972731887));
#90737=CARTESIAN_POINT('Ctrl Pts',(-27.3547593967746,2.54677607952012,-3.27361988454557));
#90738=CARTESIAN_POINT('Ctrl Pts',(-27.2888200656289,3.2702900962885,-2.19631348578418));
#90739=CARTESIAN_POINT('Ctrl Pts',(-27.2228807344832,3.99380411305689,-1.11900708702278));
#90740=CARTESIAN_POINT('Ctrl Pts',(-27.1569414033375,4.1327366610638,0.350915867726706));
#90741=CARTESIAN_POINT('Ctrl Pts',(-27.0910020721918,3.62387579505931,1.54470660957893));
#90742=CARTESIAN_POINT('Ctrl Pts',(-27.0250627410461,3.11501492905483,2.73849735143115));
#90743=CARTESIAN_POINT('Ctrl Pts',(-26.9591234099004,1.95836064903894,3.65615588038611));
#90744=CARTESIAN_POINT('Ctrl Pts',(-26.8931840787547,0.680129861679127,
3.8802055933119));
#90745=CARTESIAN_POINT('Ctrl Pts',(-26.827244747609,-0.598100925680689,
4.10425530623768));
#90746=CARTESIAN_POINT('Ctrl Pts',(-26.7613054164633,-1.99790822038444,
3.6346962031343));
#90747=CARTESIAN_POINT('Ctrl Pts',(-26.6953660853176,-2.88245804158793,
2.68514790245118));
#90748=CARTESIAN_POINT('Ctrl Pts',(-26.6456318975567,-3.54962232923244,
1.96895905652796));
#90749=CARTESIAN_POINT('Ctrl Pts',(-26.5958977097959,-3.92366673042445,
0.979713755669241));
#90750=CARTESIAN_POINT('Ctrl Pts',(-26.546163522035,-3.93250329400039,-0.00353456554338567));
#90751=CARTESIAN_POINT('Origin',(-14.6,0.,0.));
#90752=CARTESIAN_POINT('',(-25.112836477965,-3.93848364963218,0.00166216559900585));
#90753=CARTESIAN_POINT('',(-25.296163522035,-3.93847615505153,0.0016688492094424));
#90754=CARTESIAN_POINT('',(-14.6,-3.933,-4.81653586104654E-16));
#90755=CARTESIAN_POINT('Ctrl Pts',(-25.112836477965,-3.93848364963218,0.00166216559900585));
#90756=CARTESIAN_POINT('Ctrl Pts',(-25.1176407118562,-3.93898935420615,
0.0962682400339248));
#90757=CARTESIAN_POINT('Ctrl Pts',(-25.1224449457473,-3.93587384866819,
0.190840450324815));
#90758=CARTESIAN_POINT('Ctrl Pts',(-25.1272491796384,-3.92903008168484,
0.2851420889527));
#90759=CARTESIAN_POINT('Ctrl Pts',(-25.1931885107842,-3.83509764050396,
1.57945604575908));
#90760=CARTESIAN_POINT('Ctrl Pts',(-25.2591278419299,-3.0388256093705,2.82279900881076));
#90761=CARTESIAN_POINT('Ctrl Pts',(-25.3250671730756,-1.90247401912017,
3.44951822876883));
#90762=CARTESIAN_POINT('Ctrl Pts',(-25.3910065042213,-0.76612242886986,
4.0762374487269));
#90763=CARTESIAN_POINT('Ctrl Pts',(-25.456945835367,0.710308720497307,4.08633292559138));
#90764=CARTESIAN_POINT('Ctrl Pts',(-25.5228851665127,1.85512436849494,3.47521178397906));
#90765=CARTESIAN_POINT('Ctrl Pts',(-25.5888244976584,2.99994001649258,2.86409064236673));
#90766=CARTESIAN_POINT('Ctrl Pts',(-25.6547638288041,3.81314016312069,1.63175288227759));
#90767=CARTESIAN_POINT('Ctrl Pts',(-25.7207031599498,3.92476341178622,0.338844461100057));
#90768=CARTESIAN_POINT('Ctrl Pts',(-25.7866424910955,4.03638666045175,-0.954063960077469));
#90769=CARTESIAN_POINT('Ctrl Pts',(-25.8525818222412,3.44643301115472,-2.3075430423434));
#90770=CARTESIAN_POINT('Ctrl Pts',(-25.9185211533869,2.42329897262029,-3.10583411496569));
#90771=CARTESIAN_POINT('Ctrl Pts',(-25.9844604845326,1.40016493408586,-3.90412518758798));
#90772=CARTESIAN_POINT('Ctrl Pts',(-26.0503998156783,-0.0561494936859615,
-4.14722825056663));
#90773=CARTESIAN_POINT('Ctrl Pts',(-26.116339146824,-1.28310126714286,-3.72454484960586));
#90774=CARTESIAN_POINT('Ctrl Pts',(-26.1822784779697,-2.51005304059976,
-3.30186144864509));
#90775=CARTESIAN_POINT('Ctrl Pts',(-26.2482178091154,-3.50764215974172,
-2.21339158374489));
#90776=CARTESIAN_POINT('Ctrl Pts',(-26.3141571402611,-3.82202034886068,
-0.95432908552708));
#90777=CARTESIAN_POINT('Ctrl Pts',(-26.3303835861624,-3.8993829879663,-0.644497166417136));
#90778=CARTESIAN_POINT('Ctrl Pts',(-26.3466100320637,-3.93537305294025,
-0.32433482655703));
#90779=CARTESIAN_POINT('Ctrl Pts',(-26.362836477965,-3.9324910341208,-0.0035343705844948));
#90780=CARTESIAN_POINT('Ctrl Pts',(-26.546163522035,-3.93250329400039,-0.00353456554338567));
#90781=CARTESIAN_POINT('Ctrl Pts',(-26.5299583786502,-3.93538255645996,
-0.32391136760875));
#90782=CARTESIAN_POINT('Ctrl Pts',(-26.5137532352653,-3.89948824923301,
-0.643651479317923));
#90783=CARTESIAN_POINT('Ctrl Pts',(-26.4975480918805,-3.82232660328557,
-0.953101486990109));
#90784=CARTESIAN_POINT('Ctrl Pts',(-26.4316087607348,-3.50835299607651,
-2.21226507748542));
#90785=CARTESIAN_POINT('Ctrl Pts',(-26.3656694295891,-2.51111343395517,
-3.30105476021319));
#90786=CARTESIAN_POINT('Ctrl Pts',(-26.2997300984434,-1.28429752491345,
-3.72413212926964));
#90787=CARTESIAN_POINT('Ctrl Pts',(-26.2337907672977,-0.0574816158717277,
-4.14720949832609));
#90788=CARTESIAN_POINT('Ctrl Pts',(-26.167851436152,1.39891064009036,-3.90457455371123));
#90789=CARTESIAN_POINT('Ctrl Pts',(-26.1019121050063,2.42230098071725,-3.10661229877343));
#90790=CARTESIAN_POINT('Ctrl Pts',(-26.0359727738606,3.44569132134414,-2.30865004383564));
#90791=CARTESIAN_POINT('Ctrl Pts',(-25.9700334427149,4.03607974663582,-0.955360478574905));
#90792=CARTESIAN_POINT('Ctrl Pts',(-25.9040941115692,3.92487185002737,0.33758369389623));
#90793=CARTESIAN_POINT('Ctrl Pts',(-25.8381547804235,3.81366395341891,1.63052786636736));
#90794=CARTESIAN_POINT('Ctrl Pts',(-25.7722154492778,3.00085973491032,2.86312664604889));
#90795=CARTESIAN_POINT('Ctrl Pts',(-25.7062761181321,1.85624051708109,3.47461545772335));
#90796=CARTESIAN_POINT('Ctrl Pts',(-25.6403367869864,0.71162129925185,4.08610426939782));
#90797=CARTESIAN_POINT('Ctrl Pts',(-25.5743974558406,-0.764812917898037,
4.07648311306521));
#90798=CARTESIAN_POINT('Ctrl Pts',(-25.5084581246949,-1.90136570512696,
3.45012900550375));
#90799=CARTESIAN_POINT('Ctrl Pts',(-25.4425187935492,-3.03791849235588,
2.82377489794229));
#90800=CARTESIAN_POINT('Ctrl Pts',(-25.3765794624036,-3.83458984966384,
1.58068783915199));
#90801=CARTESIAN_POINT('Ctrl Pts',(-25.3106401312579,-3.92893806068268,
0.286404192041365));
#90802=CARTESIAN_POINT('Ctrl Pts',(-25.3058145948502,-3.93584260034595,
0.191686627389066));
#90803=CARTESIAN_POINT('Ctrl Pts',(-25.3009890584426,-3.93898583025972,
0.0966948780857186));
#90804=CARTESIAN_POINT('Ctrl Pts',(-25.296163522035,-3.93847615505153,0.0016688492094424));
#90805=CARTESIAN_POINT('Origin',(-14.6,0.,0.));
#90806=CARTESIAN_POINT('',(-23.862836477965,-3.92784938859273,0.00213917922607304));
#90807=CARTESIAN_POINT('',(-24.046163522035,-3.92784218437645,0.00213368844150495));
#90808=CARTESIAN_POINT('',(-14.6,-3.933,-4.81653586104654E-16));
#90809=CARTESIAN_POINT('Ctrl Pts',(-23.862836477965,-3.92784938859273,0.00213917922607304));
#90810=CARTESIAN_POINT('Ctrl Pts',(-23.8886713916486,-3.93039759682621,
0.514429414290928));
#90811=CARTESIAN_POINT('Ctrl Pts',(-23.9145063053322,-3.83728702899802,
1.02582969131807));
#90812=CARTESIAN_POINT('Ctrl Pts',(-23.9403412190158,-3.6441795653241,1.4961746851344));
#90813=CARTESIAN_POINT('Ctrl Pts',(-24.0062805501615,-3.15130480097032,
2.69665225126127));
#90814=CARTESIAN_POINT('Ctrl Pts',(-24.0722198813072,-2.00700932293093,
3.62967889640143));
#90815=CARTESIAN_POINT('Ctrl Pts',(-24.1381592124529,-0.731884709970319,
3.8707787542536));
#90816=CARTESIAN_POINT('Ctrl Pts',(-24.2040985435986,0.543239902990295,
4.11187861210578));
#90817=CARTESIAN_POINT('Ctrl Pts',(-24.2700378747443,1.94919365087213,3.66105168266996));
#90818=CARTESIAN_POINT('Ctrl Pts',(-24.33597720589,2.84634481683359,2.72339945215828));
#90819=CARTESIAN_POINT('Ctrl Pts',(-24.4019165370357,3.74349598279505,1.7857472216466));
#90820=CARTESIAN_POINT('Ctrl Pts',(-24.4678558681814,4.13184456683614,0.361269690059079));
#90821=CARTESIAN_POINT('Ctrl Pts',(-24.5337951993271,3.83471329770221,-0.901974122230396));
#90822=CARTESIAN_POINT('Ctrl Pts',(-24.5997345304728,3.53758202856828,-2.16521793451989));
#90823=CARTESIAN_POINT('Ctrl Pts',(-24.6656738616185,2.55497090625931,-3.26722802751132));
#90824=CARTESIAN_POINT('Ctrl Pts',(-24.7316131927642,1.33391401022604,-3.70665034875255));
#90825=CARTESIAN_POINT('Ctrl Pts',(-24.7975525239099,0.112857114192773,
-4.14607266999378));
#90826=CARTESIAN_POINT('Ctrl Pts',(-24.8634918550556,-1.3466455555648,-3.9229072194848));
#90827=CARTESIAN_POINT('Ctrl Pts',(-24.9294311862013,-2.38060046482942,
-3.13868201894977));
#90828=CARTESIAN_POINT('Ctrl Pts',(-24.9905662834559,-3.33922307801683,
-2.41159420851614));
#90829=CARTESIAN_POINT('Ctrl Pts',(-25.0517013807105,-3.93204843040415,
-1.20222417559595));
#90830=CARTESIAN_POINT('Ctrl Pts',(-25.112836477965,-3.93848364963218,0.00166216559900585));
#90831=CARTESIAN_POINT('Ctrl Pts',(-25.296163522035,-3.93847615505153,0.0016688492094424));
#90832=CARTESIAN_POINT('Ctrl Pts',(-25.2350497272969,-3.9320212900531,-1.20180382884279));
#90833=CARTESIAN_POINT('Ctrl Pts',(-25.1739359325588,-3.33966345243659,
-2.41077473447204));
#90834=CARTESIAN_POINT('Ctrl Pts',(-25.1128221378207,-2.3816084582775,-3.13791694536259));
#90835=CARTESIAN_POINT('Ctrl Pts',(-25.046882806675,-1.34790558012376,-3.92247420022496));
#90836=CARTESIAN_POINT('Ctrl Pts',(-24.9809434755293,0.111525240913435,
-4.14610847451873));
#90837=CARTESIAN_POINT('Ctrl Pts',(-24.9150041443836,1.33272316167415,-3.70707844764346));
#90838=CARTESIAN_POINT('Ctrl Pts',(-24.8490648132379,2.55392108243488,-3.26804842076819));
#90839=CARTESIAN_POINT('Ctrl Pts',(-24.7831254820922,3.53688610291912,-2.16635409272388));
#90840=CARTESIAN_POINT('Ctrl Pts',(-24.7171861509465,3.83442313744424,-0.903205865383198));
#90841=CARTESIAN_POINT('Ctrl Pts',(-24.6512468198008,4.13196017196935,0.359942361957476));
#90842=CARTESIAN_POINT('Ctrl Pts',(-24.5853074886551,3.74406922053537,1.78454448859452));
#90843=CARTESIAN_POINT('Ctrl Pts',(-24.5193681575094,2.84721935774838,2.72248481292816));
#90844=CARTESIAN_POINT('Ctrl Pts',(-24.4534288263637,1.9503694949614,3.66042513726181));
#90845=CARTESIAN_POINT('Ctrl Pts',(-24.387489495218,0.544560720821429,4.11170365929207));
#90846=CARTESIAN_POINT('Ctrl Pts',(-24.3215501640723,-0.73064120346497,
3.87101344158701));
#90847=CARTESIAN_POINT('Ctrl Pts',(-24.2556108329266,-2.00584312775137,
3.63032322388195));
#90848=CARTESIAN_POINT('Ctrl Pts',(-24.1896715017809,-3.1504382021842,2.69766426644156));
#90849=CARTESIAN_POINT('Ctrl Pts',(-24.1237321706352,-3.64369854781322,
1.49734515859372));
#90850=CARTESIAN_POINT('Ctrl Pts',(-24.0978759544351,-3.83711643540636,
1.02667447051812));
#90851=CARTESIAN_POINT('Ctrl Pts',(-24.072019738235,-3.93038567262406,0.514848595044744));
#90852=CARTESIAN_POINT('Ctrl Pts',(-24.046163522035,-3.92784218437645,0.00213368844150495));
#90853=CARTESIAN_POINT('Origin',(-14.6,0.,0.));
#90854=CARTESIAN_POINT('',(-22.612836477965,-3.93087436129151,-0.00338089423011334));
#90855=CARTESIAN_POINT('',(-22.796163522035,-3.93088572622165,-0.00338294474049346));
#90856=CARTESIAN_POINT('',(-14.6,-3.933,-4.81653586104654E-16));
#90857=CARTESIAN_POINT('Ctrl Pts',(-22.612836477965,-3.93087436129151,-0.00338089423011334));
#90858=CARTESIAN_POINT('Ctrl Pts',(-22.6597020714411,-3.92317635965085,
0.924132377966204));
#90859=CARTESIAN_POINT('Ctrl Pts',(-22.7065676649171,-3.59478909080291,
1.85655093763582));
#90860=CARTESIAN_POINT('Ctrl Pts',(-22.7534332583932,-2.99587824469287,
2.55798689124243));
#90861=CARTESIAN_POINT('Ctrl Pts',(-22.8193725895389,-2.15321782626481,
3.54489891329993));
#90862=CARTESIAN_POINT('Ctrl Pts',(-22.8853119206846,-0.77502475658801,
4.07455420132641));
#90863=CARTESIAN_POINT('Ctrl Pts',(-22.9512512518303,0.511698830953477,
3.90598869675791));
#90864=CARTESIAN_POINT('Ctrl Pts',(-23.017190582976,1.79842241849496,3.7374231921894));
#90865=CARTESIAN_POINT('Ctrl Pts',(-23.0831299141217,2.99367652390115,2.87063689502596));
#90866=CARTESIAN_POINT('Ctrl Pts',(-23.1490692452674,3.55368619247757,1.69996995214067));
#90867=CARTESIAN_POINT('Ctrl Pts',(-23.2150085764131,4.11369586105398,0.529303009255378));
#90868=CARTESIAN_POINT('Ctrl Pts',(-23.2809479075588,4.03846109280059,-0.945244579351747));
#90869=CARTESIAN_POINT('Ctrl Pts',(-23.3468872387045,3.36220957412427,-2.05283466758846));
#90870=CARTESIAN_POINT('Ctrl Pts',(-23.4128265698502,2.68595805544795,-3.16042475582517));
#90871=CARTESIAN_POINT('Ctrl Pts',(-23.4787659009959,1.40868978634868,-3.90105734369146));
#90872=CARTESIAN_POINT('Ctrl Pts',(-23.5447052321416,0.111491660421779,
-3.93778529156826));
#90873=CARTESIAN_POINT('Ctrl Pts',(-23.6106445632873,-1.18570646550513,
-3.97451323944505));
#90874=CARTESIAN_POINT('Ctrl Pts',(-23.676583894433,-2.50283444825967,-3.30733654733236));
#90875=CARTESIAN_POINT('Ctrl Pts',(-23.7425232255787,-3.24067141430286,
-2.23978395771922));
#90876=CARTESIAN_POINT('Ctrl Pts',(-23.7826276430408,-3.68942515794924,
-1.59049659048769));
#90877=CARTESIAN_POINT('Ctrl Pts',(-23.8227320605029,-3.92389371805991,
-0.793106421375654));
#90878=CARTESIAN_POINT('Ctrl Pts',(-23.862836477965,-3.92784938859273,0.00213917922607304));
#90879=CARTESIAN_POINT('Ctrl Pts',(-24.046163522035,-3.92784218437645,0.00213368844150495));
#90880=CARTESIAN_POINT('Ctrl Pts',(-24.0060804070893,-3.92389918935342,
-0.792692993726209));
#90881=CARTESIAN_POINT('Ctrl Pts',(-23.9659972921437,-3.68969742380163,
-1.58965621061758));
#90882=CARTESIAN_POINT('Ctrl Pts',(-23.9259141771981,-3.24139055871715,
-2.23874269998632));
#90883=CARTESIAN_POINT('Ctrl Pts',(-23.8599748460524,-2.50389660716684,
-3.30653219246322));
#90884=CARTESIAN_POINT('Ctrl Pts',(-23.7940355149067,-1.18698308724101,
-3.97413191916171));
#90885=CARTESIAN_POINT('Ctrl Pts',(-23.728096183761,0.110226696404494,-3.93782067989699));
#90886=CARTESIAN_POINT('Ctrl Pts',(-23.6621568526153,1.40743648004999,-3.90150944063227));
#90887=CARTESIAN_POINT('Ctrl Pts',(-23.5962175214696,2.68494252741516,-3.16128723540433));
#90888=CARTESIAN_POINT('Ctrl Pts',(-23.5302781903239,3.36154976881573,-2.05391450238099));
#90889=CARTESIAN_POINT('Ctrl Pts',(-23.4643388591782,4.03815701021631,-0.946541769357638));
#90890=CARTESIAN_POINT('Ctrl Pts',(-23.3983995280325,4.1138654456523,0.52798149146113));
#90891=CARTESIAN_POINT('Ctrl Pts',(-23.3324601968868,3.55423189619171,1.69882820184466));
#90892=CARTESIAN_POINT('Ctrl Pts',(-23.2665208657411,2.99459834673113,2.8696749122282));
#90893=CARTESIAN_POINT('Ctrl Pts',(-23.2005815345954,1.79962281237397,3.73684507217651));
#90894=CARTESIAN_POINT('Ctrl Pts',(-23.1346422034497,0.512953513280088,
3.90582389830908));
#90895=CARTESIAN_POINT('Ctrl Pts',(-23.068702872304,-0.773715785813794,
4.07480272444165));
#90896=CARTESIAN_POINT('Ctrl Pts',(-23.0027635411583,-2.15207884964439,
3.54559021675848));
#90897=CARTESIAN_POINT('Ctrl Pts',(-22.9368242100126,-2.99505620682083,
2.55894899310702));
#90898=CARTESIAN_POINT('Ctrl Pts',(-22.88993731402,-3.59446464762908,1.8573867595887));
#90899=CARTESIAN_POINT('Ctrl Pts',(-22.8430504180275,-3.92317782141207,
0.92454493291896));
#90900=CARTESIAN_POINT('Ctrl Pts',(-22.796163522035,-3.93088572622165,-0.00338294474049346));
#90901=CARTESIAN_POINT('Origin',(-14.6,0.,0.));
#90902=CARTESIAN_POINT('',(-21.362836477965,-3.9392053084022,0.000704079325613109));
#90903=CARTESIAN_POINT('',(-21.546163522035,-3.9392017186225,0.000711618128540299));
#90904=CARTESIAN_POINT('',(-14.6,-3.933,-4.81653586104654E-16));
#90905=CARTESIAN_POINT('Ctrl Pts',(-21.362836477965,-3.9392053084022,0.000704079325613109));
#90906=CARTESIAN_POINT('Ctrl Pts',(-21.3647934200878,-3.93930094846521,
0.0392218073737966));
#90907=CARTESIAN_POINT('Ctrl Pts',(-21.3667503622106,-3.93878454105988,
0.0777369080014598));
#90908=CARTESIAN_POINT('Ctrl Pts',(-21.3687073043334,-3.93764817090949,
0.116233708220938));
#90909=CARTESIAN_POINT('Ctrl Pts',(-21.4346466354791,-3.89935808211342,
1.41338666341404));
#90910=CARTESIAN_POINT('Ctrl Pts',(-21.5005859666248,-3.1571878645482,2.68976209000154));
#90911=CARTESIAN_POINT('Ctrl Pts',(-21.5665252977705,-2.04878419485562,
3.36467928868465));
#90912=CARTESIAN_POINT('Ctrl Pts',(-21.6324646289162,-0.940380525163057,
4.03959648736776));
#90913=CARTESIAN_POINT('Ctrl Pts',(-21.6984039600619,0.534256596656856,
4.1130554581465));
#90914=CARTESIAN_POINT('Ctrl Pts',(-21.7643432912076,1.70424829180925,3.55163640490676));
#90915=CARTESIAN_POINT('Ctrl Pts',(-21.8302826223533,2.87423998696165,2.99021735166702));
#90916=CARTESIAN_POINT('Ctrl Pts',(-21.896221953499,3.73958625544654,1.7939202744088));
#90917=CARTESIAN_POINT('Ctrl Pts',(-21.9621612846447,3.90660208433412,0.506994622722924));
#90918=CARTESIAN_POINT('Ctrl Pts',(-22.0281006157904,4.07361791322169,-0.77993102896295));
#90919=CARTESIAN_POINT('Ctrl Pts',(-22.0940399469361,3.54230330251196,-2.15748525507647));
#90920=CARTESIAN_POINT('Ctrl Pts',(-22.1599792780818,2.55437721142949,-2.99895656095968));
#90921=CARTESIAN_POINT('Ctrl Pts',(-22.2259186092275,1.56645112034702,-3.84042786684288));
#90922=CARTESIAN_POINT('Ctrl Pts',(-22.2918579403732,0.121913548891806,
-4.14581625249578));
#90923=CARTESIAN_POINT('Ctrl Pts',(-22.357797271519,-1.1220502659885,-3.7761867794628));
#90924=CARTESIAN_POINT('Ctrl Pts',(-22.4237366026647,-2.36601408086881,
-3.40655730642983));
#90925=CARTESIAN_POINT('Ctrl Pts',(-22.4896759338103,-3.40940413917422,
-2.36190997471099));
#90926=CARTESIAN_POINT('Ctrl Pts',(-22.555615264956,-3.77753528473724,-1.1175019308073));
#90927=CARTESIAN_POINT('Ctrl Pts',(-22.5746890026257,-3.88402160749027,
-0.757542068142264));
#90928=CARTESIAN_POINT('Ctrl Pts',(-22.5937627402954,-3.93400735616011,
-0.380867735361056));
#90929=CARTESIAN_POINT('Ctrl Pts',(-22.612836477965,-3.93087436129151,-0.00338089423011334));
#90930=CARTESIAN_POINT('Ctrl Pts',(-22.796163522035,-3.93088572622165,-0.00338294474049346));
#90931=CARTESIAN_POINT('Ctrl Pts',(-22.7771110868818,-3.93401782429389,
-0.380445348674258));
#90932=CARTESIAN_POINT('Ctrl Pts',(-22.7580586517286,-3.88414573503703,
-0.756696364450129));
#90933=CARTESIAN_POINT('Ctrl Pts',(-22.7390062165754,-3.77789385546023,
-1.11628833560879));
#90934=CARTESIAN_POINT('Ctrl Pts',(-22.6730668854297,-3.41016249640089,
-2.36081450105337));
#90935=CARTESIAN_POINT('Ctrl Pts',(-22.6071275542841,-2.36710812775992,
-3.40579689232276));
#90936=CARTESIAN_POINT('Ctrl Pts',(-22.5411882231384,-1.12326318534757,
-3.77582592922345));
#90937=CARTESIAN_POINT('Ctrl Pts',(-22.4752488919926,0.120581757064785,
-4.14585496612414));
#90938=CARTESIAN_POINT('Ctrl Pts',(-22.4093095608469,1.56521727324854,-3.84093064865612));
#90939=CARTESIAN_POINT('Ctrl Pts',(-22.3433702297012,2.55341356678447,-2.99977678974731));
#90940=CARTESIAN_POINT('Ctrl Pts',(-22.2774308985555,3.54160986032041,-2.1586229308385));
#90941=CARTESIAN_POINT('Ctrl Pts',(-22.2114915674098,4.07336693120854,-0.781239530488878));
#90942=CARTESIAN_POINT('Ctrl Pts',(-22.1455522362641,3.90676452515084,0.505739632982661));
#90943=CARTESIAN_POINT('Ctrl Pts',(-22.0796129051184,3.74016211909313,1.79271879645421));
#90944=CARTESIAN_POINT('Ctrl Pts',(-22.0136735739727,2.87520023608961,2.98929372304766));
#90945=CARTESIAN_POINT('Ctrl Pts',(-21.947734242827,1.70538901479264,3.55108855698822));
#90946=CARTESIAN_POINT('Ctrl Pts',(-21.8817949116813,0.535577793495685,
4.11288339092877));
#90947=CARTESIAN_POINT('Ctrl Pts',(-21.8158555805356,-0.939082766094701,
4.03989813221641));
#90948=CARTESIAN_POINT('Ctrl Pts',(-21.7499162493899,-2.04770312228556,
3.36533706399953));
#90949=CARTESIAN_POINT('Ctrl Pts',(-21.6839769182442,-3.15632347847641,
2.69077599578264));
#90950=CARTESIAN_POINT('Ctrl Pts',(-21.6180375870985,-3.89890363126774,
1.41463911806121));
#90951=CARTESIAN_POINT('Ctrl Pts',(-21.5520982559528,-3.93761040601042,
0.117498603504866));
#90952=CARTESIAN_POINT('Ctrl Pts',(-21.5501200113135,-3.93877164723486,
0.0785831152110228));
#90953=CARTESIAN_POINT('Ctrl Pts',(-21.5481417666742,-3.93929936097659,
0.0396487224073827));
#90954=CARTESIAN_POINT('Ctrl Pts',(-21.546163522035,-3.9392017186225,0.000711618128540299));
#90955=CARTESIAN_POINT('Origin',(-14.6,0.,0.));
#90956=CARTESIAN_POINT('',(-20.112836477965,-3.9289412454305,0.00279384190022436));
#90957=CARTESIAN_POINT('',(-20.296163522035,-3.92893175430004,0.00278958524027692));
#90958=CARTESIAN_POINT('',(-14.6,-3.933,-4.81653586104654E-16));
#90959=CARTESIAN_POINT('Ctrl Pts',(-20.112836477965,-3.9289412454305,0.00279384190022436));
#90960=CARTESIAN_POINT('Ctrl Pts',(-20.1358240998803,-3.93195496054311,
0.458305859925948));
#90961=CARTESIAN_POINT('Ctrl Pts',(-20.1588117217955,-3.85874422505227,
0.912879494791886));
#90962=CARTESIAN_POINT('Ctrl Pts',(-20.1817993437108,-3.70504127758559,
1.33837682443348));
#90963=CARTESIAN_POINT('Ctrl Pts',(-20.2477386748565,-3.26414880125882,
2.55890365510319));
#90964=CARTESIAN_POINT('Ctrl Pts',(-20.3136780060022,-2.16095618577067,
3.54018695495582));
#90965=CARTESIAN_POINT('Ctrl Pts',(-20.3796173371479,-0.897355465454369,
3.83579673098208));
#90966=CARTESIAN_POINT('Ctrl Pts',(-20.4455566682936,0.366245254861932,
4.13140650700835));
#90967=CARTESIAN_POINT('Ctrl Pts',(-20.5114959994393,1.79025408000638,3.7413427592083));
#90968=CARTESIAN_POINT('Ctrl Pts',(-20.577435330585,2.72682522482214,2.84306306403276));
#90969=CARTESIAN_POINT('Ctrl Pts',(-20.6433746617307,3.66339636963791,1.94478336885722));
#90970=CARTESIAN_POINT('Ctrl Pts',(-20.7093139928764,4.11252983412497,0.538287726306191));
#90971=CARTESIAN_POINT('Ctrl Pts',(-20.7752533240221,3.86989456583263,-0.736545614427758));
#90972=CARTESIAN_POINT('Ctrl Pts',(-20.8411926551678,3.62725929754029,-2.0113789551617));
#90973=CARTESIAN_POINT('Ctrl Pts',(-20.9071319863135,2.69285529646856,-3.15454999407856));
#90974=CARTESIAN_POINT('Ctrl Pts',(-20.9730713174592,1.49178505007331,-3.64597871046602));
#90975=CARTESIAN_POINT('Ctrl Pts',(-21.0390106486049,0.290714803678051,
-4.13740742685348));
#90976=CARTESIAN_POINT('Ctrl Pts',(-21.1049499797506,-1.17702168804074,
-3.97709382071151));
#90977=CARTESIAN_POINT('Ctrl Pts',(-21.1708893108963,-2.24368495388664,
-3.23797177574116));
#90978=CARTESIAN_POINT('Ctrl Pts',(-21.2348716999192,-3.27869187382335,
-2.52078533488684));
#90979=CARTESIAN_POINT('Ctrl Pts',(-21.2988540889421,-3.93607834841387,
-1.25863631278614));
#90980=CARTESIAN_POINT('Ctrl Pts',(-21.362836477965,-3.9392053084022,0.000704079325613109));
#90981=CARTESIAN_POINT('Ctrl Pts',(-21.546163522035,-3.9392017186225,0.000711618128540299));
#90982=CARTESIAN_POINT('Ctrl Pts',(-21.4822024355285,-3.93604472229705,
-1.25821230141494));
#90983=CARTESIAN_POINT('Ctrl Pts',(-21.4182413490221,-3.27915675941927,
-2.51997072647733));
#90984=CARTESIAN_POINT('Ctrl Pts',(-21.3542802625157,-2.24472485856745,
-3.23725067621843));
#90985=CARTESIAN_POINT('Ctrl Pts',(-21.28834093137,-1.17829913968773,-3.97671528999414));
#90986=CARTESIAN_POINT('Ctrl Pts',(-21.2224016002243,0.289385694765753,
-4.13750036615427));
#90987=CARTESIAN_POINT('Ctrl Pts',(-21.1564622690786,1.49061367481441,-3.64645752804053));
#90988=CARTESIAN_POINT('Ctrl Pts',(-21.0905229379329,2.69184165486307,-3.15541468992679));
#90989=CARTESIAN_POINT('Ctrl Pts',(-21.0245836067872,3.6266127805069,-2.0125439375392));
#90990=CARTESIAN_POINT('Ctrl Pts',(-20.9586442756415,3.86965754277835,-0.737788677715975));
#90991=CARTESIAN_POINT('Ctrl Pts',(-20.8927049444958,4.11270230504979,0.536966582107239));
#90992=CARTESIAN_POINT('Ctrl Pts',(-20.8267656133501,3.66402070394882,1.94360634936608));
#90993=CARTESIAN_POINT('Ctrl Pts',(-20.7608262822044,2.72773821890935,2.84218680604363));
#90994=CARTESIAN_POINT('Ctrl Pts',(-20.6948869510587,1.79145573386986,3.74076726272119));
#90995=CARTESIAN_POINT('Ctrl Pts',(-20.628947619913,0.367572364891867,4.13128840881747));
#90996=CARTESIAN_POINT('Ctrl Pts',(-20.5630082887673,-0.89612317853138,
3.83608457678478));
#90997=CARTESIAN_POINT('Ctrl Pts',(-20.4970689576216,-2.15981872195464,
3.54088074475208));
#90998=CARTESIAN_POINT('Ctrl Pts',(-20.4311296264759,-3.26332643982314,
2.55995193459039));
#90999=CARTESIAN_POINT('Ctrl Pts',(-20.3651902953302,-3.70461094353127,
1.33956686597407));
#91000=CARTESIAN_POINT('Ctrl Pts',(-20.3421813708984,-3.85859312112231,
0.913724696611549));
#91001=CARTESIAN_POINT('Ctrl Pts',(-20.3191724464667,-3.93194320050247,
0.458726405663346));
#91002=CARTESIAN_POINT('Ctrl Pts',(-20.296163522035,-3.92893175430004,0.00278958524027692));
#91003=CARTESIAN_POINT('Origin',(-14.6,0.,0.));
#91004=CARTESIAN_POINT('',(-18.862836477965,-3.92942440079457,-0.0029931669997546));
#91005=CARTESIAN_POINT('',(-19.046163522035,-3.92943419637598,-0.00299686489160711));
#91006=CARTESIAN_POINT('',(-14.6,-3.933,-4.81653586104654E-16));
#91007=CARTESIAN_POINT('Ctrl Pts',(-18.862836477965,-3.92942440079457,-0.0029931669997546));
#91008=CARTESIAN_POINT('Ctrl Pts',(-18.9068547796727,-3.92319085932645,
0.868982802255619));
#91009=CARTESIAN_POINT('Ctrl Pts',(-18.9508730813804,-3.63664096818252,
1.74467880622105));
#91010=CARTESIAN_POINT('Ctrl Pts',(-18.9948913830881,-3.10291356106906,
2.42703745857526));
#91011=CARTESIAN_POINT('Ctrl Pts',(-19.0608307142338,-2.30339093357437,
3.44920940506477));
#91012=CARTESIAN_POINT('Ctrl Pts',(-19.1267700453795,-0.949202398378664,
4.03753267723891));
#91013=CARTESIAN_POINT('Ctrl Pts',(-19.1927093765252,0.343570655594563,
3.92435250677204));
#91014=CARTESIAN_POINT('Ctrl Pts',(-19.2586487076709,1.63634370956779,3.81117233630516));
#91015=CARTESIAN_POINT('Ctrl Pts',(-19.3245880388166,2.86770128231855,2.99648872319727));
#91016=CARTESIAN_POINT('Ctrl Pts',(-19.3905273699623,3.47744332491339,1.85093795541854));
#91017=CARTESIAN_POINT('Ctrl Pts',(-19.456466701108,4.08718536750824,0.7053871876398));
#91018=CARTESIAN_POINT('Ctrl Pts',(-19.5224060322537,4.07531187994718,-0.771030734809761));
#91019=CARTESIAN_POINT('Ctrl Pts',(-19.5883453633994,3.44722464678077,-1.90662676668006));
#91020=CARTESIAN_POINT('Ctrl Pts',(-19.6542846945451,2.81913741361437,-3.04222279855036));
#91021=CARTESIAN_POINT('Ctrl Pts',(-19.7202240256909,1.57483643484262,-3.83699693984138));
#91022=CARTESIAN_POINT('Ctrl Pts',(-19.7861633568366,0.280410298071069,
-3.92937061849978));
#91023=CARTESIAN_POINT('Ctrl Pts',(-19.8521026879823,-1.01401583870047,
-4.02174429715819));
#91024=CARTESIAN_POINT('Ctrl Pts',(-19.9180420191279,-2.35856713347181,
-3.411717513184));
#91025=CARTESIAN_POINT('Ctrl Pts',(-19.9839813502736,-3.14154661227478,
-2.37681894045351));
#91026=CARTESIAN_POINT('Ctrl Pts',(-20.0269330595041,-3.6515655391069,-1.70270438990228));
#91027=CARTESIAN_POINT('Ctrl Pts',(-20.0698847687346,-3.92331020557359,
-0.848317239591968));
#91028=CARTESIAN_POINT('Ctrl Pts',(-20.112836477965,-3.9289412454305,0.00279384190022436));
#91029=CARTESIAN_POINT('Ctrl Pts',(-20.296163522035,-3.92893175430004,0.00278958524027692));
#91030=CARTESIAN_POINT('Ctrl Pts',(-20.253233115321,-3.9233129514459,-0.847904378952598));
#91031=CARTESIAN_POINT('Ctrl Pts',(-20.210302708607,-3.6518592668377,-1.70186561511352));
#91032=CARTESIAN_POINT('Ctrl Pts',(-20.167372301893,-3.14230978779631,-2.37580951022315));
#91033=CARTESIAN_POINT('Ctrl Pts',(-20.1014329707473,-2.35966283880543,
-3.41095949073314));
#91034=CARTESIAN_POINT('Ctrl Pts',(-20.0354936396016,-1.01530765127591,
-4.02141812468219));
#91035=CARTESIAN_POINT('Ctrl Pts',(-19.9695543084559,0.279148018845661,
-3.92946027017984));
#91036=CARTESIAN_POINT('Ctrl Pts',(-19.9036149773102,1.57360368896723,-3.83750241567748));
#91037=CARTESIAN_POINT('Ctrl Pts',(-19.8376756461645,2.81815984168083,-3.04312807272373));
#91038=CARTESIAN_POINT('Ctrl Pts',(-19.7717363150188,3.4466117992558,-1.90773392709203));
#91039=CARTESIAN_POINT('Ctrl Pts',(-19.7057969838731,4.07506375683076,-0.772339781460326));
#91040=CARTESIAN_POINT('Ctrl Pts',(-19.6398576527274,4.08741151926708,0.704074166849339));
#91041=CARTESIAN_POINT('Ctrl Pts',(-19.5739183215817,3.47803753300102,1.84982068060216));
#91042=CARTESIAN_POINT('Ctrl Pts',(-19.507978990436,2.86866354673495,2.99556719435499));
#91043=CARTESIAN_POINT('Ctrl Pts',(-19.4420396592903,1.63756781176651,3.81064627355099));
#91044=CARTESIAN_POINT('Ctrl Pts',(-19.3761003281446,0.34483125522266,3.92424171487547));
#91045=CARTESIAN_POINT('Ctrl Pts',(-19.3101609969989,-0.947905301321183,
4.03783715619996));
#91046=CARTESIAN_POINT('Ctrl Pts',(-19.2442216658532,-2.30228267944042,
3.44994895965294));
#91047=CARTESIAN_POINT('Ctrl Pts',(-19.1782823347075,-3.10213357705578,
2.42803395805132));
#91048=CARTESIAN_POINT('Ctrl Pts',(-19.1342427304833,-3.63633852510867,
1.7455166889295));
#91049=CARTESIAN_POINT('Ctrl Pts',(-19.0902031262592,-3.92318885129781,
0.869395435115258));
#91050=CARTESIAN_POINT('Ctrl Pts',(-19.046163522035,-3.92943419637598,-0.00299686489160711));
#91051=CARTESIAN_POINT('Origin',(-14.6,0.,0.));
#91052=CARTESIAN_POINT('',(-17.612836477965,-3.93932967304405,-0.000322413107344821));
#91053=CARTESIAN_POINT('',(-17.796163522035,-3.93933102250188,-0.000314724560625571));
#91054=CARTESIAN_POINT('',(-14.6,-3.933,-4.81653586104654E-16));
#91055=CARTESIAN_POINT('Ctrl Pts',(-17.612836477965,-3.93932967304405,-0.000322413107344821));
#91056=CARTESIAN_POINT('Ctrl Pts',(-17.6778854594652,-3.93781527033072,
1.27990257303665));
#91057=CARTESIAN_POINT('Ctrl Pts',(-17.7429344409653,-3.25516936666837,
2.56151443250391));
#91058=CARTESIAN_POINT('Ctrl Pts',(-17.8079834224655,-2.19131799049156,
3.27363847383026));
#91059=CARTESIAN_POINT('Ctrl Pts',(-17.8739227536112,-1.11290528416235,
3.99550962223137));
#91060=CARTESIAN_POINT('Ctrl Pts',(-17.9398620847569,0.357219713964903,
4.13219667838001));
#91061=CARTESIAN_POINT('Ctrl Pts',(-18.0058014159026,1.5502308934945,3.62151454085841));
#91062=CARTESIAN_POINT('Ctrl Pts',(-18.0717407470483,2.74324207302409,3.11083240333683));
#91063=CARTESIAN_POINT('Ctrl Pts',(-18.137680078194,3.65913943395602,1.95278107214503));
#91064=CARTESIAN_POINT('Ctrl Pts',(-18.2036194093397,3.88123999340509,0.674210283506955));
#91065=CARTESIAN_POINT('Ctrl Pts',(-18.2695587404854,4.10334055285416,-0.604360505131115));
#91066=CARTESIAN_POINT('Ctrl Pts',(-18.3354980716311,3.63164431082037,-2.00345075121548));
#91067=CARTESIAN_POINT('Ctrl Pts',(-18.4014374027768,2.68074714401463,-2.88655125411816));
#91068=CARTESIAN_POINT('Ctrl Pts',(-18.4673767339225,1.72984997720887,-3.76965175702084));
#91069=CARTESIAN_POINT('Ctrl Pts',(-18.5333160650682,0.299751885631159,
-4.13676251674186));
#91070=CARTESIAN_POINT('Ctrl Pts',(-18.5992553962139,-0.958931063858458,
-3.82086830544589));
#91071=CARTESIAN_POINT('Ctrl Pts',(-18.6651947273596,-2.21761401334808,
-3.50497409414993));
#91072=CARTESIAN_POINT('Ctrl Pts',(-18.7311340585053,-3.30488182074959,
-2.50607491183698));
#91073=CARTESIAN_POINT('Ctrl Pts',(-18.797073389651,-3.72608736455351,-1.27861501027807));
#91074=CARTESIAN_POINT('Ctrl Pts',(-18.818994419089,-3.86611394602996,-0.870555295862867));
#91075=CARTESIAN_POINT('Ctrl Pts',(-18.840915448527,-3.9325286924352,-0.437235519605974));
#91076=CARTESIAN_POINT('Ctrl Pts',(-18.862836477965,-3.92942440079457,-0.0029931669997546));
#91077=CARTESIAN_POINT('Ctrl Pts',(-19.046163522035,-3.92943419637598,-0.00299686489160711));
#91078=CARTESIAN_POINT('Ctrl Pts',(-19.0242637951135,-3.93253984081017,
-0.436814413326903));
#91079=CARTESIAN_POINT('Ctrl Pts',(-19.0023640681919,-3.86625723115108,
-0.869709862684471));
#91080=CARTESIAN_POINT('Ctrl Pts',(-18.9804643412704,-3.72649769590772,
-1.27741792446391));
#91081=CARTESIAN_POINT('Ctrl Pts',(-18.9145250101247,-3.30568650003283,
-2.50501299872126));
#91082=CARTESIAN_POINT('Ctrl Pts',(-18.848585678979,-2.2187396911716,-3.50426134057971));
#91083=CARTESIAN_POINT('Ctrl Pts',(-18.7826463478333,-0.960158354132277,
-3.82055984985672));
#91084=CARTESIAN_POINT('Ctrl Pts',(-18.7167070166876,0.298422982907047,
-4.13685835913373));
#91085=CARTESIAN_POINT('Ctrl Pts',(-18.6507676855419,1.72863884812446,-3.7702070358293));
#91086=CARTESIAN_POINT('Ctrl Pts',(-18.5848283543962,2.67981959412393,-2.88741208944908));
#91087=CARTESIAN_POINT('Ctrl Pts',(-18.5188890232505,3.6310003401234,-2.00461714306886));
#91088=CARTESIAN_POINT('Ctrl Pts',(-18.4529496921048,4.10314596690491,-0.605678573612871));
#91089=CARTESIAN_POINT('Ctrl Pts',(-18.3870103609591,3.88145615238507,0.67296342282425));
#91090=CARTESIAN_POINT('Ctrl Pts',(-18.3210710298134,3.65976633786522,1.95160541926137));
#91091=CARTESIAN_POINT('Ctrl Pts',(-18.2551316986677,2.74424108204401,3.10995084267962));
#91092=CARTESIAN_POINT('Ctrl Pts',(-18.189192367522,1.55139408042348,3.62101616104847));
#91093=CARTESIAN_POINT('Ctrl Pts',(-18.1232530363763,0.35854707880295,4.13208147941732));
#91094=CARTESIAN_POINT('Ctrl Pts',(-18.0573137052306,-1.11162166861691,
3.99586669273678));
#91095=CARTESIAN_POINT('Ctrl Pts',(-17.9913743740849,-2.19026614791571,
3.27434204576152));
#91096=CARTESIAN_POINT('Ctrl Pts',(-17.9263040900682,-3.25469463697409,
2.56232672974422));
#91097=CARTESIAN_POINT('Ctrl Pts',(-17.8612338060516,-3.93785103528598,
1.28032806316714));
#91098=CARTESIAN_POINT('Ctrl Pts',(-17.796163522035,-3.93933102250188,-0.000314724560625571));
#91099=CARTESIAN_POINT('Origin',(-14.6,0.,0.));
#91100=CARTESIAN_POINT('',(-16.362836477965,-3.93030695978332,0.00326161695698352));
#91101=CARTESIAN_POINT('',(-16.546163522035,-3.93029567594467,0.0032589082896274));
#91102=CARTESIAN_POINT('',(-14.6,-3.933,-4.81653586104654E-16));
#91103=CARTESIAN_POINT('Ctrl Pts',(-16.362836477965,-3.93030695978332,0.00326161695698352));
#91104=CARTESIAN_POINT('Ctrl Pts',(-16.3829768081119,-3.93346431809964,
0.402003105813639));
#91105=CARTESIAN_POINT('Ctrl Pts',(-16.4031171382588,-3.87761320067396,
0.799880981706207));
#91106=CARTESIAN_POINT('Ctrl Pts',(-16.4232574684057,-3.75907374795352,
1.17811202788205));
#91107=CARTESIAN_POINT('Ctrl Pts',(-16.4891967995514,-3.37097622573056,
2.41643841188208));
#91108=CARTESIAN_POINT('Ctrl Pts',(-16.5551361306971,-2.31091991010657,
3.44416963605641));
#91109=CARTESIAN_POINT('Ctrl Pts',(-16.6210754618428,-1.06117218874064,
3.79374445352307));
#91110=CARTESIAN_POINT('Ctrl Pts',(-16.6870147929885,0.188575532625281,
4.14331927098974));
#91111=CARTESIAN_POINT('Ctrl Pts',(-16.7529541241342,1.62801465973314,3.81473768174875));
#91112=CARTESIAN_POINT('Ctrl Pts',(-16.8188934552799,2.60227946772191,2.95748625773082));
#91113=CARTESIAN_POINT('Ctrl Pts',(-16.8848327864256,3.57654427571069,2.10023483371288));
#91114=CARTESIAN_POINT('Ctrl Pts',(-16.9507721175713,4.08563476458038,0.714313574917998));
#91115=CARTESIAN_POINT('Ctrl Pts',(-17.016711448717,3.89794272962465,-0.569759483782462));
#91116=CARTESIAN_POINT('Ctrl Pts',(-17.0826507798627,3.71025069466892,-1.85383254248292));
#91117=CARTESIAN_POINT('Ctrl Pts',(-17.1485901110084,2.82577613588777,-3.03605740108896));
#91118=CARTESIAN_POINT('Ctrl Pts',(-17.2145294421541,1.6469063874515,-3.57858669641594));
#91119=CARTESIAN_POINT('Ctrl Pts',(-17.2804687732998,0.468036639015227,
-4.12111599174291));
#91120=CARTESIAN_POINT('Ctrl Pts',(-17.3464081044455,-1.00522829907616,
-4.02394972379083));
#91121=CARTESIAN_POINT('Ctrl Pts',(-17.4123474355913,-2.10263381624111,
-3.33129320648799));
#91122=CARTESIAN_POINT('Ctrl Pts',(-17.478286766737,-3.20003933340606,-2.63863668918514));
#91123=CARTESIAN_POINT('Ctrl Pts',(-17.5442260978827,-3.92158542964458,
-1.35048992253154));
#91124=CARTESIAN_POINT('Ctrl Pts',(-17.6101654290284,-3.93900827049825,
-0.0528889188779602));
#91125=CARTESIAN_POINT('Ctrl Pts',(-17.6110557786739,-3.939243523418,-0.035367986020451));
#91126=CARTESIAN_POINT('Ctrl Pts',(-17.6119461283195,-3.93935040123822,
-0.0178453294752127));
#91127=CARTESIAN_POINT('Ctrl Pts',(-17.612836477965,-3.93932967304405,-0.000322413107344821));
#91128=CARTESIAN_POINT('Ctrl Pts',(-17.796163522035,-3.93933102250188,-0.000314724560625571));
#91129=CARTESIAN_POINT('Ctrl Pts',(-17.7952944749059,-3.93935078849277,
-0.0174183680265255));
#91130=CARTESIAN_POINT('Ctrl Pts',(-17.7944254277768,-3.9392489640186,-0.0345217696446254));
#91131=CARTESIAN_POINT('Ctrl Pts',(-17.7935563806478,-3.93902483345017,
-0.0516235683591434));
#91132=CARTESIAN_POINT('Ctrl Pts',(-17.7276170495021,-3.92201882850808,
-1.34923002823458));
#91133=CARTESIAN_POINT('Ctrl Pts',(-17.6616777183564,-3.20088660744617,
-2.63760844071548));
#91134=CARTESIAN_POINT('Ctrl Pts',(-17.5957383872107,-2.10370371425439,
-3.33061740732549));
#91135=CARTESIAN_POINT('Ctrl Pts',(-17.529799056065,-1.00652082106261,-4.02362637393549));
#91136=CARTESIAN_POINT('Ctrl Pts',(-17.4638597249192,0.466712744259044,
-4.12126589467459));
#91137=CARTESIAN_POINT('Ctrl Pts',(-17.3979203937735,1.64575664401571,-3.57911535159533));
#91138=CARTESIAN_POINT('Ctrl Pts',(-17.3319810626278,2.8248005437724,-3.03696480851606));
#91139=CARTESIAN_POINT('Ctrl Pts',(-17.2660417314821,3.70965477796409,-1.85502420161841));
#91140=CARTESIAN_POINT('Ctrl Pts',(-17.2001024003364,3.8977592809668,-0.571011575175547));
#91141=CARTESIAN_POINT('Ctrl Pts',(-17.1341630691907,4.08586378396949,0.713001051267284));
#91142=CARTESIAN_POINT('Ctrl Pts',(-17.068223738045,3.57721855578324,2.09908569725531));
#91143=CARTESIAN_POINT('Ctrl Pts',(-17.0022844068993,2.60322923196453,2.95664999572026));
#91144=CARTESIAN_POINT('Ctrl Pts',(-16.9363450757536,1.62923990814581,3.81421429418521));
#91145=CARTESIAN_POINT('Ctrl Pts',(-16.8704057446079,0.189906488694602,
4.14325824512707));
#91146=CARTESIAN_POINT('Ctrl Pts',(-16.8044664134622,-1.05995339270459,
3.79408492744183));
#91147=CARTESIAN_POINT('Ctrl Pts',(-16.7385270823165,-2.3098132741038,3.44491160975658));
#91148=CARTESIAN_POINT('Ctrl Pts',(-16.6725877511708,-3.37019961745101,
2.41752102344424));
#91149=CARTESIAN_POINT('Ctrl Pts',(-16.6066484200251,-3.75869489060368,
1.17931944387305));
#91150=CARTESIAN_POINT('Ctrl Pts',(-16.5864867873617,-3.87748133949039,
0.800726501288189));
#91151=CARTESIAN_POINT('Ctrl Pts',(-16.5663251546984,-3.93345310289138,
0.40242496779342));
#91152=CARTESIAN_POINT('Ctrl Pts',(-16.546163522035,-3.93029567594467,0.0032589082896274));
#91153=CARTESIAN_POINT('Origin',(-14.6,0.,0.));
#91154=CARTESIAN_POINT('',(-15.112836477965,-3.92822229680268,-0.00240354736792903));
#91155=CARTESIAN_POINT('',(-15.296163522035,-3.92822997878168,-0.00240860774561585));
#91156=CARTESIAN_POINT('',(-14.6,-3.933,-4.81653586104654E-16));
#91157=CARTESIAN_POINT('Ctrl Pts',(-15.112836477965,-3.92822229680268,-0.00240354736792903));
#91158=CARTESIAN_POINT('Ctrl Pts',(-15.1540074879044,-3.92363278539411,
0.813797469098643));
#91159=CARTESIAN_POINT('Ctrl Pts',(-15.1951784978437,-3.67557873714955,
1.63255455559306));
#91160=CARTESIAN_POINT('Ctrl Pts',(-15.2363495077831,-3.20422949520173,
2.29161443852864));
#91161=CARTESIAN_POINT('Ctrl Pts',(-15.3022888389288,-2.44931836244454,
3.34716221182241));
#91162=CARTESIAN_POINT('Ctrl Pts',(-15.3682281700745,-1.12163044217474,
3.99306905325299));
#91163=CARTESIAN_POINT('Ctrl Pts',(-15.4341675012202,0.174809200620274,
3.93548283393184));
#91164=CARTESIAN_POINT('Ctrl Pts',(-15.5001068323659,1.47124884341531,3.87789661461069));
#91165=CARTESIAN_POINT('Ctrl Pts',(-15.5660461635116,2.73644020873557,3.11681733453777));
#91166=CARTESIAN_POINT('Ctrl Pts',(-15.6319854946573,3.39479073074392,1.99849425499521));
#91167=CARTESIAN_POINT('Ctrl Pts',(-15.697924825803,4.05314125275225,0.880171175452675));
#91168=CARTESIAN_POINT('Ctrl Pts',(-15.7638641569487,4.1046509314487,-0.595395703559483));
#91169=CARTESIAN_POINT('Ctrl Pts',(-15.8298034880944,3.52588569279593,-1.75690451480171));
#91170=CARTESIAN_POINT('Ctrl Pts',(-15.8957428192401,2.94712045414315,-2.91841332604395));
#91171=CARTESIAN_POINT('Ctrl Pts',(-15.9616821503858,1.73808029814112,-3.76586406951625));
#91172=CARTESIAN_POINT('Ctrl Pts',(-16.0276214815315,0.448812075146874,
-3.91371321304922));
#91173=CARTESIAN_POINT('Ctrl Pts',(-16.0935608126772,-0.840456147847376,
-4.06156235658218));
#91174=CARTESIAN_POINT('Ctrl Pts',(-16.1595001438229,-2.20995243783385,
-3.50980990017581));
#91175=CARTESIAN_POINT('Ctrl Pts',(-16.2254394749686,-3.03663121841612,
-2.50947290005976));
#91176=CARTESIAN_POINT('Ctrl Pts',(-16.2712384759674,-3.61081147835717,
-1.81467611532709));
#91177=CARTESIAN_POINT('Ctrl Pts',(-16.3170374769662,-3.92312714417811,
-0.903474355751184));
#91178=CARTESIAN_POINT('Ctrl Pts',(-16.362836477965,-3.93030695978332,0.00326161695698352));
#91179=CARTESIAN_POINT('Ctrl Pts',(-16.546163522035,-3.93029567594467,0.0032589082896274));
#91180=CARTESIAN_POINT('Ctrl Pts',(-16.5003858235527,-3.92312662663404,
-0.903061716702896));
#91181=CARTESIAN_POINT('Ctrl Pts',(-16.4546081250703,-3.61112705848366,
-1.81383925900364));
#91182=CARTESIAN_POINT('Ctrl Pts',(-16.408830426588,-3.03743701831446,-2.50849715788562));
#91183=CARTESIAN_POINT('Ctrl Pts',(-16.3428910954423,-2.21107966991449,
-3.50909960724294));
#91184=CARTESIAN_POINT('Ctrl Pts',(-16.2769517642966,-0.841760770156474,
-4.0612919331276));
#91185=CARTESIAN_POINT('Ctrl Pts',(-16.2110124331509,0.447554807371917,
-3.91385696286228));
#91186=CARTESIAN_POINT('Ctrl Pts',(-16.1450731020052,1.73687038490033,-3.76642199259695));
#91187=CARTESIAN_POINT('Ctrl Pts',(-16.0791337708595,2.9461826401991,-2.91935972618162));
#91188=CARTESIAN_POINT('Ctrl Pts',(-16.0131944397138,3.52532093267943,-1.75803696006639));
#91189=CARTESIAN_POINT('Ctrl Pts',(-15.9472551085681,4.10445922515975,-0.596714193951166));
#91190=CARTESIAN_POINT('Ctrl Pts',(-15.8813157774224,4.05342355482162,0.878869071863958));
#91191=CARTESIAN_POINT('Ctrl Pts',(-15.8153764462767,3.39543234793979,1.9974035150443));
#91192=CARTESIAN_POINT('Ctrl Pts',(-15.749437115131,2.73744114105796,3.11593795822463));
#91193=CARTESIAN_POINT('Ctrl Pts',(-15.6834977839853,1.47249439763243,3.87742357877017));
#91194=CARTESIAN_POINT('Ctrl Pts',(-15.6175584528396,0.176073393976921,
3.93542625280676));
#91195=CARTESIAN_POINT('Ctrl Pts',(-15.5516191216939,-1.12034760967857,
3.99342892684335));
#91196=CARTESIAN_POINT('Ctrl Pts',(-15.4856797905482,-2.44824287356404,
3.34794865437101));
#91197=CARTESIAN_POINT('Ctrl Pts',(-15.4197404594025,-3.20349300273775,
2.29264349883656));
#91198=CARTESIAN_POINT('Ctrl Pts',(-15.3785481469467,-3.67529789918852,
1.63339417149699));
#91199=CARTESIAN_POINT('Ctrl Pts',(-15.3373558344908,-3.92362784693915,
0.814210551230189));
#91200=CARTESIAN_POINT('Ctrl Pts',(-15.296163522035,-3.92822997878168,-0.00240860774561585));
#91201=CARTESIAN_POINT('Origin',(-14.6,0.,0.));
#91202=CARTESIAN_POINT('',(-13.862836477965,-3.93881447356001,-0.00131697643526163));
#91203=CARTESIAN_POINT('',(-14.046163522035,-3.93882016358904,-0.0013098913562943));
#91204=CARTESIAN_POINT('',(-14.6,-3.933,-4.81653586104654E-16));
#91205=CARTESIAN_POINT('Ctrl Pts',(-13.862836477965,-3.93881447356001,-0.00131697643526163));
#91206=CARTESIAN_POINT('Ctrl Pts',(-13.9250381676968,-3.93345678725095,
1.2232994368523));
#91207=CARTESIAN_POINT('Ctrl Pts',(-13.9872398574286,-3.31693161062816,
2.45257298663125));
#91208=CARTESIAN_POINT('Ctrl Pts',(-14.0494415471604,-2.32981268385847,
3.17656359151299));
#91209=CARTESIAN_POINT('Ctrl Pts',(-14.1153808783061,-1.28337870315618,
3.94405811533566));
#91210=CARTESIAN_POINT('Ctrl Pts',(-14.1813202094518,0.179524393308559,
4.143721311221));
#91211=CARTESIAN_POINT('Ctrl Pts',(-14.2472595405975,1.39335606364934,3.68471739386962));
#91212=CARTESIAN_POINT('Ctrl Pts',(-14.3131988717432,2.60718773399009,3.22571347651824));
#91213=CARTESIAN_POINT('Ctrl Pts',(-14.3791382028889,3.57194797820692,2.10804244593017));
#91214=CARTESIAN_POINT('Ctrl Pts',(-14.4450775340346,3.84872388588344,0.840183219913357));
#91215=CARTESIAN_POINT('Ctrl Pts',(-14.5110168651803,4.12549979355995,-0.427676006103479));
#91216=CARTESIAN_POINT('Ctrl Pts',(-14.576956196326,3.71429136469616,-1.84572342754904));
#91217=CARTESIAN_POINT('Ctrl Pts',(-14.6428955274717,2.80217584400881,-2.76882537044993));
#91218=CARTESIAN_POINT('Ctrl Pts',(-14.7088348586174,1.89006032332144,-3.69192731335084));
#91219=CARTESIAN_POINT('Ctrl Pts',(-14.7747741897631,0.477037710810491,
-4.12008377770702));
#91220=CARTESIAN_POINT('Ctrl Pts',(-14.8407135209088,-0.794044331569596,
-3.85850709372108));
#91221=CARTESIAN_POINT('Ctrl Pts',(-14.9066528520546,-2.06512637394967,
-3.59693040973513));
#91222=CARTESIAN_POINT('Ctrl Pts',(-14.9725921832003,-3.19426784619889,
-2.64562057740708));
#91223=CARTESIAN_POINT('Ctrl Pts',(-15.038531514346,-3.6677714097012,-1.43737130866458));
#91224=CARTESIAN_POINT('Ctrl Pts',(-15.0632998355523,-3.84563018001938,
-0.983525243416702));
#91225=CARTESIAN_POINT('Ctrl Pts',(-15.0880681567587,-3.93098332921153,
-0.493426939181124));
#91226=CARTESIAN_POINT('Ctrl Pts',(-15.112836477965,-3.92822229680268,-0.00240354736792903));
#91227=CARTESIAN_POINT('Ctrl Pts',(-15.296163522035,-3.92822997878168,-0.00240860774561585));
#91228=CARTESIAN_POINT('Ctrl Pts',(-15.2714165033451,-3.93099479182398,
-0.49300717783927));
#91229=CARTESIAN_POINT('Ctrl Pts',(-15.2466694846552,-3.84579285967439,
-0.982680177283143));
#91230=CARTESIAN_POINT('Ctrl Pts',(-15.2219224659653,-3.66823274535127,
-1.43619293873765));
#91231=CARTESIAN_POINT('Ctrl Pts',(-15.1559831348196,-3.19511736432913,
-2.64459418218073));
#91232=CARTESIAN_POINT('Ctrl Pts',(-15.090043803674,-2.06628160782294,-3.59626663047032));
#91233=CARTESIAN_POINT('Ctrl Pts',(-15.0241044725283,-0.795283730580655,
-3.85825160133719));
#91234=CARTESIAN_POINT('Ctrl Pts',(-14.9581651413826,0.475714146661664,
-4.12023657220405));
#91235=CARTESIAN_POINT('Ctrl Pts',(-14.8922258102368,1.88887414464008,-3.69253406564815));
#91236=CARTESIAN_POINT('Ctrl Pts',(-14.8262864790911,2.80128609855997,-2.76972522560667));
#91237=CARTESIAN_POINT('Ctrl Pts',(-14.7603471479454,3.71369805247985,-1.84691638556519));
#91238=CARTESIAN_POINT('Ctrl Pts',(-14.6944078167997,4.1253619623412,-0.429001212038141));
#91239=CARTESIAN_POINT('Ctrl Pts',(-14.628468485654,3.84899336459595,0.838946786538663));
#91240=CARTESIAN_POINT('Ctrl Pts',(-14.5625291545083,3.57262476685072,2.10689478511543));
#91241=CARTESIAN_POINT('Ctrl Pts',(-14.4965898233626,2.60822366149893,3.22487560874196));
#91242=CARTESIAN_POINT('Ctrl Pts',(-14.4306504922169,1.39453957050327,3.68426940079682));
#91243=CARTESIAN_POINT('Ctrl Pts',(-14.3647111610712,0.180855479507593,
4.14366319285169));
#91244=CARTESIAN_POINT('Ctrl Pts',(-14.2987718299255,-1.28211159713196,
3.94446995333486));
#91245=CARTESIAN_POINT('Ctrl Pts',(-14.2328324987798,-2.32879201006434,
3.17731166321589));
#91246=CARTESIAN_POINT('Ctrl Pts',(-14.1706095065316,-3.3164815435904,2.45339039331705));
#91247=CARTESIAN_POINT('Ctrl Pts',(-14.1083865142833,-3.93348591101852,
1.22372095160461));
#91248=CARTESIAN_POINT('Ctrl Pts',(-14.046163522035,-3.93882016358904,-0.0013098913562943));
#91249=CARTESIAN_POINT('Origin',(-14.6,0.,0.));
#91250=CARTESIAN_POINT('',(-12.612836477965,-3.9318717373109,0.00350585034690487));
#91251=CARTESIAN_POINT('',(-12.796163522035,-3.93185928339207,0.00350492153532546));
#91252=CARTESIAN_POINT('',(-14.6,-3.933,-4.81653586104654E-16));
#91253=CARTESIAN_POINT('Ctrl Pts',(-12.612836477965,-3.9318717373109,0.00350585034690487));
#91254=CARTESIAN_POINT('Ctrl Pts',(-12.6301295163436,-3.93487740264675,
0.345530407337765));
#91255=CARTESIAN_POINT('Ctrl Pts',(-12.6474225547221,-3.89392515658943,
0.686846730394007));
#91256=CARTESIAN_POINT('Ctrl Pts',(-12.6647155931007,-3.80617738217334,
1.01567570032258));
#91257=CARTESIAN_POINT('Ctrl Pts',(-12.7306549242464,-3.47159016691004,
2.26951911775896));
#91258=CARTESIAN_POINT('Ctrl Pts',(-12.7965942553921,-2.45662407837034,
3.34180392160147));
#91259=CARTESIAN_POINT('Ctrl Pts',(-12.8625335865378,-1.2230329279963,3.74469943384385));
#91260=CARTESIAN_POINT('Ctrl Pts',(-12.9284729176835,0.0105582223777351,
4.14759494608623));
#91261=CARTESIAN_POINT('Ctrl Pts',(-12.9944122488292,1.46277443458609,3.88110116672849));
#91262=CARTESIAN_POINT('Ctrl Pts',(-13.0603515799749,2.47293711197736,3.06645812510113));
#91263=CARTESIAN_POINT('Ctrl Pts',(-13.1262909111206,3.48309978936863,2.25181508347378));
#91264=CARTESIAN_POINT('Ctrl Pts',(-13.1922302422663,4.05120893194283,0.889022779576799));
#91265=CARTESIAN_POINT('Ctrl Pts',(-13.258169573412,3.91880608984557,-0.401923155569485));
#91266=CARTESIAN_POINT('Ctrl Pts',(-13.3241089045577,3.78640324774831,-1.69286909071581));
#91267=CARTESIAN_POINT('Ctrl Pts',(-13.3900482357034,2.95348842097959,-2.91196865711145));
#91268=CARTESIAN_POINT('Ctrl Pts',(-13.4559875668491,1.79899209816333,-3.50459852530066));
#91269=CARTESIAN_POINT('Ctrl Pts',(-13.5219268979948,0.644495775347081,
-4.09722839348988));
#91270=CARTESIAN_POINT('Ctrl Pts',(-13.5878662291405,-0.831582043516668,
-4.06338856347267));
#91271=CARTESIAN_POINT('Ctrl Pts',(-13.6538055602862,-1.95770704162521,
-3.41847429885976));
#91272=CARTESIAN_POINT('Ctrl Pts',(-13.7197448914319,-3.08383203973376,
-2.77356003424685));
#91273=CARTESIAN_POINT('Ctrl Pts',(-13.7856842225776,-3.86000421708709,
-1.51757133503824));
#91274=CARTESIAN_POINT('Ctrl Pts',(-13.8516235537233,-3.93310787329384,
-0.221914059553938));
#91275=CARTESIAN_POINT('Ctrl Pts',(-13.8553611951372,-3.93725161039578,
-0.148472272885356));
#91276=CARTESIAN_POINT('Ctrl Pts',(-13.8590988365511,-3.93913641192402,
-0.0749030324119008));
#91277=CARTESIAN_POINT('Ctrl Pts',(-13.862836477965,-3.93881447356001,-0.00131697643526163));
#91278=CARTESIAN_POINT('Ctrl Pts',(-14.046163522035,-3.93882016358904,-0.0013098913562943));
#91279=CARTESIAN_POINT('Ctrl Pts',(-14.0424471831376,-3.93913875788354,
-0.074476250088611));
#91280=CARTESIAN_POINT('Ctrl Pts',(-14.0387308442401,-3.9372753956192,-0.147626061958944));
#91281=CARTESIAN_POINT('Ctrl Pts',(-14.0350145053427,-3.9331787335674,-0.220650586131847));
#91282=CARTESIAN_POINT('Ctrl Pts',(-13.969075174197,-3.8604912949129,-1.51633120463951));
#91283=CARTESIAN_POINT('Ctrl Pts',(-13.9031358430513,-3.08472266837869,
-2.77256910093373));
#91284=CARTESIAN_POINT('Ctrl Pts',(-13.8371965119056,-1.95880496090319,
-3.41784504571058));
#91285=CARTESIAN_POINT('Ctrl Pts',(-13.7712571807599,-0.832887253427681,
-4.06312099048742));
#91286=CARTESIAN_POINT('Ctrl Pts',(-13.7053178496142,0.64317953498912,-4.0974349837469));
#91287=CARTESIAN_POINT('Ctrl Pts',(-13.6393785184685,1.79786610579188,-3.50517604365201));
#91288=CARTESIAN_POINT('Ctrl Pts',(-13.5734391873228,2.95255267659464,-2.91291710355713));
#91289=CARTESIAN_POINT('Ctrl Pts',(-13.5074998561771,3.78585902978335,-1.69408523010788));
#91290=CARTESIAN_POINT('Ctrl Pts',(-13.4415605250314,3.91867655372215,-0.403181967175553));
#91291=CARTESIAN_POINT('Ctrl Pts',(-13.3756211938857,4.05149407766094,0.88772129575677));
#91292=CARTESIAN_POINT('Ctrl Pts',(-13.30968186274,3.48382277234982,2.25069594817216));
#91293=CARTESIAN_POINT('Ctrl Pts',(-13.2437425315943,2.47392189574176,3.06566340049209));
#91294=CARTESIAN_POINT('Ctrl Pts',(-13.1778032004486,1.46402101913371,3.88063085281201));
#91295=CARTESIAN_POINT('Ctrl Pts',(-13.1118638693029,0.0118905712287158,
4.14759110503647));
#91296=CARTESIAN_POINT('Ctrl Pts',(-13.0459245381572,-1.22182986936823,
3.74509190830704));
#91297=CARTESIAN_POINT('Ctrl Pts',(-12.9799852070115,-2.45555030996515,
3.34259271157761));
#91298=CARTESIAN_POINT('Ctrl Pts',(-12.9140458758658,-3.47086074325403,
2.27063406589432));
#91299=CARTESIAN_POINT('Ctrl Pts',(-12.8481065447201,-3.80585069984909,
1.01689826521902));
#91300=CARTESIAN_POINT('Ctrl Pts',(-12.830792203825,-3.89381231856922,0.687692483661536));
#91301=CARTESIAN_POINT('Ctrl Pts',(-12.81347786293,-3.93486707364353,0.345953496776215));
#91302=CARTESIAN_POINT('Ctrl Pts',(-12.796163522035,-3.93185928339207,0.00350492153532546));
#91303=CARTESIAN_POINT('Origin',(-14.6,0.,0.));
#91304=CARTESIAN_POINT('',(-11.362836477965,-3.92733190008639,-0.00165504447000753));
#91305=CARTESIAN_POINT('',(-11.546163522035,-3.92733705745214,-0.0016611125421626));
#91306=CARTESIAN_POINT('',(-14.6,-3.933,-4.81653586104654E-16));
#91307=CARTESIAN_POINT('Ctrl Pts',(-11.362836477965,-3.92733190008639,-0.00165504447000753));
#91308=CARTESIAN_POINT('Ctrl Pts',(-11.401160196136,-3.92443034344515,0.758531279775249));
#91309=CARTESIAN_POINT('Ctrl Pts',(-11.439483914307,-3.71165434622295,1.52021948759287));
#91310=CARTESIAN_POINT('Ctrl Pts',(-11.477807632478,-3.29963929855811,2.15196744682735));
#91311=CARTESIAN_POINT('Ctrl Pts',(-11.5437469636237,-2.59073113511326,
3.23894542998406));
#91312=CARTESIAN_POINT('Ctrl Pts',(-11.6096862947694,-1.2919910634956,3.94124528603681));
#91313=CARTESIAN_POINT('Ctrl Pts',(-11.6756256259151,0.0057255321462002,
3.93935916248764));
#91314=CARTESIAN_POINT('Ctrl Pts',(-11.7415649570608,1.303442127788,3.93747303893847));
#91315=CARTESIAN_POINT('Ctrl Pts',(-11.8075042882065,2.60013524745393,3.23140093578738));
#91316=CARTESIAN_POINT('Ctrl Pts',(-11.8734436193522,3.30588075768066,2.14236687072743));
#91317=CARTESIAN_POINT('Ctrl Pts',(-11.9393829504979,4.01162626790739,1.05333280566748));
#91318=CARTESIAN_POINT('Ctrl Pts',(-12.0053222816437,4.12642416869491,-0.418663221301322));
#91319=CARTESIAN_POINT('Ctrl Pts',(-12.0712616127894,3.59804772179776,-1.60394388444846));
#91320=CARTESIAN_POINT('Ctrl Pts',(-12.1372009439351,3.06967127490061,-2.7892245475956));
#91321=CARTESIAN_POINT('Ctrl Pts',(-12.2031402750808,1.89812048031879,-3.68778984692108));
#91322=CARTESIAN_POINT('Ctrl Pts',(-12.2690796062265,0.616386588503315,
-3.8908419354051));
#91323=CARTESIAN_POINT('Ctrl Pts',(-12.3350189373722,-0.665347303312165,
-4.09389402388912));
#91324=CARTESIAN_POINT('Ctrl Pts',(-12.4009582685179,-2.0572642923613,-3.60143290153169));
#91325=CARTESIAN_POINT('Ctrl Pts',(-12.4668975996636,-2.92611861589242,
-2.63750132483786));
#91326=CARTESIAN_POINT('Ctrl Pts',(-12.5155438924307,-3.56710997962201,
-1.92636736468688));
#91327=CARTESIAN_POINT('Ctrl Pts',(-12.5641901851979,-3.92341663111804,
-0.958628528165194));
#91328=CARTESIAN_POINT('Ctrl Pts',(-12.612836477965,-3.9318717373109,0.00350585034690487));
#91329=CARTESIAN_POINT('Ctrl Pts',(-12.796163522035,-3.93185928339207,0.00350492153532546));
#91330=CARTESIAN_POINT('Ctrl Pts',(-12.7475385317843,-3.92341231029966,
-0.958215696846525));
#91331=CARTESIAN_POINT('Ctrl Pts',(-12.6989135415336,-3.56744781444277,
-1.92553277784049));
#91332=CARTESIAN_POINT('Ctrl Pts',(-12.650288551283,-2.92696555489341,-2.63656106923674));
#91333=CARTESIAN_POINT('Ctrl Pts',(-12.5843492201373,-2.0584209734415,-3.60077164734977));
#91334=CARTESIAN_POINT('Ctrl Pts',(-12.5184098889916,-0.666662330636484,
-4.09367984790849));
#91335=CARTESIAN_POINT('Ctrl Pts',(-12.4524705578459,0.615136649612009,
-3.89103951838726));
#91336=CARTESIAN_POINT('Ctrl Pts',(-12.3865312267001,1.89693562986052,-3.68839918886602));
#91337=CARTESIAN_POINT('Ctrl Pts',(-12.3205918955544,3.06877494755251,-2.7902103292648));
#91338=CARTESIAN_POINT('Ctrl Pts',(-12.2546525644087,3.59753209007232,-1.60509952720919));
#91339=CARTESIAN_POINT('Ctrl Pts',(-12.188713233263,4.12628923259211,-0.419988725153615));
#91340=CARTESIAN_POINT('Ctrl Pts',(-12.1227739021173,4.01196419993977,1.05204401935632));
#91341=CARTESIAN_POINT('Ctrl Pts',(-12.0568345709716,3.30656860133704,2.14130467612604));
#91342=CARTESIAN_POINT('Ctrl Pts',(-11.9908952398259,2.6011730027343,3.23056533289578));
#91343=CARTESIAN_POINT('Ctrl Pts',(-11.9249559086802,1.30470683818116,3.93705390192528));
#91344=CARTESIAN_POINT('Ctrl Pts',(-11.8590165775345,0.0069909890327869,
3.93935689642606));
#91345=CARTESIAN_POINT('Ctrl Pts',(-11.7930772463888,-1.29072486011559,
3.94165989092684));
#91346=CARTESIAN_POINT('Ctrl Pts',(-11.7271379152431,-2.58969039385919,
3.23977731089889));
#91347=CARTESIAN_POINT('Ctrl Pts',(-11.6611985840974,-3.29894765516817,
2.15302717117264));
#91348=CARTESIAN_POINT('Ctrl Pts',(-11.6228535634099,-3.71139473167168,
1.52106054570216));
#91349=CARTESIAN_POINT('Ctrl Pts',(-11.5845085427225,-3.92442300853275,
0.758945115536301));
#91350=CARTESIAN_POINT('Ctrl Pts',(-11.546163522035,-3.92733705745214,-0.0016611125421626));
#91351=CARTESIAN_POINT('Origin',(-14.6,0.,0.));
#91352=CARTESIAN_POINT('',(-10.112836477965,-3.93779509892002,-0.00218943587030118));
#91353=CARTESIAN_POINT('',(-10.296163522035,-3.93780400755292,-0.00218353918451927));
#91354=CARTESIAN_POINT('',(-14.6,-3.933,-4.81653586104654E-16));
#91355=CARTESIAN_POINT('Ctrl Pts',(-10.112836477965,-3.93779509892002,-0.00218943587030118));
#91356=CARTESIAN_POINT('Ctrl Pts',(-10.1721908759285,-3.9299575440291,1.167171333214));
#91357=CARTESIAN_POINT('Ctrl Pts',(-10.2315452738919,-3.37542498846826,
2.34298987769126));
#91358=CARTESIAN_POINT('Ctrl Pts',(-10.2908996718554,-2.46401299743278,
3.07363357303306));
#91359=CARTESIAN_POINT('Ctrl Pts',(-10.3568390030011,-1.45148656048612,
3.88533680362308));
#91360=CARTESIAN_POINT('Ctrl Pts',(-10.4227783341468,0.00149816796940136,
4.14760811412465));
#91361=CARTESIAN_POINT('Ctrl Pts',(-10.4887176652925,1.23391295860962,3.74112846656847));
#91362=CARTESIAN_POINT('Ctrl Pts',(-10.5546569964382,2.46632774924983,3.33464881901229));
#91363=CARTESIAN_POINT('Ctrl Pts',(-10.6205963275839,3.47817260207474,2.2594182133984));
#91364=CARTESIAN_POINT('Ctrl Pts',(-10.6865356587296,3.80911369642228,1.00460750570652));
#91365=CARTESIAN_POINT('Ctrl Pts',(-10.7524749898753,4.14005479076982,-0.25020320198539));
#91366=CARTESIAN_POINT('Ctrl Pts',(-10.818414321021,3.79009212663995,-1.68459401175529));
#91367=CARTESIAN_POINT('Ctrl Pts',(-10.8843536521667,2.91843949043304,-2.64599590579325));
#91368=CARTESIAN_POINT('Ctrl Pts',(-10.9502929833124,2.04678685422614,-3.60739779983119));
#91369=CARTESIAN_POINT('Ctrl Pts',(-11.0162323144581,0.653444245942222,
-4.0958107781372));
#91370=CARTESIAN_POINT('Ctrl Pts',(-11.0821716456038,-0.627693993233959,
-3.88903376735812));
#91371=CARTESIAN_POINT('Ctrl Pts',(-11.1481109767495,-1.90883223241014,
-3.68225675657904));
#91372=CARTESIAN_POINT('Ctrl Pts',(-11.2140503078952,-3.07776610247859,
-2.78028975671487));
#91373=CARTESIAN_POINT('Ctrl Pts',(-11.2799896390409,-3.6026949098768,-1.59347820165245));
#91374=CARTESIAN_POINT('Ctrl Pts',(-11.3076052520156,-3.82253685447201,
-1.09643754307974));
#91375=CARTESIAN_POINT('Ctrl Pts',(-11.3352208649903,-3.92942272710039,
-0.549436218137531));
#91376=CARTESIAN_POINT('Ctrl Pts',(-11.362836477965,-3.92733190008639,-0.00165504447000753));
#91377=CARTESIAN_POINT('Ctrl Pts',(-11.546163522035,-3.92733705745214,-0.0016611125421626));
#91378=CARTESIAN_POINT('Ctrl Pts',(-11.5185692115768,-3.92943410080041,
-0.549017823211577));
#91379=CARTESIAN_POINT('Ctrl Pts',(-11.4909749011185,-3.82271919215505,
-1.09559296270092));
#91380=CARTESIAN_POINT('Ctrl Pts',(-11.4633805906603,-3.60320639947517,
-1.59232071961913));
#91381=CARTESIAN_POINT('Ctrl Pts',(-11.3974412595146,-3.07865889359882,
-2.77930077126006));
#91382=CARTESIAN_POINT('Ctrl Pts',(-11.3315019283689,-1.91001489297174,
-3.68164317511733));
#91383=CARTESIAN_POINT('Ctrl Pts',(-11.2655625972232,-0.628943216485102,
-3.88883170911067));
#91384=CARTESIAN_POINT('Ctrl Pts',(-11.1996232660775,0.652128460001497,
-4.096020243104));
#91385=CARTESIAN_POINT('Ctrl Pts',(-11.1336839349318,2.04562781234766,-3.60805490723346));
#91386=CARTESIAN_POINT('Ctrl Pts',(-11.0677446037861,2.91758918943131,-2.64693312213603));
#91387=CARTESIAN_POINT('Ctrl Pts',(-11.0018052726404,3.78955056651497,-1.68581133703858));
#91388=CARTESIAN_POINT('Ctrl Pts',(-10.9358659414947,4.13997396833612,-0.251533102714276));
#91389=CARTESIAN_POINT('Ctrl Pts',(-10.869926610349,3.80943599815624,1.00338377867027));
#91390=CARTESIAN_POINT('Ctrl Pts',(-10.8039872792033,3.47889802797636,2.25830066005483));
#91391=CARTESIAN_POINT('Ctrl Pts',(-10.7380479480576,2.4673986857954,3.33385618849958));
#91392=CARTESIAN_POINT('Ctrl Pts',(-10.6721086169119,1.23511460391369,3.7407316859869));
#91393=CARTESIAN_POINT('Ctrl Pts',(-10.6061692857662,0.0028305220320006,
4.1476071834742));
#91394=CARTESIAN_POINT('Ctrl Pts',(-10.5402299546205,-1.45023829955045,
3.88580265000409));
#91395=CARTESIAN_POINT('Ctrl Pts',(-10.4742906234748,-2.46302537375653,
3.07442476563971));
#91396=CARTESIAN_POINT('Ctrl Pts',(-10.4149149229948,-3.37499916729004,
2.34381180064602));
#91397=CARTESIAN_POINT('Ctrl Pts',(-10.3555392225149,-3.92998045545785,
1.16758970334765));
#91398=CARTESIAN_POINT('Ctrl Pts',(-10.296163522035,-3.93780400755292,-0.00218353918451927));
#91399=CARTESIAN_POINT('Origin',(-14.6,0.,0.));
#91400=CARTESIAN_POINT('',(-8.86283647796501,-3.93354422253028,0.0035021652868221));
#91401=CARTESIAN_POINT('',(-9.04616352203496,-3.93353134025131,0.00350314687873205));
#91402=CARTESIAN_POINT('',(-14.6,-3.933,-4.81653586104654E-16));
#91403=CARTESIAN_POINT('Ctrl Pts',(-8.86283647796501,-3.93354422253028,
0.0035021652868221));
#91404=CARTESIAN_POINT('Ctrl Pts',(-8.87728222457522,-3.93615140491192,
0.288902068067195));
#91405=CARTESIAN_POINT('Ctrl Pts',(-8.89172797118542,-3.9077075457056,0.573786733317711));
#91406=CARTESIAN_POINT('Ctrl Pts',(-8.90617371779562,-3.84626535743036,
0.851367249208478));
#91407=CARTESIAN_POINT('Ctrl Pts',(-8.97211304894133,-3.56580517019878,
2.11841657873129));
#91408=CARTESIAN_POINT('Ctrl Pts',(-9.03805238008703,-2.59780012432051,
3.23327849510991));
#91409=CARTESIAN_POINT('Ctrl Pts',(-9.10399171123273,-1.38263933670938,
3.68875207317834));
#91410=CARTESIAN_POINT('Ctrl Pts',(-9.16993104237844,-0.16747854909823,
4.14422565124678));
#91411=CARTESIAN_POINT('Ctrl Pts',(-9.23587037352414,1.29483798024581,3.94031089100503));
#91412=CARTESIAN_POINT('Ctrl Pts',(-9.30180970466984,2.33903656525223,3.16977780596791));
#91413=CARTESIAN_POINT('Ctrl Pts',(-9.36774903581554,3.38323515025861,2.39924472093081));
#91414=CARTESIAN_POINT('Ctrl Pts',(-9.43368836696125,4.00931579092741,1.06209331109839));
#91415=CARTESIAN_POINT('Ctrl Pts',(-9.49962769810695,3.93244619053149,-0.233345990683485));
#91416=CARTESIAN_POINT('Ctrl Pts',(-9.56556702925265,3.85557659013557,-1.52878529246538));
#91417=CARTESIAN_POINT('Ctrl Pts',(-9.63150636039835,3.07575674867495,-2.78251248619667));
#91418=CARTESIAN_POINT('Ctrl Pts',(-9.69744569154406,1.94776185331931,-3.42415057431005));
#91419=CARTESIAN_POINT('Ctrl Pts',(-9.76338502268976,0.819766957963639,
-4.06578866242344));
#91420=CARTESIAN_POINT('Ctrl Pts',(-9.82932435383547,-0.656402991287067,
-4.09533764491883));
#91421=CARTESIAN_POINT('Ctrl Pts',(-9.89526368498117,-1.80917176336531,
-3.49935435808312));
#91422=CARTESIAN_POINT('Ctrl Pts',(-9.96120301612687,-2.96194053544351,
-2.90337107124743));
#91423=CARTESIAN_POINT('Ctrl Pts',(-10.0271423472726,-3.79130813034929,
-1.68185551508067));
#91424=CARTESIAN_POINT('Ctrl Pts',(-10.0930816784183,-3.91995785508327,
-0.390530161658051));
#91425=CARTESIAN_POINT('Ctrl Pts',(-10.0996666116005,-3.93280526840349,
-0.261573876826474));
#91426=CARTESIAN_POINT('Ctrl Pts',(-10.1062515447828,-3.93866461789486,
-0.131921398362811));
#91427=CARTESIAN_POINT('Ctrl Pts',(-10.112836477965,-3.93779509892002,-0.00218943587030118));
#91428=CARTESIAN_POINT('Ctrl Pts',(-10.296163522035,-3.93780400755292,-0.00218353918451927));
#91429=CARTESIAN_POINT('Ctrl Pts',(-10.2895998913692,-3.93866885472156,
-0.131495016179637));
#91430=CARTESIAN_POINT('Ctrl Pts',(-10.2830362607034,-3.93284744093761,
-0.26072768824709));
#91431=CARTESIAN_POINT('Ctrl Pts',(-10.2764726300377,-3.92008288206673,
-0.389270894204289));
#91432=CARTESIAN_POINT('Ctrl Pts',(-10.210533298892,-3.79184798934113,-1.68063743442522));
#91433=CARTESIAN_POINT('Ctrl Pts',(-10.1445939677463,-2.96287287706023,
-2.90241927960841));
#91434=CARTESIAN_POINT('Ctrl Pts',(-10.0786546366006,-1.81029568019072,
-3.49877281080525));
#91435=CARTESIAN_POINT('Ctrl Pts',(-10.0127153054549,-0.657718483321177,
-4.09512634200211));
#91436=CARTESIAN_POINT('Ctrl Pts',(-9.94677597430915,0.818460798136971,
-4.06605155921256));
#91437=CARTESIAN_POINT('Ctrl Pts',(-9.88083664316344,1.94666168747457,-3.42477589133448));
#91438=CARTESIAN_POINT('Ctrl Pts',(-9.81489731201774,3.07486257681215,-2.78350022345642));
#91439=CARTESIAN_POINT('Ctrl Pts',(-9.74895798087205,3.85508507402917,-1.53002367048987));
#91440=CARTESIAN_POINT('Ctrl Pts',(-9.68301864972635,3.93237080570732,-0.234609202223619));
#91441=CARTESIAN_POINT('Ctrl Pts',(-9.61707931858065,4.00965653738547,1.06080526604262));
#91442=CARTESIAN_POINT('Ctrl Pts',(-9.55113998743494,3.38400550352473,2.39815764960857));
#91443=CARTESIAN_POINT('Ctrl Pts',(-9.48520065628923,2.34005455335575,3.16902608362037));
#91444=CARTESIAN_POINT('Ctrl Pts',(-9.41926132514353,1.29610360318675,3.93989451763218));
#91445=CARTESIAN_POINT('Ctrl Pts',(-9.35332199399783,-0.166147263290487,
4.14427900208985));
#91446=CARTESIAN_POINT('Ctrl Pts',(-9.28738266285213,-1.3814542330026,3.6891958247654));
#91447=CARTESIAN_POINT('Ctrl Pts',(-9.22144333170643,-2.59676120271469,
3.23411264744095));
#91448=CARTESIAN_POINT('Ctrl Pts',(-9.15550400056072,-3.56512427566165,
2.11956180833439));
#91449=CARTESIAN_POINT('Ctrl Pts',(-9.08956466941502,-3.84599145228225,
0.852602709542451));
#91450=CARTESIAN_POINT('Ctrl Pts',(-9.07509762028834,-3.90761353991406,
0.574632654262041));
#91451=CARTESIAN_POINT('Ctrl Pts',(-9.06063057116165,-3.93614226116156,
0.289326260823524));
#91452=CARTESIAN_POINT('Ctrl Pts',(-9.04616352203496,-3.93353134025131,
0.00350314687873205));
#91453=CARTESIAN_POINT('Origin',(-14.6,0.,0.));
#91454=CARTESIAN_POINT('',(-7.61283647796501,-3.92679881921828,-0.000798651706886422));
#91455=CARTESIAN_POINT('',(-7.79616352203497,-3.92680118028447,-0.000805323033976586));
#91456=CARTESIAN_POINT('',(-14.6,-3.933,-4.81653586104654E-16));
#91457=CARTESIAN_POINT('Ctrl Pts',(-7.61283647796501,-3.92679881921828,
-0.000798651706886422));
#91458=CARTESIAN_POINT('Ctrl Pts',(-7.64831290436767,-3.92551283842261,
0.703147926407711));
#91459=CARTESIAN_POINT('Ctrl Pts',(-7.68378933077033,-3.74491780739553,
1.40771013463382));
#91460=CARTESIAN_POINT('Ctrl Pts',(-7.71926575717298,-3.38896710896084,
2.00835388494562));
#91461=CARTESIAN_POINT('Ctrl Pts',(-7.78520508831869,-2.72736859536671,
3.12475852792963));
#91462=CARTESIAN_POINT('Ctrl Pts',(-7.85114441946439,-1.45997024859465,
3.88215689869411));
#91463=CARTESIAN_POINT('Ctrl Pts',(-7.91708375061009,-0.163368689798379,
3.93597434747573));
#91464=CARTESIAN_POINT('Ctrl Pts',(-7.98302308175579,1.1332328689979,3.98979179625734));
#91465=CARTESIAN_POINT('Ctrl Pts',(-8.04896241290149,2.45903763981833,3.34002832305605));
#91466=CARTESIAN_POINT('Ctrl Pts',(-8.11490174404719,3.21087728722124,2.2822906123455));
#91467=CARTESIAN_POINT('Ctrl Pts',(-8.1808410751929,3.96271693462414,1.22455290163496));
#91468=CARTESIAN_POINT('Ctrl Pts',(-8.24678040633861,4.14059145860952,-0.241159046584857));
#91469=CARTESIAN_POINT('Ctrl Pts',(-8.31271973748431,3.66357772259559,-1.44802681718783));
#91470=CARTESIAN_POINT('Ctrl Pts',(-8.37865906863001,3.18656398658166,-2.6548945877908));
#91471=CARTESIAN_POINT('Ctrl Pts',(-8.44459839977571,2.05466199056844,-3.60291818077695));
#91472=CARTESIAN_POINT('Ctrl Pts',(-8.51053773092141,0.782824959830684,
-3.86079894258426));
#91473=CARTESIAN_POINT('Ctrl Pts',(-8.57647706206711,-0.489012070907112,
-4.11867970439156));
#91474=CARTESIAN_POINT('Ctrl Pts',(-8.64241639321282,-1.90078413636944,
-3.68641763501997));
#91475=CARTESIAN_POINT('Ctrl Pts',(-8.70835572435852,-2.81021250480815,
-2.76066822900065));
#91476=CARTESIAN_POINT('Ctrl Pts',(-8.75984930889402,-3.52040664471687,
-2.03772860451146));
#91477=CARTESIAN_POINT('Ctrl Pts',(-8.81134289342952,-3.92425061036948,
-1.01383978434024));
#91478=CARTESIAN_POINT('Ctrl Pts',(-8.86283647796501,-3.93354422253028,
0.0035021652868221));
#91479=CARTESIAN_POINT('Ctrl Pts',(-9.04616352203496,-3.93353134025131,
0.00350314687873205));
#91480=CARTESIAN_POINT('Ctrl Pts',(-8.99469124001595,-3.92424195053232,
-1.01342627664713));
#91481=CARTESIAN_POINT('Ctrl Pts',(-8.94321895799693,-3.52076714574602,
-2.03689667730455));
#91482=CARTESIAN_POINT('Ctrl Pts',(-8.89174667597791,-2.81109902180865,
-2.75976519307961));
#91483=CARTESIAN_POINT('Ctrl Pts',(-8.82580734483221,-1.90196813442025,
-3.68580663843232));
#91484=CARTESIAN_POINT('Ctrl Pts',(-8.75986801368651,-0.490335079349264,
-4.11852217066041));
#91485=CARTESIAN_POINT('Ctrl Pts',(-8.69392868254081,0.781584653747444,
-3.86104999454471));
#91486=CARTESIAN_POINT('Ctrl Pts',(-8.6279893513951,2.05350438684415,-3.60357781842901));
#91487=CARTESIAN_POINT('Ctrl Pts',(-8.5620500202494,3.18571079796658,-2.65591793396953));
#91488=CARTESIAN_POINT('Ctrl Pts',(-8.4961106891037,3.66311216968885,-1.44920352732965));
#91489=CARTESIAN_POINT('Ctrl Pts',(-8.430171357958,4.14051354141113,-0.242489120689763));
#91490=CARTESIAN_POINT('Ctrl Pts',(-8.36423202681229,3.96310987373324,1.22327980813051));
#91491=CARTESIAN_POINT('Ctrl Pts',(-8.29829269566659,3.21161008948428,2.28125892096229));
#91492=CARTESIAN_POINT('Ctrl Pts',(-8.23235336452089,2.46011030523531,3.33923803379406));
#91493=CARTESIAN_POINT('Ctrl Pts',(-8.16641403337519,1.13451440441526,3.98942733063732));
#91494=CARTESIAN_POINT('Ctrl Pts',(-8.10047470222949,-0.16210430190959,
3.93602640065455));
#91495=CARTESIAN_POINT('Ctrl Pts',(-8.03453537108379,-1.45872300823444,
3.88262547067178));
#91496=CARTESIAN_POINT('Ctrl Pts',(-7.96859603993807,-2.7263645200641,3.12563431386297));
#91497=CARTESIAN_POINT('Ctrl Pts',(-7.90265670879237,-3.38832158950249,
2.00944232001286));
#91498=CARTESIAN_POINT('Ctrl Pts',(-7.86715897987324,-3.74467905019782,
1.4085523787447));
#91499=CARTESIAN_POINT('Ctrl Pts',(-7.8316612509541,-3.92550363005813,0.703562755676425));
#91500=CARTESIAN_POINT('Ctrl Pts',(-7.79616352203497,-3.92680118028447,
-0.000805323033976586));
#91501=CARTESIAN_POINT('Origin',(-14.6,0.,0.));
#91502=CARTESIAN_POINT('',(-6.36283647796501,-3.93641844162456,-0.00287374819983588));
#91503=CARTESIAN_POINT('',(-6.54616352203497,-3.93642949564762,-0.0028694466954664));
#91504=CARTESIAN_POINT('',(-14.6,-3.933,-4.81653586104654E-16));
#91505=CARTESIAN_POINT('Ctrl Pts',(-6.36283647796501,-3.93641844162456,
-0.00287374819983588));
#91506=CARTESIAN_POINT('Ctrl Pts',(-6.41934358416012,-3.92725780126381,
1.11141212263338));
#91507=CARTESIAN_POINT('Ctrl Pts',(-6.47585069035523,-3.43070555928188,
2.23284140174591));
#91508=CARTESIAN_POINT('Ctrl Pts',(-6.53235779655034,-2.59367156922317,
2.96503814205455));
#91509=CARTESIAN_POINT('Ctrl Pts',(-6.59829712769604,-1.616918994775,3.81945392396189));
#91510=CARTESIAN_POINT('Ctrl Pts',(-6.66423645884175,-0.176530818837051,
4.14384992282044));
#91511=CARTESIAN_POINT('Ctrl Pts',(-6.73017578998745,1.07219546863473,3.79064378039207));
#91512=CARTESIAN_POINT('Ctrl Pts',(-6.79611512113315,2.32092175610655,3.43743763796369));
#91513=CARTESIAN_POINT('Ctrl Pts',(-6.86205445227885,3.37798615511219,2.40662935424836));
#91514=CARTESIAN_POINT('Ctrl Pts',(-6.92799378342455,3.76248243569573,1.16718006917013));
#91515=CARTESIAN_POINT('Ctrl Pts',(-6.99393311457025,4.14697871627925,-0.0722692159080598));
#91516=CARTESIAN_POINT('Ctrl Pts',(-7.05987244571596,3.85890687844073,-1.52035950234914));
#91517=CARTESIAN_POINT('Ctrl Pts',(-7.12581177686166,3.02932378268899,-2.51828926305827));
#91518=CARTESIAN_POINT('Ctrl Pts',(-7.19175110800737,2.19974068693724,-3.51621902376742));
#91519=CARTESIAN_POINT('Ctrl Pts',(-7.25769043915306,0.828646333272257,
-4.06398825874461));
#91520=CARTESIAN_POINT('Ctrl Pts',(-7.32362977029876,-0.46018667072598,
-3.91239205868715));
#91521=CARTESIAN_POINT('Ctrl Pts',(-7.38956910144447,-1.74901967472424,
-3.76079585862969));
#91522=CARTESIAN_POINT('Ctrl Pts',(-7.45550843259018,-2.95559132905574,
-2.90983422353755));
#91523=CARTESIAN_POINT('Ctrl Pts',(-7.52144776373588,-3.53097781601342,
-1.74664794838972));
#91524=CARTESIAN_POINT('Ctrl Pts',(-7.55191066847893,-3.7967970689248,-1.209274698122));
#91525=CARTESIAN_POINT('Ctrl Pts',(-7.58237357322197,-3.92790306545872,
-0.605263636705807));
#91526=CARTESIAN_POINT('Ctrl Pts',(-7.61283647796501,-3.92679881921828,
-0.000798651706886422));
#91527=CARTESIAN_POINT('Ctrl Pts',(-7.79616352203497,-3.92680118028447,
-0.000805323033976586));
#91528=CARTESIAN_POINT('Ctrl Pts',(-7.7657219198084,-3.92791391366382,-0.604846582181445));
#91529=CARTESIAN_POINT('Ctrl Pts',(-7.73528031758184,-3.79699935314037,
-1.2084307468191));
#91530=CARTESIAN_POINT('Ctrl Pts',(-7.70483871535528,-3.5315385167675,-1.74551348775504));
#91531=CARTESIAN_POINT('Ctrl Pts',(-7.63889938420957,-2.95652574754698,
-2.90888447078147));
#91532=CARTESIAN_POINT('Ctrl Pts',(-7.57296005306386,-1.75022758205879,
-3.76023360594288));
#91533=CARTESIAN_POINT('Ctrl Pts',(-7.50702072191815,-0.461443415611824,
-3.91224380701605));
#91534=CARTESIAN_POINT('Ctrl Pts',(-7.44108139077245,0.827340750835101,
-4.06425400808922));
#91535=CARTESIAN_POINT('Ctrl Pts',(-7.37514205962676,2.1986109182408,-3.5169252750742));
#91536=CARTESIAN_POINT('Ctrl Pts',(-7.30920272848106,3.02851449343374,-2.5192621130819));
#91537=CARTESIAN_POINT('Ctrl Pts',(-7.24326339733536,3.85841806862672,-1.52159895108955));
#91538=CARTESIAN_POINT('Ctrl Pts',(-7.17732406618965,4.1469550516069,-0.0736013601199095));
#91539=CARTESIAN_POINT('Ctrl Pts',(-7.11138473504394,3.76285696637598,1.16597130408181));
#91540=CARTESIAN_POINT('Ctrl Pts',(-7.04544540389824,3.37875888114507,2.40554396828349));
#91541=CARTESIAN_POINT('Ctrl Pts',(-6.97950607275254,2.32202572770306,3.43669170571723));
#91542=CARTESIAN_POINT('Ctrl Pts',(-6.91356674160684,1.07341303747873,3.79029894366082));
#91543=CARTESIAN_POINT('Ctrl Pts',(-6.84762741046114,-0.175199652745603,
4.14390618160442));
#91544=CARTESIAN_POINT('Ctrl Pts',(-6.78168807931544,-1.61569187975229,
3.81997292005788));
#91545=CARTESIAN_POINT('Ctrl Pts',(-6.71574874816973,-2.59271881607825,
2.96587099721264));
#91546=CARTESIAN_POINT('Ctrl Pts',(-6.65922033945814,-3.43030356283321,
2.23366729212402));
#91547=CARTESIAN_POINT('Ctrl Pts',(-6.60269193074656,-3.92727496395024,
1.11182810600055));
#91548=CARTESIAN_POINT('Ctrl Pts',(-6.54616352203497,-3.93642949564762,
-0.0028694466954664));
#91549=CARTESIAN_POINT('Origin',(-14.6,0.,0.));
#91550=CARTESIAN_POINT('',(-5.11283647796501,-3.93521788455812,0.00324097164884296));
#91551=CARTESIAN_POINT('',(-5.29616352203496,-3.93520542350542,0.00324387462324732));
#91552=CARTESIAN_POINT('',(-14.6,-3.933,-4.81653586104654E-16));
#91553=CARTESIAN_POINT('Ctrl Pts',(-5.11283647796501,-3.93521788455812,
0.00324097164884296));
#91554=CARTESIAN_POINT('Ctrl Pts',(-5.12443493280686,-3.937249357363,0.23213678076217));
#91555=CARTESIAN_POINT('Ctrl Pts',(-5.13603338764872,-3.91898391613797,
0.460708744038742));
#91556=CARTESIAN_POINT('Ctrl Pts',(-5.14763184249057,-3.87926378197342,
0.685489532446667));
#91557=CARTESIAN_POINT('Ctrl Pts',(-5.21357117363628,-3.65344757494068,
1.96340931091013));
#91558=CARTESIAN_POINT('Ctrl Pts',(-5.27951050478199,-2.73418782810802,
3.11879339388157));
#91559=CARTESIAN_POINT('Ctrl Pts',(-5.3454498359277,-1.53969722382919,3.62600549551672));
#91560=CARTESIAN_POINT('Ctrl Pts',(-5.4113891670734,-0.345206619550455,
4.13321759715182));
#91561=CARTESIAN_POINT('Ctrl Pts',(-5.47732849821909,1.12451484217442,3.99225771745075));
#91562=CARTESIAN_POINT('Ctrl Pts',(-5.54326782936479,2.20082463711376,3.26725485835136));
#91563=CARTESIAN_POINT('Ctrl Pts',(-5.60920716051049,3.27713443205317,2.54225199925191));
#91564=CARTESIAN_POINT('Ctrl Pts',(-5.6751464916562,3.96003256020699,1.2332061607541));
#91565=CARTESIAN_POINT('Ctrl Pts',(-5.74108582280191,3.93883788978656,-0.0643387155085294));
#91566=CARTESIAN_POINT('Ctrl Pts',(-5.80702515394761,3.91764321936612,-1.3618835917711));
#91567=CARTESIAN_POINT('Ctrl Pts',(-5.87296448509331,3.19235575037146,-2.64792750579845));
#91568=CARTESIAN_POINT('Ctrl Pts',(-5.93890381623901,2.09294143612736,-3.33739112751421));
#91569=CARTESIAN_POINT('Ctrl Pts',(-6.00484314738471,0.993527121883229,
-4.02685474922998));
#91570=CARTESIAN_POINT('Ctrl Pts',(-6.07078247853041,-0.480014037610387,
-4.11973807863413));
#91571=CARTESIAN_POINT('Ctrl Pts',(-6.13672180967612,-1.65730176610455,
-3.57378430362403));
#91572=CARTESIAN_POINT('Ctrl Pts',(-6.20266114082182,-2.83458949459872,
-3.02783052861393));
#91573=CARTESIAN_POINT('Ctrl Pts',(-6.26860047196753,-3.71562379209344,
-1.84303964918957));
#91574=CARTESIAN_POINT('Ctrl Pts',(-6.33453980311323,-3.89958245436161,
-0.55842642699929));
#91575=CARTESIAN_POINT('Ctrl Pts',(-6.34397202806382,-3.92589663519989,
-0.374670227540233));
#91576=CARTESIAN_POINT('Ctrl Pts',(-6.35340425301442,-3.93794754524342,
-0.188871504954147));
#91577=CARTESIAN_POINT('Ctrl Pts',(-6.36283647796501,-3.93641844162456,
-0.00287374819983588));
#91578=CARTESIAN_POINT('Ctrl Pts',(-6.54616352203497,-3.93642949564762,
-0.0028694466954664));
#91579=CARTESIAN_POINT('Ctrl Pts',(-6.53675259960086,-3.93795355389883,
-0.188445733822925));
#91580=CARTESIAN_POINT('Ctrl Pts',(-6.52734167716674,-3.92595726999319,
-0.373824083294776));
#91581=CARTESIAN_POINT('Ctrl Pts',(-6.51793075473263,-3.89976141760876,
-0.557173686627855));
#91582=CARTESIAN_POINT('Ctrl Pts',(-6.45199142358692,-3.71621543716804,
-1.84184586347916));
#91583=CARTESIAN_POINT('Ctrl Pts',(-6.38605209244122,-2.83556183064135,
-3.02691963303782));
#91584=CARTESIAN_POINT('Ctrl Pts',(-6.32011276129552,-1.65844960882676,
-3.5732515341523));
#91585=CARTESIAN_POINT('Ctrl Pts',(-6.25417343014981,-0.481337387012155,
-4.1195834352668));
#91586=CARTESIAN_POINT('Ctrl Pts',(-6.18823409900411,0.992233450090349,
-4.02717346793708));
#91587=CARTESIAN_POINT('Ctrl Pts',(-6.12229476785841,2.09186912464122,-3.33806309059033));
#91588=CARTESIAN_POINT('Ctrl Pts',(-6.05635543671271,3.1915047991921,-2.64895271324358));
#91589=CARTESIAN_POINT('Ctrl Pts',(-5.990416105567,3.91720531119132,-1.3631419258798));
#91590=CARTESIAN_POINT('Ctrl Pts',(-5.9244767744213,3.93881679526393,-0.0656039986291013));
#91591=CARTESIAN_POINT('Ctrl Pts',(-5.85853744327559,3.96042827933653,1.23193392862154));
#91592=CARTESIAN_POINT('Ctrl Pts',(-5.79259811212989,3.27795073548254,2.54119899575913));
#91593=CARTESIAN_POINT('Ctrl Pts',(-5.72665878098419,2.20187395307353,3.26654752392988));
#91594=CARTESIAN_POINT('Ctrl Pts',(-5.66071944983849,1.12579717066446,3.99189605210066));
#91595=CARTESIAN_POINT('Ctrl Pts',(-5.59478011869279,-0.34387885029961,
4.13332804130459));
#91596=CARTESIAN_POINT('Ctrl Pts',(-5.52884078754709,-1.53853225927603,
3.6264997061618));
#91597=CARTESIAN_POINT('Ctrl Pts',(-5.46290145640139,-2.73318566825241,
3.11967137101902));
#91598=CARTESIAN_POINT('Ctrl Pts',(-5.39696212525568,-3.65281646524112,
1.96458271152948));
#91599=CARTESIAN_POINT('Ctrl Pts',(-5.33102279410998,-3.8790431592278,0.686735611229462));
#91600=CARTESIAN_POINT('Ctrl Pts',(-5.31940303675164,-3.91890858167644,
0.461554782298517));
#91601=CARTESIAN_POINT('Ctrl Pts',(-5.3077832793933,-3.93724165312964,0.232561922513211));
#91602=CARTESIAN_POINT('Ctrl Pts',(-5.29616352203496,-3.93520542350542,
0.00324387462324732));
#91603=CARTESIAN_POINT('Origin',(-14.6,0.,0.));
#91604=CARTESIAN_POINT('',(-3.86283647796501,-3.9266497763299,0.000109410655622921));
#91605=CARTESIAN_POINT('',(-4.04616352203497,-3.92664918805101,0.000102552286748496));
#91606=CARTESIAN_POINT('',(-14.6,-3.933,-4.81653586104654E-16));
#91607=CARTESIAN_POINT('Ctrl Pts',(-3.86283647796501,-3.9266497763299,0.000109410655622921));
#91608=CARTESIAN_POINT('Ctrl Pts',(-3.89546561259932,-3.92681141280058,
0.647619536085308));
#91609=CARTESIAN_POINT('Ctrl Pts',(-3.92809474723363,-3.77541687798498,
1.29505849841556));
#91610=CARTESIAN_POINT('Ctrl Pts',(-3.96072388186793,-3.47204825468472,
1.86103845086822));
#91611=CARTESIAN_POINT('Ctrl Pts',(-4.02666321301364,-2.858978851061,3.00481195037645));
#91612=CARTESIAN_POINT('Ctrl Pts',(-4.09260254415934,-1.62525837440169,
3.81591280553418));
#91613=CARTESIAN_POINT('Ctrl Pts',(-4.15854187530505,-0.332161796206972,
3.92533463561106));
#91614=CARTESIAN_POINT('Ctrl Pts',(-4.22448120645075,0.960934781987714,
4.03475646568794));
#91615=CARTESIAN_POINT('Ctrl Pts',(-4.29042053759645,2.31340746171779,3.44249927068401));
#91616=CARTESIAN_POINT('Ctrl Pts',(-4.35635986874215,3.10995543804893,2.41800756422801));
#91617=CARTESIAN_POINT('Ctrl Pts',(-4.42229919988785,3.90650341438011,1.39351585777196));
#91618=CARTESIAN_POINT('Ctrl Pts',(-4.48823853103356,4.14712668731228,-0.0632103601362513));
#91619=CARTESIAN_POINT('Ctrl Pts',(-4.55417786217927,3.72235490549252,-1.28944070187289));
#91620=CARTESIAN_POINT('Ctrl Pts',(-4.62011719332497,3.29758312367278,-2.51567104360945));
#91621=CARTESIAN_POINT('Ctrl Pts',(-4.68605652447066,2.20741628710125,-3.51140550917451));
#91622=CARTESIAN_POINT('Ctrl Pts',(-4.75199585561636,0.947820406481901,
-3.82363961182173));
#91623=CARTESIAN_POINT('Ctrl Pts',(-4.81793518676207,-0.311775474137514,
-4.13587371446897));
#91624=CARTESIAN_POINT('Ctrl Pts',(-4.88387451790777,-1.74080039880474,
-3.76460745419828));
#91625=CARTESIAN_POINT('Ctrl Pts',(-4.94981384905348,-2.68912652752191,
-2.8787465870852));
#91626=CARTESIAN_POINT('Ctrl Pts',(-5.00415472535732,-3.47064602371538,
-2.1487049720764));
#91627=CARTESIAN_POINT('Ctrl Pts',(-5.05849560166116,-3.92570006395965,
-1.06917764092437));
#91628=CARTESIAN_POINT('Ctrl Pts',(-5.11283647796501,-3.93521788455812,
0.00324097164884296));
#91629=CARTESIAN_POINT('Ctrl Pts',(-5.29616352203496,-3.93520542350542,
0.00324387462324732));
#91630=CARTESIAN_POINT('Ctrl Pts',(-5.2418439482476,-3.92568653925424,-1.06876290133542));
#91631=CARTESIAN_POINT('Ctrl Pts',(-5.18752437446023,-3.47102960783475,
-2.14787613604391));
#91632=CARTESIAN_POINT('Ctrl Pts',(-5.13320480067287,-2.69005098778536,
-2.87788243582242));
#91633=CARTESIAN_POINT('Ctrl Pts',(-5.06726546952716,-1.74200953137151,
-3.76404784146379));
#91634=CARTESIAN_POINT('Ctrl Pts',(-5.00132613838146,-0.313104027559104,
-4.13577311163589));
#91635=CARTESIAN_POINT('Ctrl Pts',(-4.93538680723576,0.946592018069592,
-3.82394366910327));
#91636=CARTESIAN_POINT('Ctrl Pts',(-4.86944747609006,2.20628806369818,-3.51211422657067));
#91637=CARTESIAN_POINT('Ctrl Pts',(-4.80350814494435,3.29677465114311,-2.51673007133348));
#91638=CARTESIAN_POINT('Ctrl Pts',(-4.73756881379865,3.72194029202664,-1.29063631219266));
#91639=CARTESIAN_POINT('Ctrl Pts',(-4.67162948265295,4.1471059329102,-0.0645425530517454));
#91640=CARTESIAN_POINT('Ctrl Pts',(-4.60569015150725,3.90695062723229,1.3922608099928));
#91641=CARTESIAN_POINT('Ctrl Pts',(-4.53975082036155,3.11073184340648,2.41700828104648));
#91642=CARTESIAN_POINT('Ctrl Pts',(-4.47381148921585,2.31451305958069,3.44175575210011));
#91643=CARTESIAN_POINT('Ctrl Pts',(-4.40787215807014,0.962230797607039,
4.03444733116288));
#91644=CARTESIAN_POINT('Ctrl Pts',(-4.34193282692444,-0.330900798702454,
3.92544090568989));
#91645=CARTESIAN_POINT('Ctrl Pts',(-4.27599349577874,-1.62403239501198,
3.8164344802169));
#91646=CARTESIAN_POINT('Ctrl Pts',(-4.21005416463304,-2.85801332565737,
3.00573005020813));
#91647=CARTESIAN_POINT('Ctrl Pts',(-4.14411483348733,-3.4714500665587,1.86215360266608));
#91648=CARTESIAN_POINT('Ctrl Pts',(-4.11146439633654,-3.77519863978166,
1.29590171204423));
#91649=CARTESIAN_POINT('Ctrl Pts',(-4.07881395918575,-3.92680082759742,
0.648035530114968));
#91650=CARTESIAN_POINT('Ctrl Pts',(-4.04616352203497,-3.92664918805101,
0.000102552286748496));
#91651=CARTESIAN_POINT('Origin',(-14.6,0.,0.));
#91652=CARTESIAN_POINT('',(-2.61283647796502,-3.93482597683023,-0.00332506251532583));
#91653=CARTESIAN_POINT('',(-2.79616352203497,-3.93483613066414,-0.00332402043238414));
#91654=CARTESIAN_POINT('',(-14.6,-3.933,-4.81653586104654E-16));
#91655=CARTESIAN_POINT('Ctrl Pts',(-2.61283647796502,-3.93482597683023,
-0.00332506251532583));
#91656=CARTESIAN_POINT('Ctrl Pts',(-2.66649629239178,-3.92529592795581,
1.05592713778507));
#91657=CARTESIAN_POINT('Ctrl Pts',(-2.72015610681853,-3.48282948623788,
2.12219777834594));
#91658=CARTESIAN_POINT('Ctrl Pts',(-2.77381592124529,-2.718548420221,2.85097673606072));
#91659=CARTESIAN_POINT('Ctrl Pts',(-2.83975525239099,-1.77936920689613,
3.74652953545347));
#91660=CARTESIAN_POINT('Ctrl Pts',(-2.9056945835367,-0.354234475111307,
4.13245370603341));
#91661=CARTESIAN_POINT('Ctrl Pts',(-2.97163391468241,0.90850115995116,3.83317244788512));
#91662=CARTESIAN_POINT('Ctrl Pts',(-3.03757324582811,2.17123679501352,3.53389118973686));
#91663=CARTESIAN_POINT('Ctrl Pts',(-3.1035125769738,3.27157333335356,2.5494045028605));
#91664=CARTESIAN_POINT('Ctrl Pts',(-3.1694519081195,3.70891632543792,1.32760105294568));
#91665=CARTESIAN_POINT('Ctrl Pts',(-3.23539123926521,4.1462593175223,0.10579760303079));
#91666=CARTESIAN_POINT('Ctrl Pts',(-3.30133057041091,3.92060876335093,-1.35332260992259));
#91667=CARTESIAN_POINT('Ctrl Pts',(-3.36726990155662,3.13462419475558,-2.38594073109377));
#91668=CARTESIAN_POINT('Ctrl Pts',(-3.43320923270232,2.34863962616026,-3.41855885226493));
#91669=CARTESIAN_POINT('Ctrl Pts',(-3.49914856384802,1.00232104314098,-4.02467488165392));
#91670=CARTESIAN_POINT('Ctrl Pts',(-3.56508789499372,-0.291831044969713,
-3.92853896723417));
#91671=CARTESIAN_POINT('Ctrl Pts',(-3.63102722613942,-1.58598313308048,
-3.83240305281441));
#91672=CARTESIAN_POINT('Ctrl Pts',(-3.69696655728513,-2.82796872628265,
-3.03401519458584));
#91673=CARTESIAN_POINT('Ctrl Pts',(-3.76290588843083,-3.45275235758963,
-1.89659819354216));
#91674=CARTESIAN_POINT('Ctrl Pts',(-3.79621608494223,-3.76837074762076,
-1.32201572262741));
#91675=CARTESIAN_POINT('Ctrl Pts',(-3.82952628145362,-3.92648476605112,
-0.660916073560029));
#91676=CARTESIAN_POINT('Ctrl Pts',(-3.86283647796501,-3.9266497763299,0.000109410655622921));
#91677=CARTESIAN_POINT('Ctrl Pts',(-4.04616352203497,-3.92664918805101,
0.000102552286748496));
#91678=CARTESIAN_POINT('Ctrl Pts',(-4.01287462804005,-3.92649458329757,
-0.660500309326387));
#91679=CARTESIAN_POINT('Ctrl Pts',(-3.97958573404514,-3.76859324143987,
-1.32117260467504));
#91680=CARTESIAN_POINT('Ctrl Pts',(-3.94629684005023,-3.45336120237453,
-1.8954888688236));
#91681=CARTESIAN_POINT('Ctrl Pts',(-3.88035750890452,-2.82894304613174,
-3.033106427696));
#91682=CARTESIAN_POINT('Ctrl Pts',(-3.81441817775881,-1.58721418248879,
-3.83189308036553));
#91683=CARTESIAN_POINT('Ctrl Pts',(-3.74847884661311,-0.293093059405651,
-3.92844475050617));
#91684=CARTESIAN_POINT('Ctrl Pts',(-3.68253951546741,1.00102806367751,-4.02499642064681));
#91685=CARTESIAN_POINT('Ctrl Pts',(-3.61660018432172,2.34754144620083,-3.41931310825863));
#91686=CARTESIAN_POINT('Ctrl Pts',(-3.55066085317602,3.13385753223803,-2.38694750757919));
#91687=CARTESIAN_POINT('Ctrl Pts',(-3.48472152203031,3.92017361827524,-1.35458190689974));
#91688=CARTESIAN_POINT('Ctrl Pts',(-3.4187821908846,4.14629240782621,0.104465982070971));
#91689=CARTESIAN_POINT('Ctrl Pts',(-3.3528428597389,3.70934215864998,1.3264096424498));
#91690=CARTESIAN_POINT('Ctrl Pts',(-3.28690352859319,3.27239190947374,2.54835330282863));
#91691=CARTESIAN_POINT('Ctrl Pts',(-3.2209641974475,2.1723726215703,3.53319273461559));
#91692=CARTESIAN_POINT('Ctrl Pts',(-3.15502486630179,0.909732860103698,
3.83287987540983));
#91693=CARTESIAN_POINT('Ctrl Pts',(-3.08908553515609,-0.35290690136287,
4.13256701620405));
#91694=CARTESIAN_POINT('Ctrl Pts',(-3.02314620401039,-1.77816713639261,
3.74710186600559));
#91695=CARTESIAN_POINT('Ctrl Pts',(-2.95720687286468,-2.71763315930033,
2.85185032219934));
#91696=CARTESIAN_POINT('Ctrl Pts',(-2.90352575592145,-3.48245113005701,
2.12302729682641));
#91697=CARTESIAN_POINT('Ctrl Pts',(-2.84984463897821,-3.92530581696798,
1.05634001278133));
#91698=CARTESIAN_POINT('Ctrl Pts',(-2.79616352203497,-3.93483613066414,
-0.00332402043238414));
#91699=CARTESIAN_POINT('Origin',(-14.6,0.,0.));
#91700=CARTESIAN_POINT('',(-1.36283647796502,-3.93682057842306,0.00276514463350926));
#91701=CARTESIAN_POINT('',(-1.54616352203498,-3.93676751258924,0.00274060645320142));
#91702=CARTESIAN_POINT('',(-14.6,-3.933,-4.81653586104654E-16));
#91703=CARTESIAN_POINT('Ctrl Pts',(-1.36283647796502,-3.93682057842306,
0.00276514463350926));
#91704=CARTESIAN_POINT('Ctrl Pts',(-1.37158764103853,-3.93820694651525,
0.175305934189915));
#91705=CARTESIAN_POINT('Ctrl Pts',(-1.38033880411203,-3.92785596749255,
0.347679209261104));
#91706=CARTESIAN_POINT('Ctrl Pts',(-1.38908996718554,-3.90520506174835,
0.518417021592109));
#91707=CARTESIAN_POINT('Ctrl Pts',(-1.45502929833124,-3.73453225379453,
1.8049131195188));
#91708=CARTESIAN_POINT('Ctrl Pts',(-1.52096862947694,-2.86553049728958,
2.99855573940384));
#91709=CARTESIAN_POINT('Ctrl Pts',(-1.58690796062265,-1.69386838589715,
3.55653944458954));
#91710=CARTESIAN_POINT('Ctrl Pts',(-1.65284729176835,-0.522206274504723,
4.11452314977523));
#91711=CARTESIAN_POINT('Ctrl Pts',(-1.71878662291405,0.952116191775279,
4.03684794026153));
#91712=CARTESIAN_POINT('Ctrl Pts',(-1.78472595405975,2.05853064267987,3.35872836780381));
#91713=CARTESIAN_POINT('Ctrl Pts',(-1.85066528520546,3.16494509358447,2.6806087953461));
#91714=CARTESIAN_POINT('Ctrl Pts',(-1.91660461635116,3.90345152911377,1.40204485994436));
#91715=CARTESIAN_POINT('Ctrl Pts',(-1.98254394749686,3.93798269334203,0.104777353878543));
#91716=CARTESIAN_POINT('Ctrl Pts',(-2.04848327864256,3.9725138575703,-1.19249015218735));
#91717=CARTESIAN_POINT('Ctrl Pts',(-2.11442260978827,3.30306975049746,-2.50846122891732));
#91718=CARTESIAN_POINT('Ctrl Pts',(-2.18036194093398,2.2342563079641,-3.24447498598491));
#91719=CARTESIAN_POINT('Ctrl Pts',(-2.24630127207968,1.16544286543083,-3.98048874305243));
#91720=CARTESIAN_POINT('Ctrl Pts',(-2.31224060322537,-0.30273991256285,
-4.13654518045766));
#91721=CARTESIAN_POINT('Ctrl Pts',(-2.37817993437107,-1.50237335701287,
-3.64162961614031));
#91722=CARTESIAN_POINT('Ctrl Pts',(-2.44411926551678,-2.70200680146297,
-3.14671405182294));
#91723=CARTESIAN_POINT('Ctrl Pts',(-2.51005859666248,-3.63309091236934,
-2.00082648578291));
#91724=CARTESIAN_POINT('Ctrl Pts',(-2.57599792780818,-3.87202112039005,
-0.725291988660146));
#91725=CARTESIAN_POINT('Ctrl Pts',(-2.58827744452713,-3.91651577074627,
-0.48775625830218));
#91726=CARTESIAN_POINT('Ctrl Pts',(-2.60055696124607,-3.93700683406457,
-0.245724430499025));
#91727=CARTESIAN_POINT('Ctrl Pts',(-2.61283647796502,-3.93482597683023,
-0.00332506251532583));
#91728=CARTESIAN_POINT('Ctrl Pts',(-2.79616352203497,-3.93483613066414,
-0.00332402043238414));
#91729=CARTESIAN_POINT('Ctrl Pts',(-2.78390530783251,-3.93701240108019,
-0.245300891284708));
#91730=CARTESIAN_POINT('Ctrl Pts',(-2.77164709363004,-3.9165930421361,-0.486911535858293));
#91731=CARTESIAN_POINT('Ctrl Pts',(-2.75938887942757,-3.87225203266108,
-0.724049240203662));
#91732=CARTESIAN_POINT('Ctrl Pts',(-2.69344954828187,-3.63373307232837,
-1.99965932138625));
#91733=CARTESIAN_POINT('Ctrl Pts',(-2.62751021713617,-2.70302334087727,
-3.14584154633738));
#91734=CARTESIAN_POINT('Ctrl Pts',(-2.56157088599047,-1.50354618345133,
-3.64114439342657));
#91735=CARTESIAN_POINT('Ctrl Pts',(-2.49563155484477,-0.304069026025359,
-4.13644724051578));
#91736=CARTESIAN_POINT('Ctrl Pts',(-2.42969222369907,1.16417555737546,-3.98087070974302));
#91737=CARTESIAN_POINT('Ctrl Pts',(-2.36375289255336,2.23321990412611,-3.24519659418834));
#91738=CARTESIAN_POINT('Ctrl Pts',(-2.29781356140766,3.30226425087672,-2.50952247863368));
#91739=CARTESIAN_POINT('Ctrl Pts',(-2.23187423026196,3.97210836097718,-1.19375077829715));
#91740=CARTESIAN_POINT('Ctrl Pts',(-2.16593489911625,3.93800429215139,0.103520445762184));
#91741=CARTESIAN_POINT('Ctrl Pts',(-2.09999556797055,3.90390022332561,1.40079166982155));
#91742=CARTESIAN_POINT('Ctrl Pts',(-2.03405623682485,3.16584797557354,2.67956241760371));
#91743=CARTESIAN_POINT('Ctrl Pts',(-1.96811690567915,2.05963163241508,3.35805118788789));
#91744=CARTESIAN_POINT('Ctrl Pts',(-1.90217757453345,0.953415289256656,
4.03653995817205));
#91745=CARTESIAN_POINT('Ctrl Pts',(-1.83623824338775,-0.520965149308136,
4.11474675095826));
#91746=CARTESIAN_POINT('Ctrl Pts',(-1.77029891224204,-1.69276836578185,
3.5571129497935));
#91747=CARTESIAN_POINT('Ctrl Pts',(-1.70435958109634,-2.8645715822556,2.99947914862873));
#91748=CARTESIAN_POINT('Ctrl Pts',(-1.63842024995063,-3.73379757663826,
1.80600475351295));
#91749=CARTESIAN_POINT('Ctrl Pts',(-1.57248091880493,-3.90495648382779,
0.519614505660644));
#91750=CARTESIAN_POINT('Ctrl Pts',(-1.56370845321495,-3.92772719741634,
0.348475156982074));
#91751=CARTESIAN_POINT('Ctrl Pts',(-1.55493598762496,-3.93814266395565,
0.175691269638936));
#91752=CARTESIAN_POINT('Ctrl Pts',(-1.54616352203498,-3.93676751258924,
0.00274060645320142));
#91753=CARTESIAN_POINT('Origin',(-31.5777734492731,0.,0.));
#91754=CARTESIAN_POINT('',(-0.952773449273097,-3.22588063033637,0.00226579452538821));
#91755=CARTESIAN_POINT('',(-0.7062265507269,-3.21712659271395,0.000156184947003868));
#91756=CARTESIAN_POINT('',(-31.5777734492731,-3.22275,-1.53308031181269E-14));
#91757=CARTESIAN_POINT('',(-0.399999999999999,3.01795629612512,-1.14523995189157));
#91758=CARTESIAN_POINT('Ctrl Pts',(-0.952773449273097,-3.22588063033637,
0.00226579452538841));
#91759=CARTESIAN_POINT('Ctrl Pts',(-0.895585281200896,-3.21845690948414,
-0.921655251058599));
#91760=CARTESIAN_POINT('Ctrl Pts',(-0.772457781982996,-2.31816799471971,
-2.9235001872406));
#91761=CARTESIAN_POINT('Ctrl Pts',(-0.588199965558632,0.985855557350958,
-3.63123937118558));
#91762=CARTESIAN_POINT('Ctrl Pts',(-0.461130317206463,2.66302220805322,
-2.06570245611714));
#91763=CARTESIAN_POINT('Ctrl Pts',(-0.399999999999999,3.01796675574746,
-1.14524144678479));
#91764=CARTESIAN_POINT('',(-0.400000000000005,-0.101608697681796,-3.22114781328883));
#91765=CARTESIAN_POINT('Origin',(-0.4,0.,0.));
#91766=CARTESIAN_POINT('Ctrl Pts',(-0.706226550726901,-3.21712659271395,
0.000156184947003798));
#91767=CARTESIAN_POINT('Ctrl Pts',(-0.670090364963638,-3.21533286770883,
-0.587810425121163));
#91768=CARTESIAN_POINT('Ctrl Pts',(-0.568014848054673,-2.77994359672653,
-2.24993778652945));
#91769=CARTESIAN_POINT('Ctrl Pts',(-0.465939331145708,-1.16924921554908,
-3.18746989196983));
#91770=CARTESIAN_POINT('Ctrl Pts',(-0.400000000000005,-0.101608697681796,
-3.22114781328883));
#91771=CARTESIAN_POINT('Origin',(-31.5777734492731,0.,0.));
#91772=CARTESIAN_POINT('',(-2.20277344927309,-3.22424622853537,-0.00272459832720938));
#91773=CARTESIAN_POINT('',(-1.9562265507269,-3.2258371475202,0.00224568762937409));
#91774=CARTESIAN_POINT('',(-31.5777734492731,-3.22275,-1.53308031181269E-14));
#91775=CARTESIAN_POINT('Ctrl Pts',(-2.20277344927309,-3.22424622853537,
-0.00272459832720937));
#91776=CARTESIAN_POINT('Ctrl Pts',(-2.19049393255415,-3.22603325056741,
-0.201349709735698));
#91777=CARTESIAN_POINT('Ctrl Pts',(-2.1122750846895,-3.11907918299394,-1.4646462045877));
#91778=CARTESIAN_POINT('Ctrl Pts',(-1.96811690567914,-1.45111647622458,
-3.51741211898495));
#91779=CARTESIAN_POINT('Ctrl Pts',(-1.77029891224204,2.15802619942714,-3.13378825655336));
#91780=CARTESIAN_POINT('Ctrl Pts',(-1.57248091880493,3.80367913311811,0.10118183309678));
#91781=CARTESIAN_POINT('Ctrl Pts',(-1.37466292536782,1.98825456019507,3.24419626697628));
#91782=CARTESIAN_POINT('Ctrl Pts',(-1.17684493193072,-1.63598093042552,
3.4351404175943));
#91783=CARTESIAN_POINT('Ctrl Pts',(-1.03621510656581,-3.15462579133896,
1.3491616299952));
#91784=CARTESIAN_POINT('Ctrl Pts',(-0.9615246123466,-3.22701663790542,0.143647902214853));
#91785=CARTESIAN_POINT('Ctrl Pts',(-0.952773449273097,-3.22588063033637,
0.00226579452538841));
#91786=CARTESIAN_POINT('Ctrl Pts',(-1.9562265507269,-3.2258371475202,0.00224568762937397));
#91787=CARTESIAN_POINT('Ctrl Pts',(-1.89905968517118,-3.21849410771212,
-0.921277086382614));
#91788=CARTESIAN_POINT('Ctrl Pts',(-1.77595348846977,-2.31915348223847,
-2.92253791405406));
#91789=CARTESIAN_POINT('Ctrl Pts',(-1.58690796062265,1.07186168277273,-3.65071665635791));
#91790=CARTESIAN_POINT('Ctrl Pts',(-1.38908996718554,3.64542809306271,-1.09141468478898));
#91791=CARTESIAN_POINT('Ctrl Pts',(-1.19127197374844,2.90115349698225,2.46187399806776));
#91792=CARTESIAN_POINT('Ctrl Pts',(-0.993453980311327,-0.481122552182907,
3.77336366075504));
#91793=CARTESIAN_POINT('Ctrl Pts',(-0.831772172637481,-2.89047138994435,
2.04190708737574));
#91794=CARTESIAN_POINT('Ctrl Pts',(-0.736029696109339,-3.21860595878357,
0.485078818306275));
#91795=CARTESIAN_POINT('Ctrl Pts',(-0.706226550726901,-3.21712659271395,
0.000156184947003798));
#91796=CARTESIAN_POINT('Origin',(-31.5777734492731,0.,0.));
#91797=CARTESIAN_POINT('',(-3.45277344927309,-3.21754654631761,8.96524766731527E-5));
#91798=CARTESIAN_POINT('',(-3.20622655072689,-3.22425454871545,-0.00272374443152645));
#91799=CARTESIAN_POINT('',(-31.5777734492731,-3.22275,-1.53308031181269E-14));
#91800=CARTESIAN_POINT('Ctrl Pts',(-3.45277344927309,-3.21754654631761,
8.96524766732035E-5));
#91801=CARTESIAN_POINT('Ctrl Pts',(-3.41946325276169,-3.21741133480582,
-0.541562999253872));
#91802=CARTESIAN_POINT('Ctrl Pts',(-3.32021372510459,-2.8313784513742,-2.15562737063988));
#91803=CARTESIAN_POINT('Ctrl Pts',(-3.15502486630179,-0.281875939904123,
-3.79452870799989));
#91804=CARTESIAN_POINT('Ctrl Pts',(-2.95720687286468,3.02769554249517,-2.30455126046869));
#91805=CARTESIAN_POINT('Ctrl Pts',(-2.75938887942757,3.58239830638208,1.28231347354763));
#91806=CARTESIAN_POINT('Ctrl Pts',(-2.56157088599047,0.877509230153572,
3.70241604420433));
#91807=CARTESIAN_POINT('Ctrl Pts',(-2.37603240927231,-2.40834311719199,
2.81261256561713));
#91808=CARTESIAN_POINT('Ctrl Pts',(-2.25643326369985,-3.21643718581731,
0.865240066945609));
#91809=CARTESIAN_POINT('Ctrl Pts',(-2.20277344927309,-3.22424622853537,
-0.00272459832720937));
#91810=CARTESIAN_POINT('Ctrl Pts',(-3.20622655072689,-3.22425454871545,
-0.00272374443152663));
#91811=CARTESIAN_POINT('Ctrl Pts',(-3.19396833652443,-3.22603781225048,
-0.201002656340778));
#91812=CARTESIAN_POINT('Ctrl Pts',(-3.11577079117626,-3.11930186990163,
-1.46394827087633));
#91813=CARTESIAN_POINT('Ctrl Pts',(-2.9716339146824,-1.45225621275822,-3.51693862418514));
#91814=CARTESIAN_POINT('Ctrl Pts',(-2.7738159212453,2.15703839529281,-3.13449448646742));
#91815=CARTESIAN_POINT('Ctrl Pts',(-2.57599792780818,3.80367463162103,0.0999854885590033));
#91816=CARTESIAN_POINT('Ctrl Pts',(-2.37817993437108,1.98936656034495,3.24350831648798));
#91817=CARTESIAN_POINT('Ctrl Pts',(-2.18036194093398,-1.63501143994855,
3.43575922529938));
#91818=CARTESIAN_POINT('Ctrl Pts',(-2.03971081305258,-3.15427827586105,
1.34975848472338));
#91819=CARTESIAN_POINT('Ctrl Pts',(-1.96499901631689,-3.22696396396214,
0.14396365096069));
#91820=CARTESIAN_POINT('Ctrl Pts',(-1.9562265507269,-3.2258371475202,0.00224568762937397));
#91821=CARTESIAN_POINT('Origin',(-31.5777734492731,0.,0.));
#91822=CARTESIAN_POINT('',(-4.70277344927309,-3.22456736268998,0.00265569320671698));
#91823=CARTESIAN_POINT('',(-4.45622655072689,-3.21754606427445,8.40326422851811E-5));
#91824=CARTESIAN_POINT('',(-31.5777734492731,-3.22275,-1.53308031181269E-14));
#91825=CARTESIAN_POINT('Ctrl Pts',(-4.70277344927309,-3.22456736268998,
0.00265569320671703));
#91826=CARTESIAN_POINT('Ctrl Pts',(-4.64843257296924,-3.21676833997614,
-0.876097696996831));
#91827=CARTESIAN_POINT('Ctrl Pts',(-4.52815236551969,-2.39142780303548,
-2.83405782554972));
#91828=CARTESIAN_POINT('Ctrl Pts',(-4.34193282692443,0.91548834647712,-3.69320756511369));
#91829=CARTESIAN_POINT('Ctrl Pts',(-4.14411483348733,3.59537787550923,-1.24545527762321));
#91830=CARTESIAN_POINT('Ctrl Pts',(-3.94629684005022,3.00386860560673,2.33552444683395));
#91831=CARTESIAN_POINT('Ctrl Pts',(-3.74847884661311,-0.320831111098236,
3.79143358123437));
#91832=CARTESIAN_POINT('Ctrl Pts',(-3.5839710496874,-2.84292582825253,2.13330013806421));
#91833=CARTESIAN_POINT('Ctrl Pts',(-3.48540258390739,-3.21767899328834,
0.530667648085214));
#91834=CARTESIAN_POINT('Ctrl Pts',(-3.45277344927309,-3.21754654631761,
8.96524766732035E-5));
#91835=CARTESIAN_POINT('Ctrl Pts',(-4.45622655072689,-3.21754606427445,
8.40326422848689E-5));
#91836=CARTESIAN_POINT('Ctrl Pts',(-4.42293765673198,-3.21741937918185,
-0.541222316776413));
#91837=CARTESIAN_POINT('Ctrl Pts',(-4.32370943159137,-2.83174183907037,
-2.15492909527557));
#91838=CARTESIAN_POINT('Ctrl Pts',(-4.15854187530505,-0.283095044828532,
-3.79443760733249));
#91839=CARTESIAN_POINT('Ctrl Pts',(-3.96072388186794,3.02695530111143,-2.30552388116989));
#91840=CARTESIAN_POINT('Ctrl Pts',(-3.76290588843083,3.58280909899496,1.28116306328493));
#91841=CARTESIAN_POINT('Ctrl Pts',(-3.56508789499372,0.878699899841087,
3.70213276488018));
#91842=CARTESIAN_POINT('Ctrl Pts',(-3.37952811575908,-2.40781911009861,
2.81328558268817));
#91843=CARTESIAN_POINT('Ctrl Pts',(-3.25990766767013,-3.21644528899918,
0.865578381945218));
#91844=CARTESIAN_POINT('Ctrl Pts',(-3.20622655072689,-3.22425454871545,
-0.00272374443152663));
#91845=CARTESIAN_POINT('Origin',(-31.5777734492731,0.,0.));
#91846=CARTESIAN_POINT('',(-5.95277344927308,-3.22555111435178,-0.00235478566260707));
#91847=CARTESIAN_POINT('',(-5.70622655072688,-3.22455715194561,0.0026580719403356));
#91848=CARTESIAN_POINT('',(-31.5777734492731,-3.22275,-1.53308031181269E-14));
#91849=CARTESIAN_POINT('Ctrl Pts',(-5.95277344927308,-3.22555111435178,
-0.00235478566260758));
#91850=CARTESIAN_POINT('Ctrl Pts',(-5.94334122432249,-3.22680408121872,
-0.154763702667427));
#91851=CARTESIAN_POINT('Ctrl Pts',(-5.86796966822619,-3.14789702397088,
-1.37133825070766));
#91852=CARTESIAN_POINT('Ctrl Pts',(-5.72665878098419,-1.60076786459875,
-3.45187532233801));
#91853=CARTESIAN_POINT('Ctrl Pts',(-5.52884078754708,2.02154698800078,-3.22354599370549));
#91854=CARTESIAN_POINT('Ctrl Pts',(-5.33102279410997,3.80447619524911,-0.0621439922320252));
#91855=CARTESIAN_POINT('Ctrl Pts',(-5.13320480067286,2.12575007586871,3.15580221373199));
#91856=CARTESIAN_POINT('Ctrl Pts',(-4.93538680723576,-1.48717505057987,
3.50231514455317));
#91857=CARTESIAN_POINT('Ctrl Pts',(-4.7919096901025,-3.12617529492704,1.44231545368255));
#91858=CARTESIAN_POINT('Ctrl Pts',(-4.71437190411494,-3.22623197722897,
0.190215817493454));
#91859=CARTESIAN_POINT('Ctrl Pts',(-4.70277344927309,-3.22456736268998,
0.00265569320671703));
#91860=CARTESIAN_POINT('Ctrl Pts',(-5.70622655072688,-3.22455715194561,
0.0026580719403353));
#91861=CARTESIAN_POINT('Ctrl Pts',(-5.65190697693952,-3.21675725766117,
-0.875757854126423));
#91862=CARTESIAN_POINT('Ctrl Pts',(-5.53164807200646,-2.39195967703322,
-2.83338771458464));
#91863=CARTESIAN_POINT('Ctrl Pts',(-5.34544983592769,0.914301858020527,
-3.69350124840367));
#91864=CARTESIAN_POINT('Ctrl Pts',(-5.14763184249059,3.59497741079579,-1.24661010706821));
#91865=CARTESIAN_POINT('Ctrl Pts',(-4.94981384905348,3.00461851577406,2.33455925849379));
#91866=CARTESIAN_POINT('Ctrl Pts',(-4.75199585561637,-0.319613108768782,
3.79153621228826));
#91867=CARTESIAN_POINT('Ctrl Pts',(-4.58746675617418,-2.84256693314919,
2.13399857022515));
#91868=CARTESIAN_POINT('Ctrl Pts',(-4.48887698787768,-3.21767031963884,
0.531008518860414));
#91869=CARTESIAN_POINT('Ctrl Pts',(-4.45622655072689,-3.21754606427445,
8.40326422848689E-5));
#91870=CARTESIAN_POINT('Origin',(-31.5777734492731,0.,0.));
#91871=CARTESIAN_POINT('',(-7.20277344927309,-3.21766867394755,-0.000654425321133341));
#91872=CARTESIAN_POINT('',(-6.95622655072689,-3.22556017215824,-0.00235126095564336));
#91873=CARTESIAN_POINT('',(-31.5777734492731,-3.22275,-1.53308031181269E-14));
#91874=CARTESIAN_POINT('Ctrl Pts',(-7.20277344927309,-3.21766867394755,
-0.000654425321134147));
#91875=CARTESIAN_POINT('Ctrl Pts',(-7.17231054453004,-3.21857350729905,
-0.495960687819342));
#91876=CARTESIAN_POINT('Ctrl Pts',(-7.07590830864129,-2.8786031740959,-2.0622188852842));
#91877=CARTESIAN_POINT('Ctrl Pts',(-6.91356674160684,-0.444488776435454,
-3.77893248484412));
#91878=CARTESIAN_POINT('Ctrl Pts',(-6.71574874816972,2.92598744650415,-2.43238534371312));
#91879=CARTESIAN_POINT('Ctrl Pts',(-6.51793075473262,3.63413658105342,1.12736520596504));
#91880=CARTESIAN_POINT('Ctrl Pts',(-6.32011276129551,1.03562072148409,3.66133728555581));
#91881=CARTESIAN_POINT('Ctrl Pts',(-6.131726992809,-2.33636534844852,2.90191784046031));
#91882=CARTESIAN_POINT('Ctrl Pts',(-6.00928055546819,-3.21804476964733,
0.910705166086102));
#91883=CARTESIAN_POINT('Ctrl Pts',(-5.95277344927308,-3.22555111435178,
-0.00235478566260758));
#91884=CARTESIAN_POINT('Ctrl Pts',(-6.95622655072689,-3.22556017215824,
-0.00235126095564378));
#91885=CARTESIAN_POINT('Ctrl Pts',(-6.94681562829278,-3.22680900478704,
-0.154414820411473));
#91886=CARTESIAN_POINT('Ctrl Pts',(-6.87146537471296,-3.14810407601409,
-1.37064060382828));
#91887=CARTESIAN_POINT('Ctrl Pts',(-6.73017578998745,-1.60187655206341,
-3.45136072672716));
#91888=CARTESIAN_POINT('Ctrl Pts',(-6.53235779655034,2.02051125516165,-3.22419503472727));
#91889=CARTESIAN_POINT('Ctrl Pts',(-6.33453980311323,3.80445582041375,-0.0633661140739026));
#91890=CARTESIAN_POINT('Ctrl Pts',(-6.13672180967612,2.12676359733563,3.1551190080601));
#91891=CARTESIAN_POINT('Ctrl Pts',(-5.93890381623902,-1.48604982490852,
3.50279249639495));
#91892=CARTESIAN_POINT('Ctrl Pts',(-5.79540539658927,-3.12595508153286,
1.44301375609325));
#91893=CARTESIAN_POINT('Ctrl Pts',(-5.71784630808522,-3.22622566428263,
0.190564184027195));
#91894=CARTESIAN_POINT('Ctrl Pts',(-5.70622655072688,-3.22455715194561,
0.0026580719403353));
#91895=CARTESIAN_POINT('Origin',(-31.5777734492731,0.,0.));
#91896=CARTESIAN_POINT('',(-8.45277344927309,-3.22319594283231,0.00286971858088855));
#91897=CARTESIAN_POINT('',(-8.20622655072689,-3.21767060863508,-0.000659891891161835));
#91898=CARTESIAN_POINT('',(-31.5777734492731,-3.22275,-1.53308031181269E-14));
#91899=CARTESIAN_POINT('Ctrl Pts',(-8.45277344927309,-3.22319594283231,
0.00286971858088854));
#91900=CARTESIAN_POINT('Ctrl Pts',(-8.40127986473759,-3.21558063935123,
-0.8307531566189));
#91901=CARTESIAN_POINT('Ctrl Pts',(-8.28384694905639,-2.46091776083998,
-2.7440933325883));
#91902=CARTESIAN_POINT('Ctrl Pts',(-8.10047470222948,0.756121223608606,
-3.72909931385589));
#91903=CARTESIAN_POINT('Ctrl Pts',(-7.90265670879237,3.53860570694324,-1.39863170569708));
#91904=CARTESIAN_POINT('Ctrl Pts',(-7.70483871535527,3.10134779529267,2.20443708234665));
#91905=CARTESIAN_POINT('Ctrl Pts',(-7.50702072191815,-0.15779585471615,
3.80171033426082));
#91906=CARTESIAN_POINT('Ctrl Pts',(-7.3396656332241,-2.79358212650196,2.22656213163102));
#91907=CARTESIAN_POINT('Ctrl Pts',(-7.23824987567574,-3.21661492500036,
0.576168314220868));
#91908=CARTESIAN_POINT('Ctrl Pts',(-7.20277344927309,-3.21766867394755,
-0.000654425321134147));
#91909=CARTESIAN_POINT('Ctrl Pts',(-8.20622655072689,-3.21767060863508,
-0.000659891891162043));
#91910=CARTESIAN_POINT('Ctrl Pts',(-8.17578494850033,-3.21858239645565,
-0.495618948061391));
#91911=CARTESIAN_POINT('Ctrl Pts',(-8.07940401512807,-2.87894598482745,
-2.06151932593722));
#91912=CARTESIAN_POINT('Ctrl Pts',(-7.91708375061009,-0.445702651221169,
-3.77878929033658));
#91913=CARTESIAN_POINT('Ctrl Pts',(-7.71926575717298,2.92520576373441,-2.43332500786197));
#91914=CARTESIAN_POINT('Ctrl Pts',(-7.52144776373588,3.63449833574001,1.12619767428708));
#91915=CARTESIAN_POINT('Ctrl Pts',(-7.32362977029877,1.03679675659798,3.66100421190307));
#91916=CARTESIAN_POINT('Ctrl Pts',(-7.13522269929578,-2.33581422869672,
2.90258229478908));
#91917=CARTESIAN_POINT('Ctrl Pts',(-7.01275495943848,-3.21805883296996,
0.911046028124277));
#91918=CARTESIAN_POINT('Ctrl Pts',(-6.95622655072689,-3.22556017215824,
-0.00235126095564378));
#91919=CARTESIAN_POINT('Origin',(-31.5777734492731,0.,0.));
#91920=CARTESIAN_POINT('',(-9.70277344927309,-3.22667916477104,-0.00179405147487009));
#91921=CARTESIAN_POINT('',(-9.45622655072689,-3.2231853869298,0.00287052290945347));
#91922=CARTESIAN_POINT('',(-31.5777734492731,-3.22275,-1.53308031181269E-14));
#91923=CARTESIAN_POINT('Ctrl Pts',(-9.70277344927309,-3.22667916477104,
-0.00179405147487066));
#91924=CARTESIAN_POINT('Ctrl Pts',(-9.69618851609084,-3.22739165962895,
-0.10809806421905));
#91925=CARTESIAN_POINT('Ctrl Pts',(-9.62366425176289,-3.17451256225385,
-1.27817778786519));
#91926=CARTESIAN_POINT('Ctrl Pts',(-9.48520065628923,-1.74745727030714,
-3.37998433218895));
#91927=CARTESIAN_POINT('Ctrl Pts',(-9.28738266285213,1.88131977313113,-3.30734590096318));
#91928=CARTESIAN_POINT('Ctrl Pts',(-9.08956466941502,3.79830252985678,-0.225386088913072));
#91929=CARTESIAN_POINT('Ctrl Pts',(-8.8917466759779,2.25924731649643,3.06165030013156));
#91930=CARTESIAN_POINT('Ctrl Pts',(-8.69392868254081,-1.33547472388757,
3.56292130971895));
#91931=CARTESIAN_POINT('Ctrl Pts',(-8.54760427363919,-3.09563628545797,
1.53572413753069));
#91932=CARTESIAN_POINT('Ctrl Pts',(-8.46721919588329,-3.22533230108819,
0.236730012678338));
#91933=CARTESIAN_POINT('Ctrl Pts',(-8.45277344927309,-3.22319594283231,
0.00286971858088854));
#91934=CARTESIAN_POINT('Ctrl Pts',(-9.45622655072689,-3.2231853869298,0.00287052290945312));
#91935=CARTESIAN_POINT('Ctrl Pts',(-9.40475426870788,-3.21557354337093,
-0.830414323179482));
#91936=CARTESIAN_POINT('Ctrl Pts',(-9.28734265554316,-2.46142530178796,
-2.74341705299499));
#91937=CARTESIAN_POINT('Ctrl Pts',(-9.10399171123273,0.754923226864277,
-3.72934180192827));
#91938=CARTESIAN_POINT('Ctrl Pts',(-8.90617371779564,3.53815603498388,-1.3997682758857));
#91939=CARTESIAN_POINT('Ctrl Pts',(-8.70835572435851,3.10205560019449,2.20344058403463));
#91940=CARTESIAN_POINT('Ctrl Pts',(-8.51053773092143,-0.156574597645193,
3.80176061180093));
#91941=CARTESIAN_POINT('Ctrl Pts',(-8.34316133971087,-2.79320214739646,
2.22725889318856));
#91942=CARTESIAN_POINT('Ctrl Pts',(-8.24172427964603,-3.21660737954993,
0.576508230576168));
#91943=CARTESIAN_POINT('Ctrl Pts',(-8.20622655072689,-3.21767060863508,
-0.000659891891162043));
#91944=CARTESIAN_POINT('Origin',(-31.5777734492731,0.,0.));
#91945=CARTESIAN_POINT('',(-10.9527734492731,-3.2181054871608,-0.00135616439500266));
#91946=CARTESIAN_POINT('',(-10.7062265507269,-3.22668646461764,-0.00178921965619527));
#91947=CARTESIAN_POINT('',(-31.5777734492731,-3.22275,-1.53308031181269E-14));
#91948=CARTESIAN_POINT('Ctrl Pts',(-10.9527734492731,-3.2181054871608,-0.00135616439500295));
#91949=CARTESIAN_POINT('Ctrl Pts',(-10.9251578362984,-3.21981873729031,
-0.450214994152712));
#91950=CARTESIAN_POINT('Ctrl Pts',(-10.831602892178,-2.92310678984398,-1.96867411684349));
#91951=CARTESIAN_POINT('Ctrl Pts',(-10.6721086169119,-0.606282086762444,
-3.75637099188338));
#91952=CARTESIAN_POINT('Ctrl Pts',(-10.4742906234748,2.81888564080964,-2.55573565562428));
#91953=CARTESIAN_POINT('Ctrl Pts',(-10.2764726300377,3.67917715554996,0.970338320108655));
#91954=CARTESIAN_POINT('Ctrl Pts',(-10.0786546366006,1.19182170212393,3.61351103882891));
#91955=CARTESIAN_POINT('Ctrl Pts',(-9.88742157634569,-2.2610636442974,2.99024725147983));
#91956=CARTESIAN_POINT('Ctrl Pts',(-9.76212784723654,-3.22025697305356,
0.956394969264087));
#91957=CARTESIAN_POINT('Ctrl Pts',(-9.70277344927309,-3.22667916477104,
-0.00179405147487066));
#91958=CARTESIAN_POINT('Ctrl Pts',(-10.7062265507269,-3.22668646461764,
-0.00178921965619555));
#91959=CARTESIAN_POINT('Ctrl Pts',(-10.6996629200611,-3.22739513133839,
-0.10774868125948));
#91960=CARTESIAN_POINT('Ctrl Pts',(-10.6271599582497,-3.1747033654712,-1.27748131867));
#91961=CARTESIAN_POINT('Ctrl Pts',(-10.4887176652925,-1.74854284806569,
-3.37942262266014));
#91962=CARTESIAN_POINT('Ctrl Pts',(-10.2908996718554,1.88025713615946,-3.30794988716429));
#91963=CARTESIAN_POINT('Ctrl Pts',(-10.0930816784183,3.79822971656082,-0.226606209763087));
#91964=CARTESIAN_POINT('Ctrl Pts',(-9.89526368498117,2.26023057897525,3.06092422054745));
#91965=CARTESIAN_POINT('Ctrl Pts',(-9.69744569154406,-1.33433004645538,
3.56334992404553));
#91966=CARTESIAN_POINT('Ctrl Pts',(-9.55109998012597,-3.09539896911836,
1.53642335041516));
#91967=CARTESIAN_POINT('Ctrl Pts',(-9.47069359985358,-3.22532480858339,
0.237077601593841));
#91968=CARTESIAN_POINT('Ctrl Pts',(-9.45622655072689,-3.2231853869298,0.00287052290945312));
#91969=CARTESIAN_POINT('Origin',(-31.5777734492731,0.,0.));
#91970=CARTESIAN_POINT('',(-12.2027734492731,-3.22182548726639,0.00287273816568898));
#91971=CARTESIAN_POINT('',(-11.9562265507269,-3.21810971317159,-0.00136113665029886));
#91972=CARTESIAN_POINT('',(-31.5777734492731,-3.22275,-1.53308031181269E-14));
#91973=CARTESIAN_POINT('Ctrl Pts',(-12.2027734492731,-3.22182548726639,
0.00287273816568887));
#91974=CARTESIAN_POINT('Ctrl Pts',(-12.1541271565059,-3.21489726619265,
-0.78551235421924));
#91975=CARTESIAN_POINT('Ctrl Pts',(-12.0395415325931,-2.52718466035753,
-2.65335903695121));
#91976=CARTESIAN_POINT('Ctrl Pts',(-11.8590165775345,0.595360400383641,
-3.75811747967609));
#91977=CARTESIAN_POINT('Ctrl Pts',(-11.6611985840974,3.47531106646949,-1.54923012773011));
#91978=CARTESIAN_POINT('Ctrl Pts',(-11.4633805906603,3.19311050600954,2.06928642140315));
#91979=CARTESIAN_POINT('Ctrl Pts',(-11.2655625972232,0.00553022271176743,
3.80497968641473));
#91980=CARTESIAN_POINT('Ctrl Pts',(-11.0953602167608,-2.74138972731681,
2.31956968971646));
#91981=CARTESIAN_POINT('Ctrl Pts',(-10.9910971674441,-3.21572791490918,
0.621550135239206));
#91982=CARTESIAN_POINT('Ctrl Pts',(-10.9527734492731,-3.2181054871608,-0.00135616439500295));
#91983=CARTESIAN_POINT('Ctrl Pts',(-11.9562265507269,-3.21810971317159,
-0.00136113665029847));
#91984=CARTESIAN_POINT('Ctrl Pts',(-11.9286322402687,-3.2198280570441,-0.449872156052723));
#91985=CARTESIAN_POINT('Ctrl Pts',(-11.8350985986648,-2.92342951382292,
-1.96797377055099));
#91986=CARTESIAN_POINT('Ctrl Pts',(-11.6756256259151,-0.607488696492234,
-3.75617582624975));
#91987=CARTESIAN_POINT('Ctrl Pts',(-11.477807632478,2.81806434528784,-2.55664090162977));
#91988=CARTESIAN_POINT('Ctrl Pts',(-11.2799896390409,3.67948846292253,0.969156336866661));
#91989=CARTESIAN_POINT('Ctrl Pts',(-11.0821716456038,1.1929823568862,3.61312779323221));
#91990=CARTESIAN_POINT('Ctrl Pts',(-10.8909172828325,-2.26048748756761,
2.99090395355496));
#91991=CARTESIAN_POINT('Ctrl Pts',(-10.7656022512068,-3.22027574696849,
0.956737787048822));
#91992=CARTESIAN_POINT('Ctrl Pts',(-10.7062265507269,-3.22668646461764,
-0.00178921965619555));
#91993=CARTESIAN_POINT('Origin',(-31.5777734492731,0.,0.));
#91994=CARTESIAN_POINT('',(-13.4527734492731,-3.22751445325846,-0.00107914716668534));
#91995=CARTESIAN_POINT('',(-13.2062265507269,-3.22181528236761,0.00287197708553733));
#91996=CARTESIAN_POINT('',(-31.5777734492731,-3.22275,-1.53308031181269E-14));
#91997=CARTESIAN_POINT('Ctrl Pts',(-13.4527734492731,-3.22751445325846,
-0.0010791471666857));
#91998=CARTESIAN_POINT('Ctrl Pts',(-13.4490358078592,-3.22777825363035,
-0.061376493187223));
#91999=CARTESIAN_POINT('Ctrl Pts',(-13.3793588352996,-3.19898704244113,
-1.18518051592563));
#92000=CARTESIAN_POINT('Ctrl Pts',(-13.2437425315943,-1.8909257110314,-3.30186325470216));
#92001=CARTESIAN_POINT('Ctrl Pts',(-13.0459245381572,1.7376248539901,-3.38504961029937));
#92002=CARTESIAN_POINT('Ctrl Pts',(-12.8481065447201,3.78512772048049,-0.388212747140301));
#92003=CARTESIAN_POINT('Ctrl Pts',(-12.6502885512829,2.38858024585731,2.96185506169566));
#92004=CARTESIAN_POINT('Ctrl Pts',(-12.4524705578458,-1.18131281127045,
3.61696019321754));
#92005=CARTESIAN_POINT('Ctrl Pts',(-12.3032988571759,-3.06277764869808,
1.62924239957152));
#92006=CARTESIAN_POINT('Ctrl Pts',(-12.2200664876516,-3.22428836750058,
0.283131990909709));
#92007=CARTESIAN_POINT('Ctrl Pts',(-12.2027734492731,-3.22182548726639,
0.00287273816568887));
#92008=CARTESIAN_POINT('Ctrl Pts',(-13.2062265507269,-3.22181528236761,
0.00287197708553705));
#92009=CARTESIAN_POINT('Ctrl Pts',(-13.1576015604762,-3.21489372565932,
-0.785174075009538));
#92010=CARTESIAN_POINT('Ctrl Pts',(-13.0430372390799,-2.52766830833463,
-2.65267741427113));
#92011=CARTESIAN_POINT('Ctrl Pts',(-12.8625335865378,0.594153099425664,
-3.75830832270474));
#92012=CARTESIAN_POINT('Ctrl Pts',(-12.6647155931007,3.47481302398082,-1.55034634918851));
#92013=CARTESIAN_POINT('Ctrl Pts',(-12.4668975996636,3.19377488593328,2.0682604603992));
#92014=CARTESIAN_POINT('Ctrl Pts',(-12.2690796062265,0.00675251231494511,
3.80497749765308));
#92015=CARTESIAN_POINT('Ctrl Pts',(-12.0988559232476,-2.74098816878215,
2.32026426362444));
#92016=CARTESIAN_POINT('Ctrl Pts',(-11.9945715714144,-3.21572190458911,
0.621889237501745));
#92017=CARTESIAN_POINT('Ctrl Pts',(-11.9562265507269,-3.21810971317159,
-0.00136113665029847));
#92018=CARTESIAN_POINT('Origin',(-31.5777734492731,0.,0.));
#92019=CARTESIAN_POINT('',(-14.7027734492731,-3.21883508950441,-0.00196949714717019));
#92020=CARTESIAN_POINT('',(-14.4562265507269,-3.2275191157403,-0.00107334156349448));
#92021=CARTESIAN_POINT('',(-31.5777734492731,-3.22275,-1.53308031181269E-14));
#92022=CARTESIAN_POINT('Ctrl Pts',(-14.7027734492731,-3.21883508950441,
-0.00196949714717044));
#92023=CARTESIAN_POINT('Ctrl Pts',(-14.6780051280667,-3.22109751442067,
-0.404320281781302));
#92024=CARTESIAN_POINT('Ctrl Pts',(-14.5872974757147,-2.96496213196803,
-1.87505121301113));
#92025=CARTESIAN_POINT('Ctrl Pts',(-14.4306504922169,-0.766957879978414,
-3.7268856445739));
#92026=CARTESIAN_POINT('Ctrl Pts',(-14.2328324987798,2.70658798155444,-2.6743751598265));
#92027=CARTESIAN_POINT('Ctrl Pts',(-14.0350145053427,3.71743616166189,0.811522877903334));
#92028=CARTESIAN_POINT('Ctrl Pts',(-13.8371965119056,1.34582588168488,3.55902426144851));
#92029=CARTESIAN_POINT('Ctrl Pts',(-13.6431161598824,-2.18239091772659,
3.07747832470855));
#92030=CARTESIAN_POINT('Ctrl Pts',(-13.5149751390049,-3.2231242972573,1.00238704808438));
#92031=CARTESIAN_POINT('Ctrl Pts',(-13.4527734492731,-3.22751445325846,
-0.0010791471666857));
#92032=CARTESIAN_POINT('Ctrl Pts',(-14.4562265507269,-3.2275191157403,-0.00107334156349525));
#92033=CARTESIAN_POINT('Ctrl Pts',(-14.4525102118295,-3.22778017593927,
-0.0610267823477145));
#92034=CARTESIAN_POINT('Ctrl Pts',(-14.3828545417863,-3.19916205398302,
-1.18448531601658));
#92035=CARTESIAN_POINT('Ctrl Pts',(-14.2472595405976,-1.89198617807126,
-3.3012554666454));
#92036=CARTESIAN_POINT('Ctrl Pts',(-14.0494415471604,1.73653727148651,-3.38560742833646));
#92037=CARTESIAN_POINT('Ctrl Pts',(-13.8516235537233,3.78500260309515,-0.389428618146851));
#92038=CARTESIAN_POINT('Ctrl Pts',(-13.6538055602862,2.38953143666386,2.96108744674385));
#92039=CARTESIAN_POINT('Ctrl Pts',(-13.4559875668491,-1.18015079139549,
3.61733927958623));
#92040=CARTESIAN_POINT('Ctrl Pts',(-13.3067945636627,-3.06252272261062,
1.62994232206525));
#92041=CARTESIAN_POINT('Ctrl Pts',(-13.2235408916219,-3.22427990378457,
0.283478675752636));
#92042=CARTESIAN_POINT('Ctrl Pts',(-13.2062265507269,-3.22181528236761,
0.00287197708553705));
#92043=CARTESIAN_POINT('Origin',(-31.5777734492731,0.,0.));
#92044=CARTESIAN_POINT('',(-15.9527734492731,-3.22054328874694,0.00267261023343764));
#92045=CARTESIAN_POINT('',(-15.7062265507269,-3.21884138421527,-0.0019736436849066));
#92046=CARTESIAN_POINT('',(-31.5777734492731,-3.22275,-1.53308031181269E-14));
#92047=CARTESIAN_POINT('Ctrl Pts',(-15.9527734492731,-3.22054328874694,
0.00267261023343748));
#92048=CARTESIAN_POINT('Ctrl Pts',(-15.9069744482743,-3.21466005692855,
-0.740318326976134));
#92049=CARTESIAN_POINT('Ctrl Pts',(-15.7952361161298,-2.59028920630862,
-2.56196187539477));
#92050=CARTESIAN_POINT('Ctrl Pts',(-15.6175584528396,0.433502191222674,
-3.78020857197022));
#92051=CARTESIAN_POINT('Ctrl Pts',(-15.4197404594025,3.40561062963269,-1.69697296287383));
#92052=CARTESIAN_POINT('Ctrl Pts',(-15.2219224659654,3.27898758080047,1.93032159039582));
#92053=CARTESIAN_POINT('Ctrl Pts',(-15.0241044725282,0.168846106669414,
3.80123558723405));
#92054=CARTESIAN_POINT('Ctrl Pts',(-14.8510548002975,-2.68627752097958,
2.41224661168182));
#92055=CARTESIAN_POINT('Ctrl Pts',(-14.7439444592124,-3.21507438574341,
0.666835950556258));
#92056=CARTESIAN_POINT('Ctrl Pts',(-14.7027734492731,-3.21883508950441,
-0.00196949714717044));
#92057=CARTESIAN_POINT('Ctrl Pts',(-15.7062265507269,-3.21884138421527,
-0.00197364368490657));
#92058=CARTESIAN_POINT('Ctrl Pts',(-15.681479532037,-3.22110690703042,-0.403976324022853));
#92059=CARTESIAN_POINT('Ctrl Pts',(-15.5907931822014,-2.96526531461261,
-1.87435049020682));
#92060=CARTESIAN_POINT('Ctrl Pts',(-15.4341675012202,-0.768155000592636,
-3.72663886754987));
#92061=CARTESIAN_POINT('Ctrl Pts',(-15.236349507783,2.70572858711511,-2.67524431911123));
#92062=CARTESIAN_POINT('Ctrl Pts',(-15.038531514346,3.71769644791273,0.81032862176155));
#92063=CARTESIAN_POINT('Ctrl Pts',(-14.8407135209088,1.34696901673613,3.5585915503218));
#92064=CARTESIAN_POINT('Ctrl Pts',(-14.6466118663692,-2.18178936818306,
3.07812631949869));
#92065=CARTESIAN_POINT('Ctrl Pts',(-14.5184495429752,-3.22314816164128,
1.00273244260953));
#92066=CARTESIAN_POINT('Ctrl Pts',(-14.4562265507269,-3.2275191157403,-0.00107334156349525));
#92067=CARTESIAN_POINT('Origin',(-31.5777734492731,0.,0.));
#92068=CARTESIAN_POINT('',(-17.2027734492731,-3.22793661423918,-0.000264189382539215));
#92069=CARTESIAN_POINT('',(-16.9562265507269,-3.22053404262666,0.00267039071692468));
#92070=CARTESIAN_POINT('',(-31.5777734492731,-3.22275,-1.53308031181269E-14));
#92071=CARTESIAN_POINT('Ctrl Pts',(-17.2027734492731,-3.22793661423918,
-0.00026418938253939));
#92072=CARTESIAN_POINT('Ctrl Pts',(-17.2018830996275,-3.22795359918395,
-0.0146226889311297));
#92073=CARTESIAN_POINT('Ctrl Pts',(-17.1350534188363,-3.22138006304283,
-1.09235627156946));
#92074=CARTESIAN_POINT('Ctrl Pts',(-17.0022844068993,-2.03090874143955,
-3.21765608499983));
#92075=CARTESIAN_POINT('Ctrl Pts',(-16.8044664134622,1.59072709321647,-3.45651389586373));
#92076=CARTESIAN_POINT('Ctrl Pts',(-16.6066484200251,3.7649760515017,-0.55032384012566));
#92077=CARTESIAN_POINT('Ctrl Pts',(-16.408830426588,2.51351047331346,2.85660044422309));
#92078=CARTESIAN_POINT('Ctrl Pts',(-16.2110124331509,-1.02497346786645,
3.66433218848425));
#92079=CARTESIAN_POINT('Ctrl Pts',(-16.0589934407126,-3.02753062537622,
1.72284050673799));
#92080=CARTESIAN_POINT('Ctrl Pts',(-15.97291377942,-3.22313046813009,0.329406435103203));
#92081=CARTESIAN_POINT('Ctrl Pts',(-15.9527734492731,-3.22054328874694,
0.00267261023343748));
#92082=CARTESIAN_POINT('Ctrl Pts',(-16.9562265507269,-3.22053404262666,
0.00267039071692496));
#92083=CARTESIAN_POINT('Ctrl Pts',(-16.9104488522446,-3.21465963284635,
-0.739980205315209));
#92084=CARTESIAN_POINT('Ctrl Pts',(-16.7987318226165,-2.5907494278201,-2.5612756850456));
#92085=CARTESIAN_POINT('Ctrl Pts',(-16.6210754618428,0.432287811384032,
-3.7803474181876));
#92086=CARTESIAN_POINT('Ctrl Pts',(-16.4232574684057,3.40506513462136,-1.69806677814945));
#92087=CARTESIAN_POINT('Ctrl Pts',(-16.2254394749686,3.27960731114141,1.92926805778166));
#92088=CARTESIAN_POINT('Ctrl Pts',(-16.0276214815315,0.170067175844205,
3.80118093620512));
#92089=CARTESIAN_POINT('Ctrl Pts',(-15.8545505067843,-2.68585385572339,
2.41293840251175));
#92090=CARTESIAN_POINT('Ctrl Pts',(-15.7474188631827,-3.21507033911092,
0.667174435285191));
#92091=CARTESIAN_POINT('Ctrl Pts',(-15.7062265507269,-3.21884138421527,
-0.00197364368490657));
#92092=CARTESIAN_POINT('Origin',(-31.5777734492731,0.,0.));
#92093=CARTESIAN_POINT('',(-18.4527734492731,-3.21982010873651,-0.00245263893930523));
#92094=CARTESIAN_POINT('',(-18.2062265507269,-3.22793772000202,-0.000257889290232183));
#92095=CARTESIAN_POINT('',(-31.5777734492731,-3.22275,-1.53308031181269E-14));
#92096=CARTESIAN_POINT('Ctrl Pts',(-18.4527734492731,-3.21982010873651,
-0.00245263893930543));
#92097=CARTESIAN_POINT('Ctrl Pts',(-18.4308524198351,-3.22236380461367,
-0.35827632108061));
#92098=CARTESIAN_POINT('Ctrl Pts',(-18.3429920592514,-3.00424192805471,
-1.78140187471239));
#92099=CARTESIAN_POINT('Ctrl Pts',(-18.189192367522,-0.926219993698007,
-3.69053079118249));
#92100=CARTESIAN_POINT('Ctrl Pts',(-17.9913743740849,2.5893014591106,-2.78808517646783));
#92101=CARTESIAN_POINT('Ctrl Pts',(-17.7935563806477,3.74884307925887,0.651211612676593));
#92102=CARTESIAN_POINT('Ctrl Pts',(-17.5957383872107,1.49734939509152,3.49797738506285));
#92103=CARTESIAN_POINT('Ctrl Pts',(-17.3988107434191,-2.10030201134441,
3.1634803998261));
#92104=CARTESIAN_POINT('Ctrl Pts',(-17.2678224307732,-3.22669569348036,
1.04876837458784));
#92105=CARTESIAN_POINT('Ctrl Pts',(-17.2027734492731,-3.22793661423918,
-0.00026418938253939));
#92106=CARTESIAN_POINT('Ctrl Pts',(-18.2062265507269,-3.22793772000202,
-0.000257889290232734));
#92107=CARTESIAN_POINT('Ctrl Pts',(-18.2053575035978,-3.22795391650523,
-0.0142728313140034));
#92108=CARTESIAN_POINT('Ctrl Pts',(-18.138549125323,-3.22153971724754,-1.09166239659244));
#92109=CARTESIAN_POINT('Ctrl Pts',(-18.0058014159026,-2.03194214307649,
-3.21700333870802));
#92110=CARTESIAN_POINT('Ctrl Pts',(-17.8079834224654,1.5896165698452,-3.45702451755008));
#92111=CARTESIAN_POINT('Ctrl Pts',(-17.6101654290284,3.76479886064709,-0.551533220159296));
#92112=CARTESIAN_POINT('Ctrl Pts',(-17.4123474355912,2.51442783918464,2.85579270879419));
#92113=CARTESIAN_POINT('Ctrl Pts',(-17.2145294421542,-1.0237962474182,3.66466104815183));
#92114=CARTESIAN_POINT('Ctrl Pts',(-17.0624891471994,-3.02725756873777,
1.72354089465449));
#92115=CARTESIAN_POINT('Ctrl Pts',(-16.9763881833903,-3.22312127824644,
0.329752114150966));
#92116=CARTESIAN_POINT('Ctrl Pts',(-16.9562265507269,-3.22053404262666,
0.00267039071692496));
#92117=CARTESIAN_POINT('Origin',(-31.5777734492731,0.,0.));
#92118=CARTESIAN_POINT('',(-19.7027734492731,-3.21942420511343,0.00228930942898773));
#92119=CARTESIAN_POINT('',(-19.4562265507269,-3.21982813535995,-0.0024556690389646));
#92120=CARTESIAN_POINT('',(-31.5777734492731,-3.22275,-1.53308031181269E-14));
#92121=CARTESIAN_POINT('Ctrl Pts',(-19.7027734492731,-3.21942420511343,
0.00228930942898737));
#92122=CARTESIAN_POINT('Ctrl Pts',(-19.6598217400426,-3.21481005975396,
-0.695121887590858));
#92123=CARTESIAN_POINT('Ctrl Pts',(-19.5509306996665,-2.6502951772353,-2.47000221202959));
#92124=CARTESIAN_POINT('Ctrl Pts',(-19.3761003281446,0.270844937974172,
-3.7953318717822));
#92125=CARTESIAN_POINT('Ctrl Pts',(-19.1782823347075,3.32963287034385,-1.84158788715549));
#92126=CARTESIAN_POINT('Ctrl Pts',(-18.9804643412704,3.35882072849595,1.78779873341992));
#92127=CARTESIAN_POINT('Ctrl Pts',(-18.7826463478333,0.331850768478793,
3.79048493795346));
#92128=CARTESIAN_POINT('Ctrl Pts',(-18.6067493838342,-2.62817580074329,
2.50451000044191));
#92129=CARTESIAN_POINT('Ctrl Pts',(-18.4967917509808,-3.21471226592786,
0.71205551130674));
#92130=CARTESIAN_POINT('Ctrl Pts',(-18.4527734492731,-3.21982010873651,
-0.00245263893930543));
#92131=CARTESIAN_POINT('Ctrl Pts',(-19.4562265507269,-3.21982813535995,
-0.00245566903896481));
#92132=CARTESIAN_POINT('Ctrl Pts',(-19.4343268238054,-3.22237293973325,
-0.357931261263622));
#92133=CARTESIAN_POINT('Ctrl Pts',(-19.3464877657381,-3.00452611195908,
-1.78070113839176));
#92134=CARTESIAN_POINT('Ctrl Pts',(-19.1927093765252,-0.927405418628458,
-3.69023285763479));
#92135=CARTESIAN_POINT('Ctrl Pts',(-18.9948913830881,2.58840554981504,-2.78891664697164));
#92136=CARTESIAN_POINT('Ctrl Pts',(-18.797073389651,3.74905186462063,0.650007284923323));
#92137=CARTESIAN_POINT('Ctrl Pts',(-18.5992553962139,1.49847290337135,3.4974960059921));
#92138=CARTESIAN_POINT('Ctrl Pts',(-18.4023064499059,-2.09967475031009,
3.16411868726491));
#92139=CARTESIAN_POINT('Ctrl Pts',(-18.2712968347435,-3.22672499973764,
1.04911702658821));
#92140=CARTESIAN_POINT('Ctrl Pts',(-18.2062265507269,-3.22793772000202,
-0.000257889290232734));
#92141=CARTESIAN_POINT('Origin',(-31.5777734492731,0.,0.));
#92142=CARTESIAN_POINT('',(-20.9527734492731,-3.22783470827694,0.000576931514566297));
#92143=CARTESIAN_POINT('',(-20.7062265507269,-3.21941642796096,0.00228582146781398));
#92144=CARTESIAN_POINT('',(-31.5777734492731,-3.22275,-1.53308031181269E-14));
#92145=CARTESIAN_POINT('Ctrl Pts',(-20.9527734492731,-3.22783470827694,
0.000576931514566295));
#92146=CARTESIAN_POINT('Ctrl Pts',(-20.8887910602502,-3.22527243766867,
-1.03134253166322));
#92147=CARTESIAN_POINT('Ctrl Pts',(-20.7588693400816,-2.1314552457683,-3.13141661665854));
#92148=CARTESIAN_POINT('Ctrl Pts',(-20.5630082887673,1.44089725711671,-3.52160703256702));
#92149=CARTESIAN_POINT('Ctrl Pts',(-20.3651902953302,3.73788466707397,-0.711420559897795));
#92150=CARTESIAN_POINT('Ctrl Pts',(-20.1673723018931,2.63380772376682,2.7460804561444));
#92151=CARTESIAN_POINT('Ctrl Pts',(-19.9695543084559,-0.866744862987072,
3.70494997805335));
#92152=CARTESIAN_POINT('Ctrl Pts',(-19.8146880242493,-2.98982485439288,
1.81648289572435));
#92153=CARTESIAN_POINT('Ctrl Pts',(-19.7257610711883,-3.22189368143663,
0.375541624733414));
#92154=CARTESIAN_POINT('Ctrl Pts',(-19.7027734492731,-3.21942420511343,
0.00228930942898737));
#92155=CARTESIAN_POINT('Ctrl Pts',(-20.7062265507269,-3.21941642796096,
0.00228582146781373));
#92156=CARTESIAN_POINT('Ctrl Pts',(-20.6632961440129,-3.21481230975648,
-0.69478358435536));
#92157=CARTESIAN_POINT('Ctrl Pts',(-20.5544264061532,-2.65073246007064,
-2.46931218000302));
#92158=CARTESIAN_POINT('Ctrl Pts',(-20.3796173371479,0.269625717635743,
-3.79541846526285));
#92159=CARTESIAN_POINT('Ctrl Pts',(-20.1817993437108,3.3290409282824,-1.84265728009565));
#92160=CARTESIAN_POINT('Ctrl Pts',(-19.9839813502737,3.35939466694879,1.78671957109805));
#92161=CARTESIAN_POINT('Ctrl Pts',(-19.7861633568365,0.333068366514352,
3.79037792539165));
#92162=CARTESIAN_POINT('Ctrl Pts',(-19.610245090321,-2.62772951399423,2.50519836286118));
#92163=CARTESIAN_POINT('Ctrl Pts',(-19.5002661549511,-3.21471062052383,
0.712393627896549));
#92164=CARTESIAN_POINT('Ctrl Pts',(-19.4562265507269,-3.21982813535995,
-0.00245566903896481));
#92165=CARTESIAN_POINT('Origin',(-31.5777734492731,0.,0.));
#92166=CARTESIAN_POINT('',(-22.2027734492731,-3.22100822472723,-0.00277034754127511));
#92167=CARTESIAN_POINT('',(-21.9562265507269,-3.22783176676599,0.000583108904914156));
#92168=CARTESIAN_POINT('',(-31.5777734492731,-3.22275,-1.53308031181269E-14));
#92169=CARTESIAN_POINT('Ctrl Pts',(-22.2027734492731,-3.22100822472723,
-0.00277034754127548));
#92170=CARTESIAN_POINT('Ctrl Pts',(-22.1836997116034,-3.22357544039283,
-0.312087844936352));
#92171=CARTESIAN_POINT('Ctrl Pts',(-22.0986866427881,-3.04101832689042,
-1.68777152984388));
#92172=CARTESIAN_POINT('Ctrl Pts',(-21.947734242827,-1.08377487127288,-3.64737344205279));
#92173=CARTESIAN_POINT('Ctrl Pts',(-21.7499162493899,2.46724225947258,-2.89665611187517));
#92174=CARTESIAN_POINT('Ctrl Pts',(-21.5520982559528,3.7733400181795,0.489700014903892));
#92175=CARTESIAN_POINT('Ctrl Pts',(-21.3542802625157,1.64611294971294,3.43048293308387));
#92176=CARTESIAN_POINT('Ctrl Pts',(-21.1564622690786,-1.97889603910867,
3.24990330068325));
#92177=CARTESIAN_POINT('Ctrl Pts',(-21.0226266646644,-3.21323182514106,
1.12710744043192));
#92178=CARTESIAN_POINT('Ctrl Pts',(-20.9547303913959,-3.22791307695557,
0.0321388455921796));
#92179=CARTESIAN_POINT('Ctrl Pts',(-20.9527734492731,-3.22783470827694,
0.000576931514566295));
#92180=CARTESIAN_POINT('Ctrl Pts',(-21.9562265507269,-3.22783176676599,
0.000583108904914152));
#92181=CARTESIAN_POINT('Ctrl Pts',(-21.8922654642205,-3.22524488400269,
-1.03099509137694));
#92182=CARTESIAN_POINT('Ctrl Pts',(-21.7623650465684,-2.13207240585389,
-3.13077414396875));
#92183=CARTESIAN_POINT('Ctrl Pts',(-21.5665252977705,1.43976583982743,-3.52206951670956));
#92184=CARTESIAN_POINT('Ctrl Pts',(-21.3687073043334,3.7376557293535,-0.712621219793359));
#92185=CARTESIAN_POINT('Ctrl Pts',(-21.1708893108963,2.63468957378667,2.74523408908033));
#92186=CARTESIAN_POINT('Ctrl Pts',(-20.9730713174592,-0.865554611853212,
3.70522800485591));
#92187=CARTESIAN_POINT('Ctrl Pts',(-20.8181837307361,-2.98953313583763,
1.81718346053193));
#92188=CARTESIAN_POINT('Ctrl Pts',(-20.7292354751586,-3.22188404511044,
0.375886225235549));
#92189=CARTESIAN_POINT('Ctrl Pts',(-20.7062265507269,-3.21941642796096,
0.00228582146781373));
#92190=CARTESIAN_POINT('Origin',(-31.5777734492731,0.,0.));
#92191=CARTESIAN_POINT('',(-23.4527734492731,-3.21852952379537,0.00175287054439046));
#92192=CARTESIAN_POINT('',(-23.2062265507269,-3.2210175372949,-0.0027720277556742));
#92193=CARTESIAN_POINT('',(-31.5777734492731,-3.22275,-1.53308031181269E-14));
#92194=CARTESIAN_POINT('Ctrl Pts',(-23.4527734492731,-3.21852952379537,
0.00175287054439036));
#92195=CARTESIAN_POINT('Ctrl Pts',(-23.412669031811,-3.21528819727374,-0.649881444060061));
#92196=CARTESIAN_POINT('Ctrl Pts',(-23.3066252832032,-2.70726897394943,
-2.37757378032704));
#92197=CARTESIAN_POINT('Ctrl Pts',(-23.1346422034496,0.107688455305257,
-3.80345950341412));
#92198=CARTESIAN_POINT('Ctrl Pts',(-22.9368242100126,3.24751783306243,-1.98280834205173));
#92199=CARTESIAN_POINT('Ctrl Pts',(-22.7390062165755,3.43246279827112,1.64198055282517));
#92200=CARTESIAN_POINT('Ctrl Pts',(-22.5411882231383,0.494243753116372,
3.77274755449071));
#92201=CARTESIAN_POINT('Ctrl Pts',(-22.3624439673709,-2.56701675396682,
2.59627028778708));
#92202=CARTESIAN_POINT('Ctrl Pts',(-22.2496390427492,-3.21470038471007,
0.7572457719529));
#92203=CARTESIAN_POINT('Ctrl Pts',(-22.2027734492731,-3.22100822472723,
-0.00277034754127548));
#92204=CARTESIAN_POINT('Ctrl Pts',(-23.2062265507269,-3.2210175372949,-0.00277202775567441));
#92205=CARTESIAN_POINT('Ctrl Pts',(-23.1871741155737,-3.22358401811418,
-0.311741735937044));
#92206=CARTESIAN_POINT('Ctrl Pts',(-23.1021823492748,-3.04128404879359,
-1.68707109660414));
#92207=CARTESIAN_POINT('Ctrl Pts',(-22.9512512518303,-1.08494641550995,
-3.6470249011433));
#92208=CARTESIAN_POINT('Ctrl Pts',(-22.7534332583931,2.46631148668775,-2.89744836100596));
#92209=CARTESIAN_POINT('Ctrl Pts',(-22.555615264956,3.77349691781262,0.488487835391227));
#92210=CARTESIAN_POINT('Ctrl Pts',(-22.357797271519,1.64721476033769,3.42995377336155));
#92211=CARTESIAN_POINT('Ctrl Pts',(-22.1599792780818,-1.97785184410161,
3.25053863795708));
#92212=CARTESIAN_POINT('Ctrl Pts',(-22.0261223711511,-3.21306598821237,
1.12780169803537));
#92213=CARTESIAN_POINT('Ctrl Pts',(-21.9582047953662,-3.2279117761473,0.0324886651761775));
#92214=CARTESIAN_POINT('Ctrl Pts',(-21.9562265507269,-3.22783176676599,
0.000583108904914152));
#92215=CARTESIAN_POINT('Origin',(-31.5777734492731,0.,0.));
#92216=CARTESIAN_POINT('',(-24.7027734492731,-3.22724337194307,0.00136199953838144));
#92217=CARTESIAN_POINT('',(-24.4562265507269,-3.21852362056934,0.00174837132580694));
#92218=CARTESIAN_POINT('',(-31.5777734492731,-3.22275,-1.53308031181269E-14));
#92219=CARTESIAN_POINT('Ctrl Pts',(-24.7027734492731,-3.22724337194307,
0.00136199953838148));
#92220=CARTESIAN_POINT('Ctrl Pts',(-24.6416383520185,-3.22197027182432,
-0.985117712154));
#92221=CARTESIAN_POINT('Ctrl Pts',(-24.5145639236183,-2.2122594842165,-3.04493847307747));
#92222=CARTESIAN_POINT('Ctrl Pts',(-24.3215501640723,1.28841151633002,-3.5802090396263));
#92223=CARTESIAN_POINT('Ctrl Pts',(-24.1237321706352,3.70390350292133,-0.871205967781821));
#92224=CARTESIAN_POINT('Ctrl Pts',(-23.925914177198,2.74925026171735,2.63049881095482));
#92225=CARTESIAN_POINT('Ctrl Pts',(-23.728096183761,-0.706918648264489,
3.73873869412743));
#92226=CARTESIAN_POINT('Ctrl Pts',(-23.570382607786,-2.94958875270477,1.91012798661397));
#92227=CARTESIAN_POINT('Ctrl Pts',(-23.4786083629567,-3.22061755788753,
0.421529975821576));
#92228=CARTESIAN_POINT('Ctrl Pts',(-23.4527734492731,-3.21852952379537,
0.00175287054439036));
#92229=CARTESIAN_POINT('Ctrl Pts',(-24.4562265507269,-3.21852362056934,
0.00174837132580694));
#92230=CARTESIAN_POINT('Ctrl Pts',(-24.4161434357813,-3.21529268052088,
-0.649542676209371));
#92231=CARTESIAN_POINT('Ctrl Pts',(-24.3101209896899,-2.70768382376327,
-2.37688058269757));
#92232=CARTESIAN_POINT('Ctrl Pts',(-24.1381592124529,0.106466641732784,
-3.80349368464174));
#92233=CARTESIAN_POINT('Ctrl Pts',(-23.9403412190158,3.2468805350555,-1.98385134146986));
#92234=CARTESIAN_POINT('Ctrl Pts',(-23.7425232255787,3.43298988692531,1.64087774991356));
#92235=CARTESIAN_POINT('Ctrl Pts',(-23.5447052321416,0.495455635705227,
3.77258837765834));
#92236=CARTESIAN_POINT('Ctrl Pts',(-23.3659396738577,-2.56654734681356,
2.59695452658232));
#92237=CARTESIAN_POINT('Ctrl Pts',(-23.2531134467194,-3.21470158249578,
0.757583824704844));
#92238=CARTESIAN_POINT('Ctrl Pts',(-23.2062265507269,-3.2210175372949,-0.00277202775567441));
#92239=CARTESIAN_POINT('Origin',(-31.5777734492731,0.,0.));
#92240=CARTESIAN_POINT('',(-25.9527734492731,-3.22233294691401,-0.00289610800939979));
#92241=CARTESIAN_POINT('',(-25.7062265507269,-3.22723723078879,0.00136747617323019));
#92242=CARTESIAN_POINT('',(-31.5777734492731,-3.22275,-1.53308031181269E-14));
#92243=CARTESIAN_POINT('Ctrl Pts',(-25.9527734492731,-3.22233294691401,
-0.00289610800939966));
#92244=CARTESIAN_POINT('Ctrl Pts',(-25.9365470033718,-3.22469450962706,
-0.265764063637563));
#92245=CARTESIAN_POINT('Ctrl Pts',(-25.8543812263248,-3.07536251639807,
-1.59419957501449));
#92246=CARTESIAN_POINT('Ctrl Pts',(-25.706276118132,-1.23933208819682,-3.59749306908928));
#92247=CARTESIAN_POINT('Ctrl Pts',(-25.508458124695,2.34063535810499,-2.99988788509652));
#92248=CARTESIAN_POINT('Ctrl Pts',(-25.3106401312578,3.79088182894556,0.327285808551454));
#92249=CARTESIAN_POINT('Ctrl Pts',(-25.1128221378208,1.79184233806401,3.35666530231748));
#92250=CARTESIAN_POINT('Ctrl Pts',(-24.9150041443836,-1.83757679742267,
3.3318482175997));
#92251=CARTESIAN_POINT('Ctrl Pts',(-24.7783212482011,-3.19006587685143,
1.21999735035492));
#92252=CARTESIAN_POINT('Ctrl Pts',(-24.7075776831642,-3.22765775267426,
0.0788834148409687));
#92253=CARTESIAN_POINT('Ctrl Pts',(-24.7027734492731,-3.22724337194307,
0.00136199953838148));
#92254=CARTESIAN_POINT('Ctrl Pts',(-25.7062265507269,-3.22723723078879,
0.00136747617323013));
#92255=CARTESIAN_POINT('Ctrl Pts',(-25.6451127559888,-3.22194803267696,
-0.98477327470211));
#92256=CARTESIAN_POINT('Ctrl Pts',(-25.5180596301051,-2.21285103742733,
-3.04428668153654));
#92257=CARTESIAN_POINT('Ctrl Pts',(-25.3250671730756,1.28726128874941,-3.58062253845296));
#92258=CARTESIAN_POINT('Ctrl Pts',(-25.1272491796384,3.70362324127845,-0.872395691996212));
#92259=CARTESIAN_POINT('Ctrl Pts',(-24.9294311862013,2.750094969933,2.62961537102403));
#92260=CARTESIAN_POINT('Ctrl Pts',(-24.7316131927642,-0.705717560089592,
3.7389653762666));
#92261=CARTESIAN_POINT('Ctrl Pts',(-24.5738783142728,-2.94927783324677,
1.91082839397675));
#92262=CARTESIAN_POINT('Ctrl Pts',(-24.482082766927,-3.22060778704532,0.421873457838835));
#92263=CARTESIAN_POINT('Ctrl Pts',(-24.4562265507269,-3.21852362056934,
0.00174837132580694));
#92264=CARTESIAN_POINT('Origin',(-31.5777734492731,0.,0.));
#92265=CARTESIAN_POINT('',(-27.2027734492731,-3.21790541760435,0.00110453296622242));
#92266=CARTESIAN_POINT('',(-26.9562265507269,-3.22234299281458,-0.0028962677614916));
#92267=CARTESIAN_POINT('',(-31.5777734492731,-3.22275,-1.53308031181269E-14));
#92268=CARTESIAN_POINT('Ctrl Pts',(-27.2027734492731,-3.21790541760435,
0.00110453296622223));
#92269=CARTESIAN_POINT('Ctrl Pts',(-27.1655163235793,-3.21603557647176,
-0.60456104426713));
#92270=CARTESIAN_POINT('Ctrl Pts',(-27.0623198667399,-2.76128025085132,
-2.28476931242144));
#92271=CARTESIAN_POINT('Ctrl Pts',(-26.8931840787547,-0.0556657981542161,
-3.80457269099369));
#92272=CARTESIAN_POINT('Ctrl Pts',(-26.6953660853176,3.15941649666726,-2.12037600768663));
#92273=CARTESIAN_POINT('Ctrl Pts',(-26.4975480918805,3.49977824828921,1.49313686004087));
#92274=CARTESIAN_POINT('Ctrl Pts',(-26.2997300984434,0.655725629921395,
3.7480555903611));
#92275=CARTESIAN_POINT('Ctrl Pts',(-26.1181385509076,-2.5027348685329,2.68743146592178));
#92276=CARTESIAN_POINT('Ctrl Pts',(-26.0024863345175,-3.21509783844571,
0.802451199222868));
#92277=CARTESIAN_POINT('Ctrl Pts',(-25.9527734492731,-3.22233294691401,
-0.00289610800939966));
#92278=CARTESIAN_POINT('Ctrl Pts',(-26.9562265507269,-3.22234299281458,
-0.00289626776149219));
#92279=CARTESIAN_POINT('Ctrl Pts',(-26.9400214073421,-3.22470229693142,
-0.265417076013672));
#92280=CARTESIAN_POINT('Ctrl Pts',(-26.8578769328116,-3.07561050857835,
-1.59350023865848));
#92281=CARTESIAN_POINT('Ctrl Pts',(-26.7097931271353,-1.24048741938786,
-3.59709412115127));
#92282=CARTESIAN_POINT('Ctrl Pts',(-26.5119751336982,2.33967134712765,-3.0006396835025));
#92283=CARTESIAN_POINT('Ctrl Pts',(-26.3141571402611,3.79098660083381,0.326068132244285));
#92284=CARTESIAN_POINT('Ctrl Pts',(-26.116339146824,1.79292039549545,3.35608927428751));
#92285=CARTESIAN_POINT('Ctrl Pts',(-25.9185211533869,-1.83650628133122,
3.33243818231883));
#92286=CARTESIAN_POINT('Ctrl Pts',(-25.7818169546879,-3.18988452276931,
1.22069290348142));
#92287=CARTESIAN_POINT('Ctrl Pts',(-25.7110520871345,-3.22765486510794,
0.0792330074626153));
#92288=CARTESIAN_POINT('Ctrl Pts',(-25.7062265507269,-3.22723723078879,
0.00136747617323013));
#92289=CARTESIAN_POINT('Origin',(-31.5777734492731,0.,0.));
#92290=CARTESIAN_POINT('',(-28.4527734492731,-3.22624365146105,0.00223892240347571));
#92291=CARTESIAN_POINT('',(-28.2062265507269,-3.21789432005771,0.00111814815214523));
#92292=CARTESIAN_POINT('',(-31.5777734492731,-3.22275,-1.53308031181269E-14));
#92293=CARTESIAN_POINT('Ctrl Pts',(-28.4527734492731,-3.22624365146105,
0.0022389224034757));
#92294=CARTESIAN_POINT('Ctrl Pts',(-28.3944856437869,-3.21930460272821,
-0.938987714550561));
#92295=CARTESIAN_POINT('Ctrl Pts',(-28.270258507155,-2.28972814938004,-2.95761805447462));
#92296=CARTESIAN_POINT('Ctrl Pts',(-28.0800920393773,1.13358660582709,-3.63202487607056));
#92297=CARTESIAN_POINT('Ctrl Pts',(-27.8822740459403,3.66307656578549,-1.02948321404113));
#92298=CARTESIAN_POINT('Ctrl Pts',(-27.6844560525031,2.85963502885877,2.51011956145336));
#92299=CARTESIAN_POINT('Ctrl Pts',(-27.4866380590661,-0.545794501053909,
3.76560941640859));
#92300=CARTESIAN_POINT('Ctrl Pts',(-27.3260771913227,-2.90674871047044,
2.00373429321426));
#92301=CARTESIAN_POINT('Ctrl Pts',(-27.231455654725,-3.21934490512597,0.467373043966351));
#92302=CARTESIAN_POINT('Ctrl Pts',(-27.2027734492731,-3.21790541760435,
0.00110453296622223));
#92303=CARTESIAN_POINT('Ctrl Pts',(-28.2062265507269,-3.21789432005771,
0.00111814815214498));
#92304=CARTESIAN_POINT('Ctrl Pts',(-28.1689907275496,-3.21603799243794,
-0.604211702459132));
#92305=CARTESIAN_POINT('Ctrl Pts',(-28.0658155732266,-2.76168588303602,
-2.28410602743074));
#92306=CARTESIAN_POINT('Ctrl Pts',(-27.896701087758,-0.056879441065127,
-3.80453263781198));
#92307=CARTESIAN_POINT('Ctrl Pts',(-27.6988830943209,3.15873057113267,-2.12140205749341));
#92308=CARTESIAN_POINT('Ctrl Pts',(-27.5010651008837,3.50025983817255,1.49201838676206));
#92309=CARTESIAN_POINT('Ctrl Pts',(-27.3032471074467,0.656928350055686,
3.74784144106381));
#92310=CARTESIAN_POINT('Ctrl Pts',(-27.1216342573943,-2.50224137881404,
2.6881120697053));
#92311=CARTESIAN_POINT('Ctrl Pts',(-27.0059607384878,-3.21510220073116,
0.802789856618959));
#92312=CARTESIAN_POINT('Ctrl Pts',(-26.9562265507269,-3.22234299281458,
-0.00289626776149219));
#92313=CARTESIAN_POINT('Origin',(-0.4,5.160062080289E-16,2.1385152528819E-16));
#92314=CARTESIAN_POINT('',(-0.4,-0.4995344189117,3.90114782651498));
#92315=CARTESIAN_POINT('Ctrl Pts',(-0.399999999999999,3.01796675574746,
-1.14524144678479));
#92316=CARTESIAN_POINT('Ctrl Pts',(-0.4,3.05385943172044,-1.07546057251878));
#92317=CARTESIAN_POINT('Ctrl Pts',(-0.399999999999999,3.08696973524706,
-1.00441532534134));
#92318=CARTESIAN_POINT('Ctrl Pts',(-0.399999999999999,3.11717685628419,
-0.932224456809624));
#92319=CARTESIAN_POINT('Ctrl Pts',(-0.399999999999998,3.15685849482143,
-0.837390793341891));
#92320=CARTESIAN_POINT('Ctrl Pts',(-0.4,3.1915324278058,-0.740581154760933));
#92321=CARTESIAN_POINT('Ctrl Pts',(-0.4,3.2213387732556,-0.642171654880859));
#92322=CARTESIAN_POINT('Ctrl Pts',(-0.4,3.24002793996668,-0.580466956721544));
#92323=CARTESIAN_POINT('Ctrl Pts',(-0.399999999999998,3.25680254187822,
-0.518132581512819));
#92324=CARTESIAN_POINT('Ctrl Pts',(-0.399999999999998,3.27168843256541,
-0.455255819308803));
#92325=CARTESIAN_POINT('Ctrl Pts',(-0.399999999999998,3.27945954784241,
-0.422431275746028));
#92326=CARTESIAN_POINT('Ctrl Pts',(-0.399999999999996,3.28671581835832,
-0.389458854605961));
#92327=CARTESIAN_POINT('Ctrl Pts',(-0.399999999999996,3.29346019208002,
-0.356350636477125));
#92328=CARTESIAN_POINT('Ctrl Pts',(-0.399999999999996,3.29755533371787,
-0.336247533029876));
#92329=CARTESIAN_POINT('Ctrl Pts',(-0.399999999999985,3.30146027548614,
-0.316101286577043));
#92330=CARTESIAN_POINT('Ctrl Pts',(-0.399999999999986,3.30517468015687,
-0.295922536912268));
#92331=CARTESIAN_POINT('Ctrl Pts',(-0.399999999999987,3.32438655606123,
-0.191552747180045));
#92332=CARTESIAN_POINT('Ctrl Pts',(-0.399999999999996,3.33851780246706,
-0.0862519001458806));
#92333=CARTESIAN_POINT('Ctrl Pts',(-0.399999999999995,3.34771253438542,
0.0195864485897636));
#92334=CARTESIAN_POINT('Ctrl Pts',(-0.399999999999995,3.3564903695163,0.120625998624962));
#92335=CARTESIAN_POINT('Ctrl Pts',(-0.399999999999991,3.36076889984354,
0.222156205388883));
#92336=CARTESIAN_POINT('Ctrl Pts',(-0.399999999999991,3.36063532362138,
0.323852939879256));
#92337=CARTESIAN_POINT('Ctrl Pts',(-0.39999999999999,3.36057596369294,0.36904594491764));
#92338=CARTESIAN_POINT('Ctrl Pts',(-0.399999999999997,3.35964479686966,
0.414272015762765));
#92339=CARTESIAN_POINT('Ctrl Pts',(-0.399999999999998,3.35784710386715,
0.459503349194265));
#92340=CARTESIAN_POINT('Ctrl Pts',(-0.399999999999998,3.35707420233503,
0.478950143980882));
#92341=CARTESIAN_POINT('Ctrl Pts',(-0.399999999999997,3.35614110588597,
0.498397914812365));
#92342=CARTESIAN_POINT('Ctrl Pts',(-0.399999999999997,3.35504815107657,
0.517844463495855));
#92343=CARTESIAN_POINT('Ctrl Pts',(-0.399999999999998,3.35409082912369,
0.534877745935509));
#92344=CARTESIAN_POINT('Ctrl Pts',(-0.399999999999992,3.35301137108497,
0.551900908779291));
#92345=CARTESIAN_POINT('Ctrl Pts',(-0.399999999999992,3.35181049692923,
0.568910960665313));
#92346=CARTESIAN_POINT('Ctrl Pts',(-0.399999999999994,3.34397265912955,
0.679931775801685));
#92347=CARTESIAN_POINT('Ctrl Pts',(-0.399999999999999,3.33096547612328,
0.790412525141181));
#92348=CARTESIAN_POINT('Ctrl Pts',(-0.399999999999999,3.31293843234414,
0.899937431786043));
#92349=CARTESIAN_POINT('Ctrl Pts',(-0.4,3.29463178445671,1.01116109804079));
#92350=CARTESIAN_POINT('Ctrl Pts',(-0.399999999999993,3.27114846169325,
1.12139992524088));
#92351=CARTESIAN_POINT('Ctrl Pts',(-0.399999999999994,3.24259365432844,
1.23023390508146));
#92352=CARTESIAN_POINT('Ctrl Pts',(-0.399999999999994,3.21411812812659,
1.33876571217816));
#92353=CARTESIAN_POINT('Ctrl Pts',(-0.399999999999998,3.18059920173942,
1.4459014170632));
#92354=CARTESIAN_POINT('Ctrl Pts',(-0.400000000000001,3.14209018890566,
1.5512257962275));
#92355=CARTESIAN_POINT('Ctrl Pts',(-0.400000000000002,3.11694027798415,
1.62001225838068));
#92356=CARTESIAN_POINT('Ctrl Pts',(-0.399999999999998,3.08966091557709,
1.68802613622077));
#92357=CARTESIAN_POINT('Ctrl Pts',(-0.399999999999997,3.06025526189474,
1.75514908035963));
#92358=CARTESIAN_POINT('Ctrl Pts',(-0.399999999999997,3.05164036528084,
1.77481391183808));
#92359=CARTESIAN_POINT('Ctrl Pts',(-0.399999999999994,3.04284290901892,
1.79440225257972));
#92360=CARTESIAN_POINT('Ctrl Pts',(-0.399999999999994,3.03386282258109,
1.81391106505042));
#92361=CARTESIAN_POINT('Ctrl Pts',(-0.399999999999994,3.02664727008747,
1.82958651109929));
#92362=CARTESIAN_POINT('Ctrl Pts',(-0.399999999999994,3.01931673828124,
1.84520414701729));
#92363=CARTESIAN_POINT('Ctrl Pts',(-0.399999999999994,3.01187496318844,
1.86075544310257));
#92364=CARTESIAN_POINT('Ctrl Pts',(-0.399999999999995,2.96187696416847,
1.96523773082757));
#92365=CARTESIAN_POINT('Ctrl Pts',(-0.39999999999999,2.90681611202108,2.06682489248903));
#92366=CARTESIAN_POINT('Ctrl Pts',(-0.399999999999992,2.84680781566502,
2.16508365912674));
#92367=CARTESIAN_POINT('Ctrl Pts',(-0.399999999999992,2.81303601982972,
2.22038226294357));
#92368=CARTESIAN_POINT('Ctrl Pts',(-0.399999999999999,2.77769628795341,
2.27462673936948));
#92369=CARTESIAN_POINT('Ctrl Pts',(-0.399999999999999,2.74080195646948,
2.32773919637629));
#92370=CARTESIAN_POINT('Ctrl Pts',(-0.399999999999999,2.67744566437209,
2.41894584533261));
#92371=CARTESIAN_POINT('Ctrl Pts',(-0.399999999999998,2.60950780329113,
2.50681584887859));
#92372=CARTESIAN_POINT('Ctrl Pts',(-0.399999999999997,2.53736550365763,
2.59125872319195));
#92373=CARTESIAN_POINT('Ctrl Pts',(-0.399999999999997,2.46387235100471,
2.67728277681779));
#92374=CARTESIAN_POINT('Ctrl Pts',(-0.400000000000003,2.38601536697427,
2.75975066336544));
#92375=CARTESIAN_POINT('Ctrl Pts',(-0.400000000000003,2.30414671759461,
2.83853907492399));
#92376=CARTESIAN_POINT('Ctrl Pts',(-0.400000000000003,2.27577470203401,
2.86584361769675));
#92377=CARTESIAN_POINT('Ctrl Pts',(-0.4,2.24692051240199,2.89270597751155));
#92378=CARTESIAN_POINT('Ctrl Pts',(-0.4,2.21759770087157,2.91912009175765));
#92379=CARTESIAN_POINT('Ctrl Pts',(-0.4,2.20688460243407,2.92877049672527));
#92380=CARTESIAN_POINT('Ctrl Pts',(-0.400000000000001,2.19610981880862,
2.93836022592291));
#92381=CARTESIAN_POINT('Ctrl Pts',(-0.400000000000001,2.18528158294958,
2.94788250838123));
#92382=CARTESIAN_POINT('Ctrl Pts',(-0.400000000000001,2.09969869901333,
3.02314355783082));
#92383=CARTESIAN_POINT('Ctrl Pts',(-0.399999999999996,2.01065587601546,
3.09430616390818));
#92384=CARTESIAN_POINT('Ctrl Pts',(-0.399999999999996,1.91856670100604,
3.16129393881534));
#92385=CARTESIAN_POINT('Ctrl Pts',(-0.399999999999996,1.8235125715356,3.23043848950015));
#92386=CARTESIAN_POINT('Ctrl Pts',(-0.399999999999996,1.72521235437322,
3.29513561360273));
#92387=CARTESIAN_POINT('Ctrl Pts',(-0.399999999999994,1.62407296298976,
3.35527343326626));
#92388=CARTESIAN_POINT('Ctrl Pts',(-0.399999999999991,1.52197936605142,
3.41597862673732));
#92389=CARTESIAN_POINT('Ctrl Pts',(-0.400000000000002,1.41699210619484,
3.47203860011689));
#92390=CARTESIAN_POINT('Ctrl Pts',(-0.400000000000002,1.30949015933882,
3.52330219657907));
#92391=CARTESIAN_POINT('Ctrl Pts',(-0.400000000000002,1.23934879114686,
3.55674995170775));
#92392=CARTESIAN_POINT('Ctrl Pts',(-0.400000000000001,1.16813610343819,
3.58815507998474));
#92393=CARTESIAN_POINT('Ctrl Pts',(-0.400000000000001,1.09595051685845,
3.61746580574807));
#92394=CARTESIAN_POINT('Ctrl Pts',(-0.400000000000001,1.05572480653037,
3.6337993263292));
#92395=CARTESIAN_POINT('Ctrl Pts',(-0.400000000000002,1.01519689475796,
3.64948232247901));
#92396=CARTESIAN_POINT('Ctrl Pts',(-0.400000000000002,0.974383269726773,
3.66450467150052));
#92397=CARTESIAN_POINT('Ctrl Pts',(-0.400000000000002,0.958753801871717,
3.67025743962537));
#92398=CARTESIAN_POINT('Ctrl Pts',(-0.399999999999996,0.943091728437667,
3.6759098874143));
#92399=CARTESIAN_POINT('Ctrl Pts',(-0.399999999999996,0.927399385258908,
3.68146132666716));
#92400=CARTESIAN_POINT('Ctrl Pts',(-0.399999999999996,0.811870525443297,
3.72233166960525));
#92401=CARTESIAN_POINT('Ctrl Pts',(-0.400000000000004,0.694682613315391,
3.75773824573158));
#92402=CARTESIAN_POINT('Ctrl Pts',(-0.400000000000003,0.576262045218899,
3.78756373718036));
#92403=CARTESIAN_POINT('Ctrl Pts',(-0.400000000000002,0.45763889427005,
3.81744025129545));
#92404=CARTESIAN_POINT('Ctrl Pts',(-0.400000000000002,0.337778087304372,
3.84171704650798));
#92405=CARTESIAN_POINT('Ctrl Pts',(-0.400000000000001,0.217075768755943,
3.86023502674498));
#92406=CARTESIAN_POINT('Ctrl Pts',(-0.4,0.0986485754491533,3.87840396046184));
#92407=CARTESIAN_POINT('Ctrl Pts',(-0.399999999999999,-0.0205895151206229,
3.89102943611732));
#92408=CARTESIAN_POINT('Ctrl Pts',(-0.399999999999998,-0.14028364083043,
3.89791601923602));
#92409=CARTESIAN_POINT('Ctrl Pts',(-0.399999999999997,-0.259694075762963,
3.90478628024948));
#92410=CARTESIAN_POINT('Ctrl Pts',(-0.4,-0.379559128612082,3.90594525600568));
#92411=CARTESIAN_POINT('Ctrl Pts',(-0.4,-0.499534418911701,3.90114782651498));
#92412=CARTESIAN_POINT('',(-0.4,-4.81653586104654E-16,3.933));
#92413=CARTESIAN_POINT('Origin',(-0.4,0.,0.));
#92414=CARTESIAN_POINT('',(-0.40000000000001,-3.41554413377521,1.96277079485755));
#92415=CARTESIAN_POINT('Origin',(-0.4,0.,0.));
#92416=CARTESIAN_POINT('Ctrl Pts',(-0.399999999999993,-3.41555626699905,
1.96277456084997));
#92417=CARTESIAN_POINT('Ctrl Pts',(-0.399999999999994,-3.45586581128785,
1.87693662981294));
#92418=CARTESIAN_POINT('Ctrl Pts',(-0.4,-3.49279526202284,1.78967478039338));
#92419=CARTESIAN_POINT('Ctrl Pts',(-0.400000000000001,-3.52617474615515,
1.70109144698049));
#92420=CARTESIAN_POINT('Ctrl Pts',(-0.400000000000002,-3.56906103703463,
1.58727870533473));
#92421=CARTESIAN_POINT('Ctrl Pts',(-0.399999999999999,-3.60608888168847,
1.4712842047269));
#92422=CARTESIAN_POINT('Ctrl Pts',(-0.400000000000001,-3.63733134408434,
1.3535520921038));
#92423=CARTESIAN_POINT('Ctrl Pts',(-0.400000000000001,-3.65528841060761,
1.28588382218609));
#92424=CARTESIAN_POINT('Ctrl Pts',(-0.400000000000002,-3.67133327041293,
1.2176413971065));
#92425=CARTESIAN_POINT('Ctrl Pts',(-0.400000000000004,-3.68547211562788,
1.14890933338331));
#92426=CARTESIAN_POINT('Ctrl Pts',(-0.400000000000005,-3.69433691436354,
1.10581557980372));
#92427=CARTESIAN_POINT('Ctrl Pts',(-0.400000000000003,-3.70245233702665,
1.06252935589371));
#92428=CARTESIAN_POINT('Ctrl Pts',(-0.400000000000002,-3.70981882690422,
1.0190717129688));
#92429=CARTESIAN_POINT('Ctrl Pts',(-0.400000000000002,-3.71320117185905,
0.999118011580692));
#92430=CARTESIAN_POINT('Ctrl Pts',(-0.400000000000009,-3.71642544923357,
0.979128724847171));
#92431=CARTESIAN_POINT('Ctrl Pts',(-0.400000000000009,-3.71948985922468,
0.959119148092641));
#92432=CARTESIAN_POINT('Ctrl Pts',(-0.40000000000001,-3.73823141925564,
0.83674300226789));
#92433=CARTESIAN_POINT('Ctrl Pts',(-0.400000000000023,-3.75102036592465,
0.713479450781438));
#92434=CARTESIAN_POINT('Ctrl Pts',(-0.400000000000019,-3.75793544512979,
0.58979761469609));
#92435=CARTESIAN_POINT('Ctrl Pts',(-0.400000000000016,-3.76398613943429,
0.481576008121411));
#92436=CARTESIAN_POINT('Ctrl Pts',(-0.400000000000006,-3.76553866286515,
0.373033640931303));
#92437=CARTESIAN_POINT('Ctrl Pts',(-0.400000000000004,-3.76261070624249,
0.264490932332908));
#92438=CARTESIAN_POINT('Ctrl Pts',(-0.400000000000003,-3.76132972522008,
0.21700349732111));
#92439=CARTESIAN_POINT('Ctrl Pts',(-0.400000000000014,-3.75919074263992,
0.169516123263878));
#92440=CARTESIAN_POINT('Ctrl Pts',(-0.400000000000015,-3.75619336846896,
0.122056406365339));
#92441=CARTESIAN_POINT('Ctrl Pts',(-0.400000000000015,-3.7544301202536,
0.0941375492758329));
#92442=CARTESIAN_POINT('Ctrl Pts',(-0.400000000000005,-3.75236980031072,
0.0662282734061994));
#92443=CARTESIAN_POINT('Ctrl Pts',(-0.400000000000004,-3.75001215099025,
0.0383342975575875));
#92444=CARTESIAN_POINT('Ctrl Pts',(-0.400000000000004,-3.74818369217564,
0.0167013152595263));
#92445=CARTESIAN_POINT('Ctrl Pts',(-0.400000000000019,-3.74617606664209,
-0.0049248646594703));
#92446=CARTESIAN_POINT('Ctrl Pts',(-0.400000000000019,-3.74399167965982,
-0.0265186312542417));
#92447=CARTESIAN_POINT('Ctrl Pts',(-0.400000000000018,-3.7320274191325,
-0.144791378438078));
#92448=CARTESIAN_POINT('Ctrl Pts',(-0.400000000000008,-3.71475353950831,
-0.262239439074446));
#92449=CARTESIAN_POINT('Ctrl Pts',(-0.400000000000008,-3.69223626798488,
-0.378452392337834));
#92450=CARTESIAN_POINT('Ctrl Pts',(-0.400000000000008,-3.66987919815232,
-0.4938385353194));
#92451=CARTESIAN_POINT('Ctrl Pts',(-0.400000000000015,-3.64235278957465,
-0.608007931120418));
#92452=CARTESIAN_POINT('Ctrl Pts',(-0.400000000000015,-3.6096739605563,
-0.720541241088965));
#92453=CARTESIAN_POINT('Ctrl Pts',(-0.400000000000015,-3.57795867401629,
-0.829756481602768));
#92454=CARTESIAN_POINT('Ctrl Pts',(-0.400000000000005,-3.54138992891154,
-0.937431313648108));
#92455=CARTESIAN_POINT('Ctrl Pts',(-0.400000000000006,-3.49994321149449,
-1.04315520271956));
#92456=CARTESIAN_POINT('Ctrl Pts',(-0.400000000000006,-3.4716806339255,
-1.11524847818238));
#92457=CARTESIAN_POINT('Ctrl Pts',(-0.400000000000003,-3.44114903570196,
-1.18643402337789));
#92458=CARTESIAN_POINT('Ctrl Pts',(-0.400000000000003,-3.40833081899823,
-1.25657189330865));
#92459=CARTESIAN_POINT('Ctrl Pts',(-0.400000000000003,-3.39794175690299,
-1.2787750097216));
#92460=CARTESIAN_POINT('Ctrl Pts',(-0.400000000000002,-3.38732348880224,
-1.3008730681313));
#92461=CARTESIAN_POINT('Ctrl Pts',(-0.400000000000002,-3.3764752978588,
-1.32286143260974));
#92462=CARTESIAN_POINT('Ctrl Pts',(-0.400000000000002,-3.36937925489342,
-1.33724451084749));
#92463=CARTESIAN_POINT('Ctrl Pts',(-0.400000000000004,-3.36218359172965,
-1.3515830717022));
#92464=CARTESIAN_POINT('Ctrl Pts',(-0.400000000000004,-3.35489225176958,
-1.36586767082509));
#92465=CARTESIAN_POINT('Ctrl Pts',(-0.400000000000006,-3.30395288020021,
-1.4656639368647));
#92466=CARTESIAN_POINT('Ctrl Pts',(-0.400000000000003,-3.24844027608969,
-1.56265069548797));
#92467=CARTESIAN_POINT('Ctrl Pts',(-0.400000000000004,-3.18837281836721,
-1.65645757823181));
#92468=CARTESIAN_POINT('Ctrl Pts',(-0.400000000000005,-3.14561797202901,
-1.72322749008171));
#92469=CARTESIAN_POINT('Ctrl Pts',(-0.400000000000004,-3.10055458235714,
-1.78838591080347));
#92470=CARTESIAN_POINT('Ctrl Pts',(-0.400000000000004,-3.05317683241366,
-1.85178896301253));
#92471=CARTESIAN_POINT('Ctrl Pts',(-0.400000000000004,-2.98537511675161,
-1.94252429179267));
#92472=CARTESIAN_POINT('Ctrl Pts',(-0.40000000000001,-2.91283434670415,
-2.02966653669181));
#92473=CARTESIAN_POINT('Ctrl Pts',(-0.400000000000008,-2.83593089936814,
-2.11303626961663));
#92474=CARTESIAN_POINT('Ctrl Pts',(-0.400000000000005,-2.75873941564364,
-2.19671825794237));
#92475=CARTESIAN_POINT('Ctrl Pts',(-0.400000000000014,-2.67715161752483,
-2.27659978388866));
#92476=CARTESIAN_POINT('Ctrl Pts',(-0.400000000000015,-2.59152627560853,
-2.35245214060421));
#92477=CARTESIAN_POINT('Ctrl Pts',(-0.400000000000015,-2.57282073634438,
-2.36902269325915));
#92478=CARTESIAN_POINT('Ctrl Pts',(-0.400000000000002,-2.55392245661421,
-2.3854007680765));
#92479=CARTESIAN_POINT('Ctrl Pts',(-0.400000000000002,-2.53483510403623,
-2.40158365556471));
#92480=CARTESIAN_POINT('Ctrl Pts',(-0.400000000000002,-2.51820440401829,
-2.4156837119314));
#92481=CARTESIAN_POINT('Ctrl Pts',(-0.400000000000011,-2.50142627206165,
-2.42963864398316));
#92482=CARTESIAN_POINT('Ctrl Pts',(-0.400000000000011,-2.48452672290024,
-2.44342770418704));
#92483=CARTESIAN_POINT('Ctrl Pts',(-0.400000000000008,-2.39827220288853,
-2.51380643192344));
#92484=CARTESIAN_POINT('Ctrl Pts',(-0.400000000000015,-2.30875623932578,
-2.57995647049072));
#92485=CARTESIAN_POINT('Ctrl Pts',(-0.400000000000014,-2.21635638722814,
-2.64173828957315));
#92486=CARTESIAN_POINT('Ctrl Pts',(-0.400000000000013,-2.1238561535402,
-2.703587227348));
#92487=CARTESIAN_POINT('Ctrl Pts',(-0.400000000000001,-2.02846485802401,
-2.76105874771976));
#92488=CARTESIAN_POINT('Ctrl Pts',(-0.400000000000003,-1.93053914104806,
-2.81396554239287));
#92489=CARTESIAN_POINT('Ctrl Pts',(-0.400000000000004,-1.83380515901436,
-2.86622847273859));
#92490=CARTESIAN_POINT('Ctrl Pts',(-0.400000000000014,-1.73459720535212,
-2.91403727878679));
#92491=CARTESIAN_POINT('Ctrl Pts',(-0.400000000000016,-1.6332506304093,
-2.95716191024929));
#92492=CARTESIAN_POINT('Ctrl Pts',(-0.400000000000017,-1.57298067615276,
-2.98280776524775));
#92493=CARTESIAN_POINT('Ctrl Pts',(-0.400000000000011,-1.51195428265001,
-3.0067960672628));
#92494=CARTESIAN_POINT('Ctrl Pts',(-0.400000000000011,-1.45024239915814,
-3.02906958386214));
#92495=CARTESIAN_POINT('Ctrl Pts',(-0.400000000000012,-1.42096324775188,
-3.0396372351468));
#92496=CARTESIAN_POINT('Ctrl Pts',(-0.40000000000001,-1.39152980408315,
-3.04981878609203));
#92497=CARTESIAN_POINT('Ctrl Pts',(-0.40000000000001,-1.36194974487981,
-3.05960757992356));
#92498=CARTESIAN_POINT('Ctrl Pts',(-0.40000000000001,-1.34596495330587,
-3.06489735395956));
#92499=CARTESIAN_POINT('Ctrl Pts',(-0.40000000000001,-1.32994425166988,
-3.07007010522677));
#92500=CARTESIAN_POINT('Ctrl Pts',(-0.40000000000001,-1.31389608522276,
-3.07512291332643));
#92501=CARTESIAN_POINT('Ctrl Pts',(-0.400000000000011,-1.21135478554361,
-3.10740831560437));
#92502=CARTESIAN_POINT('Ctrl Pts',(-0.400000000000022,-1.10760140379211,
-3.13483125191197));
#92503=CARTESIAN_POINT('Ctrl Pts',(-0.40000000000002,-1.00295989448995,
-3.15722300264388));
#92504=CARTESIAN_POINT('Ctrl Pts',(-0.400000000000018,-0.899785788764044,
-3.17930075049756));
#92505=CARTESIAN_POINT('Ctrl Pts',(-0.400000000000015,-0.795747515823994,
-3.1964875260079));
#92506=CARTESIAN_POINT('Ctrl Pts',(-0.400000000000016,-0.691154690506712,
-3.20857188447556));
#92507=CARTESIAN_POINT('Ctrl Pts',(-0.400000000000016,-0.589773280006148,
-3.22028520518115));
#92508=CARTESIAN_POINT('Ctrl Pts',(-0.400000000000013,-0.48787023799748,
-3.2272045644463));
#92509=CARTESIAN_POINT('Ctrl Pts',(-0.400000000000014,-0.385736684885698,
-3.22909034216834));
#92510=CARTESIAN_POINT('Ctrl Pts',(-0.400000000000014,-0.29114362765779,
-3.23083689337062));
#92511=CARTESIAN_POINT('Ctrl Pts',(-0.40000000000001,-0.196352551596845,
-3.22826531799378));
#92512=CARTESIAN_POINT('Ctrl Pts',(-0.40000000000001,-0.101608697681888,
-3.22114781328883));
#92513=CARTESIAN_POINT('Ctrl Pts',(-29.6770630286919,-1.43290239521317,
2.8866777250487));
#92514=CARTESIAN_POINT('Ctrl Pts',(-29.6111236975462,-2.38968372905088,
2.41174619630378));
#92515=CARTESIAN_POINT('Ctrl Pts',(-29.4792450352548,-3.77781470893137,
0.444337671635494));
#92516=CARTESIAN_POINT('Ctrl Pts',(-29.2814270418177,-2.42921825930742,
-2.93180374517478));
#92517=CARTESIAN_POINT('Ctrl Pts',(-29.0836090483806,1.13283940936973,-3.63131203549138));
#92518=CARTESIAN_POINT('Ctrl Pts',(-28.8857910549435,3.66252655955179,-1.03121985822236));
#92519=CARTESIAN_POINT('Ctrl Pts',(-28.6879730615064,2.8605553688775,2.50949297218581));
#92520=CARTESIAN_POINT('Ctrl Pts',(-28.4901550680693,-0.544644508144919,
3.76563167765424));
#92521=CARTESIAN_POINT('Ctrl Pts',(-28.2923370746322,-3.45404918098007,
1.59609170665207));
#92522=CARTESIAN_POINT('Ctrl Pts',(-28.0945190811951,-3.22076798380931,
-2.02604665891755));
#92523=CARTESIAN_POINT('Ctrl Pts',(-27.896701087758,-0.056879441065127,
-3.80453263781198));
#92524=CARTESIAN_POINT('Ctrl Pts',(-27.6988830943209,3.15873057113267,-2.12140205749341));
#92525=CARTESIAN_POINT('Ctrl Pts',(-27.5010651008837,3.50025983817255,1.49201838676206));
#92526=CARTESIAN_POINT('Ctrl Pts',(-27.3032471074467,0.656928350055686,
3.74784144106381));
#92527=CARTESIAN_POINT('Ctrl Pts',(-27.1054291140095,-2.78413111524294,
2.59355341701617));
#92528=CARTESIAN_POINT('Ctrl Pts',(-26.9076111205725,-3.69193959240583,
-0.920589964011001));
#92529=CARTESIAN_POINT('Ctrl Pts',(-26.7097931271353,-1.24048741938786,
-3.59709412115127));
#92530=CARTESIAN_POINT('Ctrl Pts',(-26.5119751336982,2.33967134712765,-3.0006396835025));
#92531=CARTESIAN_POINT('Ctrl Pts',(-26.3141571402611,3.79098660083381,0.326068132244285));
#92532=CARTESIAN_POINT('Ctrl Pts',(-26.116339146824,1.79292039549545,3.35608927428751));
#92533=CARTESIAN_POINT('Ctrl Pts',(-25.9185211533869,-1.83650628133122,
3.33243818231883));
#92534=CARTESIAN_POINT('Ctrl Pts',(-25.7207031599498,-3.79491407443894,
0.276634354159837));
#92535=CARTESIAN_POINT('Ctrl Pts',(-25.5228851665127,-2.30036699385748,
-3.03087627035208));
#92536=CARTESIAN_POINT('Ctrl Pts',(-25.3250671730756,1.28726128874941,-3.58062253845296));
#92537=CARTESIAN_POINT('Ctrl Pts',(-25.1272491796384,3.70362324127845,-0.872395691996212));
#92538=CARTESIAN_POINT('Ctrl Pts',(-24.9294311862013,2.750094969933,2.62961537102403));
#92539=CARTESIAN_POINT('Ctrl Pts',(-24.7316131927642,-0.705717560089592,
3.7389653762666));
#92540=CARTESIAN_POINT('Ctrl Pts',(-24.5337951993271,-3.51940465095792,
1.44626769885165));
#92541=CARTESIAN_POINT('Ctrl Pts',(-24.33597720589,-3.13082019758146,-2.16237467684802));
#92542=CARTESIAN_POINT('Ctrl Pts',(-24.1381592124529,0.106466641732784,
-3.80349368464174));
#92543=CARTESIAN_POINT('Ctrl Pts',(-23.9403412190158,3.2468805350555,-1.98385134146986));
#92544=CARTESIAN_POINT('Ctrl Pts',(-23.7425232255787,3.43298988692531,1.64087774991356));
#92545=CARTESIAN_POINT('Ctrl Pts',(-23.5447052321416,0.495455635705227,
3.77258837765834));
#92546=CARTESIAN_POINT('Ctrl Pts',(-23.3468872387045,-2.89288880667469,
2.47165808846236));
#92547=CARTESIAN_POINT('Ctrl Pts',(-23.1490692452673,-3.64902228624806,
-1.0782094919416));
#92548=CARTESIAN_POINT('Ctrl Pts',(-22.9512512518303,-1.08494641550995,
-3.6470249011433));
#92549=CARTESIAN_POINT('Ctrl Pts',(-22.7534332583931,2.46631148668775,-2.89744836100596));
#92550=CARTESIAN_POINT('Ctrl Pts',(-22.555615264956,3.77349691781262,0.488487835391227));
#92551=CARTESIAN_POINT('Ctrl Pts',(-22.357797271519,1.64721476033769,3.42995377336155));
#92552=CARTESIAN_POINT('Ctrl Pts',(-22.1599792780818,-1.97785184410161,
3.25053863795708));
#92553=CARTESIAN_POINT('Ctrl Pts',(-21.9621612846447,-3.80329058354344,
0.113490489462255));
#92554=CARTESIAN_POINT('Ctrl Pts',(-21.7643432912076,-2.16815277209852,
-3.12682153486743));
#92555=CARTESIAN_POINT('Ctrl Pts',(-21.5665252977705,1.43976583982743,-3.52206951670956));
#92556=CARTESIAN_POINT('Ctrl Pts',(-21.3687073043334,3.7376557293535,-0.712621219793359));
#92557=CARTESIAN_POINT('Ctrl Pts',(-21.1708893108963,2.63468957378667,2.74523408908033));
#92558=CARTESIAN_POINT('Ctrl Pts',(-20.9730713174592,-0.865554611853212,
3.70522800485591));
#92559=CARTESIAN_POINT('Ctrl Pts',(-20.7752533240221,-3.57823920205966,
1.29387154188981));
#92560=CARTESIAN_POINT('Ctrl Pts',(-20.577435330585,-3.03511927138851,-2.2947658622428));
#92561=CARTESIAN_POINT('Ctrl Pts',(-20.3796173371479,0.269625717635743,
-3.79541846526285));
#92562=CARTESIAN_POINT('Ctrl Pts',(-20.1817993437108,3.3290409282824,-1.84265728009565));
#92563=CARTESIAN_POINT('Ctrl Pts',(-19.9839813502737,3.35939466694879,1.78671957109805));
#92564=CARTESIAN_POINT('Ctrl Pts',(-19.7861633568365,0.333068366514352,
3.79037792539165));
#92565=CARTESIAN_POINT('Ctrl Pts',(-19.5883453633995,-2.99631355212319,
2.34520882895996));
#92566=CARTESIAN_POINT('Ctrl Pts',(-19.3905273699623,-3.59937935322612,
-1.23384262596099));
#92567=CARTESIAN_POINT('Ctrl Pts',(-19.1927093765252,-0.927405418628458,
-3.69023285763479));
#92568=CARTESIAN_POINT('Ctrl Pts',(-18.9948913830881,2.58840554981504,-2.78891664697164));
#92569=CARTESIAN_POINT('Ctrl Pts',(-18.797073389651,3.74905186462063,0.650007284923323));
#92570=CARTESIAN_POINT('Ctrl Pts',(-18.5992553962139,1.49847290337135,3.4974960059921));
#92571=CARTESIAN_POINT('Ctrl Pts',(-18.4014374027768,-2.11555175776316,
3.16264764308231));
#92572=CARTESIAN_POINT('Ctrl Pts',(-18.2036194093397,-3.80465676201416,
-0.0498625844572021));
#92573=CARTESIAN_POINT('Ctrl Pts',(-18.0058014159026,-2.03194214307649,
-3.21700333870802));
#92574=CARTESIAN_POINT('Ctrl Pts',(-17.8079834224654,1.5896165698452,-3.45702451755008));
#92575=CARTESIAN_POINT('Ctrl Pts',(-17.6101654290284,3.76479886064709,-0.551533220159296));
#92576=CARTESIAN_POINT('Ctrl Pts',(-17.4123474355912,2.51442783918464,2.85579270879419));
#92577=CARTESIAN_POINT('Ctrl Pts',(-17.2145294421542,-1.0237962474182,3.66466104815183));
#92578=CARTESIAN_POINT('Ctrl Pts',(-17.016711448717,-3.6304782367563,1.13909048214257));
#92579=CARTESIAN_POINT('Ctrl Pts',(-16.8188934552799,-2.93382392331867,
-2.42292726697108));
#92580=CARTESIAN_POINT('Ctrl Pts',(-16.6210754618428,0.432287811384032,
-3.7803474181876));
#92581=CARTESIAN_POINT('Ctrl Pts',(-16.4232574684057,3.40506513462136,-1.69806677814945));
#92582=CARTESIAN_POINT('Ctrl Pts',(-16.2254394749686,3.27960731114141,1.92926805778166));
#92583=CARTESIAN_POINT('Ctrl Pts',(-16.0276214815315,0.170067175844205,
3.80118093620512));
#92584=CARTESIAN_POINT('Ctrl Pts',(-15.8298034880944,-3.09421540362715,
2.21443681102563));
#92585=CARTESIAN_POINT('Ctrl Pts',(-15.6319854946573,-3.54310193749609,
-1.38720150467778));
#92586=CARTESIAN_POINT('Ctrl Pts',(-15.4341675012202,-0.768155000592636,
-3.72663886754987));
#92587=CARTESIAN_POINT('Ctrl Pts',(-15.236349507783,2.70572858711511,-2.67524431911123));
#92588=CARTESIAN_POINT('Ctrl Pts',(-15.038531514346,3.71769644791273,0.81032862176155));
#92589=CARTESIAN_POINT('Ctrl Pts',(-14.8407135209088,1.34696901673613,3.5585915503218));
#92590=CARTESIAN_POINT('Ctrl Pts',(-14.6428955274718,-2.24935222372163,
3.06892716233335));
#92591=CARTESIAN_POINT('Ctrl Pts',(-14.4450775340346,-3.79901008437419,
-0.213123750183017));
#92592=CARTESIAN_POINT('Ctrl Pts',(-14.2472595405976,-1.89198617807126,
-3.3012554666454));
#92593=CARTESIAN_POINT('Ctrl Pts',(-14.0494415471604,1.73653727148651,-3.38560742833646));
#92594=CARTESIAN_POINT('Ctrl Pts',(-13.8516235537233,3.78500260309515,-0.389428618146851));
#92595=CARTESIAN_POINT('Ctrl Pts',(-13.6538055602862,2.38953143666386,2.96108744674385));
#92596=CARTESIAN_POINT('Ctrl Pts',(-13.4559875668491,-1.18015079139549,
3.61733927958623));
#92597=CARTESIAN_POINT('Ctrl Pts',(-13.258169573412,-3.67602546636253,0.982209817056931));
#92598=CARTESIAN_POINT('Ctrl Pts',(-13.0603515799749,-2.82712086403723,
-2.54662266034728));
#92599=CARTESIAN_POINT('Ctrl Pts',(-12.8625335865378,0.594153099425664,
-3.75830832270474));
#92600=CARTESIAN_POINT('Ctrl Pts',(-12.6647155931007,3.47481302398082,-1.55034634918851));
#92601=CARTESIAN_POINT('Ctrl Pts',(-12.4668975996636,3.19377488593328,2.0682604603992));
#92602=CARTESIAN_POINT('Ctrl Pts',(-12.2690796062265,0.00675251231494511,
3.80497749765308));
#92603=CARTESIAN_POINT('Ctrl Pts',(-12.0712616127893,-3.18641390558911,
2.07958307752715));
#92604=CARTESIAN_POINT('Ctrl Pts',(-11.8734436193523,-3.48029377126023,
-1.53800345246562));
#92605=CARTESIAN_POINT('Ctrl Pts',(-11.6756256259151,-0.607488696492234,
-3.75617582624975));
#92606=CARTESIAN_POINT('Ctrl Pts',(-11.477807632478,2.81806434528784,-2.55664090162977));
#92607=CARTESIAN_POINT('Ctrl Pts',(-11.2799896390409,3.67948846292253,0.969156336866661));
#92608=CARTESIAN_POINT('Ctrl Pts',(-11.0821716456038,1.1929823568862,3.61312779323221));
#92609=CARTESIAN_POINT('Ctrl Pts',(-10.8843536521667,-2.37900661699238,
2.96954994407828));
#92610=CARTESIAN_POINT('Ctrl Pts',(-10.6865356587296,-3.78636095874714,
-0.37599207989568));
#92611=CARTESIAN_POINT('Ctrl Pts',(-10.4887176652925,-1.74854284806569,
-3.37942262266014));
#92612=CARTESIAN_POINT('Ctrl Pts',(-10.2908996718554,1.88025713615946,-3.30794988716429));
#92613=CARTESIAN_POINT('Ctrl Pts',(-10.0930816784183,3.79822971656082,-0.226606209763087));
#92614=CARTESIAN_POINT('Ctrl Pts',(-9.89526368498117,2.26023057897525,3.06092422054745));
#92615=CARTESIAN_POINT('Ctrl Pts',(-9.69744569154406,-1.33433004645538,
3.56334992404553));
#92616=CARTESIAN_POINT('Ctrl Pts',(-9.49962769810695,-3.71479693687478,
0.823518713724579));
#92617=CARTESIAN_POINT('Ctrl Pts',(-9.30180970466985,-2.71520677178563,
-2.66562404335614));
#92618=CARTESIAN_POINT('Ctrl Pts',(-9.10399171123273,0.754923226864277,
-3.72934180192827));
#92619=CARTESIAN_POINT('Ctrl Pts',(-8.90617371779564,3.53815603498388,-1.3997682758857));
#92620=CARTESIAN_POINT('Ctrl Pts',(-8.70835572435851,3.10205560019449,2.20344058403463));
#92621=CARTESIAN_POINT('Ctrl Pts',(-8.51053773092143,-0.156574597645193,
3.80176061180093));
#92622=CARTESIAN_POINT('Ctrl Pts',(-8.3127197374843,-3.27273911499761,1.94089619486303));
#92623=CARTESIAN_POINT('Ctrl Pts',(-8.11490174404721,-3.41107062439205,
-1.68597050670474));
#92624=CARTESIAN_POINT('Ctrl Pts',(-7.91708375061009,-0.445702651221169,
-3.77878929033658));
#92625=CARTESIAN_POINT('Ctrl Pts',(-7.71926575717298,2.92520576373441,-2.43332500786197));
#92626=CARTESIAN_POINT('Ctrl Pts',(-7.52144776373588,3.63449833574001,1.12619767428708));
#92627=CARTESIAN_POINT('Ctrl Pts',(-7.32362977029877,1.03679675659798,3.66100421190307));
#92628=CARTESIAN_POINT('Ctrl Pts',(-7.12581177686167,-2.50427595475653,
2.86469916335302));
#92629=CARTESIAN_POINT('Ctrl Pts',(-6.92799378342455,-3.76673270037306,
-0.538167369865845));
#92630=CARTESIAN_POINT('Ctrl Pts',(-6.73017578998745,-1.60187655206341,
-3.45136072672716));
#92631=CARTESIAN_POINT('Ctrl Pts',(-6.53235779655034,2.02051125516165,-3.22419503472727));
#92632=CARTESIAN_POINT('Ctrl Pts',(-6.33453980311323,3.80445582041375,-0.0633661140739026));
#92633=CARTESIAN_POINT('Ctrl Pts',(-6.13672180967612,2.12676359733563,3.1551190080601));
#92634=CARTESIAN_POINT('Ctrl Pts',(-5.93890381623902,-1.48604982490852,
3.50279249639495));
#92635=CARTESIAN_POINT('Ctrl Pts',(-5.74108582280191,-3.74672118340988,
0.66330967612812));
#92636=CARTESIAN_POINT('Ctrl Pts',(-5.5432678293648,-2.59828793024122,-2.77971206881013));
#92637=CARTESIAN_POINT('Ctrl Pts',(-5.34544983592769,0.914301858020527,
-3.69350124840367));
#92638=CARTESIAN_POINT('Ctrl Pts',(-5.14763184249059,3.59497741079579,-1.24661010706821));
#92639=CARTESIAN_POINT('Ctrl Pts',(-4.94981384905348,3.00461851577406,2.33455925849379));
#92640=CARTESIAN_POINT('Ctrl Pts',(-4.75199585561637,-0.319613108768782,
3.79153621228826));
#92641=CARTESIAN_POINT('Ctrl Pts',(-4.55417786217927,-3.35303190681402,
1.79863178680334));
#92642=CARTESIAN_POINT('Ctrl Pts',(-4.35635986874215,-3.33556010608343,
-1.83082991481484));
#92643=CARTESIAN_POINT('Ctrl Pts',(-4.15854187530505,-0.283095044828532,
-3.79443760733249));
#92644=CARTESIAN_POINT('Ctrl Pts',(-3.96072388186794,3.02695530111143,-2.30552388116989));
#92645=CARTESIAN_POINT('Ctrl Pts',(-3.76290588843083,3.58280909899496,1.28116306328493));
#92646=CARTESIAN_POINT('Ctrl Pts',(-3.56508789499372,0.878699899841087,
3.70213276488018));
#92647=CARTESIAN_POINT('Ctrl Pts',(-3.36726990155662,-2.62492895022921,
2.75456769027902));
#92648=CARTESIAN_POINT('Ctrl Pts',(-3.1694519081195,-3.74016222880254,-0.699349939622732));
#92649=CARTESIAN_POINT('Ctrl Pts',(-2.9716339146824,-1.45225621275822,-3.51693862418514));
#92650=CARTESIAN_POINT('Ctrl Pts',(-2.7738159212453,2.15703839529281,-3.13449448646742));
#92651=CARTESIAN_POINT('Ctrl Pts',(-2.57599792780818,3.80367463162103,0.0999854885590033));
#92652=CARTESIAN_POINT('Ctrl Pts',(-2.37817993437108,1.98936656034495,3.24350831648798));
#92653=CARTESIAN_POINT('Ctrl Pts',(-2.18036194093398,-1.63501143994855,
3.43575922529938));
#92654=CARTESIAN_POINT('Ctrl Pts',(-1.98254394749686,-3.77177579799328,
0.501915131585207));
#92655=CARTESIAN_POINT('Ctrl Pts',(-1.78472595405976,-2.47651009463211,
-2.88874751957624));
#92656=CARTESIAN_POINT('Ctrl Pts',(-1.58690796062265,1.07186168277273,-3.65071665635791));
#92657=CARTESIAN_POINT('Ctrl Pts',(-1.38908996718554,3.64542809306271,-1.09141468478898));
#92658=CARTESIAN_POINT('Ctrl Pts',(-1.19127197374844,2.90115349698225,2.46187399806776));
#92659=CARTESIAN_POINT('Ctrl Pts',(-0.993453980311327,-0.481122552182907,
3.77336366075504));
#92660=CARTESIAN_POINT('Ctrl Pts',(-0.795635986874217,-3.42896535177265,
1.65492331179306));
#92661=CARTESIAN_POINT('Ctrl Pts',(-0.597817993437111,-3.25022050800311,
-1.97620509836622));
#92662=CARTESIAN_POINT('Ctrl Pts',(-0.465939331145708,-1.16924921554908,
-3.18746989196983));
#92663=CARTESIAN_POINT('Ctrl Pts',(-0.400000000000005,-0.101608697681796,
-3.22114781328883));
#92664=CARTESIAN_POINT('Ctrl Pts',(-29.5403753524613,-1.53816642191916,
3.09873914818276));
#92665=CARTESIAN_POINT('Ctrl Pts',(-29.4744360213156,-2.5652349268952,2.5889181494416));
#92666=CARTESIAN_POINT('Ctrl Pts',(-29.3425573590242,-4.05534093105207,
0.47697965247785));
#92667=CARTESIAN_POINT('Ctrl Pts',(-29.144739365587,-2.60767374697821,-3.14718022075313));
#92668=CARTESIAN_POINT('Ctrl Pts',(-28.94692137215,1.2160601773996,-3.89807586278254));
#92669=CARTESIAN_POINT('Ctrl Pts',(-28.7491033787128,3.93158347149777,-1.10697544008076));
#92670=CARTESIAN_POINT('Ctrl Pts',(-28.5512853852758,3.07069778873066,2.69384560927059));
#92671=CARTESIAN_POINT('Ctrl Pts',(-28.3534673918386,-0.584655240377733,
4.04226290864784));
#92672=CARTESIAN_POINT('Ctrl Pts',(-28.1556493984016,-3.7077909057794,1.71334396374614));
#92673=CARTESIAN_POINT('Ctrl Pts',(-27.9578314049644,-3.45737238072711,
-2.17488431200846));
#92674=CARTESIAN_POINT('Ctrl Pts',(-27.7600134115274,-0.0610579245566097,
-4.0840216152387));
#92675=CARTESIAN_POINT('Ctrl Pts',(-27.5621954180902,3.39077756910511,-2.2772447189197));
#92676=CARTESIAN_POINT('Ctrl Pts',(-27.3643774246531,3.7573962951386,1.60162519866677));
#92677=CARTESIAN_POINT('Ctrl Pts',(-27.1665594312159,0.705187689711472,
4.02316576382289));
#92678=CARTESIAN_POINT('Ctrl Pts',(-26.9687414377789,-2.98865924852468,
2.78408131135441));
#92679=CARTESIAN_POINT('Ctrl Pts',(-26.7709234443418,-3.96315724766984,
-0.988218440926554));
#92680=CARTESIAN_POINT('Ctrl Pts',(-26.5731054509047,-1.33161623686985,
-3.86134422841449));
#92681=CARTESIAN_POINT('Ctrl Pts',(-26.3752874574675,2.51154853010259,-3.22107299203379));
#92682=CARTESIAN_POINT('Ctrl Pts',(-26.1774694640305,4.06948045786504,0.3500217837248));
#92683=CARTESIAN_POINT('Ctrl Pts',(-25.9796514705934,1.92463210246421,3.60263465810181));
#92684=CARTESIAN_POINT('Ctrl Pts',(-25.7818334771562,-1.97141989923679,
3.57724610712342));
#92685=CARTESIAN_POINT('Ctrl Pts',(-25.5840154837191,-4.07369645194989,
0.296956496227123));
#92686=CARTESIAN_POINT('Ctrl Pts',(-25.386197490282,-2.46935679629198,-3.25353082221178));
#92687=CARTESIAN_POINT('Ctrl Pts',(-25.1883794968449,1.38182621314983,-3.8436626085728));
#92688=CARTESIAN_POINT('Ctrl Pts',(-24.9905615034078,3.97569920198674,-0.936483716224004));
#92689=CARTESIAN_POINT('Ctrl Pts',(-24.7927435099707,2.95212273632246,2.82279245242654));
#92690=CARTESIAN_POINT('Ctrl Pts',(-24.5949255165336,-0.757561057832579,
4.01363764461851));
#92691=CARTESIAN_POINT('Ctrl Pts',(-24.3971075230965,-3.77794752617762,
1.55251356890149));
#92692=CARTESIAN_POINT('Ctrl Pts',(-24.1992895296594,-3.36081684075186,
-2.32122727315359));
#92693=CARTESIAN_POINT('Ctrl Pts',(-24.0014715362223,0.114287905383463,
-4.08290633838123));
#92694=CARTESIAN_POINT('Ctrl Pts',(-23.8036535427852,3.48540321496378,-2.12958923770538));
#92695=CARTESIAN_POINT('Ctrl Pts',(-23.605835549348,3.6851845516463,1.76142008403567));
#92696=CARTESIAN_POINT('Ctrl Pts',(-23.408017555911,0.53185284980909,4.0497306624805));
#92697=CARTESIAN_POINT('Ctrl Pts',(-23.2101995624738,-3.10540650894146,
2.65323129533334));
#92698=CARTESIAN_POINT('Ctrl Pts',(-23.0123815690367,-3.91708714584599,
-1.1574170312224));
#92699=CARTESIAN_POINT('Ctrl Pts',(-22.8145635755996,-1.16464886337962,
-3.91494302862625));
#92700=CARTESIAN_POINT('Ctrl Pts',(-22.6167455821625,2.64749192093593,-3.11030101773335));
#92701=CARTESIAN_POINT('Ctrl Pts',(-22.4189275887254,4.0507059459073,0.524373180214398));
#92702=CARTESIAN_POINT('Ctrl Pts',(-22.2211095952883,1.76822262458715,3.68192539878807));
#92703=CARTESIAN_POINT('Ctrl Pts',(-22.0232916018512,-2.12314900462943,
3.48933004980607));
#92704=CARTESIAN_POINT('Ctrl Pts',(-21.8254736084141,-4.08268831704865,
0.121827739754767));
#92705=CARTESIAN_POINT('Ctrl Pts',(-21.627655614977,-2.32742983944607,-3.3565244278563));
#92706=CARTESIAN_POINT('Ctrl Pts',(-21.4298376215399,1.54553406962469,-3.78080815857784));
#92707=CARTESIAN_POINT('Ctrl Pts',(-21.2320196281028,4.01223178828592,-0.764971874912774));
#92708=CARTESIAN_POINT('Ctrl Pts',(-21.0342016346657,2.82823941680707,2.94690476492853));
#92709=CARTESIAN_POINT('Ctrl Pts',(-20.8363836412285,-0.929140075930861,
3.97742185487519));
#92710=CARTESIAN_POINT('Ctrl Pts',(-20.6385656477914,-3.84110418727031,
1.38892206940278));
#92711=CARTESIAN_POINT('Ctrl Pts',(-20.4407476543543,-3.25808552303732,
-2.46334419375657));
#92712=CARTESIAN_POINT('Ctrl Pts',(-20.2429296609172,0.289432990508367,
-4.07423789638565));
#92713=CARTESIAN_POINT('Ctrl Pts',(-20.0451116674801,3.57359928365308,-1.97802276332043));
#92714=CARTESIAN_POINT('Ctrl Pts',(-19.847293674043,3.60618287186699,1.9179757524517));
#92715=CARTESIAN_POINT('Ctrl Pts',(-19.6494756806059,0.357536269942257,
4.06882706784342));
#92716=CARTESIAN_POINT('Ctrl Pts',(-19.4516576871688,-3.21642905393536,
2.51749280700861));
#92717=CARTESIAN_POINT('Ctrl Pts',(-19.2538396937317,-3.86379733844877,
-1.32448330292826));
#92718=CARTESIAN_POINT('Ctrl Pts',(-19.0560217002946,-0.995534573189098,
-3.96132513256925));
#92719=CARTESIAN_POINT('Ctrl Pts',(-18.8582037068575,2.77855527099065,-2.99379633548938));
#92720=CARTESIAN_POINT('Ctrl Pts',(-18.6603857134204,4.02446510764256,0.697758188563256));
#92721=CARTESIAN_POINT('Ctrl Pts',(-18.4625677199833,1.60855387765517,3.75442942602735));
#92722=CARTESIAN_POINT('Ctrl Pts',(-18.2647497265462,-2.27096464385436,
3.39498239740695));
#92723=CARTESIAN_POINT('Ctrl Pts',(-18.066931733109,-4.0841548578661,-0.0535255948893623));
#92724=CARTESIAN_POINT('Ctrl Pts',(-17.869113739672,-2.18121289084575,-3.45333117687081));
#92725=CARTESIAN_POINT('Ctrl Pts',(-17.6712957462348,1.70639314975703,-3.71098481683796));
#92726=CARTESIAN_POINT('Ctrl Pts',(-17.4734777527977,4.04136891114997,-0.592050011679798));
#92727=CARTESIAN_POINT('Ctrl Pts',(-17.2756597593606,2.69914300198876,3.06558525361058));
#92728=CARTESIAN_POINT('Ctrl Pts',(-17.0778417659235,-1.09900647519767,
3.9338747641242));
#92729=CARTESIAN_POINT('Ctrl Pts',(-16.8800237724864,-3.89718081143694,
1.222770467139));
#92730=CARTESIAN_POINT('Ctrl Pts',(-16.6822057790493,-3.14934880543664,
-2.60092060510013));
#92731=CARTESIAN_POINT('Ctrl Pts',(-16.4843877856122,0.464044584123203,
-4.05805969846249));
#92732=CARTESIAN_POINT('Ctrl Pts',(-16.2865697921751,3.65520838824687,-1.8228103386884));
#92733=CARTESIAN_POINT('Ctrl Pts',(-16.088751798738,3.52053416892211,2.07099615108081));
#92734=CARTESIAN_POINT('Ctrl Pts',(-15.8909338053009,0.182560668631769,
4.08042369057531));
#92735=CARTESIAN_POINT('Ctrl Pts',(-15.6931158118638,-3.32152298156795,
2.37711400131663));
#92736=CARTESIAN_POINT('Ctrl Pts',(-15.4952978184266,-3.80338566527584,
-1.4891082477489));
#92737=CARTESIAN_POINT('Ctrl Pts',(-15.2974798249896,-0.824585284167319,
-4.0004056046199));
#92738=CARTESIAN_POINT('Ctrl Pts',(-15.0996618315524,2.90449710561624,-2.87177339910489));
#92739=CARTESIAN_POINT('Ctrl Pts',(-14.9018438381154,3.99080625600933,0.869857068337309));
#92740=CARTESIAN_POINT('Ctrl Pts',(-14.7040258446782,1.4459201965398,3.82001317767071));
#92741=CARTESIAN_POINT('Ctrl Pts',(-14.5062078512411,-2.41459437373826,
3.29437701282824));
#92742=CARTESIAN_POINT('Ctrl Pts',(-14.308389857804,-4.0780933633985,-0.228780269570442));
#92743=CARTESIAN_POINT('Ctrl Pts',(-14.1105718643669,-2.03097546599567,
-3.54377264350625));
#92744=CARTESIAN_POINT('Ctrl Pts',(-13.9127538709298,1.86410695545964,-3.6343212778931));
#92745=CARTESIAN_POINT('Ctrl Pts',(-13.7149358774927,4.06305686305413,-0.418036864317439));
#92746=CARTESIAN_POINT('Ctrl Pts',(-13.5171178840555,2.5650714467888,3.17861516469175));
#92747=CARTESIAN_POINT('Ctrl Pts',(-13.3192998906185,-1.26684715315575,
3.88307663881113));
#92748=CARTESIAN_POINT('Ctrl Pts',(-13.1214818971813,-3.94607403642267,
1.05436501810828));
#92749=CARTESIAN_POINT('Ctrl Pts',(-12.9236639037443,-3.03480711477366,
-2.7337029224952));
#92750=CARTESIAN_POINT('Ctrl Pts',(-12.7258459103071,0.637800837006619,
-4.03440156462557));
#92751=CARTESIAN_POINT('Ctrl Pts',(-12.52802791687,3.73008010440203,-1.66423805601355));
#92752=CARTESIAN_POINT('Ctrl Pts',(-12.3302099234329,3.42839631305133,2.22019922822156));
#92753=CARTESIAN_POINT('Ctrl Pts',(-12.1323919299958,0.00724856608596741,
4.08449915542031));
#92754=CARTESIAN_POINT('Ctrl Pts',(-11.9345739365587,-3.42049457959367,
2.23235362864174));
#92755=CARTESIAN_POINT('Ctrl Pts',(-11.7367559431216,-3.73596347891545,
-1.65098842411134));
#92756=CARTESIAN_POINT('Ctrl Pts',(-11.5389379496845,-0.65211609510973,
-4.03211241049135));
#92757=CARTESIAN_POINT('Ctrl Pts',(-11.3411199562474,3.02508528508984,-2.74445712487416));
#92758=CARTESIAN_POINT('Ctrl Pts',(-11.1433019628103,3.94979143200078,1.04035260178115));
#92759=CARTESIAN_POINT('Ctrl Pts',(-10.9454839693731,1.28062135246228,3.87855576780291));
#92760=CARTESIAN_POINT('Ctrl Pts',(-10.7476659759361,-2.55377345170589,
3.18769933489685));
#92761=CARTESIAN_POINT('Ctrl Pts',(-10.5498479824989,-4.06451500637211,
-0.40361324967779));
#92762=CARTESIAN_POINT('Ctrl Pts',(-10.3520299890619,-1.87699448697021,
-3.62768212337065));
#92763=CARTESIAN_POINT('Ctrl Pts',(-10.1542119956247,2.01838478397135,-3.55095885025052));
#92764=CARTESIAN_POINT('Ctrl Pts',(-9.95639400218765,4.07725566812261,-0.243253179016498));
#92765=CARTESIAN_POINT('Ctrl Pts',(-9.75857600875052,2.4262718758715,3.2857861580898));
#92766=CARTESIAN_POINT('Ctrl Pts',(-9.56075801531343,-1.43235274089283,
3.82512111154619));
#92767=CARTESIAN_POINT('Ctrl Pts',(-9.3629400218763,-3.98769374078607,0.884016132225644));
#92768=CARTESIAN_POINT('Ctrl Pts',(-9.16512202843922,-2.91467157768749,
-2.86144639763884));
#92769=CARTESIAN_POINT('Ctrl Pts',(-8.96730403500207,0.810381476483423,
-4.00330710224835));
#92770=CARTESIAN_POINT('Ctrl Pts',(-8.769486041565,3.79807642635226,-1.50259820042715));
#92771=CARTESIAN_POINT('Ctrl Pts',(-8.57166804812787,3.32993913548144,2.36530996834002));
#92772=CARTESIAN_POINT('Ctrl Pts',(-8.37385005469078,-0.168076897231722,
4.08104595036081));
#92773=CARTESIAN_POINT('Ctrl Pts',(-8.17603206125366,-3.51316142062967,
2.08347851559342));
#92774=CARTESIAN_POINT('Ctrl Pts',(-7.97821406781657,-3.66165505393974,
-1.80982544967654));
#92775=CARTESIAN_POINT('Ctrl Pts',(-7.78039607437944,-0.478444906337645,
-4.05638710725913));
#92776=CARTESIAN_POINT('Ctrl Pts',(-7.58257808094236,3.14009753770512,-2.6120821859277));
#92777=CARTESIAN_POINT('Ctrl Pts',(-7.38476008750522,3.9014962353557,1.20893052647464));
#92778=CARTESIAN_POINT('Ctrl Pts',(-7.18694209406814,1.11296202915234,3.9299492889857));
#92779=CARTESIAN_POINT('Ctrl Pts',(-6.98912410063102,-2.68824533875734,
3.07514599507246));
#92780=CARTESIAN_POINT('Ctrl Pts',(-6.79130610719391,-4.04344481481362,
-0.577702277884071));
#92781=CARTESIAN_POINT('Ctrl Pts',(-6.5934881137568,-1.71955377608047,-3.70490495201694));
#92782=CARTESIAN_POINT('Ctrl Pts',(-6.3956701203197,2.16894226583871,-3.46105119002063));
#92783=CARTESIAN_POINT('Ctrl Pts',(-6.19785212688258,4.08393915467268,-0.0680211222212914));
#92784=CARTESIAN_POINT('Ctrl Pts',(-6.00003413344548,2.28300012876661,3.38690069300563));
#92785=CARTESIAN_POINT('Ctrl Pts',(-5.80221614000837,-1.59521817369359,
3.76011500776615));
#92786=CARTESIAN_POINT('Ctrl Pts',(-5.60439814657127,-4.02196320968319,
0.712037801432078));
#92787=CARTESIAN_POINT('Ctrl Pts',(-5.40658015313415,-2.78916363188875,
-2.98391556963731));
#92788=CARTESIAN_POINT('Ctrl Pts',(-5.20876215969706,0.981468397431387,
-3.9648336262051));
#92789=CARTESIAN_POINT('Ctrl Pts',(-5.01094416625994,3.85907202005989,-1.33818871007757));
#92790=CARTESIAN_POINT('Ctrl Pts',(-4.81312617282284,3.22534411770083,2.50606089667497));
#92791=CARTESIAN_POINT('Ctrl Pts',(-4.61530817938572,-0.343092560634735,
4.07007044493406));
#92792=CARTESIAN_POINT('Ctrl Pts',(-4.41749018594862,-3.59935268997692,
1.93076306460202));
#92793=CARTESIAN_POINT('Ctrl Pts',(-4.21967219251151,-3.58059737398049,
-1.9653265348854));
#92794=CARTESIAN_POINT('Ctrl Pts',(-4.0218541990744,-0.303891802834324,
-4.07318498256667));
#92795=CARTESIAN_POINT('Ctrl Pts',(-3.8240362056373,3.24932181031572,-2.47489251940337));
#92796=CARTESIAN_POINT('Ctrl Pts',(-3.62621821220018,3.84600979845569,1.37527999920385));
#92797=CARTESIAN_POINT('Ctrl Pts',(-3.42840021876308,0.943251044449692,
3.9740992320543));
#92798=CARTESIAN_POINT('Ctrl Pts',(-3.23058222532597,-2.8177617572936,2.95692403212172));
#92799=CARTESIAN_POINT('Ctrl Pts',(-3.03276423188887,-4.01492242046153,
-0.750725658560183));
#92800=CARTESIAN_POINT('Ctrl Pts',(-2.83494623845176,-1.55894201164752,
-3.77530033988628));
#92801=CARTESIAN_POINT('Ctrl Pts',(-2.63712824501465,2.31549897712062,-3.36476105063503));
#92802=CARTESIAN_POINT('Ctrl Pts',(-2.43931025157754,4.08310057810657,0.107330633052476));
#92803=CARTESIAN_POINT('Ctrl Pts',(-2.24149225814044,2.13550961617047,3.4817832661206));
#92804=CARTESIAN_POINT('Ctrl Pts',(-2.04367426470333,-1.75512282259002,
3.68815733144775));
#92805=CARTESIAN_POINT('Ctrl Pts',(-1.84585627126622,-4.04885838900248,
0.538786873855875));
#92806=CARTESIAN_POINT('Ctrl Pts',(-1.64803827782911,-2.65843974009147,
-3.10096099417392));
#92807=CARTESIAN_POINT('Ctrl Pts',(-1.45022028439201,1.15060289862765,-3.91890598795134));
#92808=CARTESIAN_POINT('Ctrl Pts',(-1.25240229095489,3.91322891566222,-1.17159230533783));
#92809=CARTESIAN_POINT('Ctrl Pts',(-1.05458429751779,3.11427834079904,2.64272844505947));
#92810=CARTESIAN_POINT('Ctrl Pts',(-0.856766304080684,-0.516466827795134,
4.05056289950572));
#92811=CARTESIAN_POINT('Ctrl Pts',(-0.658948310643573,-3.68086436566828,
1.77649746246159));
#92812=CARTESIAN_POINT('Ctrl Pts',(-0.461130317206468,-3.48898854935592,
-2.12138128548535));
#92813=CARTESIAN_POINT('Ctrl Pts',(-0.329251654915064,-1.25514472459608,
-3.42162814095714));
#92814=CARTESIAN_POINT('Ctrl Pts',(-0.263312323769361,-0.109073086534847,
-3.45778011327987));
#92815=CARTESIAN_POINT('Ctrl Pts',(-29.4036876762306,-1.64343044862514,
3.31080057131682));
#92816=CARTESIAN_POINT('Ctrl Pts',(-29.3377483450849,-2.74078612473952,
2.76609010257943));
#92817=CARTESIAN_POINT('Ctrl Pts',(-29.2058696827936,-4.33286715317278,
0.509621633320206));
#92818=CARTESIAN_POINT('Ctrl Pts',(-29.0080516893564,-2.786129234649,-3.36255669633147));
#92819=CARTESIAN_POINT('Ctrl Pts',(-28.8102336959193,1.29928094542948,-4.1648396900737));
#92820=CARTESIAN_POINT('Ctrl Pts',(-28.6124157024822,4.20064038344374,-1.18273102193916));
#92821=CARTESIAN_POINT('Ctrl Pts',(-28.4145977090451,3.28084020858381,2.87819824635538));
#92822=CARTESIAN_POINT('Ctrl Pts',(-28.216779715608,-0.624665972610546,
4.31889413964144));
#92823=CARTESIAN_POINT('Ctrl Pts',(-28.0189617221709,-3.96153263057873,
1.8305962208402));
#92824=CARTESIAN_POINT('Ctrl Pts',(-27.8211437287337,-3.69397677764492,
-2.32372196509937));
#92825=CARTESIAN_POINT('Ctrl Pts',(-27.6233257352967,-0.0652364080480912,
-4.36351059266543));
#92826=CARTESIAN_POINT('Ctrl Pts',(-27.4255077418595,3.62282456707754,-2.43308738034599));
#92827=CARTESIAN_POINT('Ctrl Pts',(-27.2276897484225,4.01453275210466,1.71123201057149));
#92828=CARTESIAN_POINT('Ctrl Pts',(-27.0298717549853,0.75344702936726,4.29849008658198));
#92829=CARTESIAN_POINT('Ctrl Pts',(-26.8320537615483,-3.19318738180644,
2.97460920569266));
#92830=CARTESIAN_POINT('Ctrl Pts',(-26.6342357681111,-4.23437490293385,
-1.05584691784211));
#92831=CARTESIAN_POINT('Ctrl Pts',(-26.436417774674,-1.42274505435184,-4.12559433567772));
#92832=CARTESIAN_POINT('Ctrl Pts',(-26.2385997812369,2.68342571307752,-3.44150630056508));
#92833=CARTESIAN_POINT('Ctrl Pts',(-26.0407817877998,4.34797431489627,0.373975435205314));
#92834=CARTESIAN_POINT('Ctrl Pts',(-25.8429637943627,2.05634380943297,3.84918004191613));
#92835=CARTESIAN_POINT('Ctrl Pts',(-25.6451458009256,-2.10633351714236,
3.822054031928));
#92836=CARTESIAN_POINT('Ctrl Pts',(-25.4473278074885,-4.35247882946084,
0.31727863829441));
#92837=CARTESIAN_POINT('Ctrl Pts',(-25.2495098140514,-2.63834659872647,
-3.47618537407148));
#92838=CARTESIAN_POINT('Ctrl Pts',(-25.0516918206143,1.47639113755023,-4.10670267869265));
#92839=CARTESIAN_POINT('Ctrl Pts',(-24.8538738271771,4.24777516269504,-1.00057174045179));
#92840=CARTESIAN_POINT('Ctrl Pts',(-24.6560558337401,3.15415050271192,3.01596953382905));
#92841=CARTESIAN_POINT('Ctrl Pts',(-24.4582378403029,-0.809404555575561,
4.28830991297042));
#92842=CARTESIAN_POINT('Ctrl Pts',(-24.2604198468659,-4.03649040139732,
1.65875943895133));
#92843=CARTESIAN_POINT('Ctrl Pts',(-24.0626018534287,-3.59081348392226,
-2.48007986945916));
#92844=CARTESIAN_POINT('Ctrl Pts',(-23.8647838599917,0.122109169034145,
-4.36231899212071));
#92845=CARTESIAN_POINT('Ctrl Pts',(-23.6669658665545,3.72392589487205,-2.27532713394089));
#92846=CARTESIAN_POINT('Ctrl Pts',(-23.4691478731174,3.93737921636729,1.88196241815778));
#92847=CARTESIAN_POINT('Ctrl Pts',(-23.2713298796803,0.568250063912948,
4.32687294730266));
#92848=CARTESIAN_POINT('Ctrl Pts',(-23.0735118862432,-3.31792421120822,
2.83480450220432));
#92849=CARTESIAN_POINT('Ctrl Pts',(-22.8756938928061,-4.18515200544392,
-1.23662457050318));
#92850=CARTESIAN_POINT('Ctrl Pts',(-22.6778758993689,-1.24435131124929,
-4.1828611561092));
#92851=CARTESIAN_POINT('Ctrl Pts',(-22.4800579059319,2.82867235518411,-3.32315367446072));
#92852=CARTESIAN_POINT('Ctrl Pts',(-22.2822399124947,4.32791497400198,0.560258525037564));
#92853=CARTESIAN_POINT('Ctrl Pts',(-22.0844219190577,1.88923048883661,3.9338970242146));
#92854=CARTESIAN_POINT('Ctrl Pts',(-21.8866039256205,-2.26844616515726,
3.72812146165506));
#92855=CARTESIAN_POINT('Ctrl Pts',(-21.6887859321835,-4.36208605055386,
0.13016499004728));
#92856=CARTESIAN_POINT('Ctrl Pts',(-21.4909679387463,-2.48670690679362,
-3.58622732084516));
#92857=CARTESIAN_POINT('Ctrl Pts',(-21.2931499453092,1.65130229942196,-4.03954680044611));
#92858=CARTESIAN_POINT('Ctrl Pts',(-21.0953319518721,4.28680784721833,-0.817322530032182));
#92859=CARTESIAN_POINT('Ctrl Pts',(-20.897513958435,3.02178925982747,3.14857544077672));
#92860=CARTESIAN_POINT('Ctrl Pts',(-20.6996959649979,-0.992725540008512,
4.24961570489448));
#92861=CARTESIAN_POINT('Ctrl Pts',(-20.5018779715608,-4.10396917248096,
1.48397259691575));
#92862=CARTESIAN_POINT('Ctrl Pts',(-20.3040599781237,-3.48105177468615,
-2.63192252527032));
#92863=CARTESIAN_POINT('Ctrl Pts',(-20.1062419846866,0.309240263380999,
-4.35305732750844));
#92864=CARTESIAN_POINT('Ctrl Pts',(-19.9084239912495,3.81815763902375,-2.1133882465452));
#92865=CARTESIAN_POINT('Ctrl Pts',(-19.7106059978124,3.8529710767852,2.04923193380534));
#92866=CARTESIAN_POINT('Ctrl Pts',(-19.5127880043752,0.382004173370155,
4.34727621029521));
#92867=CARTESIAN_POINT('Ctrl Pts',(-19.3149700109382,-3.43654455574752,
2.68977678505725));
#92868=CARTESIAN_POINT('Ctrl Pts',(-19.117152017501,-4.12821532367142,-1.41512397989553));
#92869=CARTESIAN_POINT('Ctrl Pts',(-18.9193340240639,-1.06366372774973,
-4.23241740750371));
#92870=CARTESIAN_POINT('Ctrl Pts',(-18.7215160306268,2.96870499216626,-3.19867602400712));
#92871=CARTESIAN_POINT('Ctrl Pts',(-18.5236980371897,4.2998783506645,0.745509092203192));
#92872=CARTESIAN_POINT('Ctrl Pts',(-18.3258800437526,1.71863485193899,4.01136284606261));
#92873=CARTESIAN_POINT('Ctrl Pts',(-18.1280620503155,-2.42637752994556,
3.62731715173159));
#92874=CARTESIAN_POINT('Ctrl Pts',(-17.9302440568784,-4.36365295371805,
-0.0571886053215215));
#92875=CARTESIAN_POINT('Ctrl Pts',(-17.7324260634413,-2.330483638615,-3.6896590150336));
#92876=CARTESIAN_POINT('Ctrl Pts',(-17.5346080700042,1.82316972966886,-3.96494511612583));
#92877=CARTESIAN_POINT('Ctrl Pts',(-17.3367900765671,4.31793896165287,-0.63256680320031));
#92878=CARTESIAN_POINT('Ctrl Pts',(-17.13897208313,2.88385816479288,3.27537779842697));
#92879=CARTESIAN_POINT('Ctrl Pts',(-16.9411540896929,-1.17421670297713,
4.20308848009656));
#92880=CARTESIAN_POINT('Ctrl Pts',(-16.7433360962557,-4.16388338611759,
1.30645045213544));
#92881=CARTESIAN_POINT('Ctrl Pts',(-16.5455181028187,-3.36487368755462,
-2.77891394322918));
#92882=CARTESIAN_POINT('Ctrl Pts',(-16.3477001093815,0.495801356862377,
-4.33577197873739));
#92883=CARTESIAN_POINT('Ctrl Pts',(-16.1498821159444,3.90535164187237,-1.94755389922735));
#92884=CARTESIAN_POINT('Ctrl Pts',(-15.9520641225073,3.7614610267028,2.21272424437995));
#92885=CARTESIAN_POINT('Ctrl Pts',(-15.7542461290702,0.19505416141933,4.35966644494551));
#92886=CARTESIAN_POINT('Ctrl Pts',(-15.5564281356331,-3.54883055950875,
2.53979119160763));
#92887=CARTESIAN_POINT('Ctrl Pts',(-15.358610142196,-4.0636693930556,-1.59101499082003));
#92888=CARTESIAN_POINT('Ctrl Pts',(-15.1607921487589,-0.881015567742002,
-4.27417234168993));
#92889=CARTESIAN_POINT('Ctrl Pts',(-14.9629741553218,3.10326562411736,-3.06830247909855));
#92890=CARTESIAN_POINT('Ctrl Pts',(-14.7651561618847,4.26391606410594,0.929385514913071));
#92891=CARTESIAN_POINT('Ctrl Pts',(-14.5673381684476,1.54487137634347,4.08143480501962));
#92892=CARTESIAN_POINT('Ctrl Pts',(-14.3695201750105,-2.57983652375489,
3.51982686332313));
#92893=CARTESIAN_POINT('Ctrl Pts',(-14.1717021815733,-4.3571766424228,-0.244436788957864));
#92894=CARTESIAN_POINT('Ctrl Pts',(-13.9738841881363,-2.16996475392007,
-3.7862898203671));
#92895=CARTESIAN_POINT('Ctrl Pts',(-13.7760661946991,1.99167663943278,-3.88303512744974));
#92896=CARTESIAN_POINT('Ctrl Pts',(-13.578248201262,4.3411111230131,-0.446645110488031));
#92897=CARTESIAN_POINT('Ctrl Pts',(-13.3804302078249,2.74061145691375,3.39614288263965));
#92898=CARTESIAN_POINT('Ctrl Pts',(-13.1826122143878,-1.35354351491601,
4.14881399803603));
#92899=CARTESIAN_POINT('Ctrl Pts',(-12.9847942209507,-4.21612260648281,
1.12652021915962));
#92900=CARTESIAN_POINT('Ctrl Pts',(-12.7869762275136,-3.24249336551008,
-2.92078318464312));
#92901=CARTESIAN_POINT('Ctrl Pts',(-12.5891582340765,0.681448574587572,
-4.3104948065464));
#92902=CARTESIAN_POINT('Ctrl Pts',(-12.3913402406394,3.98534718482324,-1.77812976283858));
#92903=CARTESIAN_POINT('Ctrl Pts',(-12.1935222472022,3.66301774016938,2.37213799604391));
#92904=CARTESIAN_POINT('Ctrl Pts',(-11.9957042537652,0.0077446198569954,
4.36402081318755));
#92905=CARTESIAN_POINT('Ctrl Pts',(-11.797886260328,-3.65457525359824,2.38512417975633));
#92906=CARTESIAN_POINT('Ctrl Pts',(-11.600068266891,-3.99163318657067,-1.76397339575705));
#92907=CARTESIAN_POINT('Ctrl Pts',(-11.4022502734539,-0.696743493727229,
-4.30804899473296));
#92908=CARTESIAN_POINT('Ctrl Pts',(-11.2044322800167,3.23210622489183,-2.93227334811854));
#92909=CARTESIAN_POINT('Ctrl Pts',(-11.0066142865797,4.22009440107903,1.11154886669564));
#92910=CARTESIAN_POINT('Ctrl Pts',(-10.8087962931425,1.36826034803836,4.14398374237361));
#92911=CARTESIAN_POINT('Ctrl Pts',(-10.6109782997055,-2.72854028641939,
3.40584872571541));
#92912=CARTESIAN_POINT('Ctrl Pts',(-10.4131603062683,-4.34266905399709,
-0.431234419459898));
#92913=CARTESIAN_POINT('Ctrl Pts',(-10.2153423128312,-2.00544612587474,
-3.87594162408116));
#92914=CARTESIAN_POINT('Ctrl Pts',(-10.0175243193941,2.15651243178323,-3.79396781333675));
#92915=CARTESIAN_POINT('Ctrl Pts',(-9.81970632595701,4.35628161968441,-0.259900148269901));
#92916=CARTESIAN_POINT('Ctrl Pts',(-9.62188833251987,2.59231317276776,3.51064809563215));
#92917=CARTESIAN_POINT('Ctrl Pts',(-9.42407033908278,-1.53037543533029,
4.08689229904686));
#92918=CARTESIAN_POINT('Ctrl Pts',(-9.22625234564566,-4.26059054469735,
0.944513550726706));
#92919=CARTESIAN_POINT('Ctrl Pts',(-9.02843435220857,-3.11413638358937,
-3.05726875192153));
#92920=CARTESIAN_POINT('Ctrl Pts',(-8.83061635877144,0.865839726102576,
-4.27727240256842));
#92921=CARTESIAN_POINT('Ctrl Pts',(-8.63279836533435,4.05799681772063,-1.6054281249686));
#92922=CARTESIAN_POINT('Ctrl Pts',(-8.43498037189723,3.5578226707684,2.52717935264541));
#92923=CARTESIAN_POINT('Ctrl Pts',(-8.23716237846013,-0.179579196818253,
4.36033128892069));
#92924=CARTESIAN_POINT('Ctrl Pts',(-8.03934438502301,-3.75358372626171,
2.2260608363238));
#92925=CARTESIAN_POINT('Ctrl Pts',(-7.84152639158592,-3.91223948348743,
-1.93368039264833));
#92926=CARTESIAN_POINT('Ctrl Pts',(-7.64370839814879,-0.511187161454119,
-4.33398492418169));
#92927=CARTESIAN_POINT('Ctrl Pts',(-7.44589040471171,3.35498931167584,-2.79083936399343));
#92928=CARTESIAN_POINT('Ctrl Pts',(-7.24807241127459,4.16849413497138,1.2916633786622));
#92929=CARTESIAN_POINT('Ctrl Pts',(-7.05025441783749,1.1891273017067,4.19889436606833));
#92930=CARTESIAN_POINT('Ctrl Pts',(-6.85243642440037,-2.87221472275815,
3.2855928267919));
#92931=CARTESIAN_POINT('Ctrl Pts',(-6.65461843096327,-4.32015692925418,
-0.617237185902298));
#92932=CARTESIAN_POINT('Ctrl Pts',(-6.45680043752616,-1.83723100009755,
-3.95844917730672));
#92933=CARTESIAN_POINT('Ctrl Pts',(-6.25898244408905,2.31737327651579,-3.697907345314));
#92934=CARTESIAN_POINT('Ctrl Pts',(-6.06116445065195,4.3634224889316,-0.0726761303686811));
#92935=CARTESIAN_POINT('Ctrl Pts',(-5.86334645721483,2.4392366601976,3.61868237795117));
#92936=CARTESIAN_POINT('Ctrl Pts',(-5.66552846377773,-1.70438652247867,
4.01743751913734));
#92937=CARTESIAN_POINT('Ctrl Pts',(-5.46771047034062,-4.29720523595649,
0.76076592673604));
#92938=CARTESIAN_POINT('Ctrl Pts',(-5.26989247690351,-2.9800393335363,-3.18811907046449));
#92939=CARTESIAN_POINT('Ctrl Pts',(-5.07207448346641,1.04863493684225,-4.23616600400653));
#92940=CARTESIAN_POINT('Ctrl Pts',(-4.8742564900293,4.123166629324,-1.42976731308693));
#92941=CARTESIAN_POINT('Ctrl Pts',(-4.67643849659219,3.44606971962761,2.67756253485615));
#92942=CARTESIAN_POINT('Ctrl Pts',(-4.47862050315508,-0.366572012500694,
4.34860467757986));
#92943=CARTESIAN_POINT('Ctrl Pts',(-4.28080250971799,-3.84567347313981,
2.0628943424007));
#92944=CARTESIAN_POINT('Ctrl Pts',(-4.08298451628086,-3.82563464187755,
-2.09982315495596));
#92945=CARTESIAN_POINT('Ctrl Pts',(-3.88516652284376,-0.324688560840112,
-4.35193235780086));
#92946=CARTESIAN_POINT('Ctrl Pts',(-3.68734852940666,3.47168831952001,-2.64426115763686));
#92947=CARTESIAN_POINT('Ctrl Pts',(-3.48953053596954,4.10921049791642,1.46939693512277));
#92948=CARTESIAN_POINT('Ctrl Pts',(-3.29171254253244,1.0078021890583,4.24606569922841));
#92949=CARTESIAN_POINT('Ctrl Pts',(-3.09389454909533,-3.01059456435799,
3.15928037396442));
#92950=CARTESIAN_POINT('Ctrl Pts',(-2.89607655565822,-4.28968261212052,
-0.80210137749764));
#92951=CARTESIAN_POINT('Ctrl Pts',(-2.69825856222111,-1.66562781053683,
-4.0336620555874));
#92952=CARTESIAN_POINT('Ctrl Pts',(-2.50044056878401,2.47395955894843,-3.59502761480265));
#92953=CARTESIAN_POINT('Ctrl Pts',(-2.30262257534689,4.36252652459211,0.114675777545951));
#92954=CARTESIAN_POINT('Ctrl Pts',(-2.10480458190979,2.28165267199598,3.72005821575322));
#92955=CARTESIAN_POINT('Ctrl Pts',(-1.90698658847269,-1.87523420523149,
3.94055543759611));
#92956=CARTESIAN_POINT('Ctrl Pts',(-1.70916859503558,-4.32594098001169,
0.575658616126547));
#92957=CARTESIAN_POINT('Ctrl Pts',(-1.51135060159847,-2.84036938555083,
-3.3131744687716));
#92958=CARTESIAN_POINT('Ctrl Pts',(-1.31353260816137,1.22934411448257,-4.18709531954478));
#92959=CARTESIAN_POINT('Ctrl Pts',(-1.11571461472425,4.18102973826174,-1.25176992588667));
#92960=CARTESIAN_POINT('Ctrl Pts',(-0.917896621287149,3.32740318461583,
2.82358289205118));
#92961=CARTESIAN_POINT('Ctrl Pts',(-0.720078627850039,-0.55181110340736,
4.32776213825641));
#92962=CARTESIAN_POINT('Ctrl Pts',(-0.52226063441293,-3.93276337956392,
1.89807161313012));
#92963=CARTESIAN_POINT('Ctrl Pts',(-0.324442640975823,-3.72775659070872,
-2.26655747260449));
#92964=CARTESIAN_POINT('Ctrl Pts',(-0.192563978684421,-1.34104023364309,
-3.65578638994445));
#92965=CARTESIAN_POINT('Ctrl Pts',(-0.126624647538717,-0.116537475387898,
-3.69441241327091));
#92966=CARTESIAN_POINT('Ctrl Pts',(-29.267,-1.74869447533113,3.52286199445087));
#92967=CARTESIAN_POINT('Ctrl Pts',(-29.2010606688543,-2.91633732258384,
2.94326205571725));
#92968=CARTESIAN_POINT('Ctrl Pts',(-29.0691820065629,-4.61039337529348,
0.542263614162568));
#92969=CARTESIAN_POINT('Ctrl Pts',(-28.8713640131258,-2.96458472231979,
-3.57793317190983));
#92970=CARTESIAN_POINT('Ctrl Pts',(-28.6735460196887,1.38250171345935,-4.43160351736486));
#92971=CARTESIAN_POINT('Ctrl Pts',(-28.4757280262516,4.46969729538972,-1.25848660379756));
#92972=CARTESIAN_POINT('Ctrl Pts',(-28.2779100328145,3.49098262843696,3.06255088344016));
#92973=CARTESIAN_POINT('Ctrl Pts',(-28.0800920393773,-0.66467670484336,
4.59552537063505));
#92974=CARTESIAN_POINT('Ctrl Pts',(-27.8822740459403,-4.21527435537805,
1.94784847793426));
#92975=CARTESIAN_POINT('Ctrl Pts',(-27.6844560525031,-3.93058117456272,
-2.47255961819028));
#92976=CARTESIAN_POINT('Ctrl Pts',(-27.486638059066,-0.069414891539576,
-4.64299957009216));
#92977=CARTESIAN_POINT('Ctrl Pts',(-27.2888200656289,3.85487156504997,-2.58893004177228));
#92978=CARTESIAN_POINT('Ctrl Pts',(-27.0910020721918,4.27166920907071,1.8208388224762));
#92979=CARTESIAN_POINT('Ctrl Pts',(-26.8931840787547,0.801706369023046,
4.57381440934107));
#92980=CARTESIAN_POINT('Ctrl Pts',(-26.6953660853176,-3.39771551508819,
3.16513710003091));
#92981=CARTESIAN_POINT('Ctrl Pts',(-26.4975480918805,-4.50559255819786,
-1.12347539475766));
#92982=CARTESIAN_POINT('Ctrl Pts',(-26.2997300984434,-1.51387387183383,
-4.38984444294094));
#92983=CARTESIAN_POINT('Ctrl Pts',(-26.1019121050063,2.85530289605246,-3.66193960909637));
#92984=CARTESIAN_POINT('Ctrl Pts',(-25.9040941115692,4.62646817192751,0.39792908668583));
#92985=CARTESIAN_POINT('Ctrl Pts',(-25.7062761181321,2.18805551640172,4.09572542573043));
#92986=CARTESIAN_POINT('Ctrl Pts',(-25.5084581246949,-2.24124713504792,
4.06686195673259));
#92987=CARTESIAN_POINT('Ctrl Pts',(-25.3106401312579,-4.63126120697179,
0.337600780361695));
#92988=CARTESIAN_POINT('Ctrl Pts',(-25.1128221378207,-2.80733640116096,
-3.69883992593119));
#92989=CARTESIAN_POINT('Ctrl Pts',(-24.9150041443836,1.57095606195064,-4.3697427488125));
#92990=CARTESIAN_POINT('Ctrl Pts',(-24.7171861509466,4.51985112340335,-1.06465976467958));
#92991=CARTESIAN_POINT('Ctrl Pts',(-24.5193681575094,3.35617826910138,3.20914661523155));
#92992=CARTESIAN_POINT('Ctrl Pts',(-24.3215501640723,-0.861248053318545,
4.56298218132233));
#92993=CARTESIAN_POINT('Ctrl Pts',(-24.1237321706352,-4.29503327661702,
1.76500530900118));
#92994=CARTESIAN_POINT('Ctrl Pts',(-23.9259141771981,-3.82081012709267,
-2.63893246576473));
#92995=CARTESIAN_POINT('Ctrl Pts',(-23.7280961837609,0.129930432684828,
-4.6417316458602));
#92996=CARTESIAN_POINT('Ctrl Pts',(-23.5302781903239,3.96244857478032,-2.4210650301764));
#92997=CARTESIAN_POINT('Ctrl Pts',(-23.3324601968868,4.18957388108829,2.00250475227989));
#92998=CARTESIAN_POINT('Ctrl Pts',(-23.1346422034497,0.604647278016807,
4.60401523212482));
#92999=CARTESIAN_POINT('Ctrl Pts',(-22.9368242100126,-3.53044191347499,
3.01637770907531));
#93000=CARTESIAN_POINT('Ctrl Pts',(-22.7390062165754,-4.45321686504185,
-1.31583210978398));
#93001=CARTESIAN_POINT('Ctrl Pts',(-22.5411882231384,-1.32405375911896,
-4.45077928359215));
#93002=CARTESIAN_POINT('Ctrl Pts',(-22.3433702297012,3.00985278943228,-3.53600633118811));
#93003=CARTESIAN_POINT('Ctrl Pts',(-22.1455522362642,4.60512400209667,0.596143869860738));
#93004=CARTESIAN_POINT('Ctrl Pts',(-21.947734242827,2.01023835308607,4.18586864964113));
#93005=CARTESIAN_POINT('Ctrl Pts',(-21.7499162493899,-2.41374332568508,
3.96691287350406));
#93006=CARTESIAN_POINT('Ctrl Pts',(-21.5520982559528,-4.64148378405907,
0.138502240339789));
#93007=CARTESIAN_POINT('Ctrl Pts',(-21.3542802625157,-2.64598397414117,
-3.81593021383402));
#93008=CARTESIAN_POINT('Ctrl Pts',(-21.1564622690786,1.75707052921922,-4.29828544231439));
#93009=CARTESIAN_POINT('Ctrl Pts',(-20.9586442756415,4.56138390615074,-0.869673185151591));
#93010=CARTESIAN_POINT('Ctrl Pts',(-20.7608262822044,3.21533910284787,3.35024611662491));
#93011=CARTESIAN_POINT('Ctrl Pts',(-20.5630082887673,-1.05631100408616,
4.52180955491376));
#93012=CARTESIAN_POINT('Ctrl Pts',(-20.3651902953302,-4.36683415769162,
1.57902312442871));
#93013=CARTESIAN_POINT('Ctrl Pts',(-20.167372301893,-3.70401802633496,-2.80050085678409));
#93014=CARTESIAN_POINT('Ctrl Pts',(-19.9695543084559,0.329047536253623,
-4.63187675863124));
#93015=CARTESIAN_POINT('Ctrl Pts',(-19.7717363150188,4.06271599439444,-2.24875372976998));
#93016=CARTESIAN_POINT('Ctrl Pts',(-19.5739183215817,4.0997592817034,2.18048811515899));
#93017=CARTESIAN_POINT('Ctrl Pts',(-19.3761003281446,0.406472076798061,
4.62572535274699));
#93018=CARTESIAN_POINT('Ctrl Pts',(-19.1782823347075,-3.65666005755969,
2.8620607631059));
#93019=CARTESIAN_POINT('Ctrl Pts',(-18.9804643412704,-4.39263330889407,
-1.5057646568628));
#93020=CARTESIAN_POINT('Ctrl Pts',(-18.7826463478333,-1.13179288231037,
-4.50350968243817));
#93021=CARTESIAN_POINT('Ctrl Pts',(-18.5848283543962,3.15885471334188,-3.40355571252486));
#93022=CARTESIAN_POINT('Ctrl Pts',(-18.3870103609591,4.57529159368643,0.793259995843121));
#93023=CARTESIAN_POINT('Ctrl Pts',(-18.189192367522,1.82871582622281,4.26829626609787));
#93024=CARTESIAN_POINT('Ctrl Pts',(-17.9913743740849,-2.58179041603676,
3.85965190605623));
#93025=CARTESIAN_POINT('Ctrl Pts',(-17.7935563806477,-4.64315104957,-0.0608516157536774));
#93026=CARTESIAN_POINT('Ctrl Pts',(-17.5957383872107,-2.47975438638425,
-3.92598685319639));
#93027=CARTESIAN_POINT('Ctrl Pts',(-17.3979203937735,1.93994630958068,-4.2189054154137));
#93028=CARTESIAN_POINT('Ctrl Pts',(-17.2001024003365,4.59450901215576,-0.673083594720819));
#93029=CARTESIAN_POINT('Ctrl Pts',(-17.0022844068993,3.06857332759699,3.48517034324336));
#93030=CARTESIAN_POINT('Ctrl Pts',(-16.8044664134622,-1.24942693075659,
4.47230219606893));
#93031=CARTESIAN_POINT('Ctrl Pts',(-16.6066484200251,-4.43058596079823,
1.39013043713188));
#93032=CARTESIAN_POINT('Ctrl Pts',(-16.408830426588,-3.58039856967259,-2.95690728135824));
#93033=CARTESIAN_POINT('Ctrl Pts',(-16.2110124331509,0.527558129601547,
-4.61348425901228));
#93034=CARTESIAN_POINT('Ctrl Pts',(-16.0131944397138,4.15549489549788,-2.07229745976629));
#93035=CARTESIAN_POINT('Ctrl Pts',(-15.8153764462767,4.00238788448349,2.35445233767909));
#93036=CARTESIAN_POINT('Ctrl Pts',(-15.6175584528395,0.207547654206896,
4.63890919931572));
#93037=CARTESIAN_POINT('Ctrl Pts',(-15.4197404594025,-3.77613813744956,
2.70246838189863));
#93038=CARTESIAN_POINT('Ctrl Pts',(-15.2219224659653,-4.32395312083535,
-1.69292173389115));
#93039=CARTESIAN_POINT('Ctrl Pts',(-15.0241044725283,-0.937445851316686,
-4.54793907875995));
#93040=CARTESIAN_POINT('Ctrl Pts',(-14.8262864790911,3.30203414261849,-3.26483155909222));
#93041=CARTESIAN_POINT('Ctrl Pts',(-14.6284684856541,4.53702587220254,0.988913961488839));
#93042=CARTESIAN_POINT('Ctrl Pts',(-14.4306504922169,1.64382255614715,4.34285643236852));
#93043=CARTESIAN_POINT('Ctrl Pts',(-14.2328324987798,-2.74507867377152,
3.74527671381803));
#93044=CARTESIAN_POINT('Ctrl Pts',(-14.0350145053427,-4.63625992144711,
-0.260093308345293));
#93045=CARTESIAN_POINT('Ctrl Pts',(-13.8371965119056,-2.30895404184448,
-4.02880699722795));
#93046=CARTESIAN_POINT('Ctrl Pts',(-13.6393785184685,2.11924632340592,-4.13174897700638));
#93047=CARTESIAN_POINT('Ctrl Pts',(-13.4415605250314,4.61916538297207,-0.475253356658625));
#93048=CARTESIAN_POINT('Ctrl Pts',(-13.2437425315943,2.9161514670387,3.61367060058756));
#93049=CARTESIAN_POINT('Ctrl Pts',(-13.0459245381572,-1.44023987667628,
4.41455135726092));
#93050=CARTESIAN_POINT('Ctrl Pts',(-12.8481065447201,-4.48617117654295,
1.19867542021098));
#93051=CARTESIAN_POINT('Ctrl Pts',(-12.650288551283,-3.45017961624651,-3.10786344679104));
#93052=CARTESIAN_POINT('Ctrl Pts',(-12.4524705578459,0.72509631216853,-4.58658804846722));
#93053=CARTESIAN_POINT('Ctrl Pts',(-12.2546525644087,4.24061426524445,-1.89202146966362));
#93054=CARTESIAN_POINT('Ctrl Pts',(-12.0568345709716,3.89763916728744,2.52407676386627));
#93055=CARTESIAN_POINT('Ctrl Pts',(-11.8590165775345,0.00824067362801503,
4.64354247095479));
#93056=CARTESIAN_POINT('Ctrl Pts',(-11.6611985840974,-3.88865592760281,
2.53789473087093));
#93057=CARTESIAN_POINT('Ctrl Pts',(-11.4633805906603,-4.24730289422589,
-1.87695836740277));
#93058=CARTESIAN_POINT('Ctrl Pts',(-11.2655625972232,-0.741370892344723,
-4.58398557897456));
#93059=CARTESIAN_POINT('Ctrl Pts',(-11.0677446037861,3.43912716469383,-3.12008957136294));
#93060=CARTESIAN_POINT('Ctrl Pts',(-10.869926610349,4.49039737015727,1.18274513161014));
#93061=CARTESIAN_POINT('Ctrl Pts',(-10.6721086169119,1.45589934361444,4.40941171694431));
#93062=CARTESIAN_POINT('Ctrl Pts',(-10.4742906234748,-2.90330712113289,
3.62399811653398));
#93063=CARTESIAN_POINT('Ctrl Pts',(-10.2764726300377,-4.62082310162206,
-0.458855589242014));
#93064=CARTESIAN_POINT('Ctrl Pts',(-10.0786546366006,-2.13389776477927,
-4.12420112479167));
#93065=CARTESIAN_POINT('Ctrl Pts',(-9.88083664316343,2.29464007959512,-4.03697677642298));
#93066=CARTESIAN_POINT('Ctrl Pts',(-9.68301864972636,4.6353075712462,-0.276547117523308));
#93067=CARTESIAN_POINT('Ctrl Pts',(-9.48520065628923,2.758354469664,3.7355100331745));
#93068=CARTESIAN_POINT('Ctrl Pts',(-9.28738266285214,-1.62839812976774,
4.34866348654753));
#93069=CARTESIAN_POINT('Ctrl Pts',(-9.08956466941501,-4.53348734860864,
1.00501096922777));
#93070=CARTESIAN_POINT('Ctrl Pts',(-8.89174667597792,-3.31360118949124,
-3.25309110620423));
#93071=CARTESIAN_POINT('Ctrl Pts',(-8.69392868254081,0.921297975721724,
-4.5512377028885));
#93072=CARTESIAN_POINT('Ctrl Pts',(-8.49611068910371,4.31791720908901,-1.70825804951004));
#93073=CARTESIAN_POINT('Ctrl Pts',(-8.29829269566658,3.78570620605536,2.68904873695079));
#93074=CARTESIAN_POINT('Ctrl Pts',(-8.1004747022295,-0.191081496404787,
4.63961662748058));
#93075=CARTESIAN_POINT('Ctrl Pts',(-7.90265670879236,-3.99400603189376,
2.36864315705417));
#93076=CARTESIAN_POINT('Ctrl Pts',(-7.70483871535528,-4.16282391303512,
-2.05753533562012));
#93077=CARTESIAN_POINT('Ctrl Pts',(-7.50702072191814,-0.543929416570591,
-4.61158274110426));
#93078=CARTESIAN_POINT('Ctrl Pts',(-7.30920272848107,3.56988108564655,-2.96959654205915));
#93079=CARTESIAN_POINT('Ctrl Pts',(-7.11138473504394,4.43549203458706,1.37439623084976));
#93080=CARTESIAN_POINT('Ctrl Pts',(-6.91356674160684,1.26529257426107,4.46783944315096));
#93081=CARTESIAN_POINT('Ctrl Pts',(-6.71574874816973,-3.05618410675896,
3.49603965851134));
#93082=CARTESIAN_POINT('Ctrl Pts',(-6.51793075473263,-4.59686904369474,
-0.656772093920519));
#93083=CARTESIAN_POINT('Ctrl Pts',(-6.32011276129551,-1.95490822411462,
-4.21199340259651));
#93084=CARTESIAN_POINT('Ctrl Pts',(-6.12229476785841,2.46580428719285,-3.93476350060735));
#93085=CARTESIAN_POINT('Ctrl Pts',(-5.9244767744213,4.64290582319052,-0.0773311385160742));
#93086=CARTESIAN_POINT('Ctrl Pts',(-5.72665878098419,2.59547319162859,3.85046406289671));
#93087=CARTESIAN_POINT('Ctrl Pts',(-5.52884078754709,-1.81355487126374,
4.27476003050852));
#93088=CARTESIAN_POINT('Ctrl Pts',(-5.33102279410998,-4.57244726222979,
0.809494052040002));
#93089=CARTESIAN_POINT('Ctrl Pts',(-5.13320480067286,-3.17091503518384,
-3.39232257129167));
#93090=CARTESIAN_POINT('Ctrl Pts',(-4.93538680723577,1.11580147625311,-4.50749838180796));
#93091=CARTESIAN_POINT('Ctrl Pts',(-4.73756881379865,4.3872612385881,-1.52134591609628));
#93092=CARTESIAN_POINT('Ctrl Pts',(-4.53975082036155,3.66679532155438,2.84906417303733));
#93093=CARTESIAN_POINT('Ctrl Pts',(-4.34193282692444,-0.390051464366645,
4.62713891022566));
#93094=CARTESIAN_POINT('Ctrl Pts',(-4.14411483348734,-4.09199425630271,
2.19502562019938));
#93095=CARTESIAN_POINT('Ctrl Pts',(-3.94629684005023,-4.07067190977461,
-2.23431977502652));
#93096=CARTESIAN_POINT('Ctrl Pts',(-3.74847884661311,-0.345485318845901,
-4.63067973303504));
#93097=CARTESIAN_POINT('Ctrl Pts',(-3.55066085317602,3.6940548287243,-2.81362979587035));
#93098=CARTESIAN_POINT('Ctrl Pts',(-3.35284285973889,4.37241119737715,1.5635138710417));
#93099=CARTESIAN_POINT('Ctrl Pts',(-3.1550248663018,1.0723533336669,4.51803216640253));
#93100=CARTESIAN_POINT('Ctrl Pts',(-2.95720687286468,-3.20342737142238,
3.36163671580712));
#93101=CARTESIAN_POINT('Ctrl Pts',(-2.75938887942758,-4.5644428037795,-0.853477096435094));
#93102=CARTESIAN_POINT('Ctrl Pts',(-2.56157088599047,-1.77231360942614,
-4.29202377128854));
#93103=CARTESIAN_POINT('Ctrl Pts',(-2.36375289255336,2.63242014077624,-3.82529417897026));
#93104=CARTESIAN_POINT('Ctrl Pts',(-2.16593489911625,4.64195247107765,0.122020922039425));
#93105=CARTESIAN_POINT('Ctrl Pts',(-1.96811690567915,2.42779572782149,3.95833316538584));
#93106=CARTESIAN_POINT('Ctrl Pts',(-1.77029891224204,-1.99534558787297,
4.19295354374447));
#93107=CARTESIAN_POINT('Ctrl Pts',(-1.57248091880493,-4.60302357102089,
0.612530358397211));
#93108=CARTESIAN_POINT('Ctrl Pts',(-1.37466292536783,-3.02229903101019,
-3.52538794336927));
#93109=CARTESIAN_POINT('Ctrl Pts',(-1.17684493193072,1.30808533033749,-4.45528465113822));
#93110=CARTESIAN_POINT('Ctrl Pts',(-0.979026938493605,4.44883056086126,
-1.33194754643551));
#93111=CARTESIAN_POINT('Ctrl Pts',(-0.781208945056505,3.54052802843261,
3.00443733904289));
#93112=CARTESIAN_POINT('Ctrl Pts',(-0.583390951619396,-0.587155379019583,
4.60496137700709));
#93113=CARTESIAN_POINT('Ctrl Pts',(-0.385572958182286,-4.18466239345957,
2.01964576379865));
#93114=CARTESIAN_POINT('Ctrl Pts',(-0.187754964745179,-3.96652463206152,
-2.41173365972362));
#93115=CARTESIAN_POINT('Ctrl Pts',(-0.0558763024537767,-1.4269357426901,
-3.88994463893176));
#93116=CARTESIAN_POINT('Ctrl Pts',(0.0100630286919268,-0.124001864240948,
-3.93104471326196));
#93117=CARTESIAN_POINT('Ctrl Pts',(-1.54616352203498,-3.93676751258924,
0.00274060645320142));
#93118=CARTESIAN_POINT('Ctrl Pts',(-1.48899665647926,-3.92780616728942,
-1.12431394949728));
#93119=CARTESIAN_POINT('Ctrl Pts',(-1.43182979092354,-3.41813976225738,
-2.25845087457351));
#93120=CARTESIAN_POINT('Ctrl Pts',(-1.37466292536783,-2.56402239412072,
-2.99071767770299));
#93121=CARTESIAN_POINT('Ctrl Pts',(-1.30872359422213,-1.57883757722767,
-3.83535351262556));
#93122=CARTESIAN_POINT('Ctrl Pts',(-1.24278426307642,-0.13537612344502,
-4.1453190818819));
#93123=CARTESIAN_POINT('Ctrl Pts',(-1.17684493193072,1.10981214186687,-3.77974568239293));
#93124=CARTESIAN_POINT('Ctrl Pts',(-1.11090560078501,2.35500040717879,-3.41417228290396));
#93125=CARTESIAN_POINT('Ctrl Pts',(-1.04496626963931,3.40191548402005,-2.3730599146697));
#93126=CARTESIAN_POINT('Ctrl Pts',(-0.979026938493604,3.77398926703588,
-1.12977291630615));
#93127=CARTESIAN_POINT('Ctrl Pts',(-0.913087607347902,4.1460630500517,0.113514082057356));
#93128=CARTESIAN_POINT('Ctrl Pts',(-0.847148276202203,3.84329553924214,
1.55897571055012));
#93129=CARTESIAN_POINT('Ctrl Pts',(-0.781208945056502,3.003964549262,2.54846053112388));
#93130=CARTESIAN_POINT('Ctrl Pts',(-0.715269613910799,2.16463355928184,
3.53794535169766));
#93131=CARTESIAN_POINT('Ctrl Pts',(-0.649330282765096,0.78873909013109,
4.07145336435238));
#93132=CARTESIAN_POINT('Ctrl Pts',(-0.583390951619391,-0.498792646850961,
3.90732143514497));
#93133=CARTESIAN_POINT('Ctrl Pts',(-0.522260634412929,-1.69242355161679,
3.75515979319585));
#93134=CARTESIAN_POINT('Ctrl Pts',(-0.461130317206467,-2.8101104753617,
3.00340652247003));
#93135=CARTESIAN_POINT('Ctrl Pts',(-0.400000000000004,-3.41555626699893,
1.96277456085016));
#93136=CARTESIAN_POINT('',(-29.267,-1.87158653173899,-2.62360084935061));
#93137=CARTESIAN_POINT('Ctrl Pts',(-29.267,-1.87556211950935,-2.62715993178767));
#93138=CARTESIAN_POINT('Ctrl Pts',(-29.267,-1.94413804945346,-2.58901550230507));
#93139=CARTESIAN_POINT('Ctrl Pts',(-29.267,-2.01110052498262,-2.54827549470737));
#93140=CARTESIAN_POINT('Ctrl Pts',(-29.267,-2.07628315157793,-2.50497168480714));
#93141=CARTESIAN_POINT('Ctrl Pts',(-29.267,-2.16191037886223,-2.44808558852224));
#93142=CARTESIAN_POINT('Ctrl Pts',(-29.267,-2.24446748355392,-2.38677728024994));
#93143=CARTESIAN_POINT('Ctrl Pts',(-29.267,-2.32386237913326,-2.32143742155821));
#93144=CARTESIAN_POINT('Ctrl Pts',(-29.267,-2.37364457503314,-2.28046801638769));
#93145=CARTESIAN_POINT('Ctrl Pts',(-29.267,-2.42218320448196,-2.23791254568436));
#93146=CARTESIAN_POINT('Ctrl Pts',(-29.267,-2.46945134988874,-2.19385797799918));
#93147=CARTESIAN_POINT('Ctrl Pts',(-29.267,-2.49412738319863,-2.17085957240706));
#93148=CARTESIAN_POINT('Ctrl Pts',(-29.267,-2.51845711293783,-2.14745250715669));
#93149=CARTESIAN_POINT('Ctrl Pts',(-29.267,-2.54243628966495,-2.12364846865249));
#93150=CARTESIAN_POINT('Ctrl Pts',(-29.267,-2.55699647231938,-2.1091946301209));
#93151=CARTESIAN_POINT('Ctrl Pts',(-29.267,-2.57142234337411,-2.09459937375049));
#93152=CARTESIAN_POINT('Ctrl Pts',(-29.267,-2.58570771899918,-2.07987136520091));
#93153=CARTESIAN_POINT('Ctrl Pts',(-29.267,-2.65959479463748,-2.00369489562351));
#93154=CARTESIAN_POINT('Ctrl Pts',(-29.267,-2.72977136737143,-1.9239251248109));
#93155=CARTESIAN_POINT('Ctrl Pts',(-29.267,-2.79613899963645,-1.84096944342322));
#93156=CARTESIAN_POINT('Ctrl Pts',(-29.267,-2.85949750354379,-1.76177499751697));
#93157=CARTESIAN_POINT('Ctrl Pts',(-29.267,-2.91938482899898,-1.67967617064163));
#93158=CARTESIAN_POINT('Ctrl Pts',(-29.267,-2.97569370105063,-1.59499101459634));
#93159=CARTESIAN_POINT('Ctrl Pts',(-29.267,-3.00071677359493,-1.55735781886826));
#93160=CARTESIAN_POINT('Ctrl Pts',(-29.267,-3.02503285489035,-1.51921344645886));
#93161=CARTESIAN_POINT('Ctrl Pts',(-29.267,-3.048630913558,-1.48058395925084));
#93162=CARTESIAN_POINT('Ctrl Pts',(-29.267,-3.05877704718637,-1.46397496845512));
#93163=CARTESIAN_POINT('Ctrl Pts',(-29.267,-3.06879043196106,-1.44727628527374));
#93164=CARTESIAN_POINT('Ctrl Pts',(-29.267,-3.07867012826134,-1.43048992553262));
#93165=CARTESIAN_POINT('Ctrl Pts',(-29.267,-3.0873232258654,-1.4157876508025));
#93166=CARTESIAN_POINT('Ctrl Pts',(-29.267,-3.09586909840926,-1.40102604067025));
#93167=CARTESIAN_POINT('Ctrl Pts',(-29.267,-3.10430668639324,-1.38620798147017));
#93168=CARTESIAN_POINT('Ctrl Pts',(-29.267,-3.15937851519779,-1.28949104992148));
#93169=CARTESIAN_POINT('Ctrl Pts',(-29.267,-3.20984986675861,-1.19035556854987));
#93170=CARTESIAN_POINT('Ctrl Pts',(-29.267,-3.25561444260331,-1.08923039523438));
#93171=CARTESIAN_POINT('Ctrl Pts',(-29.267,-3.3020888475654,-0.986536725080546));
#93172=CARTESIAN_POINT('Ctrl Pts',(-29.267,-3.34370992002807,-0.881790488775369));
#93173=CARTESIAN_POINT('Ctrl Pts',(-29.267,-3.38033216148825,-0.775399491221893));
#93174=CARTESIAN_POINT('Ctrl Pts',(-29.267,-3.41685272414127,-0.669303880004472));
#93175=CARTESIAN_POINT('Ctrl Pts',(-29.267,-3.44840267319171,-0.561571812339358));
#93176=CARTESIAN_POINT('Ctrl Pts',(-29.267,-3.47479600376177,-0.45257833184847));
#93177=CARTESIAN_POINT('Ctrl Pts',(-29.267,-3.49203326148151,-0.381395624989836));
#93178=CARTESIAN_POINT('Ctrl Pts',(-29.267,-3.5070702109759,-0.309674316182991));
#93179=CARTESIAN_POINT('Ctrl Pts',(-29.267,-3.51984382259218,-0.237514625278931));
#93180=CARTESIAN_POINT('Ctrl Pts',(-29.267,-3.52358595661669,-0.216374853486772));
#93181=CARTESIAN_POINT('Ctrl Pts',(-29.267,-3.5271337783978,-0.195197442610527));
#93182=CARTESIAN_POINT('Ctrl Pts',(-29.267,-3.53048554423178,-0.1739848805149));
#93183=CARTESIAN_POINT('Ctrl Pts',(-29.267,-3.53317888328294,-0.156939351472193));
#93184=CARTESIAN_POINT('Ctrl Pts',(-29.267,-3.53574447963492,-0.139878128935328));
#93185=CARTESIAN_POINT('Ctrl Pts',(-29.267,-3.53818070904561,-0.122810384767));
#93186=CARTESIAN_POINT('Ctrl Pts',(-29.267,-3.55454810859626,-0.00814360215415144));
#93187=CARTESIAN_POINT('Ctrl Pts',(-29.267,-3.56509706882811,0.106923245517097));
#93188=CARTESIAN_POINT('Ctrl Pts',(-29.267,-3.56968323623,0.221965651223056));
#93189=CARTESIAN_POINT('Ctrl Pts',(-29.267,-3.57226426632728,0.286709888746834));
#93190=CARTESIAN_POINT('Ctrl Pts',(-29.267,-3.57295596462551,0.351446964375039));
#93191=CARTESIAN_POINT('Ctrl Pts',(-29.267,-3.57172621322166,0.416104672924591));
#93192=CARTESIAN_POINT('Ctrl Pts',(-29.267,-3.56961444125406,0.527137143370704));
#93193=CARTESIAN_POINT('Ctrl Pts',(-29.267,-3.56183970729814,0.637935324401442));
#93194=CARTESIAN_POINT('Ctrl Pts',(-29.267,-3.54866558297903,0.748214710453893));
#93195=CARTESIAN_POINT('Ctrl Pts',(-29.267,-3.53524477571288,0.860559056824879));
#93196=CARTESIAN_POINT('Ctrl Pts',(-29.267,-3.51622037619464,0.972365678151204));
#93197=CARTESIAN_POINT('Ctrl Pts',(-29.267,-3.49181697551176,1.08333660943036));
#93198=CARTESIAN_POINT('Ctrl Pts',(-29.267,-3.48335985307657,1.12179414921221));
#93199=CARTESIAN_POINT('Ctrl Pts',(-29.267,-3.474256248861,1.16015129842181));
#93200=CARTESIAN_POINT('Ctrl Pts',(-29.267,-3.46451407474897,1.19839549460657));
#93201=CARTESIAN_POINT('Ctrl Pts',(-29.267,-3.46095476509623,1.21236803657475));
#93202=CARTESIAN_POINT('Ctrl Pts',(-29.267,-3.45731047162383,1.2263243188045));
#93203=CARTESIAN_POINT('Ctrl Pts',(-29.267,-3.45358428768816,1.24025414023616));
#93204=CARTESIAN_POINT('Ctrl Pts',(-29.267,-3.4241337376961,1.35035093350684));
#93205=CARTESIAN_POINT('Ctrl Pts',(-29.267,-3.38953078097407,1.45895736979579));
#93206=CARTESIAN_POINT('Ctrl Pts',(-29.267,-3.35007714113598,1.565780445815));
#93207=CARTESIAN_POINT('Ctrl Pts',(-29.267,-3.30935323107808,1.67604285399249));
#93208=CARTESIAN_POINT('Ctrl Pts',(-29.267,-3.26346122728659,1.78440591486737));
#93209=CARTESIAN_POINT('Ctrl Pts',(-29.267,-3.21267761166844,1.89055080029088));
#93210=CARTESIAN_POINT('Ctrl Pts',(-29.267,-3.16141486757542,1.99769713148479));
#93211=CARTESIAN_POINT('Ctrl Pts',(-29.267,-3.10516751118045,2.10258403490618));
#93212=CARTESIAN_POINT('Ctrl Pts',(-29.267,-3.04416698925102,2.20487550184191));
#93213=CARTESIAN_POINT('Ctrl Pts',(-29.267,-3.00436620678509,2.27161723281168));
#93214=CARTESIAN_POINT('Ctrl Pts',(-29.267,-2.96254087141324,2.33725386583506));
#93215=CARTESIAN_POINT('Ctrl Pts',(-29.267,-2.91874414438408,2.40168772232732));
#93216=CARTESIAN_POINT('Ctrl Pts',(-29.267,-2.8943383194777,2.4375936341674));
#93217=CARTESIAN_POINT('Ctrl Pts',(-29.267,-2.8693201667382,2.473125974087));
#93218=CARTESIAN_POINT('Ctrl Pts',(-29.267,-2.84369778827627,2.50826717296835));
#93219=CARTESIAN_POINT('Ctrl Pts',(-29.267,-2.83388561980058,2.5217246029401));
#93220=CARTESIAN_POINT('Ctrl Pts',(-29.267,-2.82399066498491,2.5351166552739));
#93221=CARTESIAN_POINT('Ctrl Pts',(-29.267,-2.81401448605096,2.54844146066517));
#93222=CARTESIAN_POINT('Ctrl Pts',(-29.267,-2.74056959066549,2.64653903334034));
#93223=CARTESIAN_POINT('Ctrl Pts',(-29.267,-2.66271315483198,2.74101121591069));
#93224=CARTESIAN_POINT('Ctrl Pts',(-29.267,-2.58073485214103,2.8315238453715));
#93225=CARTESIAN_POINT('Ctrl Pts',(-29.267,-2.49861629012292,2.92219133581491));
#93226=CARTESIAN_POINT('Ctrl Pts',(-29.267,-2.41236136137793,3.00888654180042));
#93227=CARTESIAN_POINT('Ctrl Pts',(-29.267,-2.32221139231555,3.09125732425718));
#93228=CARTESIAN_POINT('Ctrl Pts',(-29.267,-2.2337606222272,3.17207553436702));
#93229=CARTESIAN_POINT('Ctrl Pts',(-29.267,-2.14155975600952,3.24873150750497));
#93230=CARTESIAN_POINT('Ctrl Pts',(-29.267,-2.04579561361836,3.32086577349601));
#93231=CARTESIAN_POINT('Ctrl Pts',(-29.267,-1.95025849965636,3.39282903049885));
#93232=CARTESIAN_POINT('Ctrl Pts',(-29.267,-1.85117460884397,3.4602927682777));
#93233=CARTESIAN_POINT('Ctrl Pts',(-29.267,-1.74869447533116,3.52286199445086));
#93234=CARTESIAN_POINT('Ctrl Pts',(-29.267,-1.87556211950935,-2.62715993178767));
#93235=CARTESIAN_POINT('Ctrl Pts',(-29.2058696827935,-1.06959153349225,
-3.19605863350378));
#93236=CARTESIAN_POINT('Ctrl Pts',(-29.0788000344414,1.19433685232607,-3.56810302549924));
#93237=CARTESIAN_POINT('Ctrl Pts',(-28.8857910549435,3.66252655955179,-1.03121985822236));
#93238=CARTESIAN_POINT('Ctrl Pts',(-28.6879730615064,2.8605553688775,2.50949297218581));
#93239=CARTESIAN_POINT('Ctrl Pts',(-28.4901550680693,-0.544644508144919,
3.76563167765424));
#93240=CARTESIAN_POINT('Ctrl Pts',(-28.3295728978095,-2.90640396394737,
2.00447016268953));
#93241=CARTESIAN_POINT('Ctrl Pts',(-28.2349300586953,-3.21932528384686,
0.467741112490102));
#93242=CARTESIAN_POINT('Ctrl Pts',(-28.2062265507269,-3.21789432005771,
0.00111814815214498));
#93243=CARTESIAN_POINT('Origin',(-29.267,-5.160062080289E-16,2.1385152528819E-16));
#93244=CARTESIAN_POINT('',(-29.267,-3.933,-4.81653586104654E-16));
#93245=CARTESIAN_POINT('Origin',(-29.267,0.,0.));
#93246=CARTESIAN_POINT('Origin',(-29.267,0.,0.));
#93247=CARTESIAN_POINT('',(-29.267,1.87158653173901,-2.62360084935059));
#93248=CARTESIAN_POINT('Ctrl Pts',(-29.267,1.752798395271,3.52791786994593));
#93249=CARTESIAN_POINT('Ctrl Pts',(-29.267,1.83395735182908,3.47886451957651));
#93250=CARTESIAN_POINT('Ctrl Pts',(-29.267,1.91309406069084,3.42675125683998));
#93251=CARTESIAN_POINT('Ctrl Pts',(-29.267,1.99001035894838,3.37156906414815));
#93252=CARTESIAN_POINT('Ctrl Pts',(-29.267,2.08883318098501,3.30067043626935));
#93253=CARTESIAN_POINT('Ctrl Pts',(-29.267,2.18399221922082,3.22470642798029));
#93254=CARTESIAN_POINT('Ctrl Pts',(-29.267,2.27530185738888,3.14408709844798));
#93255=CARTESIAN_POINT('Ctrl Pts',(-29.267,2.32778341860941,3.09774994978225));
#93256=CARTESIAN_POINT('Ctrl Pts',(-29.267,2.37899256877283,3.0498742455389));
#93257=CARTESIAN_POINT('Ctrl Pts',(-29.267,2.42888757139592,3.00053373763079));
#93258=CARTESIAN_POINT('Ctrl Pts',(-29.267,2.46017084034004,2.96959812689661));
#93259=CARTESIAN_POINT('Ctrl Pts',(-29.267,2.49093741259874,2.93808663944416));
#93260=CARTESIAN_POINT('Ctrl Pts',(-29.267,2.5211759780696,2.90601703563223));
#93261=CARTESIAN_POINT('Ctrl Pts',(-29.267,2.53506009770383,2.89129218976028));
#93262=CARTESIAN_POINT('Ctrl Pts',(-29.267,2.54883244835416,2.87645004363996));
#93263=CARTESIAN_POINT('Ctrl Pts',(-29.267,2.5624830469874,2.8615023243299));
#93264=CARTESIAN_POINT('Ctrl Pts',(-29.267,2.64596845224788,2.77008388636619));
#93265=CARTESIAN_POINT('Ctrl Pts',(-29.267,2.72499364171481,2.67462471248027));
#93266=CARTESIAN_POINT('Ctrl Pts',(-29.267,2.79936387127853,2.57555879213958));
#93267=CARTESIAN_POINT('Ctrl Pts',(-29.267,2.86443782214679,2.48887611184149));
#93268=CARTESIAN_POINT('Ctrl Pts',(-29.267,2.92594727850818,2.3994310409066));
#93269=CARTESIAN_POINT('Ctrl Pts',(-29.267,2.98372919602265,2.30749997840723));
#93270=CARTESIAN_POINT('Ctrl Pts',(-29.267,3.00900878493524,2.26728013856375));
#93271=CARTESIAN_POINT('Ctrl Pts',(-29.267,3.03357448870034,2.22658434219884));
#93272=CARTESIAN_POINT('Ctrl Pts',(-29.267,3.05741067291968,2.18543533259932));
#93273=CARTESIAN_POINT('Ctrl Pts',(-29.267,3.07143266131865,2.16122881825439));
#93274=CARTESIAN_POINT('Ctrl Pts',(-29.267,3.08520217217235,2.13686546385367));
#93275=CARTESIAN_POINT('Ctrl Pts',(-29.267,3.09871581841762,2.11234988443433));
#93276=CARTESIAN_POINT('Ctrl Pts',(-29.267,3.10919621461938,2.09333703025958));
#93277=CARTESIAN_POINT('Ctrl Pts',(-29.267,3.11952377181851,2.07423043659365));
#93278=CARTESIAN_POINT('Ctrl Pts',(-29.267,3.12968628263755,2.05505274587221));
#93279=CARTESIAN_POINT('Ctrl Pts',(-29.267,3.18534814899617,1.95001314719307));
#93280=CARTESIAN_POINT('Ctrl Pts',(-29.267,3.23613492547288,1.84271397680196));
#93281=CARTESIAN_POINT('Ctrl Pts',(-29.267,3.28187401835454,1.73353344117171));
#93282=CARTESIAN_POINT('Ctrl Pts',(-29.267,3.32728770285637,1.62512966474171));
#93283=CARTESIAN_POINT('Ctrl Pts',(-29.267,3.36772549975111,1.51487033063548));
#93284=CARTESIAN_POINT('Ctrl Pts',(-29.267,3.40296884306188,1.40311370918593));
#93285=CARTESIAN_POINT('Ctrl Pts',(-29.267,3.43717304060426,1.29465221837269));
#93286=CARTESIAN_POINT('Ctrl Pts',(-29.267,3.46648459568988,1.18477969669452));
#93287=CARTESIAN_POINT('Ctrl Pts',(-29.267,3.49065535521413,1.07382410402513));
#93288=CARTESIAN_POINT('Ctrl Pts',(-29.267,3.50713741723422,0.998163388522294));
#93289=CARTESIAN_POINT('Ctrl Pts',(-29.267,3.52122807768353,0.921999073055619));
#93290=CARTESIAN_POINT('Ctrl Pts',(-29.267,3.53283505631117,0.845437826880077));
#93291=CARTESIAN_POINT('Ctrl Pts',(-29.267,3.53650941868402,0.821201221369631));
#93292=CARTESIAN_POINT('Ctrl Pts',(-29.267,3.53993479734101,0.796924862307499));
#93293=CARTESIAN_POINT('Ctrl Pts',(-29.267,3.54310802391695,0.772612209064599));
#93294=CARTESIAN_POINT('Ctrl Pts',(-29.267,3.54518371661638,0.756708649822146));
#93295=CARTESIAN_POINT('Ctrl Pts',(-29.267,3.54715182636697,0.740786860054947));
#93296=CARTESIAN_POINT('Ctrl Pts',(-29.267,3.54901039433523,0.724856886056574));
#93297=CARTESIAN_POINT('Ctrl Pts',(-29.267,3.56199475275373,0.613566637045098));
#93298=CARTESIAN_POINT('Ctrl Pts',(-29.267,3.56961554007749,0.502076700900192));
#93299=CARTESIAN_POINT('Ctrl Pts',(-29.267,3.57168257316973,0.390705415856302));
#93300=CARTESIAN_POINT('Ctrl Pts',(-29.267,3.57315383999081,0.311433885506525));
#93301=CARTESIAN_POINT('Ctrl Pts',(-29.267,3.57181041061219,0.232222349124384));
#93302=CARTESIAN_POINT('Ctrl Pts',(-29.267,3.56756762581781,0.153187282053559));
#93303=CARTESIAN_POINT('Ctrl Pts',(-29.267,3.56149580005725,0.0400806364220606));
#93304=CARTESIAN_POINT('Ctrl Pts',(-29.267,3.54948772715183,-0.0726657673483353));
#93305=CARTESIAN_POINT('Ctrl Pts',(-29.267,3.53175700430858,-0.184693834183496));
#93306=CARTESIAN_POINT('Ctrl Pts',(-29.267,3.51395987864282,-0.297141454124599));
#93307=CARTESIAN_POINT('Ctrl Pts',(-29.267,3.49039661484532,-0.408866144611942));
#93308=CARTESIAN_POINT('Ctrl Pts',(-29.267,3.46123882223617,-0.519478579222817));
#93309=CARTESIAN_POINT('Ctrl Pts',(-29.267,3.45486906339251,-0.543642772412126));
#93310=CARTESIAN_POINT('Ctrl Pts',(-29.267,3.44823216157597,-0.567753755563771));
#93311=CARTESIAN_POINT('Ctrl Pts',(-29.267,3.44132966501532,-0.591807239612535));
#93312=CARTESIAN_POINT('Ctrl Pts',(-29.267,3.43531557970422,-0.612764831380591));
#93313=CARTESIAN_POINT('Ctrl Pts',(-29.267,3.42909832027748,-0.633683474481864));
#93314=CARTESIAN_POINT('Ctrl Pts',(-29.267,3.42268802028739,-0.654531474620821));
#93315=CARTESIAN_POINT('Ctrl Pts',(-29.267,3.38997005995087,-0.760938981710492));
#93316=CARTESIAN_POINT('Ctrl Pts',(-29.267,3.35219258588973,-0.865637661248984));
#93317=CARTESIAN_POINT('Ctrl Pts',(-29.267,3.30959231005111,-0.968301959519508));
#93318=CARTESIAN_POINT('Ctrl Pts',(-29.267,3.26694576890514,-1.07107775461064));
#93319=CARTESIAN_POINT('Ctrl Pts',(-29.267,3.21946535835239,-1.1718154969129));
#93320=CARTESIAN_POINT('Ctrl Pts',(-29.267,3.16734388272138,-1.27016148531058));
#93321=CARTESIAN_POINT('Ctrl Pts',(-29.267,3.11585673221232,-1.36731059026764));
#93322=CARTESIAN_POINT('Ctrl Pts',(-29.267,3.05984017368962,-1.46212642571529));
#93323=CARTESIAN_POINT('Ctrl Pts',(-29.267,2.9994455855754,-1.55423154140084));
#93324=CARTESIAN_POINT('Ctrl Pts',(-29.267,2.96352940982248,-1.60900571282907));
#93325=CARTESIAN_POINT('Ctrl Pts',(-29.267,2.9260642937352,-1.6628204737105));
#93326=CARTESIAN_POINT('Ctrl Pts',(-29.267,2.88707751446442,-1.71558884474527));
#93327=CARTESIAN_POINT('Ctrl Pts',(-29.267,2.86858036962461,-1.74062461892943));
#93328=CARTESIAN_POINT('Ctrl Pts',(-29.267,2.84974065503184,-1.76542476192336));
#93329=CARTESIAN_POINT('Ctrl Pts',(-29.267,2.83056106449946,-1.78997947648368));
#93330=CARTESIAN_POINT('Ctrl Pts',(-29.267,2.82019641614239,-1.80324884120218));
#93331=CARTESIAN_POINT('Ctrl Pts',(-29.267,2.80973696569548,-1.81644076475104));
#93332=CARTESIAN_POINT('Ctrl Pts',(-29.267,2.79918811988956,-1.82954813134034));
#93333=CARTESIAN_POINT('Ctrl Pts',(-29.267,2.73178606534395,-1.91329790397479));
#93334=CARTESIAN_POINT('Ctrl Pts',(-29.267,2.66067793855252,-1.99367458528833));
#93335=CARTESIAN_POINT('Ctrl Pts',(-29.267,2.58603966220747,-2.07035807397434));
#93336=CARTESIAN_POINT('Ctrl Pts',(-29.267,2.51244806685979,-2.14596620087079));
#93337=CARTESIAN_POINT('Ctrl Pts',(-29.267,2.43542404680641,-2.21798450045409));
#93338=CARTESIAN_POINT('Ctrl Pts',(-29.267,2.35510789090453,-2.28606528024848));
#93339=CARTESIAN_POINT('Ctrl Pts',(-29.267,2.2772577781145,-2.35205569433528));
#93340=CARTESIAN_POINT('Ctrl Pts',(-29.267,2.19631404788083,-2.41434695939189));
#93341=CARTESIAN_POINT('Ctrl Pts',(-29.267,2.11238597055247,-2.47257820210255));
#93342=CARTESIAN_POINT('Ctrl Pts',(-29.267,2.03465401232407,-2.52651043396178));
#93343=CARTESIAN_POINT('Ctrl Pts',(-29.267,1.95436164731551,-2.57695984678878));
#93344=CARTESIAN_POINT('Ctrl Pts',(-29.267,1.87158653173901,-2.62360084935059));
#93345=CARTESIAN_POINT('Origin',(-29.267,0.,0.));
#93346=CARTESIAN_POINT('Origin',(-31.5777734492731,0.,0.));
#93347=CARTESIAN_POINT('Ctrl Pts',(-29.267,1.871586531739,-2.6236008493506));
#93348=CARTESIAN_POINT('Ctrl Pts',(-29.2010606688543,2.74117176403474,-2.0032686790181));
#93349=CARTESIAN_POINT('Ctrl Pts',(-29.069182006563,3.80053009112415,0.158992474904673));
#93350=CARTESIAN_POINT('Ctrl Pts',(-28.8713640131257,1.93474699165479,3.27922584988832));
#93351=CARTESIAN_POINT('Ctrl Pts',(-28.6735460196887,-1.69312072237911,
3.40633319030359));
#93352=CARTESIAN_POINT('Ctrl Pts',(-28.5340158317378,-3.16477800868145,
1.31315271293012));
#93353=CARTESIAN_POINT('Ctrl Pts',(-28.4604249749326,-3.22715455055888,
0.12579512260648));
#93354=CARTESIAN_POINT('Ctrl Pts',(-28.4527734492731,-3.22624365146105,
0.0022389224034757));
#93355=CARTESIAN_POINT('Ctrl Pts',(-29.6770630286919,2.28405859260864,-3.20180657528381));
#93356=CARTESIAN_POINT('Ctrl Pts',(-29.6111236975462,3.34528851072799,-2.44476168321409));
#93357=CARTESIAN_POINT('Ctrl Pts',(-29.4792450352549,4.63811491688505,0.194032240726105));
#93358=CARTESIAN_POINT('Ctrl Pts',(-29.2814270418177,2.36113875360431,4.00192235439013));
#93359=CARTESIAN_POINT('Ctrl Pts',(-29.0836090483806,-2.06626136098581,
4.15704241330045));
#93360=CARTESIAN_POINT('Ctrl Pts',(-28.8857910549435,-4.61251479306561,
0.535432936636152));
#93361=CARTESIAN_POINT('Ctrl Pts',(-28.6879730615064,-2.96244924208781,
-3.57632094417714));
#93362=CARTESIAN_POINT('Ctrl Pts',(-28.4901550680693,1.38341358179131,-4.4324734582532));
#93363=CARTESIAN_POINT('Ctrl Pts',(-28.2923370746322,4.47036851547105,-1.25636722700296));
#93364=CARTESIAN_POINT('Ctrl Pts',(-28.0945190811951,3.489859458072,3.06331556440806));
#93365=CARTESIAN_POINT('Ctrl Pts',(-27.896701087758,-0.666080140453031,
4.59549820331548));
#93366=CARTESIAN_POINT('Ctrl Pts',(-27.6988830943208,-4.2159381251684,1.94639706903792));
#93367=CARTESIAN_POINT('Ctrl Pts',(-27.5010651008838,-3.92976705706495,
-2.47377142775801));
#93368=CARTESIAN_POINT('Ctrl Pts',(-27.3032471074466,-0.0679337783385457,
-4.64304845044703));
#93369=CARTESIAN_POINT('Ctrl Pts',(-27.1054291140096,3.8557086591862,-2.58767786462851));
#93370=CARTESIAN_POINT('Ctrl Pts',(-26.9076111205724,4.27108148336715,1.82220379196051));
#93371=CARTESIAN_POINT('Ctrl Pts',(-26.7097931271353,0.800238585829137,
4.57407575421308));
#93372=CARTESIAN_POINT('Ctrl Pts',(-26.5119751336982,-3.39873305617157,
3.16404367576156));
#93373=CARTESIAN_POINT('Ctrl Pts',(-26.3141571402611,-4.50523127888368,
-1.12492171884469));
#93374=CARTESIAN_POINT('Ctrl Pts',(-26.116339146824,-1.51246392145779,-4.3903313135453));
#93375=CARTESIAN_POINT('Ctrl Pts',(-25.9185211533869,2.8564793618577,-3.66102212460931));
#93376=CARTESIAN_POINT('Ctrl Pts',(-25.7207031599498,4.62634030974878,0.39941512218846));
#93377=CARTESIAN_POINT('Ctrl Pts',(-25.5228851665127,2.18673986986448,4.09642840245587));
#93378=CARTESIAN_POINT('Ctrl Pts',(-25.3250671730756,-2.24255357823703,
4.06614197186242));
#93379=CARTESIAN_POINT('Ctrl Pts',(-25.1272491796384,-4.63136967163741,
0.336113082707444));
#93380=CARTESIAN_POINT('Ctrl Pts',(-24.9294311862014,-2.80614822532237,
-3.69974176897582));
#93381=CARTESIAN_POINT('Ctrl Pts',(-24.7316131927642,1.57235978395034,-4.36923812050275));
#93382=CARTESIAN_POINT('Ctrl Pts',(-24.5337951993272,4.52019315087723,-1.06320784152848));
#93383=CARTESIAN_POINT('Ctrl Pts',(-24.33597720589,3.35514739875397,3.21022475323414));
#93384=CARTESIAN_POINT('Ctrl Pts',(-24.1381592124529,-0.862713844891543,
4.5627055415416));
#93385=CARTESIAN_POINT('Ctrl Pts',(-23.9403412190158,-4.29560027900972,
1.76362560612109));
#93386=CARTESIAN_POINT('Ctrl Pts',(-23.7425232255787,-3.81996243101423,
-2.64015985521965));
#93387=CARTESIAN_POINT('Ctrl Pts',(-23.5447052321416,0.131421517249421,
-4.64168993155775));
#93388=CARTESIAN_POINT('Ctrl Pts',(-23.3468872387045,3.96322632454721,-2.41979216795887));
#93389=CARTESIAN_POINT('Ctrl Pts',(-23.1490692452674,4.18893062930736,2.0038505978625));
#93390=CARTESIAN_POINT('Ctrl Pts',(-22.9512512518303,0.603168313088729,
4.60420948935287));
#93391=CARTESIAN_POINT('Ctrl Pts',(-22.7534332583932,-3.53141089594158,
3.01524362527346));
#93392=CARTESIAN_POINT('Ctrl Pts',(-22.555615264956,-4.45279419747962,-1.31726264299215));
#93393=CARTESIAN_POINT('Ctrl Pts',(-22.357797271519,-1.32262402256341,-4.45120463814867));
#93394=CARTESIAN_POINT('Ctrl Pts',(-22.1599792780818,3.01098869180223,-3.53503948118999));
#93395=CARTESIAN_POINT('Ctrl Pts',(-21.9621612846447,4.60493252393142,0.597623197150572));
#93396=CARTESIAN_POINT('Ctrl Pts',(-21.7643432912076,2.00889371847677,4.18651442892525));
#93397=CARTESIAN_POINT('Ctrl Pts',(-21.5665252977705,-2.41501764698298,
3.96613751658901));
#93398=CARTESIAN_POINT('Ctrl Pts',(-21.3687073043334,-4.64152829967862,
0.137011236826592));
#93399=CARTESIAN_POINT('Ctrl Pts',(-21.1708893108963,-2.64475817975951,
-3.81678021456953));
#93400=CARTESIAN_POINT('Ctrl Pts',(-20.9730713174592,1.7584512953968,-4.29772103299545));
#93401=CARTESIAN_POINT('Ctrl Pts',(-20.7752533240221,4.56166329861203,-0.868207916244836));
#93402=CARTESIAN_POINT('Ctrl Pts',(-20.577435330585,3.21426290515085,3.35127901140825));
#93403=CARTESIAN_POINT('Ctrl Pts',(-20.3796173371479,-1.05776357028257,
4.52147025480841));
#93404=CARTESIAN_POINT('Ctrl Pts',(-20.1817993437108,-4.36734141674695,
1.57762035525057));
#93405=CARTESIAN_POINT('Ctrl Pts',(-19.9839813502736,-3.70311842824315,
-2.80169072920981));
#93406=CARTESIAN_POINT('Ctrl Pts',(-19.7861633568366,0.330535456070876,
-4.63177108113238));
#93407=CARTESIAN_POINT('Ctrl Pts',(-19.5883453633994,4.06343839238611,-2.24744865725935));
#93408=CARTESIAN_POINT('Ctrl Pts',(-19.3905273699623,4.09905885506931,2.18180511008938));
#93409=CARTESIAN_POINT('Ctrl Pts',(-19.1927093765252,0.404986136817035,
4.62585594941305));
#93410=CARTESIAN_POINT('Ctrl Pts',(-18.9948913830881,-3.65757946877007,
2.86088613289063));
#93411=CARTESIAN_POINT('Ctrl Pts',(-18.797073389651,-4.3921496281511,-1.50717572952404));
#93412=CARTESIAN_POINT('Ctrl Pts',(-18.5992553962139,-1.13034620594656,
-4.50387327646287));
#93413=CARTESIAN_POINT('Ctrl Pts',(-18.4014374027768,3.15994806878659,-3.40254099729982));
#93414=CARTESIAN_POINT('Ctrl Pts',(-18.2036194093397,4.57503679488795,0.794729740953231));
#93415=CARTESIAN_POINT('Ctrl Pts',(-18.0058014159026,1.82734471209214,4.26888373452864));
#93416=CARTESIAN_POINT('Ctrl Pts',(-17.8079834224655,-2.58303028228958,
3.85882256608273));
#93417=CARTESIAN_POINT('Ctrl Pts',(-17.6101654290284,-4.64313152588309,
-0.0623431558779312));
#93418=CARTESIAN_POINT('Ctrl Pts',(-17.4123474355912,-2.47849323716755,
-3.92678345583875));
#93419=CARTESIAN_POINT('Ctrl Pts',(-17.2145294421541,1.94130157710662,-4.218282259695));
#93420=CARTESIAN_POINT('Ctrl Pts',(-17.016711448717,4.59472525345006,-0.671607683876884));
#93421=CARTESIAN_POINT('Ctrl Pts',(-16.8188934552799,3.067453786841,3.48615609250776));
#93422=CARTESIAN_POINT('Ctrl Pts',(-16.6210754618428,-1.25086359448258,
4.47190086023073));
#93423=CARTESIAN_POINT('Ctrl Pts',(-16.4232574684057,-4.43103254135455,
1.38870718770775));
#93424=CARTESIAN_POINT('Ctrl Pts',(-16.2254394749686,-3.57944872782031,
-2.95805744376943));
#93425=CARTESIAN_POINT('Ctrl Pts',(-16.0276214815315,0.529040142139094,
-4.61331481298855));
#93426=CARTESIAN_POINT('Ctrl Pts',(-15.8298034880944,4.15616061014518,-2.07096258257165));
#93427=CARTESIAN_POINT('Ctrl Pts',(-15.6319854946573,4.00163157405578,2.3557380544649));
#93428=CARTESIAN_POINT('Ctrl Pts',(-15.4341675012202,0.206057478095051,
4.63897589468358));
#93429=CARTESIAN_POINT('Ctrl Pts',(-15.236349507783,-3.77700628271434,2.70125537039182));
#93430=CARTESIAN_POINT('Ctrl Pts',(-15.038531514346,-4.32340931844811,-1.69431074507903));
#93431=CARTESIAN_POINT('Ctrl Pts',(-14.8407135209088,-0.935984901700447,
-4.54824024206318));
#93432=CARTESIAN_POINT('Ctrl Pts',(-14.6428955274718,3.30308293583232,-3.26377084899469));
#93433=CARTESIAN_POINT('Ctrl Pts',(-14.4450775340346,4.53670822242377,0.99037141534212));
#93434=CARTESIAN_POINT('Ctrl Pts',(-14.2472595405975,1.64242748977322,4.34338450710635));
#93435=CARTESIAN_POINT('Ctrl Pts',(-14.0494415471604,-2.7462817996209,3.7443949194503));
#93436=CARTESIAN_POINT('Ctrl Pts',(-13.8516235537233,-4.63617639444042,
-0.261582635829614));
#93437=CARTESIAN_POINT('Ctrl Pts',(-13.6538055602862,-2.30765986238043,
-4.02954873345547));
#93438=CARTESIAN_POINT('Ctrl Pts',(-13.4559875668491,2.12057359421086,-4.13106822350708));
#93439=CARTESIAN_POINT('Ctrl Pts',(-13.258169573412,4.61931807451703,-0.473769524320169));
#93440=CARTESIAN_POINT('Ctrl Pts',(-13.0603515799749,2.91499064679445,3.61460738737074));
#93441=CARTESIAN_POINT('Ctrl Pts',(-12.8625335865378,-1.44165798983063,
4.41408872544398));
#93442=CARTESIAN_POINT('Ctrl Pts',(-12.6647155931007,-4.48655625544975,
1.19723431391644));
#93443=CARTESIAN_POINT('Ctrl Pts',(-12.4668975996636,-3.44918128141044,
-3.10897177917426));
#93444=CARTESIAN_POINT('Ctrl Pts',(-12.2690796062264,0.726569685736974,
-4.58635514624655));
#93445=CARTESIAN_POINT('Ctrl Pts',(-12.0712616127894,4.24122206948244,-1.89065924827013));
#93446=CARTESIAN_POINT('Ctrl Pts',(-11.8734436193522,3.89682836711986,2.52532883263629));
#93447=CARTESIAN_POINT('Ctrl Pts',(-11.6756256259152,0.00674900812206685,
4.64354514208956));
#93448=CARTESIAN_POINT('Ctrl Pts',(-11.477807632478,-3.88947120673092,2.5366455739313));
#93449=CARTESIAN_POINT('Ctrl Pts',(-11.2799896390409,-4.24669997254704,
-1.8783227568507));
#93450=CARTESIAN_POINT('Ctrl Pts',(-11.0821716456038,-0.739898362341693,
-4.58422375644321));
#93451=CARTESIAN_POINT('Ctrl Pts',(-10.8843536521667,3.44012946251005,-3.11898482152518));
#93452=CARTESIAN_POINT('Ctrl Pts',(-10.6865356587296,4.49001745489969,1.18418760778445));
#93453=CARTESIAN_POINT('Ctrl Pts',(-10.4887176652925,1.45448289642492,4.40987942462621));
#93454=CARTESIAN_POINT('Ctrl Pts',(-10.2908996718554,-2.90447128894164,
3.62306549312152));
#93455=CARTESIAN_POINT('Ctrl Pts',(-10.0930816784183,-4.62067572525506,
-0.460339958913909));
#93456=CARTESIAN_POINT('Ctrl Pts',(-9.89526368498118,-2.13257294053773,
-4.1248866274142));
#93457=CARTESIAN_POINT('Ctrl Pts',(-9.69744569154406,2.29593690721424,-4.03623967992807));
#93458=CARTESIAN_POINT('Ctrl Pts',(-9.49962769810695,4.63539643159623,-0.275058098734038));
#93459=CARTESIAN_POINT('Ctrl Pts',(-9.30180970466984,2.75715450958978,3.73639613076329));
#93460=CARTESIAN_POINT('Ctrl Pts',(-9.10399171123273,-1.62979507844226,
4.34814041148852));
#93461=CARTESIAN_POINT('Ctrl Pts',(-8.90617371779562,-4.53381021607703,
1.00355466235267));
#93462=CARTESIAN_POINT('Ctrl Pts',(-8.70835572435853,-3.31255620183176,
-3.25415556564835));
#93463=CARTESIAN_POINT('Ctrl Pts',(-8.5105377309214,0.922759994555157,-4.55094177376315));
#93464=CARTESIAN_POINT('Ctrl Pts',(-8.31271973748432,4.3184659825949,-1.70687099480464));
#93465=CARTESIAN_POINT('Ctrl Pts',(-8.11490174404719,3.78484241063877,2.69026484985475));
#93466=CARTESIAN_POINT('Ctrl Pts',(-7.91708375061009,-0.192571901822546,
4.63955526945863));
#93467=CARTESIAN_POINT('Ctrl Pts',(-7.71926575717298,-3.99476694213886,
2.36736015716507));
#93468=CARTESIAN_POINT('Ctrl Pts',(-7.52144776373589,-4.1621629833872,-2.05887258844547));
#93469=CARTESIAN_POINT('Ctrl Pts',(-7.32362977029875,-0.542448020392725,
-4.6117574937218));
#93470=CARTESIAN_POINT('Ctrl Pts',(-7.12581177686167,3.57083504060222,-2.96844978879022));
#93471=CARTESIAN_POINT('Ctrl Pts',(-6.92799378342454,4.43505055411778,1.37582107053309));
#93472=CARTESIAN_POINT('Ctrl Pts',(-6.73017578998745,1.2638573571009,4.468245921679));
#93473=CARTESIAN_POINT('Ctrl Pts',(-6.53235779655033,-3.05730717071301,
3.49505792510332));
#93474=CARTESIAN_POINT('Ctrl Pts',(-6.33453980311323,-4.59665808958816,
-0.658248769765227));
#93475=CARTESIAN_POINT('Ctrl Pts',(-6.13672180967612,-1.95355519710399,
-4.21262140803828));
#93476=CARTESIAN_POINT('Ctrl Pts',(-5.938903816239,2.46706828137679,-3.93397141982583));
#93477=CARTESIAN_POINT('Ctrl Pts',(-5.74108582280191,4.6429306883608,-0.0758396777437203));
#93478=CARTESIAN_POINT('Ctrl Pts',(-5.54326782936478,2.59423630389935,3.85129783774972));
#93479=CARTESIAN_POINT('Ctrl Pts',(-5.3454498359277,-1.8149280812755,4.27417747685288));
#93480=CARTESIAN_POINT('Ctrl Pts',(-5.14763184249057,-4.57270732177326,
0.808025227938727));
#93481=CARTESIAN_POINT('Ctrl Pts',(-4.94981384905348,-3.16982532347193,
-3.3933411939276));
#93482=CARTESIAN_POINT('Ctrl Pts',(-4.75199585561636,1.11724945052968,-4.50713997473964));
#93483=CARTESIAN_POINT('Ctrl Pts',(-4.55417786217926,4.38774996024445,-1.51993657804425));
#93484=CARTESIAN_POINT('Ctrl Pts',(-4.35635986874214,3.66588014144792,2.85024207568007));
#93485=CARTESIAN_POINT('Ctrl Pts',(-4.15854187530505,-0.391537897742414,
4.62701366069188));
#93486=CARTESIAN_POINT('Ctrl Pts',(-3.96072388186793,-4.09269932772028,
2.19371109521874));
#93487=CARTESIAN_POINT('Ctrl Pts',(-3.76290588843083,-4.06995431948468,
-2.23562733635738));
#93488=CARTESIAN_POINT('Ctrl Pts',(-3.56508789499372,-0.343997539878338,
-4.63079091104292));
#93489=CARTESIAN_POINT('Ctrl Pts',(-3.36726990155661,3.69495820917957,-2.81244282287592));
#93490=CARTESIAN_POINT('Ctrl Pts',(-3.1694519081195,4.37190987169366,1.56491781598413));
#93491=CARTESIAN_POINT('Ctrl Pts',(-2.9716339146824,1.07090025667334,4.51837787661333));
#93492=CARTESIAN_POINT('Ctrl Pts',(-2.77381592124529,-3.20450393868088,
3.36060536487351));
#93493=CARTESIAN_POINT('Ctrl Pts',(-2.57599792780818,-4.56417502327569,
-0.854938919742906));
#93494=CARTESIAN_POINT('Ctrl Pts',(-2.37817993437107,-1.7709226905566,-4.29260161786294));
#93495=CARTESIAN_POINT('Ctrl Pts',(-2.18036194093397,2.6336256434247,-3.82443230564715));
#93496=CARTESIAN_POINT('Ctrl Pts',(-1.98254394749686,4.64195796464309,0.12348092454259));
#93497=CARTESIAN_POINT('Ctrl Pts',(-1.78472595405975,2.42643865805515,3.95917273074786));
#93498=CARTESIAN_POINT('Ctrl Pts',(-1.58690796062265,-1.9965287407846,4.19219835928893));
#93499=CARTESIAN_POINT('Ctrl Pts',(-1.38908996718554,-4.60353401029951,
0.611270499633702));
#93500=CARTESIAN_POINT('Ctrl Pts',(-1.19127197374843,-3.0205655885075,-3.52677822827127));
#93501=CARTESIAN_POINT('Ctrl Pts',(-0.993453980311325,1.30836214558254,
-4.45405726657038));
#93502=CARTESIAN_POINT('Ctrl Pts',(-0.79563598687421,4.45150143479259,-1.33210124254099));
#93503=CARTESIAN_POINT('Ctrl Pts',(-0.597817993437107,3.53497485386071,
3.00893856288978));
#93504=CARTESIAN_POINT('Ctrl Pts',(-0.465939331145702,0.793490219260556,
4.06671712560122));
#93505=CARTESIAN_POINT('Ctrl Pts',(-0.4,-0.4995344189117,3.90114782651498));
#93506=CARTESIAN_POINT('Ctrl Pts',(-29.5403753524613,2.14656790565209,-3.00907133330607));
#93507=CARTESIAN_POINT('Ctrl Pts',(-29.4744360213156,3.14391626183024,-2.29759734848209));
#93508=CARTESIAN_POINT('Ctrl Pts',(-29.3425573590242,4.35891997496475,0.182352318785631));
#93509=CARTESIAN_POINT('Ctrl Pts',(-29.1447393655871,2.21900816628781,3.76102351955619));
#93510=CARTESIAN_POINT('Ctrl Pts',(-28.94692137215,-1.94188114811691,3.90680600563483));
#93511=CARTESIAN_POINT('Ctrl Pts',(-28.7491033787128,-4.33486087054888,
0.503202133750661));
#93512=CARTESIAN_POINT('Ctrl Pts',(-28.5512853852758,-2.78412230131377,
-3.36104151790357));
#93513=CARTESIAN_POINT('Ctrl Pts',(-28.3534673918386,1.30013792313657,-4.16565726419232));
#93514=CARTESIAN_POINT('Ctrl Pts',(-28.1556493984015,4.2012711989092,-1.18073922268235));
#93515=CARTESIAN_POINT('Ctrl Pts',(-27.9578314049644,3.27978464833425,2.87891689675649));
#93516=CARTESIAN_POINT('Ctrl Pts',(-27.7600134115273,-0.62598492731999,
4.31886860767985));
#93517=CARTESIAN_POINT('Ctrl Pts',(-27.5621954180902,-3.96215644422926,
1.82923218063347));
#93518=CARTESIAN_POINT('Ctrl Pts',(-27.3643774246531,-3.69321166658437,
-2.32486082884581));
#93519=CARTESIAN_POINT('Ctrl Pts',(-27.166559431216,-0.0638444516104365,
-4.36355653062925));
#93520=CARTESIAN_POINT('Ctrl Pts',(-26.9687414377789,3.62361127167989,-2.43191057898122));
#93521=CARTESIAN_POINT('Ctrl Pts',(-26.7709234443418,4.01398040500783,1.71251481465396));
#93522=CARTESIAN_POINT('Ctrl Pts',(-26.5731054509047,0.752067600526557,
4.29873569959576));
#93523=CARTESIAN_POINT('Ctrl Pts',(-26.3752874574676,-3.19414367121133,
2.97358160094932));
#93524=CARTESIAN_POINT('Ctrl Pts',(-26.1774694640304,-4.23403537110954,
-1.05720617932359));
#93525=CARTESIAN_POINT('Ctrl Pts',(-25.9796514705933,-1.42141997703747,
-4.12605189872662));
#93526=CARTESIAN_POINT('Ctrl Pts',(-25.7818334771563,2.6845313606068,-3.44064404477171));
#93527=CARTESIAN_POINT('Ctrl Pts',(-25.5840154837191,4.34785414948105,0.375372017642794));
#93528=CARTESIAN_POINT('Ctrl Pts',(-25.3861974902821,2.05510735926432,3.84984070240973));
#93529=CARTESIAN_POINT('Ctrl Pts',(-25.1883794968449,-2.10756131796558,
3.82137738710818));
#93530=CARTESIAN_POINT('Ctrl Pts',(-24.9905615034079,-4.35258076501138,
0.31588049375982));
#93531=CARTESIAN_POINT('Ctrl Pts',(-24.7927435099707,-2.63722994605843,
-3.47703292997124));
#93532=CARTESIAN_POINT('Ctrl Pts',(-24.5949255165336,1.47771036141024,-4.10622842687727));
#93533=CARTESIAN_POINT('Ctrl Pts',(-24.3971075230965,4.2480966015586,-0.999207216946258));
#93534=CARTESIAN_POINT('Ctrl Pts',(-24.1992895296594,3.15318168640843,3.01698277247436));
#93535=CARTESIAN_POINT('Ctrl Pts',(-24.0014715362223,-0.810782112682527,
4.28804992573688));
#93536=CARTESIAN_POINT('Ctrl Pts',(-23.8036535427852,-4.03702327263912,
1.65746278836132));
#93537=CARTESIAN_POINT('Ctrl Pts',(-23.6058355493481,-3.59001681556988,
-2.48123337524934));
#93538=CARTESIAN_POINT('Ctrl Pts',(-23.4080175559109,0.123510496601368,
-4.36227978884321));
#93539=CARTESIAN_POINT('Ctrl Pts',(-23.2101995624739,3.72465682738561,-2.27413089265649));
#93540=CARTESIAN_POINT('Ctrl Pts',(-23.0123815690367,3.93677468562862,1.88322724951672));
#93541=CARTESIAN_POINT('Ctrl Pts',(-22.8145635755996,0.566860126431276,
4.32705551106549));
#93542=CARTESIAN_POINT('Ctrl Pts',(-22.6167455821625,-3.31883486502011,
2.83373868546072));
#93543=CARTESIAN_POINT('Ctrl Pts',(-22.4189275887254,-4.18475478068498,
-1.23796899165007));
#93544=CARTESIAN_POINT('Ctrl Pts',(-22.2211095952883,-1.2430076387999,-4.18326090611671));
#93545=CARTESIAN_POINT('Ctrl Pts',(-22.0232916018512,2.82973988102568,-3.32224502475171));
#93546=CARTESIAN_POINT('Ctrl Pts',(-21.8254736084141,4.32773502201412,0.561648803068342));
#93547=CARTESIAN_POINT('Ctrl Pts',(-21.627655614977,1.88796679555549,3.93450393031146));
#93548=CARTESIAN_POINT('Ctrl Pts',(-21.4298376215398,-2.26964377769154,
3.72739277795376));
#93549=CARTESIAN_POINT('Ctrl Pts',(-21.2320196281028,-4.362127886521,0.128763738652503));
#93550=CARTESIAN_POINT('Ctrl Pts',(-21.0342016346657,-2.48555490006003,
-3.58702615512398));
#93551=CARTESIAN_POINT('Ctrl Pts',(-20.8363836412285,1.65259994930344,-4.03901636618597));
#93552=CARTESIAN_POINT('Ctrl Pts',(-20.6385656477914,4.28707042143268,-0.815945464129155));
#93553=CARTESIAN_POINT('Ctrl Pts',(-20.4407476543543,3.02077784468951,3.14954615965363));
#93554=CARTESIAN_POINT('Ctrl Pts',(-20.2429296609173,-0.994090667850735,
4.24929682922339));
#93555=CARTESIAN_POINT('Ctrl Pts',(-20.0451116674801,-4.10444589668216,
1.48265426852147));
#93556=CARTESIAN_POINT('Ctrl Pts',(-19.847293674043,-3.48020632860252,-2.63304077239811));
#93557=CARTESIAN_POINT('Ctrl Pts',(-19.6494756806059,0.310638616705305,
-4.35295801134899));
#93558=CARTESIAN_POINT('Ctrl Pts',(-19.4516576871688,3.81883655170536,-2.1121617338914));
#93559=CARTESIAN_POINT('Ctrl Pts',(-19.2538396937317,3.85231281287818,2.05046965119956));
#93560=CARTESIAN_POINT('Ctrl Pts',(-19.0560217002946,0.380607680704291,
4.34739894559319));
#93561=CARTESIAN_POINT('Ctrl Pts',(-18.8582037068575,-3.43740862228359,
2.68867286262318));
#93562=CARTESIAN_POINT('Ctrl Pts',(-18.6603857134204,-4.12776075846771,
-1.41645011193827));
#93563=CARTESIAN_POINT('Ctrl Pts',(-18.4625677199833,-1.06230413519704,
-4.23275911470275));
#93564=CARTESIAN_POINT('Ctrl Pts',(-18.2647497265461,2.96973253222793,-3.19772239035583));
#93565=CARTESIAN_POINT('Ctrl Pts',(-18.066931733109,4.29963888967826,0.74689036486102));
#93566=CARTESIAN_POINT('Ctrl Pts',(-17.8691137396719,1.71734627309193,4.01191495137338));
#93567=CARTESIAN_POINT('Ctrl Pts',(-17.6712957462348,-2.42754276148306,
3.6265377345241));
#93568=CARTESIAN_POINT('Ctrl Pts',(-17.4734777527977,-4.36363460527469,
-0.0585903610256284));
#93569=CARTESIAN_POINT('Ctrl Pts',(-17.2756597593606,-2.32929840525822,
-3.69040766555911));
#93570=CARTESIAN_POINT('Ctrl Pts',(-17.0778417659235,1.8244434158099,-3.96435947175124));
#93571=CARTESIAN_POINT('Ctrl Pts',(-16.8800237724864,4.31814218613394,-0.63117973595981));
#93572=CARTESIAN_POINT('Ctrl Pts',(-16.6822057790493,2.88280601566515,3.2763042097462));
#93573=CARTESIAN_POINT('Ctrl Pts',(-16.4843877856122,-1.17556688561053,
4.20271130298191));
#93574=CARTESIAN_POINT('Ctrl Pts',(-16.2865697921751,-4.1643030844093,1.30511287631955));
#93575=CARTESIAN_POINT('Ctrl Pts',(-16.088751798738,-3.36398102217285,-2.77999487071771));
#93576=CARTESIAN_POINT('Ctrl Pts',(-15.8909338053009,0.497194158500287,
-4.33561273264911));
#93577=CARTESIAN_POINT('Ctrl Pts',(-15.6931158118637,3.90597728330769,-1.94629937600571));
#93578=CARTESIAN_POINT('Ctrl Pts',(-15.4952978184266,3.76075024297067,2.21393256644188));
#93579=CARTESIAN_POINT('Ctrl Pts',(-15.2974798249895,0.193653687619838,
4.35972912553373));
#93580=CARTESIAN_POINT('Ctrl Pts',(-15.0996618315524,-3.54964644609277,
2.53865119827378));
#93581=CARTESIAN_POINT('Ctrl Pts',(-14.9018438381153,-4.06315832527685,
-1.59232038939699));
#93582=CARTESIAN_POINT('Ctrl Pts',(-14.7040258446782,-0.879642561126436,
-4.27445537623342));
#93583=CARTESIAN_POINT('Ctrl Pts',(-14.5062078512411,3.10425128440637,-3.06730561927196));
#93584=CARTESIAN_POINT('Ctrl Pts',(-14.308389857804,4.26361753550314,0.930755236195858));
#93585=CARTESIAN_POINT('Ctrl Pts',(-14.1105718643669,1.5435602870771,4.08193109188707));
#93586=CARTESIAN_POINT('Ctrl Pts',(-13.9127538709298,-2.58096722650616,
3.51899814925455));
#93587=CARTESIAN_POINT('Ctrl Pts',(-13.7149358774927,-4.35709814338938,
-0.245836465213632));
#93588=CARTESIAN_POINT('Ctrl Pts',(-13.5171178840556,-2.16874847859741,
-3.78698690720437));
#93589=CARTESIAN_POINT('Ctrl Pts',(-13.3192998906185,1.99292401413727,-3.88239535243784));
#93590=CARTESIAN_POINT('Ctrl Pts',(-13.1214818971814,4.34125462317152,-0.445250598593546));
#93591=CARTESIAN_POINT('Ctrl Pts',(-12.9236639037442,2.73952051314873,3.39702327881237));
#93592=CARTESIAN_POINT('Ctrl Pts',(-12.7258459103071,-1.3548762636439,4.14837921470184));
#93593=CARTESIAN_POINT('Ctrl Pts',(-12.52802791687,-4.21648450526471,1.12516586138155));
#93594=CARTESIAN_POINT('Ctrl Pts',(-12.3302099234329,-3.24155512621748,
-2.9218248000948));
#93595=CARTESIAN_POINT('Ctrl Pts',(-12.1323919299958,0.682833257285865,
-4.3102759240564));
#93596=CARTESIAN_POINT('Ctrl Pts',(-11.9345739365587,3.98591840181145,-1.77684954142345));
#93597=CARTESIAN_POINT('Ctrl Pts',(-11.7367559431216,3.66225574674975,2.37331469555857));
#93598=CARTESIAN_POINT('Ctrl Pts',(-11.5389379496845,0.00634274631863393,
4.36402332353129));
#93599=CARTESIAN_POINT('Ctrl Pts',(-11.3411199562474,-3.65534145636389,
2.38395021679216));
#93600=CARTESIAN_POINT('Ctrl Pts',(-11.1433019628103,-3.99106655823213,
-1.76525565471889));
#93601=CARTESIAN_POINT('Ctrl Pts',(-10.9454839693732,-0.695359603815275,
-4.30827283492326));
#93602=CARTESIAN_POINT('Ctrl Pts',(-10.7476659759361,3.23304818860991,-2.93123509955822));
#93603=CARTESIAN_POINT('Ctrl Pts',(-10.5498479824989,4.21973735511645,1.11290451189252));
#93604=CARTESIAN_POINT('Ctrl Pts',(-10.3520299890619,1.36692916499126,4.14442329602711));
#93605=CARTESIAN_POINT('Ctrl Pts',(-10.1542119956247,-2.72963437623965,
3.40497224229606));
#93606=CARTESIAN_POINT('Ctrl Pts',(-9.95639400218764,-4.34253054906534,
-0.432629436342625));
#93607=CARTESIAN_POINT('Ctrl Pts',(-9.75857600875052,-2.00420105046087,
-3.87658586233912));
#93608=CARTESIAN_POINT('Ctrl Pts',(-9.56075801531341,2.1577311958532,-3.79327508693977));
#93609=CARTESIAN_POINT('Ctrl Pts',(-9.36294002187631,4.35636513101642,-0.25850076212705));
#93610=CARTESIAN_POINT('Ctrl Pts',(-9.16512202843919,2.59118544522533,3.51148085388605));
#93611=CARTESIAN_POINT('Ctrl Pts',(-8.9673040350021,-1.53168829359069,4.08640071089866));
#93612=CARTESIAN_POINT('Ctrl Pts',(-8.76948604156497,-4.26089397690688,
0.943144907378862));
#93613=CARTESIAN_POINT('Ctrl Pts',(-8.57166804812789,-3.11315429977641,
-3.05826913539988));
#93614=CARTESIAN_POINT('Ctrl Pts',(-8.37385005469076,0.867213737572975,
-4.2769942871274));
#93615=CARTESIAN_POINT('Ctrl Pts',(-8.17603206125366,4.05851255737768,-1.60412456510211));
#93616=CARTESIAN_POINT('Ctrl Pts',(-7.97821406781655,3.55701087219007,2.52832226068538));
#93617=CARTESIAN_POINT('Ctrl Pts',(-7.78039607437944,-0.180979886120416,
4.3602736243927));
#93618=CARTESIAN_POINT('Ctrl Pts',(-7.58257808094234,-3.75429883292162,
2.22485506761286));
#93619=CARTESIAN_POINT('Ctrl Pts',(-7.38476008750524,-3.91161833901473,
-1.93493714849773));
#93620=CARTESIAN_POINT('Ctrl Pts',(-7.18694209406812,-0.509794939073633,
-4.33414915742924));
#93621=CARTESIAN_POINT('Ctrl Pts',(-6.98912410063102,3.35588584256953,-2.78976164043119));
#93622=CARTESIAN_POINT('Ctrl Pts',(-6.7913061071939,4.168079229763,1.29300244901041));
#93623=CARTESIAN_POINT('Ctrl Pts',(-6.59348811375681,1.18777847856196,4.1992763763046));
#93624=CARTESIAN_POINT('Ctrl Pts',(-6.39567012031969,-2.87327018300228,
3.28467018959145));
#93625=CARTESIAN_POINT('Ctrl Pts',(-6.19785212688259,-4.31995867369443,
-0.618624972093756));
#93626=CARTESIAN_POINT('Ctrl Pts',(-6.00003413344547,-1.83595941960225,
-3.95903937947152));
#93627=CARTESIAN_POINT('Ctrl Pts',(-5.80221614000837,2.31856118358479,-3.69716294445239));
#93628=CARTESIAN_POINT('Ctrl Pts',(-5.60439814657126,4.36344585732357,-0.0712744492398178));
#93629=CARTESIAN_POINT('Ctrl Pts',(-5.40658015313416,2.43807422788913,3.61946596307714));
#93630=CARTESIAN_POINT('Ctrl Pts',(-5.20876215969704,-1.70567707104362,
4.01689003275298));
#93631=CARTESIAN_POINT('Ctrl Pts',(-5.01094416625994,-4.29744964101308,
0.7593855196462));
#93632=CARTESIAN_POINT('Ctrl Pts',(-4.81312617282283,-2.9790152178701,-3.18907637631703));
#93633=CARTESIAN_POINT('Ctrl Pts',(-4.61530817938572,1.04999574917882,-4.23582917153099));
#93634=CARTESIAN_POINT('Ctrl Pts',(-4.41749018594862,4.12362593199937,-1.42844281123723));
#93635=CARTESIAN_POINT('Ctrl Pts',(-4.21967219251151,3.44520962950086,2.67866953273136));
#93636=CARTESIAN_POINT('Ctrl Pts',(-4.0218541990744,-0.367968968861021,
4.34848696753938));
#93637=CARTESIAN_POINT('Ctrl Pts',(-3.8240362056373,-3.84633610223394,2.06165894627568));
#93638=CARTESIAN_POINT('Ctrl Pts',(-3.62621821220018,-3.82496024749434,
-2.10105200661351));
#93639=CARTESIAN_POINT('Ctrl Pts',(-3.42840021876308,-0.323290339886936,
-4.35203684336192));
#93640=CARTESIAN_POINT('Ctrl Pts',(-3.23058222532597,3.47253732028477,-2.64314563540684));
#93641=CARTESIAN_POINT('Ctrl Pts',(-3.03276423188886,4.10873934992313,1.47071636850529));
#93642=CARTESIAN_POINT('Ctrl Pts',(-2.83494623845175,1.00643658116675,4.24639059914366));
#93643=CARTESIAN_POINT('Ctrl Pts',(-2.63712824501465,-3.0116063268114,3.15831110600399));
#93644=CARTESIAN_POINT('Ctrl Pts',(-2.43931025157754,-4.28943095087281,
-0.803475205212229));
#93645=CARTESIAN_POINT('Ctrl Pts',(-2.24149225814043,-1.6643206191126,-4.03420511823695));
#93646=CARTESIAN_POINT('Ctrl Pts',(-2.04367426470332,2.47509249542551,-3.59421762261588));
#93647=CARTESIAN_POINT('Ctrl Pts',(-1.84585627126622,4.36253168746809,0.11604789406065));
#93648=CARTESIAN_POINT('Ctrl Pts',(-1.64803827782911,2.28037729210179,3.72084724282401));
#93649=CARTESIAN_POINT('Ctrl Pts',(-1.45022028439201,-1.87634613733157,
3.93984571205739));
#93650=CARTESIAN_POINT('Ctrl Pts',(-1.25240229095489,-4.32642069300014,
0.574474595543115));
#93651=CARTESIAN_POINT('Ctrl Pts',(-1.05458429751779,-2.83874028897046,
-3.31448106439046));
#93652=CARTESIAN_POINT('Ctrl Pts',(-0.856766304080679,1.22960426661822,
-4.18594181834751));
#93653=CARTESIAN_POINT('Ctrl Pts',(-0.658948310643567,4.18353983685536,
-1.2519143701353));
#93654=CARTESIAN_POINT('Ctrl Pts',(-0.461130317206463,3.32218428771488,
2.82781316122078));
#93655=CARTESIAN_POINT('Ctrl Pts',(-0.329251654915058,0.745725457142593,
3.82191791901945));
#93656=CARTESIAN_POINT('Ctrl Pts',(-0.263312323769356,-0.469464555276475,
3.66631519292041));
#93657=CARTESIAN_POINT('Ctrl Pts',(-29.4036876762306,2.00907721869555,-2.81633609132833));
#93658=CARTESIAN_POINT('Ctrl Pts',(-29.3377483450849,2.94254401293249,-2.1504330137501));
#93659=CARTESIAN_POINT('Ctrl Pts',(-29.2058696827936,4.07972503304445,0.170672396845149));
#93660=CARTESIAN_POINT('Ctrl Pts',(-29.0080516893564,2.0768775789713,3.52012468472226));
#93661=CARTESIAN_POINT('Ctrl Pts',(-28.8102336959193,-1.81750093524801,
3.65656959796921));
#93662=CARTESIAN_POINT('Ctrl Pts',(-28.6124157024822,-4.05720694803216,
0.470971330865179));
#93663=CARTESIAN_POINT('Ctrl Pts',(-28.4145977090451,-2.60579536053973,
-3.14576209163));
#93664=CARTESIAN_POINT('Ctrl Pts',(-28.216779715608,1.21686226448183,-3.89884107013144));
#93665=CARTESIAN_POINT('Ctrl Pts',(-28.0189617221709,3.93217388234734,-1.10511121836174));
#93666=CARTESIAN_POINT('Ctrl Pts',(-27.8211437287338,3.06970983859651,2.69451822910493));
#93667=CARTESIAN_POINT('Ctrl Pts',(-27.6233257352967,-0.585889714186953,
4.04223901204422));
#93668=CARTESIAN_POINT('Ctrl Pts',(-27.4255077418596,-3.70837476329012,
1.712067292229));
#93669=CARTESIAN_POINT('Ctrl Pts',(-27.2276897484225,-3.45665627610379,
-2.1759502299336));
#93670=CARTESIAN_POINT('Ctrl Pts',(-27.0298717549854,-0.0597551248823223,
-4.08406461081147));
#93671=CARTESIAN_POINT('Ctrl Pts',(-26.8320537615482,3.39151388417357,-2.27614329333393));
#93672=CARTESIAN_POINT('Ctrl Pts',(-26.6342357681111,3.75687932664852,1.60282583734741));
#93673=CARTESIAN_POINT('Ctrl Pts',(-26.436417774674,0.703896615223974,4.02339564497843));
#93674=CARTESIAN_POINT('Ctrl Pts',(-26.2385997812369,-2.98955428625109,
2.78311952613708));
#93675=CARTESIAN_POINT('Ctrl Pts',(-26.0407817877998,-3.96283946333539,
-0.989490639802492));
#93676=CARTESIAN_POINT('Ctrl Pts',(-25.8429637943627,-1.33037603261715,
-3.86177248390795));
#93677=CARTESIAN_POINT('Ctrl Pts',(-25.6451458009256,2.51258335935589,-3.22026596493412));
#93678=CARTESIAN_POINT('Ctrl Pts',(-25.4473278074885,4.0693679892133,0.351328913097125));
#93679=CARTESIAN_POINT('Ctrl Pts',(-25.2495098140513,1.92347484866417,3.60325300236361));
#93680=CARTESIAN_POINT('Ctrl Pts',(-25.0516918206143,-1.97256905769413,
3.57661280235394));
#93681=CARTESIAN_POINT('Ctrl Pts',(-24.8538738271771,-4.07379185838536,
0.2956479048122));
#93682=CARTESIAN_POINT('Ctrl Pts',(-24.65605583374,-2.46831166679449,-3.25432409096666));
#93683=CARTESIAN_POINT('Ctrl Pts',(-24.458237840303,1.38306093887013,-3.84321873325179));
#93684=CARTESIAN_POINT('Ctrl Pts',(-24.2604198468658,3.97600005223996,-0.935206592364037));
#93685=CARTESIAN_POINT('Ctrl Pts',(-24.0626018534288,2.9512159740629,2.82374079171459));
#93686=CARTESIAN_POINT('Ctrl Pts',(-23.8647838599916,-0.758850380473512,
4.01339430993215));
#93687=CARTESIAN_POINT('Ctrl Pts',(-23.6669658665545,-3.77844626626852,
1.55129997060155));
#93688=CARTESIAN_POINT('Ctrl Pts',(-23.4691478731174,-3.36007120012553,
-2.32230689527902));
#93689=CARTESIAN_POINT('Ctrl Pts',(-23.2713298796803,0.115599475953315,
-4.08286964612867));
#93690=CARTESIAN_POINT('Ctrl Pts',(-23.0735118862432,3.48608733022402,-2.12846961735411));
#93691=CARTESIAN_POINT('Ctrl Pts',(-22.8756938928061,3.68461874194987,1.76260390117095));
#93692=CARTESIAN_POINT('Ctrl Pts',(-22.677875899369,0.530551939773822,4.0499015327781));
#93693=CARTESIAN_POINT('Ctrl Pts',(-22.4800579059319,-3.10625883409863,
2.65223374564798));
#93694=CARTESIAN_POINT('Ctrl Pts',(-22.2822399124948,-3.91671536389035,
-1.158675340308));
#93695=CARTESIAN_POINT('Ctrl Pts',(-22.0844219190576,-1.16339125503638,
-3.91531717408475));
#93696=CARTESIAN_POINT('Ctrl Pts',(-21.8866039256206,2.64849107024913,-3.10945056831344));
#93697=CARTESIAN_POINT('Ctrl Pts',(-21.6887859321834,4.05053752009681,0.52567440898612));
#93698=CARTESIAN_POINT('Ctrl Pts',(-21.4909679387464,1.76703987263422,3.68249343169766));
#93699=CARTESIAN_POINT('Ctrl Pts',(-21.2931499453092,-2.12426990840011,
3.4886480393185));
#93700=CARTESIAN_POINT('Ctrl Pts',(-21.0953319518721,-4.08272747336339,
0.120516240478409));
#93701=CARTESIAN_POINT('Ctrl Pts',(-20.897513958435,-2.32635162036054,-3.35727209567843));
#93702=CARTESIAN_POINT('Ctrl Pts',(-20.6996959649979,1.54674860321008,-3.7803116993765));
#93703=CARTESIAN_POINT('Ctrl Pts',(-20.5018779715608,4.01247754425332,-0.763683012013472));
#93704=CARTESIAN_POINT('Ctrl Pts',(-20.3040599781237,2.82729278422816,2.94781330789901));
#93705=CARTESIAN_POINT('Ctrl Pts',(-20.1062419846866,-0.930417765418907,
3.97712340363837));
#93706=CARTESIAN_POINT('Ctrl Pts',(-19.9084239912495,-3.84155037661736,
1.38768818179236));
#93707=CARTESIAN_POINT('Ctrl Pts',(-19.7106059978124,-3.2572942289619,-2.46439081558641));
#93708=CARTESIAN_POINT('Ctrl Pts',(-19.5127880043753,0.290741777339739,
-4.0741449415656));
#93709=CARTESIAN_POINT('Ctrl Pts',(-19.3149700109381,3.5742347110246,-1.97687481052344));
#93710=CARTESIAN_POINT('Ctrl Pts',(-19.117152017501,3.60556677068707,1.91913419230974));
#93711=CARTESIAN_POINT('Ctrl Pts',(-18.9193340240639,0.356229224591542,
4.06894194177332));
#93712=CARTESIAN_POINT('Ctrl Pts',(-18.7215160306268,-3.21723777579712,
2.51645959235574));
#93713=CARTESIAN_POINT('Ctrl Pts',(-18.5236980371897,-3.86337188878432,
-1.32572449435251));
#93714=CARTESIAN_POINT('Ctrl Pts',(-18.3258800437526,-0.994262064447525,
-3.96164495294261));
#93715=CARTESIAN_POINT('Ctrl Pts',(-18.1280620503155,2.77951699566927,-2.99290378341184));
#93716=CARTESIAN_POINT('Ctrl Pts',(-17.9302440568784,4.02424098446856,0.69905098876881));
#93717=CARTESIAN_POINT('Ctrl Pts',(-17.7324260634413,1.60734783409173,3.75494616821811));
#93718=CARTESIAN_POINT('Ctrl Pts',(-17.5346080700042,-2.27205524067654,
3.39425290296547));
#93719=CARTESIAN_POINT('Ctrl Pts',(-17.3367900765671,-4.08413768466629,
-0.0548375661733324));
#93720=CARTESIAN_POINT('Ctrl Pts',(-17.13897208313,-2.18010357334888,-3.45403187527947));
#93721=CARTESIAN_POINT('Ctrl Pts',(-16.9411540896928,1.70758525451319,-3.71043668380749));
#93722=CARTESIAN_POINT('Ctrl Pts',(-16.7433360962558,4.04155911881782,-0.590751788042732));
#93723=CARTESIAN_POINT('Ctrl Pts',(-16.5455181028186,2.6981582444893,3.06645232698464));
#93724=CARTESIAN_POINT('Ctrl Pts',(-16.3477001093816,-1.10027017673849,
3.93352174573308));
#93725=CARTESIAN_POINT('Ctrl Pts',(-16.1498821159444,-3.89757362746404,
1.22151856493134));
#93726=CARTESIAN_POINT('Ctrl Pts',(-15.9520641225073,-3.14851331652539,
-2.60193229766599));
#93727=CARTESIAN_POINT('Ctrl Pts',(-15.7542461290702,0.465348174861481,
-4.05791065230967));
#93728=CARTESIAN_POINT('Ctrl Pts',(-15.5564281356331,3.65579395647019,-1.82163616943977));
#93729=CARTESIAN_POINT('Ctrl Pts',(-15.358610142196,3.51986891188557,2.07212707841885));
#93730=CARTESIAN_POINT('Ctrl Pts',(-15.1607921487589,0.181249897144626,
4.08048235638389));
#93731=CARTESIAN_POINT('Ctrl Pts',(-14.9629741553218,-3.3222866094712,2.37604702615573));
#93732=CARTESIAN_POINT('Ctrl Pts',(-14.7651561618847,-3.80290733210558,
-1.49033003371495));
#93733=CARTESIAN_POINT('Ctrl Pts',(-14.5673381684476,-0.823300220552425,
-4.00067051040366));
#93734=CARTESIAN_POINT('Ctrl Pts',(-14.3695201750105,2.90541963298041,-2.87084038954923));
#93735=CARTESIAN_POINT('Ctrl Pts',(-14.1717021815733,3.99052684858251,0.871139057049595));
#93736=CARTESIAN_POINT('Ctrl Pts',(-13.9738841881363,1.44469308438099,3.8204776766678));
#93737=CARTESIAN_POINT('Ctrl Pts',(-13.7760661946991,-2.41565265339143,
3.29360137905881));
#93738=CARTESIAN_POINT('Ctrl Pts',(-13.5782482012621,-4.07801989233833,
-0.230090294597647));
#93739=CARTESIAN_POINT('Ctrl Pts',(-13.3804302078249,-2.02983709481441,
-3.54442508095327));
#93740=CARTESIAN_POINT('Ctrl Pts',(-13.1826122143878,1.86527443406369,-3.63372248136861));
#93741=CARTESIAN_POINT('Ctrl Pts',(-12.9847942209507,4.063191171826,-0.416731672866926));
#93742=CARTESIAN_POINT('Ctrl Pts',(-12.7869762275136,2.56405037950302,3.17943917025402));
#93743=CARTESIAN_POINT('Ctrl Pts',(-12.5891582340765,-1.26809453745718,
3.88266970395969));
#93744=CARTESIAN_POINT('Ctrl Pts',(-12.3913402406394,-3.94641275507968,
1.05309740884666));
#93745=CARTESIAN_POINT('Ctrl Pts',(-12.1935222472023,-3.03392897102452,
-2.73467782101535));
#93746=CARTESIAN_POINT('Ctrl Pts',(-11.9957042537652,0.639096828834754,
-4.03419670186625));
#93747=CARTESIAN_POINT('Ctrl Pts',(-11.797886260328,3.73061473414047,-1.66303983457679));
#93748=CARTESIAN_POINT('Ctrl Pts',(-11.600068266891,3.42768312637964,2.22130055848087));
#93749=CARTESIAN_POINT('Ctrl Pts',(-11.4022502734538,0.00593648451520102,
4.08450150497301));
#93750=CARTESIAN_POINT('Ctrl Pts',(-11.2044322800167,-3.42121170599686,
2.23125485965302));
#93751=CARTESIAN_POINT('Ctrl Pts',(-11.0066142865796,-3.73543314391723,
-1.65218855258708));
#93752=CARTESIAN_POINT('Ctrl Pts',(-10.8087962931425,-0.650820845288858,
-4.03232191340333));
#93753=CARTESIAN_POINT('Ctrl Pts',(-10.6109782997054,3.02596691470977,-2.74348537759124));
#93754=CARTESIAN_POINT('Ctrl Pts',(-10.4131603062683,3.9494572553332,1.04162141600058));
#93755=CARTESIAN_POINT('Ctrl Pts',(-10.2153423128312,1.2793754335576,3.87896716742802));
#93756=CARTESIAN_POINT('Ctrl Pts',(-10.0175243193941,-2.55479746353766,
3.1868789914706));
#93757=CARTESIAN_POINT('Ctrl Pts',(-9.81970632595699,-4.06438537287563,
-0.404918913771338));
#93758=CARTESIAN_POINT('Ctrl Pts',(-9.62188833251988,-1.875829160384,-3.62828509726404));
#93759=CARTESIAN_POINT('Ctrl Pts',(-9.42407033908277,2.01952548449217,-3.55031049395147));
#93760=CARTESIAN_POINT('Ctrl Pts',(-9.22625234564567,4.0773338304366,-0.241943425520061));
#93761=CARTESIAN_POINT('Ctrl Pts',(-9.02843435220854,2.42521638086088,3.2865655770088));
#93762=CARTESIAN_POINT('Ctrl Pts',(-8.83061635877145,-1.43358150873913,
3.82466101030881));
#93763=CARTESIAN_POINT('Ctrl Pts',(-8.63279836533434,-3.98797773773671,
0.88273515240505));
#93764=CARTESIAN_POINT('Ctrl Pts',(-8.43498037189723,-2.91375239772107,
-2.8623827051514));
#93765=CARTESIAN_POINT('Ctrl Pts',(-8.23716237846012,0.811667480590791,
-4.00304680049164));
#93766=CARTESIAN_POINT('Ctrl Pts',(-8.03934438502302,3.79855913216046,-1.5013781353996));
#93767=CARTESIAN_POINT('Ctrl Pts',(-7.84152639158591,3.32917933374137,2.36637967151602));
#93768=CARTESIAN_POINT('Ctrl Pts',(-7.6437083981488,-0.169387870418285,
4.08099197932676));
#93769=CARTESIAN_POINT('Ctrl Pts',(-7.4458904047117,-3.51383072370439,2.08234997806065));
#93770=CARTESIAN_POINT('Ctrl Pts',(-7.24807241127459,-3.66107369464226,
-1.81100170854999));
#93771=CARTESIAN_POINT('Ctrl Pts',(-7.05025441783748,-0.477141857754542,
-4.05654082113668));
#93772=CARTESIAN_POINT('Ctrl Pts',(-6.85243642440037,3.14093664453684,-2.61107349207216));
#93773=CARTESIAN_POINT('Ctrl Pts',(-6.65461843096327,3.90110790540821,1.21018382748773));
#93774=CARTESIAN_POINT('Ctrl Pts',(-6.45680043752616,1.11169960002302,3.9303068309302));
#93775=CARTESIAN_POINT('Ctrl Pts',(-6.25898244408904,-2.68923319529155,
3.07428245407957));
#93776=CARTESIAN_POINT('Ctrl Pts',(-6.06116445065195,-4.04325925780071,
-0.579001174422278));
#93777=CARTESIAN_POINT('Ctrl Pts',(-5.86334645721482,-1.7183636421005,-3.70545735090477));
#93778=CARTESIAN_POINT('Ctrl Pts',(-5.66552846377773,2.17005408579278,-3.46035446907894));
#93779=CARTESIAN_POINT('Ctrl Pts',(-5.46771047034061,4.08396102628634,-0.0667092207359237));
#93780=CARTESIAN_POINT('Ctrl Pts',(-5.26989247690351,2.28191215187892,3.38763408840457));
#93781=CARTESIAN_POINT('Ctrl Pts',(-5.0720744834664,-1.59642606081174,3.75960258865307));
#93782=CARTESIAN_POINT('Ctrl Pts',(-4.87425649002929,-4.02219196025289,
0.710745811353679));
#93783=CARTESIAN_POINT('Ctrl Pts',(-4.67643849659218,-2.78820511226827,
-2.98481155870647));
#93784=CARTESIAN_POINT('Ctrl Pts',(-4.47862050315508,0.982742047827972,
-3.96451836832234));
#93785=CARTESIAN_POINT('Ctrl Pts',(-4.28080250971797,3.8595019037543,-1.33694904443022));
#93786=CARTESIAN_POINT('Ctrl Pts',(-4.08298451628086,3.22453911755379,2.50709698978266));
#93787=CARTESIAN_POINT('Ctrl Pts',(-3.88516652284376,-0.34440003997963,
4.06996027438687));
#93788=CARTESIAN_POINT('Ctrl Pts',(-3.68734852940665,-3.5999728767476,1.92960679733263));
#93789=CARTESIAN_POINT('Ctrl Pts',(-3.48953053596953,-3.579966175504,-1.96647667686965));
#93790=CARTESIAN_POINT('Ctrl Pts',(-3.29171254253244,-0.302583139895528,
-4.0732827756809));
#93791=CARTESIAN_POINT('Ctrl Pts',(-3.09389454909532,3.25011643138997,-2.47384844793777));
#93792=CARTESIAN_POINT('Ctrl Pts',(-2.89607655565822,3.8455688281526,1.37651492102646));
#93793=CARTESIAN_POINT('Ctrl Pts',(-2.69825856222111,0.941972905660164,
3.97440332167399));
#93794=CARTESIAN_POINT('Ctrl Pts',(-2.50044056878401,-2.81870871494191,
2.95601684713447));
#93795=CARTESIAN_POINT('Ctrl Pts',(-2.30262257534689,-4.01468687846993,
-0.752011490681563));
#93796=CARTESIAN_POINT('Ctrl Pts',(-2.10480458190979,-1.55771854766859,
-3.77580861861094));
#93797=CARTESIAN_POINT('Ctrl Pts',(-1.90698658847268,2.31655934742633,-3.36400293958462));
#93798=CARTESIAN_POINT('Ctrl Pts',(-1.70916859503557,4.0831054102931,0.108614863578718));
#93799=CARTESIAN_POINT('Ctrl Pts',(-1.51135060159846,2.13431592614843,3.48252175490014));
#93800=CARTESIAN_POINT('Ctrl Pts',(-1.31353260816136,-1.75616353387854,
3.68749306482585));
#93801=CARTESIAN_POINT('Ctrl Pts',(-1.11571461472425,-4.04930737570077,
0.537678691452524));
#93802=CARTESIAN_POINT('Ctrl Pts',(-0.917896621287142,-2.65691498943343,
-3.10218390050965));
#93803=CARTESIAN_POINT('Ctrl Pts',(-0.720078627850037,1.1508463876539,-3.91782637012465));
#93804=CARTESIAN_POINT('Ctrl Pts',(-0.522260634412922,3.91557823891813,
-1.17172749772961));
#93805=CARTESIAN_POINT('Ctrl Pts',(-0.324442640975819,3.10939372156906,
2.64668775955179));
#93806=CARTESIAN_POINT('Ctrl Pts',(-0.192563978684414,0.697960695024636,
3.57711871243769));
#93807=CARTESIAN_POINT('Ctrl Pts',(-0.126624647538713,-0.43939469164125,
3.43148255932585));
#93808=CARTESIAN_POINT('Ctrl Pts',(-29.267,1.871586531739,-2.6236008493506));
#93809=CARTESIAN_POINT('Ctrl Pts',(-29.2010606688543,2.74117176403474,-2.0032686790181));
#93810=CARTESIAN_POINT('Ctrl Pts',(-29.069182006563,3.80053009112415,0.158992474904673));
#93811=CARTESIAN_POINT('Ctrl Pts',(-28.8713640131257,1.93474699165479,3.27922584988832));
#93812=CARTESIAN_POINT('Ctrl Pts',(-28.6735460196887,-1.69312072237911,
3.40633319030359));
#93813=CARTESIAN_POINT('Ctrl Pts',(-28.4757280262515,-3.77955302551543,
0.438740527979693));
#93814=CARTESIAN_POINT('Ctrl Pts',(-28.2779100328145,-2.4274684197657,-2.93048266535644));
#93815=CARTESIAN_POINT('Ctrl Pts',(-28.0800920393773,1.13358660582709,-3.63202487607056));
#93816=CARTESIAN_POINT('Ctrl Pts',(-27.8822740459403,3.66307656578549,-1.02948321404113));
#93817=CARTESIAN_POINT('Ctrl Pts',(-27.6844560525031,2.85963502885877,2.51011956145336));
#93818=CARTESIAN_POINT('Ctrl Pts',(-27.4866380590661,-0.545794501053909,
3.76560941640859));
#93819=CARTESIAN_POINT('Ctrl Pts',(-27.2888200656289,-3.45459308235099,
1.59490240382455));
#93820=CARTESIAN_POINT('Ctrl Pts',(-27.0910020721918,-3.2201008856232,-2.02703963102139));
#93821=CARTESIAN_POINT('Ctrl Pts',(-26.8931840787547,-0.0556657981542161,
-3.80457269099369));
#93822=CARTESIAN_POINT('Ctrl Pts',(-26.6953660853176,3.15941649666726,-2.12037600768663));
#93823=CARTESIAN_POINT('Ctrl Pts',(-26.4975480918805,3.49977824828921,1.49313686004087));
#93824=CARTESIAN_POINT('Ctrl Pts',(-26.2997300984434,0.655725629921395,
3.7480555903611));
#93825=CARTESIAN_POINT('Ctrl Pts',(-26.1019121050063,-2.78496490129086,
2.59265745132483));
#93826=CARTESIAN_POINT('Ctrl Pts',(-25.9040941115692,-3.69164355556124,
-0.921775100281393));
#93827=CARTESIAN_POINT('Ctrl Pts',(-25.706276118132,-1.23933208819682,-3.59749306908928));
#93828=CARTESIAN_POINT('Ctrl Pts',(-25.508458124695,2.34063535810499,-2.99988788509652));
#93829=CARTESIAN_POINT('Ctrl Pts',(-25.3106401312578,3.79088182894556,0.327285808551454));
#93830=CARTESIAN_POINT('Ctrl Pts',(-25.1128221378208,1.79184233806401,3.35666530231748));
#93831=CARTESIAN_POINT('Ctrl Pts',(-24.9150041443836,-1.83757679742267,
3.3318482175997));
#93832=CARTESIAN_POINT('Ctrl Pts',(-24.7171861509465,-3.79500295175934,
0.275415315864581));
#93833=CARTESIAN_POINT('Ctrl Pts',(-24.5193681575094,-2.29939338753055,
-3.03161525196208));
#93834=CARTESIAN_POINT('Ctrl Pts',(-24.3215501640723,1.28841151633002,-3.5802090396263));
#93835=CARTESIAN_POINT('Ctrl Pts',(-24.1237321706352,3.70390350292133,-0.871205967781821));
#93836=CARTESIAN_POINT('Ctrl Pts',(-23.925914177198,2.74925026171735,2.63049881095482));
#93837=CARTESIAN_POINT('Ctrl Pts',(-23.728096183761,-0.706918648264489,
3.73873869412743));
#93838=CARTESIAN_POINT('Ctrl Pts',(-23.5302781903238,-3.51986925989793,
1.44513715284179));
#93839=CARTESIAN_POINT('Ctrl Pts',(-23.3324601968868,-3.13012558468118,
-2.16338041530871));
#93840=CARTESIAN_POINT('Ctrl Pts',(-23.1346422034496,0.107688455305257,
-3.80345950341412));
#93841=CARTESIAN_POINT('Ctrl Pts',(-22.9368242100126,3.24751783306243,-1.98280834205173));
#93842=CARTESIAN_POINT('Ctrl Pts',(-22.7390062165755,3.43246279827112,1.64198055282517));
#93843=CARTESIAN_POINT('Ctrl Pts',(-22.5411882231383,0.494243753116372,
3.77274755449071));
#93844=CARTESIAN_POINT('Ctrl Pts',(-22.3433702297012,-2.89368280317716,
2.47072880583525));
#93845=CARTESIAN_POINT('Ctrl Pts',(-22.1455522362641,-3.64867594709571,
-1.07938168896592));
#93846=CARTESIAN_POINT('Ctrl Pts',(-21.947734242827,-1.08377487127288,-3.64737344205279));
#93847=CARTESIAN_POINT('Ctrl Pts',(-21.7499162493899,2.46724225947258,-2.89665611187517));
#93848=CARTESIAN_POINT('Ctrl Pts',(-21.5520982559528,3.7733400181795,0.489700014903892));
#93849=CARTESIAN_POINT('Ctrl Pts',(-21.3542802625157,1.64611294971294,3.43048293308387));
#93850=CARTESIAN_POINT('Ctrl Pts',(-21.1564622690786,-1.97889603910867,
3.24990330068325));
#93851=CARTESIAN_POINT('Ctrl Pts',(-20.9586442756415,-3.80332706020577,
0.11226874230432));
#93852=CARTESIAN_POINT('Ctrl Pts',(-20.7608262822044,-2.16714834066106,
-3.12751803623289));
#93853=CARTESIAN_POINT('Ctrl Pts',(-20.5630082887673,1.44089725711671,-3.52160703256702));
#93854=CARTESIAN_POINT('Ctrl Pts',(-20.3651902953302,3.73788466707397,-0.711420559897795));
#93855=CARTESIAN_POINT('Ctrl Pts',(-20.1673723018931,2.63380772376682,2.7460804561444));
#93856=CARTESIAN_POINT('Ctrl Pts',(-19.9695543084559,-0.866744862987072,
3.70494997805335));
#93857=CARTESIAN_POINT('Ctrl Pts',(-19.7717363150188,-3.57865485655257,
1.29272209506325));
#93858=CARTESIAN_POINT('Ctrl Pts',(-19.5739183215817,-3.03438212932128,
-2.29574085877471));
#93859=CARTESIAN_POINT('Ctrl Pts',(-19.3761003281446,0.270844937974172,
-3.7953318717822));
#93860=CARTESIAN_POINT('Ctrl Pts',(-19.1782823347075,3.32963287034385,-1.84158788715549));
#93861=CARTESIAN_POINT('Ctrl Pts',(-18.9804643412704,3.35882072849595,1.78779873341992));
#93862=CARTESIAN_POINT('Ctrl Pts',(-18.7826463478333,0.331850768478793,
3.79048493795346));
#93863=CARTESIAN_POINT('Ctrl Pts',(-18.5848283543962,-2.99706692931064,
2.34424632208829));
#93864=CARTESIAN_POINT('Ctrl Pts',(-18.3870103609591,-3.59898301910093,
-1.23499887676674));
#93865=CARTESIAN_POINT('Ctrl Pts',(-18.189192367522,-0.926219993698007,
-3.69053079118249));
#93866=CARTESIAN_POINT('Ctrl Pts',(-17.9913743740849,2.5893014591106,-2.78808517646783));
#93867=CARTESIAN_POINT('Ctrl Pts',(-17.7935563806477,3.74884307925887,0.651211612676593));
#93868=CARTESIAN_POINT('Ctrl Pts',(-17.5957383872107,1.49734939509152,3.49797738506285));
#93869=CARTESIAN_POINT('Ctrl Pts',(-17.3979203937735,-2.11656771987002,
3.16196807140684));
#93870=CARTESIAN_POINT('Ctrl Pts',(-17.2001024003364,-3.80464076405789,
-0.0510847713210306));
#93871=CARTESIAN_POINT('Ctrl Pts',(-17.0022844068993,-2.03090874143955,
-3.21765608499983));
#93872=CARTESIAN_POINT('Ctrl Pts',(-16.8044664134622,1.59072709321647,-3.45651389586373));
#93873=CARTESIAN_POINT('Ctrl Pts',(-16.6066484200251,3.7649760515017,-0.55032384012566));
#93874=CARTESIAN_POINT('Ctrl Pts',(-16.408830426588,2.51351047331346,2.85660044422309));
#93875=CARTESIAN_POINT('Ctrl Pts',(-16.2110124331509,-1.02497346786645,
3.66433218848425));
#93876=CARTESIAN_POINT('Ctrl Pts',(-16.0131944397138,-3.63084417051879,
1.13792425354314));
#93877=CARTESIAN_POINT('Ctrl Pts',(-15.8153764462767,-2.93304561087793,
-2.42386972461428));
#93878=CARTESIAN_POINT('Ctrl Pts',(-15.6175584528396,0.433502191222674,
-3.78020857197022));
#93879=CARTESIAN_POINT('Ctrl Pts',(-15.4197404594025,3.40561062963269,-1.69697296287383));
#93880=CARTESIAN_POINT('Ctrl Pts',(-15.2219224659654,3.27898758080047,1.93032159039582));
#93881=CARTESIAN_POINT('Ctrl Pts',(-15.0241044725282,0.168846106669414,
3.80123558723405));
#93882=CARTESIAN_POINT('Ctrl Pts',(-14.8262864790911,-3.09492677284964,
2.21344285403769));
#93883=CARTESIAN_POINT('Ctrl Pts',(-14.628468485654,-3.54265633893431,-1.38833967803291));
#93884=CARTESIAN_POINT('Ctrl Pts',(-14.4306504922169,-0.766957879978414,
-3.7268856445739));
#93885=CARTESIAN_POINT('Ctrl Pts',(-14.2328324987798,2.70658798155444,-2.6743751598265));
#93886=CARTESIAN_POINT('Ctrl Pts',(-14.0350145053427,3.71743616166189,0.811522877903334));
#93887=CARTESIAN_POINT('Ctrl Pts',(-13.8371965119056,1.34582588168488,3.55902426144851));
#93888=CARTESIAN_POINT('Ctrl Pts',(-13.6393785184685,-2.2503380802767,3.06820460886307));
#93889=CARTESIAN_POINT('Ctrl Pts',(-13.4415605250314,-3.79894164128729,
-0.214344123981669));
#93890=CARTESIAN_POINT('Ctrl Pts',(-13.2437425315943,-1.8909257110314,-3.30186325470216));
#93891=CARTESIAN_POINT('Ctrl Pts',(-13.0459245381572,1.7376248539901,-3.38504961029937));
#93892=CARTESIAN_POINT('Ctrl Pts',(-12.8481065447201,3.78512772048049,-0.388212747140301));
#93893=CARTESIAN_POINT('Ctrl Pts',(-12.6502885512829,2.38858024585731,2.96185506169566));
#93894=CARTESIAN_POINT('Ctrl Pts',(-12.4524705578458,-1.18131281127045,
3.61696019321754));
#93895=CARTESIAN_POINT('Ctrl Pts',(-12.2546525644087,-3.67634100489465,
0.98102895631177));
#93896=CARTESIAN_POINT('Ctrl Pts',(-12.0568345709716,-2.82630281583156,
-2.54753084193589));
#93897=CARTESIAN_POINT('Ctrl Pts',(-11.8590165775345,0.595360400383641,
-3.75811747967609));
#93898=CARTESIAN_POINT('Ctrl Pts',(-11.6611985840974,3.47531106646949,-1.54923012773011));
#93899=CARTESIAN_POINT('Ctrl Pts',(-11.4633805906603,3.19311050600954,2.06928642140315));
#93900=CARTESIAN_POINT('Ctrl Pts',(-11.2655625972232,0.00553022271176743,
3.80497968641473));
#93901=CARTESIAN_POINT('Ctrl Pts',(-11.0677446037861,-3.18708195562982,
2.07855950251388));
#93902=CARTESIAN_POINT('Ctrl Pts',(-10.869926610349,-3.47979972960233,-1.53912145045528));
#93903=CARTESIAN_POINT('Ctrl Pts',(-10.6721086169119,-0.606282086762444,
-3.75637099188338));
#93904=CARTESIAN_POINT('Ctrl Pts',(-10.4742906234748,2.81888564080964,-2.55573565562428));
#93905=CARTESIAN_POINT('Ctrl Pts',(-10.2764726300377,3.67917715554996,0.970338320108655));
#93906=CARTESIAN_POINT('Ctrl Pts',(-10.0786546366006,1.19182170212393,3.61351103882891));
#93907=CARTESIAN_POINT('Ctrl Pts',(-9.88083664316345,-2.37996055083567,
2.96878574064515));
#93908=CARTESIAN_POINT('Ctrl Pts',(-9.68301864972634,-3.78624019668592,
-0.377208391200055));
#93909=CARTESIAN_POINT('Ctrl Pts',(-9.48520065628923,-1.74745727030714,
-3.37998433218895));
#93910=CARTESIAN_POINT('Ctrl Pts',(-9.28738266285213,1.88131977313113,-3.30734590096318));
#93911=CARTESIAN_POINT('Ctrl Pts',(-9.08956466941502,3.79830252985678,-0.225386088913072));
#93912=CARTESIAN_POINT('Ctrl Pts',(-8.8917466759779,2.25924731649643,3.06165030013156));
#93913=CARTESIAN_POINT('Ctrl Pts',(-8.69392868254081,-1.33547472388757,
3.56292130971895));
#93914=CARTESIAN_POINT('Ctrl Pts',(-8.49611068910369,-3.71506149856655,
0.822325397431237));
#93915=CARTESIAN_POINT('Ctrl Pts',(-8.2982926956666,-2.71435049566573,-2.66649627490293));
#93916=CARTESIAN_POINT('Ctrl Pts',(-8.10047470222948,0.756121223608606,
-3.72909931385589));
#93917=CARTESIAN_POINT('Ctrl Pts',(-7.90265670879237,3.53860570694324,-1.39863170569708));
#93918=CARTESIAN_POINT('Ctrl Pts',(-7.70483871535527,3.10134779529267,2.20443708234665));
#93919=CARTESIAN_POINT('Ctrl Pts',(-7.50702072191815,-0.15779585471615,
3.80171033426082));
#93920=CARTESIAN_POINT('Ctrl Pts',(-7.30920272848106,-3.27336261448717,
1.93984488850845));
#93921=CARTESIAN_POINT('Ctrl Pts',(-7.11138473504394,-3.41052905026979,
-1.68706626860225));
#93922=CARTESIAN_POINT('Ctrl Pts',(-6.91356674160684,-0.444488776435454,
-3.77893248484412));
#93923=CARTESIAN_POINT('Ctrl Pts',(-6.71574874816972,2.92598744650415,-2.43238534371312));
#93924=CARTESIAN_POINT('Ctrl Pts',(-6.51793075473262,3.63413658105342,1.12736520596504));
#93925=CARTESIAN_POINT('Ctrl Pts',(-6.32011276129551,1.03562072148409,3.66133728555581));
#93926=CARTESIAN_POINT('Ctrl Pts',(-6.12229476785841,-2.50519620758082,
2.86389471856769));
#93927=CARTESIAN_POINT('Ctrl Pts',(-5.92447677442129,-3.766559841907,-0.539377376750802));
#93928=CARTESIAN_POINT('Ctrl Pts',(-5.72665878098419,-1.60076786459875,
-3.45187532233801));
#93929=CARTESIAN_POINT('Ctrl Pts',(-5.52884078754708,2.02154698800078,-3.22354599370549));
#93930=CARTESIAN_POINT('Ctrl Pts',(-5.33102279410997,3.80447619524911,-0.0621439922320252));
#93931=CARTESIAN_POINT('Ctrl Pts',(-5.13320480067286,2.12575007586871,3.15580221373199));
#93932=CARTESIAN_POINT('Ctrl Pts',(-4.93538680723576,-1.48717505057987,
3.50231514455317));
#93933=CARTESIAN_POINT('Ctrl Pts',(-4.73756881379864,-3.7469342794927,0.662106103061155));
#93934=CARTESIAN_POINT('Ctrl Pts',(-4.53975082036155,-2.59739500666645,
-2.78054674109591));
#93935=CARTESIAN_POINT('Ctrl Pts',(-4.34193282692443,0.91548834647712,-3.69320756511369));
#93936=CARTESIAN_POINT('Ctrl Pts',(-4.14411483348733,3.59537787550923,-1.24545527762321));
#93937=CARTESIAN_POINT('Ctrl Pts',(-3.94629684005022,3.00386860560673,2.33552444683395));
#93938=CARTESIAN_POINT('Ctrl Pts',(-3.74847884661311,-0.320831111098236,
3.79143358123437));
#93939=CARTESIAN_POINT('Ctrl Pts',(-3.55066085317601,-3.35360965126126,
1.79755464838957));
#93940=CARTESIAN_POINT('Ctrl Pts',(-3.35284285973889,-3.33497210351366,
-1.8319013471258));
#93941=CARTESIAN_POINT('Ctrl Pts',(-3.15502486630179,-0.281875939904123,
-3.79452870799989));
#93942=CARTESIAN_POINT('Ctrl Pts',(-2.95720687286468,3.02769554249517,-2.30455126046869));
#93943=CARTESIAN_POINT('Ctrl Pts',(-2.75938887942757,3.58239830638208,1.28231347354763));
#93944=CARTESIAN_POINT('Ctrl Pts',(-2.56157088599047,0.877509230153572,
3.70241604420433));
#93945=CARTESIAN_POINT('Ctrl Pts',(-2.36375289255336,-2.62581110307242,
2.75372258826496));
#93946=CARTESIAN_POINT('Ctrl Pts',(-2.16593489911625,-3.73994280606706,
-0.70054777615089));
#93947=CARTESIAN_POINT('Ctrl Pts',(-1.96811690567914,-1.45111647622458,
-3.51741211898495));
#93948=CARTESIAN_POINT('Ctrl Pts',(-1.77029891224204,2.15802619942714,-3.13378825655336));
#93949=CARTESIAN_POINT('Ctrl Pts',(-1.57248091880493,3.80367913311811,0.10118183309678));
#93950=CARTESIAN_POINT('Ctrl Pts',(-1.37466292536782,1.98825456019507,3.24419626697628));
#93951=CARTESIAN_POINT('Ctrl Pts',(-1.17684493193072,-1.63598093042552,
3.4351404175943));
#93952=CARTESIAN_POINT('Ctrl Pts',(-0.979026938493603,-3.77219405840141,
0.500882787361939));
#93953=CARTESIAN_POINT('Ctrl Pts',(-0.781208945056499,-2.47508968989639,
-2.88988673662884));
#93954=CARTESIAN_POINT('Ctrl Pts',(-0.583390951619393,1.07208850868958,
-3.64971092190177));
#93955=CARTESIAN_POINT('Ctrl Pts',(-0.385572958182278,3.64761664098089,
-1.09154062532392));
#93956=CARTESIAN_POINT('Ctrl Pts',(-0.187754964745176,2.89660315542323,
2.4655623578828));
#93957=CARTESIAN_POINT('Ctrl Pts',(-0.0558763024537703,0.650195932906673,
3.33231950585592));
#93958=CARTESIAN_POINT('Ctrl Pts',(0.0100630286919312,-0.409324828006024,
3.19664992573129));
#93959=CARTESIAN_POINT('Ctrl Pts',(-0.400000000000005,-0.499534418911589,
3.90114782651499));
#93960=CARTESIAN_POINT('Ctrl Pts',(-0.465939331145705,0.793490219260627,
4.06671712560119));
#93961=CARTESIAN_POINT('Ctrl Pts',(-0.531878662291405,2.16423253656064,
3.53782784424547));
#93962=CARTESIAN_POINT('Ctrl Pts',(-0.597817993437104,3.00235812536596,
2.54987656932921));
#93963=CARTESIAN_POINT('Ctrl Pts',(-0.663757324582806,3.84048371417132,
1.56192529441289));
#93964=CARTESIAN_POINT('Ctrl Pts',(-0.729696655728509,4.14599257448196,
0.114912025935935));
#93965=CARTESIAN_POINT('Ctrl Pts',(-0.795635986874212,3.7748904564356,-1.12892061230742));
#93966=CARTESIAN_POINT('Ctrl Pts',(-0.861575318019917,3.40378833838922,
-2.37275325055082));
#93967=CARTESIAN_POINT('Ctrl Pts',(-0.92751464916562,2.3560752419859,-3.41340525856059));
#93968=CARTESIAN_POINT('Ctrl Pts',(-0.993453980311325,1.11073073810251,
-3.77918475618231));
#93969=CARTESIAN_POINT('Ctrl Pts',(-1.05939331145703,-0.134613765780807,
-4.144964253804));
#93970=CARTESIAN_POINT('Ctrl Pts',(-1.12533264260273,-1.57758967714414,
-3.83587124103763));
#93971=CARTESIAN_POINT('Ctrl Pts',(-1.19127197374843,-2.56290570312447,
-2.99164994667031));
#93972=CARTESIAN_POINT('Ctrl Pts',(-1.24846014182062,-3.41745514302525,
-2.25946979813762));
#93973=CARTESIAN_POINT('Ctrl Pts',(-1.30564830989282,-3.92776077108088,
-1.12477545649334));
#93974=CARTESIAN_POINT('Ctrl Pts',(-1.36283647796502,-3.93682057842306,
0.00276514463350926));
#93975=CARTESIAN_POINT('Origin',(-0.4,0.,0.));
#93976=CARTESIAN_POINT('',(0.,-5.30639458070548E-16,4.333));
#93977=CARTESIAN_POINT('Origin',(-0.4,-5.30639458070548E-16,4.333));
#93978=CARTESIAN_POINT('Origin',(0.,0.,0.));
#93979=CARTESIAN_POINT('Origin',(-0.4,0.,0.));
#93980=CARTESIAN_POINT('Origin',(-14.6,0.,0.));
#93981=CARTESIAN_POINT('Origin',(0.,5.8,0.));
#93982=CARTESIAN_POINT('',(0.,-5.8,-7.10295143505465E-16));
#93983=CARTESIAN_POINT('Origin',(0.,0.,0.));
#93984=CARTESIAN_POINT('Origin',(4.8215647221589,0.,0.));
#93985=CARTESIAN_POINT('',(4.55911872188336,3.75277674973257,-6.5));
#93986=CARTESIAN_POINT('',(4.55911872188336,-3.75277674973257,-6.5));
#93987=CARTESIAN_POINT('Ctrl Pts',(4.55911872188336,3.75277674973257,-6.5));
#93988=CARTESIAN_POINT('Ctrl Pts',(5.74495593589618,-6.10622663543836E-15,
-6.5));
#93989=CARTESIAN_POINT('Ctrl Pts',(4.55911872188336,-3.75277674973257,-6.5));
#93990=CARTESIAN_POINT('',(4.55911872188336,7.50555349946513,0.));
#93991=CARTESIAN_POINT('Ctrl Pts',(4.55911872188336,7.50555349946513,0.));
#93992=CARTESIAN_POINT('Ctrl Pts',(5.74495593589617,5.62916512459885,-3.25000000000001));
#93993=CARTESIAN_POINT('Ctrl Pts',(4.55911872188336,3.75277674973257,-6.5));
#93994=CARTESIAN_POINT('',(4.55911872188336,3.75277674973257,6.5));
#93995=CARTESIAN_POINT('Ctrl Pts',(4.55911872188336,3.75277674973257,6.5));
#93996=CARTESIAN_POINT('Ctrl Pts',(5.74495593589617,5.62916512459886,3.25));
#93997=CARTESIAN_POINT('Ctrl Pts',(4.55911872188336,7.50555349946513,0.));
#93998=CARTESIAN_POINT('',(4.55911872188336,-3.75277674973257,6.5));
#93999=CARTESIAN_POINT('Ctrl Pts',(4.55911872188336,-3.75277674973257,6.5));
#94000=CARTESIAN_POINT('Ctrl Pts',(5.74495593589617,6.66133814775094E-15,
6.5));
#94001=CARTESIAN_POINT('Ctrl Pts',(4.55911872188336,3.75277674973257,6.5));
#94002=CARTESIAN_POINT('',(4.55911872188336,-7.50555349946513,9.19165206894919E-16));
#94003=CARTESIAN_POINT('Ctrl Pts',(4.55911872188336,-7.50555349946513,9.19165206894919E-16));
#94004=CARTESIAN_POINT('Ctrl Pts',(5.74495593589617,-5.62916512459885,3.25000000000001));
#94005=CARTESIAN_POINT('Ctrl Pts',(4.55911872188336,-3.75277674973257,6.5));
#94006=CARTESIAN_POINT('',(5.3,-6.33323321723195,-7.7559737877368E-16));
#94007=CARTESIAN_POINT('',(4.8215647221589,-7.09027674973257,-8.68308472662889E-16));
#94008=CARTESIAN_POINT('Origin',(5.3,0.,0.));
#94009=CARTESIAN_POINT('Ctrl Pts',(4.55911872188336,-3.75277674973257,-6.5));
#94010=CARTESIAN_POINT('Ctrl Pts',(5.74495593589617,-5.62916512459886,-3.24999999999999));
#94011=CARTESIAN_POINT('Ctrl Pts',(4.55911872188336,-7.50555349946513,9.19165206894919E-16));
#94012=CARTESIAN_POINT('Origin',(0.2,3.75277674973257,6.5));
#94013=CARTESIAN_POINT('',(0.2,3.75277674973257,6.5));
#94014=CARTESIAN_POINT('',(0.2,3.75277674973257,6.5));
#94015=CARTESIAN_POINT('',(0.2,-3.75277674973257,6.5));
#94016=CARTESIAN_POINT('',(0.2,3.75277674973257,6.5));
#94017=CARTESIAN_POINT('',(0.2,-3.75277674973257,6.5));
#94018=CARTESIAN_POINT('Origin',(0.2,7.50555349946513,0.));
#94019=CARTESIAN_POINT('',(0.2,7.50555349946513,0.));
#94020=CARTESIAN_POINT('',(0.2,7.50555349946513,0.));
#94021=CARTESIAN_POINT('',(0.2,7.50555349946513,0.));
#94022=CARTESIAN_POINT('Origin',(0.2,3.75277674973257,-6.5));
#94023=CARTESIAN_POINT('',(0.2,3.75277674973257,-6.5));
#94024=CARTESIAN_POINT('',(0.2,3.75277674973257,-6.5));
#94025=CARTESIAN_POINT('',(0.2,3.75277674973257,-6.5));
#94026=CARTESIAN_POINT('Origin',(0.125,0.,0.));
#94027=CARTESIAN_POINT('',(0.2,-5.8,-7.10295143505465E-16));
#94028=CARTESIAN_POINT('Origin',(0.2,0.,0.));
#94029=CARTESIAN_POINT('',(0.125,-5.8,-7.10295143505465E-16));
#94030=CARTESIAN_POINT('Origin',(-30.,3.2,0.));
#94031=CARTESIAN_POINT('',(-30.,-3.2,-3.91886975727153E-16));
#94032=CARTESIAN_POINT('Origin',(-30.,0.,0.));
#94033=CARTESIAN_POINT('Origin',(-29.6,0.,0.));
#94034=CARTESIAN_POINT('',(-29.6,-3.6,-4.40872847693047E-16));
#94035=CARTESIAN_POINT('Origin',(0.2,-3.75277674973257,-6.5));
#94036=CARTESIAN_POINT('',(0.2,-3.75277674973257,-6.5));
#94037=CARTESIAN_POINT('',(0.2,-3.75277674973257,-6.5));
#94038=CARTESIAN_POINT('',(0.2,-3.75277674973257,-6.5));
#94039=CARTESIAN_POINT('Origin',(0.2,-7.50555349946513,9.19165206894919E-16));
#94040=CARTESIAN_POINT('',(0.2,-7.50555349946513,9.19165206894919E-16));
#94041=CARTESIAN_POINT('',(0.2,-7.50555349946513,9.19165206894919E-16));
#94042=CARTESIAN_POINT('',(0.2,-7.50555349946513,9.19165206894919E-16));
#94043=CARTESIAN_POINT('Origin',(0.2,-3.75277674973257,6.5));
#94044=CARTESIAN_POINT('',(0.2,-3.75277674973257,6.5));
#94045=CARTESIAN_POINT('Origin',(5.3,0.,0.));
#94046=CARTESIAN_POINT('Origin',(0.2,0.,0.));
#94047=CARTESIAN_POINT('',(0.,0.,0.));
#94048=CARTESIAN_POINT('Origin',(0.1,0.,0.));
#94049=CARTESIAN_POINT('',(0.2,-8.,-9.79717439317883E-16));
#94050=CARTESIAN_POINT('Origin',(0.2,0.,0.));
#94051=CARTESIAN_POINT('',(-1.21430643318376E-16,-7.8,-9.55224503334936E-16));
#94052=CARTESIAN_POINT('',(0.1,-7.9,-9.67470971326409E-16));
#94053=CARTESIAN_POINT('Origin',(0.,0.,0.));
#94054=CARTESIAN_POINT('Origin',(0.8,0.,0.));
#94055=CARTESIAN_POINT('',(1.4,-8.,-9.79717439317883E-16));
#94056=CARTESIAN_POINT('Origin',(1.4,0.,0.));
#94057=CARTESIAN_POINT('',(0.8,-8.,-9.79717439317883E-16));
#94058=CARTESIAN_POINT('Origin',(1.5,0.,0.));
#94059=CARTESIAN_POINT('',(1.6,-7.8,-9.55224503334936E-16));
#94060=CARTESIAN_POINT('Origin',(1.6,0.,0.));
#94061=CARTESIAN_POINT('',(1.5,-7.9,-9.67470971326409E-16));
#94062=CARTESIAN_POINT('Origin',(1.6,4.4,0.));
#94063=CARTESIAN_POINT('',(1.6,-4.4,-5.38844591624835E-16));
#94064=CARTESIAN_POINT('Origin',(1.6,0.,0.));
#94065=CARTESIAN_POINT('Origin',(1.5,0.,0.));
#94066=CARTESIAN_POINT('',(1.4,-4.2,-5.14351655641888E-16));
#94067=CARTESIAN_POINT('',(1.5,-4.3,-5.26598123633362E-16));
#94068=CARTESIAN_POINT('Origin',(1.4,0.,0.));
#94069=CARTESIAN_POINT('Origin',(0.8,0.,0.));
#94070=CARTESIAN_POINT('',(0.2,-4.2,-5.14351655641888E-16));
#94071=CARTESIAN_POINT('',(0.8,-4.2,-5.14351655641888E-16));
#94072=CARTESIAN_POINT('Origin',(0.2,0.,0.));
#94073=CARTESIAN_POINT('Origin',(0.1,0.,0.));
#94074=CARTESIAN_POINT('',(-5.20417042793042E-17,-4.4,-5.38844591624835E-16));
#94075=CARTESIAN_POINT('',(0.1,-4.3,-5.26598123633362E-16));
#94076=CARTESIAN_POINT('Origin',(0.,0.,0.));
#94077=CARTESIAN_POINT('Origin',(0.,7.8,0.));
#94078=CARTESIAN_POINT('',(0.,0.,0.));
#94079=CARTESIAN_POINT('Origin',(1.,0.,0.));
#94080=CARTESIAN_POINT('',(1.85,-7.4,-9.06238631369041E-16));
#94081=CARTESIAN_POINT('',(0.15,-7.4,-9.06238631369041E-16));
#94082=CARTESIAN_POINT('',(1.,-7.4,-9.06238631369041E-16));
#94083=CARTESIAN_POINT('',(1.85,0.768097998000808,7.36002890384726));
#94084=CARTESIAN_POINT('Origin',(1.85,0.,0.));
#94085=CARTESIAN_POINT('',(0.15,-0.213397459621556,7.39692243600182));
#94086=CARTESIAN_POINT('Origin',(0.519615242270663,0.,0.));
#94087=CARTESIAN_POINT('Origin',(0.15,0.,0.));
#94088=CARTESIAN_POINT('Origin',(2.2,1.57017059221718,0.));
#94089=CARTESIAN_POINT('',(2.,1.45470053837925,4.31118850708701));
#94090=CARTESIAN_POINT('',(1.5,1.16602540378444,3.87851579315198));
#94091=CARTESIAN_POINT('Ctrl Pts',(2.,1.45470053837925,4.31118850708701));
#94092=CARTESIAN_POINT('Ctrl Pts',(1.73679217533305,1.30273742995497,4.08467677256398));
#94093=CARTESIAN_POINT('Ctrl Pts',(1.5,1.16602540378444,3.87851579315198));
#94094=CARTESIAN_POINT('',(2.,1.45470053837925,7.10255914045347));
#94095=CARTESIAN_POINT('',(2.,1.45470053837925,0.));
#94096=CARTESIAN_POINT('',(1.85,1.36809799800081,7.2724347963984));
#94097=CARTESIAN_POINT('Ctrl Pts',(1.85,1.36809799800081,7.2724347963984));
#94098=CARTESIAN_POINT('Ctrl Pts',(1.92588630814391,1.4119109784355,7.18697522907551));
#94099=CARTESIAN_POINT('Ctrl Pts',(2.,1.45470053837925,7.10255914045347));
#94100=CARTESIAN_POINT('',(0.15,0.386602540378444,7.3898943480792));
#94101=CARTESIAN_POINT('Origin',(-0.519615242270663,0.,0.));
#94102=CARTESIAN_POINT('',(0.,0.3,7.24379044423567));
#94103=CARTESIAN_POINT('Ctrl Pts',(2.86229373536173E-16,0.3,7.24379044423567));
#94104=CARTESIAN_POINT('Ctrl Pts',(0.0742511938739692,0.342868946770787,
7.31632987999105));
#94105=CARTESIAN_POINT('Ctrl Pts',(0.15,0.386602540378444,7.3898943480792));
#94106=CARTESIAN_POINT('',(0.,0.3,4.54009911786075));
#94107=CARTESIAN_POINT('',(5.55111512312578E-16,0.300000000000001,0.));
#94108=CARTESIAN_POINT('',(0.5,0.588675134594813,4.0069890923123));
#94109=CARTESIAN_POINT('Ctrl Pts',(0.5,0.588675134594813,4.0069890923123));
#94110=CARTESIAN_POINT('Ctrl Pts',(0.26559332290833,0.453340376476092,4.26379419596142));
#94111=CARTESIAN_POINT('Ctrl Pts',(3.12250225675825E-16,0.3,4.54009911786075));
#94112=CARTESIAN_POINT('Origin',(-0.519615242270663,0.,0.));
#94113=CARTESIAN_POINT('Origin',(-0.2,-0.415470053837925,0.));
#94114=CARTESIAN_POINT('',(1.5,0.566025403784439,4.01025126921876));
#94115=CARTESIAN_POINT('',(2.,0.854700538379251,4.4690029077742));
#94116=CARTESIAN_POINT('Ctrl Pts',(1.5,0.566025403784439,4.01025126921876));
#94117=CARTESIAN_POINT('Ctrl Pts',(1.73647429275706,0.702553900364154,4.22979918009891));
#94118=CARTESIAN_POINT('Ctrl Pts',(2.,0.854700538379252,4.4690029077742));
#94119=CARTESIAN_POINT('',(0.5,-0.011324865405187,4.04998416631764));
#94120=CARTESIAN_POINT('Origin',(0.519615242270663,0.,0.));
#94121=CARTESIAN_POINT('',(0.,-0.3,4.54009911786075));
#94122=CARTESIAN_POINT('Ctrl Pts',(0.,-0.3,4.54009911786075));
#94123=CARTESIAN_POINT('Ctrl Pts',(0.264263975543855,-0.147427122582635,
4.28534053319701));
#94124=CARTESIAN_POINT('Ctrl Pts',(0.5,-0.011324865405187,4.04998416631764));
#94125=CARTESIAN_POINT('',(0.,-0.3,7.24379044423567));
#94126=CARTESIAN_POINT('',(2.77555756156289E-16,-0.3,0.));
#94127=CARTESIAN_POINT('Ctrl Pts',(0.15,-0.213397459621556,7.39692243600182));
#94128=CARTESIAN_POINT('Ctrl Pts',(0.0742155505352446,-0.25715163192042,
7.31984416998126));
#94129=CARTESIAN_POINT('Ctrl Pts',(8.67361737988404E-18,-0.3,7.24379044423567));
#94130=CARTESIAN_POINT('',(2.,0.854700538379251,7.19944351944608));
#94131=CARTESIAN_POINT('Ctrl Pts',(2.,0.854700538379252,7.19944351944608));
#94132=CARTESIAN_POINT('Ctrl Pts',(1.92582722117148,0.811876864556063,7.27922108309076));
#94133=CARTESIAN_POINT('Ctrl Pts',(1.85,0.768097998000808,7.36002890384726));
#94134=CARTESIAN_POINT('',(2.,0.854700538379251,0.));
#94135=CARTESIAN_POINT('Origin',(0.075,0.,0.));
#94136=CARTESIAN_POINT('Origin',(0.15,0.,0.));
#94137=CARTESIAN_POINT('Origin',(0.,0.,0.));
#94138=CARTESIAN_POINT('Origin',(1.,0.,0.));
#94139=CARTESIAN_POINT('Origin',(1.85,0.,0.));
#94140=CARTESIAN_POINT('Origin',(1.925,0.,0.));
#94141=CARTESIAN_POINT('Origin',(2.,0.,0.));
#94142=CARTESIAN_POINT('Origin',(2.,4.05,0.));
#94143=CARTESIAN_POINT('Origin',(2.,0.,0.));
#94144=CARTESIAN_POINT('Origin',(1.75,0.,0.));
#94145=CARTESIAN_POINT('Origin',(1.5,0.,0.));
#94146=CARTESIAN_POINT('Origin',(1.,0.,0.));
#94147=CARTESIAN_POINT('Origin',(0.5,0.,0.));
#94148=CARTESIAN_POINT('Origin',(0.25,0.,0.));
#94149=CARTESIAN_POINT('Origin',(0.,0.,0.));
#94150=CARTESIAN_POINT('Origin',(0.,7.4,0.));
#94151=CARTESIAN_POINT('',(0.,0.,0.));
#94152=CARTESIAN_POINT('Origin',(0.25,0.,0.));
#94153=CARTESIAN_POINT('',(0.,-4.69285714285714,-5.74709247885579E-16));
#94154=CARTESIAN_POINT('Origin',(0.,0.,0.));
#94155=CARTESIAN_POINT('',(0.600000000000001,-4.05,-4.95981953654678E-16));
#94156=CARTESIAN_POINT('',(0.25,-4.425,-5.41906208622704E-16));
#94157=CARTESIAN_POINT('Origin',(0.600000000000001,0.,0.));
#94158=CARTESIAN_POINT('Origin',(3.4,0.,0.));
#94159=CARTESIAN_POINT('',(6.2,-4.05,-4.95981953654678E-16));
#94160=CARTESIAN_POINT('',(3.4,-4.05,-4.95981953654678E-16));
#94161=CARTESIAN_POINT('Origin',(6.2,0.,0.));
#94162=CARTESIAN_POINT('Origin',(6.55,0.,0.));
#94163=CARTESIAN_POINT('',(6.8,-4.69285714285714,5.74709247885579E-16));
#94164=CARTESIAN_POINT('',(6.55,-4.425,-5.41906208622704E-16));
#94165=CARTESIAN_POINT('Origin',(6.8,0.,0.));
#94166=CARTESIAN_POINT('Origin',(0.478435277841104,0.,0.));
#94167=CARTESIAN_POINT('',(0.,-6.33323321723195,7.75597378773681E-16));
#94168=CARTESIAN_POINT('Origin',(0.,0.,0.));
#94169=CARTESIAN_POINT('',(0.740881278116643,-7.50555349946513,9.19165206894919E-16));
#94170=CARTESIAN_POINT('',(0.478435277841104,-7.09027674973257,-8.68308472662889E-16));
#94171=CARTESIAN_POINT('',(0.740881278116643,-3.75277674973257,6.5));
#94172=CARTESIAN_POINT('Ctrl Pts',(0.740881278116643,-3.75277674973257,
6.5));
#94173=CARTESIAN_POINT('Ctrl Pts',(-0.444955935896173,-5.62916512459885,
3.25));
#94174=CARTESIAN_POINT('Ctrl Pts',(0.740881278116643,-7.50555349946513,
9.19165206894919E-16));
#94175=CARTESIAN_POINT('',(0.740881278116644,3.75277674973257,6.5));
#94176=CARTESIAN_POINT('Ctrl Pts',(0.740881278116644,3.75277674973257,6.5));
#94177=CARTESIAN_POINT('Ctrl Pts',(-0.444955935896173,-5.55111512312578E-15,
6.5));
#94178=CARTESIAN_POINT('Ctrl Pts',(0.740881278116643,-3.75277674973257,
6.5));
#94179=CARTESIAN_POINT('',(0.740881278116643,7.50555349946513,0.));
#94180=CARTESIAN_POINT('Ctrl Pts',(0.740881278116643,7.50555349946513,0.));
#94181=CARTESIAN_POINT('Ctrl Pts',(-0.444955935896173,5.62916512459885,
3.25000000000001));
#94182=CARTESIAN_POINT('Ctrl Pts',(0.740881278116644,3.75277674973257,6.5));
#94183=CARTESIAN_POINT('',(0.740881278116644,3.75277674973257,-6.5));
#94184=CARTESIAN_POINT('Ctrl Pts',(0.740881278116644,3.75277674973257,-6.5));
#94185=CARTESIAN_POINT('Ctrl Pts',(-0.444955935896173,5.62916512459886,
-3.24999999999999));
#94186=CARTESIAN_POINT('Ctrl Pts',(0.740881278116643,7.50555349946513,0.));
#94187=CARTESIAN_POINT('',(0.740881278116643,-3.75277674973257,-6.5));
#94188=CARTESIAN_POINT('Ctrl Pts',(0.740881278116643,-3.75277674973257,
-6.5));
#94189=CARTESIAN_POINT('Ctrl Pts',(-0.444955935896175,4.44089209850063E-15,
-6.5));
#94190=CARTESIAN_POINT('Ctrl Pts',(0.740881278116644,3.75277674973257,-6.5));
#94191=CARTESIAN_POINT('Ctrl Pts',(0.740881278116643,-7.50555349946513,
9.19165206894919E-16));
#94192=CARTESIAN_POINT('Ctrl Pts',(-0.444955935896174,-5.62916512459885,
-3.25));
#94193=CARTESIAN_POINT('Ctrl Pts',(0.740881278116643,-3.75277674973257,
-6.5));
#94194=CARTESIAN_POINT('Origin',(0.,-3.75277674973257,-6.5));
#94195=CARTESIAN_POINT('',(6.05911872188336,3.75277674973257,-6.5));
#94196=CARTESIAN_POINT('',(0.,3.75277674973257,-6.5));
#94197=CARTESIAN_POINT('',(6.05911872188336,-3.75277674973257,-6.5));
#94198=CARTESIAN_POINT('Ctrl Pts',(6.05911872188336,3.75277674973257,-6.5));
#94199=CARTESIAN_POINT('Ctrl Pts',(7.24495593589617,-9.99200722162641E-15,
-6.5));
#94200=CARTESIAN_POINT('Ctrl Pts',(6.05911872188336,-3.75277674973257,-6.5));
#94201=CARTESIAN_POINT('',(0.,-3.75277674973257,-6.5));
#94202=CARTESIAN_POINT('Origin',(0.,3.75277674973257,-6.5));
#94203=CARTESIAN_POINT('',(6.05911872188336,7.50555349946513,0.));
#94204=CARTESIAN_POINT('',(0.,7.50555349946513,0.));
#94205=CARTESIAN_POINT('Ctrl Pts',(6.05911872188336,7.50555349946513,0.));
#94206=CARTESIAN_POINT('Ctrl Pts',(7.24495593589617,5.62916512459885,-3.25000000000001));
#94207=CARTESIAN_POINT('Ctrl Pts',(6.05911872188336,3.75277674973257,-6.5));
#94208=CARTESIAN_POINT('Origin',(0.,7.50555349946513,0.));
#94209=CARTESIAN_POINT('',(6.05911872188336,3.75277674973257,6.5));
#94210=CARTESIAN_POINT('',(0.,3.75277674973257,6.5));
#94211=CARTESIAN_POINT('Ctrl Pts',(6.05911872188336,3.75277674973257,6.5));
#94212=CARTESIAN_POINT('Ctrl Pts',(7.24495593589617,5.62916512459885,3.25));
#94213=CARTESIAN_POINT('Ctrl Pts',(6.05911872188336,7.50555349946513,0.));
#94214=CARTESIAN_POINT('Origin',(6.3215647221589,0.,0.));
#94215=CARTESIAN_POINT('',(6.05911872188336,-3.75277674973257,6.5));
#94216=CARTESIAN_POINT('Ctrl Pts',(6.05911872188336,-3.75277674973257,6.5));
#94217=CARTESIAN_POINT('Ctrl Pts',(7.24495593589618,7.7715611723761E-15,
6.5));
#94218=CARTESIAN_POINT('Ctrl Pts',(6.05911872188336,3.75277674973257,6.5));
#94219=CARTESIAN_POINT('',(6.05911872188336,-7.50555349946513,9.19165206894919E-16));
#94220=CARTESIAN_POINT('Ctrl Pts',(6.05911872188336,-7.50555349946513,9.19165206894919E-16));
#94221=CARTESIAN_POINT('Ctrl Pts',(7.24495593589617,-5.62916512459885,3.25000000000001));
#94222=CARTESIAN_POINT('Ctrl Pts',(6.05911872188336,-3.75277674973257,6.5));
#94223=CARTESIAN_POINT('',(6.8,-6.33323321723195,-7.75597378773681E-16));
#94224=CARTESIAN_POINT('',(6.3215647221589,-7.09027674973257,-8.68308472662889E-16));
#94225=CARTESIAN_POINT('Origin',(6.8,0.,0.));
#94226=CARTESIAN_POINT('Ctrl Pts',(6.05911872188336,-3.75277674973257,-6.5));
#94227=CARTESIAN_POINT('Ctrl Pts',(7.24495593589618,-5.62916512459886,-3.24999999999999));
#94228=CARTESIAN_POINT('Ctrl Pts',(6.05911872188336,-7.50555349946513,9.19165206894919E-16));
#94229=CARTESIAN_POINT('Origin',(0.,3.75277674973257,6.5));
#94230=CARTESIAN_POINT('',(0.,-3.75277674973257,6.5));
#94231=CARTESIAN_POINT('Origin',(0.,-7.50555349946513,9.19165206894919E-16));
#94232=CARTESIAN_POINT('',(0.,-7.50555349946513,9.19165206894919E-16));
#94233=CARTESIAN_POINT('Origin',(0.,-3.75277674973257,6.5));
#94234=CARTESIAN_POINT('Origin',(6.8,0.,0.));
#94235=CARTESIAN_POINT('Origin',(0.,0.,0.));
#94236=CARTESIAN_POINT('',(0.,0.,40.4));
#94237=CARTESIAN_POINT('',(0.,0.,46.9));
#94238=CARTESIAN_POINT('',(0.,0.,28.4));
#94239=CARTESIAN_POINT('',(0.,0.,28.4));
#94240=CARTESIAN_POINT('',(0.,0.,68.9));
#94241=CARTESIAN_POINT('',(0.,0.,79.1));
#94242=CARTESIAN_POINT('',(0.,0.,74.9));
#94243=CARTESIAN_POINT('',(0.,0.,76.9));
#94244=CARTESIAN_POINT('',(35.,0.,33.9));
#94245=CARTESIAN_POINT('',(2.14313189850787E-15,35.,33.9));
#94246=CARTESIAN_POINT('',(-35.,4.28626379701574E-15,33.9));
#94247=CARTESIAN_POINT('',(-6.4293956955236E-15,-35.,33.9));
#94248=CARTESIAN_POINT('',(24.7487373415292,24.7487373415292,18.9));
#94249=CARTESIAN_POINT('',(-24.7487373415292,-24.7487373415292,18.9));
#94250=CARTESIAN_POINT('',(75.,50.,30.));
#94251=CARTESIAN_POINT('',(75.,-50.,30.));
#94252=CARTESIAN_POINT('',(-75.,50.,30.));
#94253=CARTESIAN_POINT('',(-75.,-50.,30.));
#94254=CARTESIAN_POINT('',(75.,50.,28.4));
#94255=CARTESIAN_POINT('',(75.,-50.,28.4));
#94256=CARTESIAN_POINT('',(-75.,50.,28.4));
#94257=CARTESIAN_POINT('',(-75.,-50.,28.4));
#94258=CARTESIAN_POINT('',(75.,50.,10.8));
#94259=CARTESIAN_POINT('',(75.,-50.,10.8));
#94260=CARTESIAN_POINT('',(-75.,50.,10.8));
#94261=CARTESIAN_POINT('',(-75.,-50.,10.8));
#94262=CARTESIAN_POINT('',(75.,50.,8.8));
#94263=CARTESIAN_POINT('',(75.,-50.,8.8));
#94264=CARTESIAN_POINT('',(-75.,50.,8.8));
#94265=CARTESIAN_POINT('',(-75.,-50.,8.8));
#94266=CARTESIAN_POINT('',(75.,50.,2.));
#94267=CARTESIAN_POINT('',(75.,-50.,2.));
#94268=CARTESIAN_POINT('',(-75.,50.,2.));
#94269=CARTESIAN_POINT('',(-75.,-50.,2.));
#94270=UNCERTAINTY_MEASURE_WITH_UNIT(LENGTH_MEASURE(0.01),#94302,
'DISTANCE_ACCURACY_VALUE',
'Maximum model space distance between geometric entities at asserted c
onnectivities');
#94271=UNCERTAINTY_MEASURE_WITH_UNIT(LENGTH_MEASURE(0.01),#94302,
'DISTANCE_ACCURACY_VALUE',
'Maximum model space distance between geometric entities at asserted c
onnectivities');
#94272=UNCERTAINTY_MEASURE_WITH_UNIT(LENGTH_MEASURE(0.01),#94302,
'DISTANCE_ACCURACY_VALUE',
'Maximum model space distance between geometric entities at asserted c
onnectivities');
#94273=UNCERTAINTY_MEASURE_WITH_UNIT(LENGTH_MEASURE(0.01),#94302,
'DISTANCE_ACCURACY_VALUE',
'Maximum model space distance between geometric entities at asserted c
onnectivities');
#94274=UNCERTAINTY_MEASURE_WITH_UNIT(LENGTH_MEASURE(0.01),#94302,
'DISTANCE_ACCURACY_VALUE',
'Maximum model space distance between geometric entities at asserted c
onnectivities');
#94275=UNCERTAINTY_MEASURE_WITH_UNIT(LENGTH_MEASURE(0.01),#94302,
'DISTANCE_ACCURACY_VALUE',
'Maximum model space distance between geometric entities at asserted c
onnectivities');
#94276=UNCERTAINTY_MEASURE_WITH_UNIT(LENGTH_MEASURE(0.01),#94302,
'DISTANCE_ACCURACY_VALUE',
'Maximum model space distance between geometric entities at asserted c
onnectivities');
#94277=UNCERTAINTY_MEASURE_WITH_UNIT(LENGTH_MEASURE(0.01),#94302,
'DISTANCE_ACCURACY_VALUE',
'Maximum model space distance between geometric entities at asserted c
onnectivities');
#94278=UNCERTAINTY_MEASURE_WITH_UNIT(LENGTH_MEASURE(0.01),#94302,
'DISTANCE_ACCURACY_VALUE',
'Maximum model space distance between geometric entities at asserted c
onnectivities');
#94279=UNCERTAINTY_MEASURE_WITH_UNIT(LENGTH_MEASURE(0.01),#94302,
'DISTANCE_ACCURACY_VALUE',
'Maximum model space distance between geometric entities at asserted c
onnectivities');
#94280=UNCERTAINTY_MEASURE_WITH_UNIT(LENGTH_MEASURE(0.01),#94302,
'DISTANCE_ACCURACY_VALUE',
'Maximum model space distance between geometric entities at asserted c
onnectivities');
#94281=UNCERTAINTY_MEASURE_WITH_UNIT(LENGTH_MEASURE(0.01),#94302,
'DISTANCE_ACCURACY_VALUE',
'Maximum model space distance between geometric entities at asserted c
onnectivities');
#94282=UNCERTAINTY_MEASURE_WITH_UNIT(LENGTH_MEASURE(0.01),#94302,
'DISTANCE_ACCURACY_VALUE',
'Maximum model space distance between geometric entities at asserted c
onnectivities');
#94283=UNCERTAINTY_MEASURE_WITH_UNIT(LENGTH_MEASURE(0.01),#94302,
'DISTANCE_ACCURACY_VALUE',
'Maximum model space distance between geometric entities at asserted c
onnectivities');
#94284=UNCERTAINTY_MEASURE_WITH_UNIT(LENGTH_MEASURE(0.01),#94302,
'DISTANCE_ACCURACY_VALUE',
'Maximum model space distance between geometric entities at asserted c
onnectivities');
#94285=UNCERTAINTY_MEASURE_WITH_UNIT(LENGTH_MEASURE(0.01),#94302,
'DISTANCE_ACCURACY_VALUE',
'Maximum model space distance between geometric entities at asserted c
onnectivities');
#94286=(
GEOMETRIC_REPRESENTATION_CONTEXT(3)
GLOBAL_UNCERTAINTY_ASSIGNED_CONTEXT((#94270))
GLOBAL_UNIT_ASSIGNED_CONTEXT((#94302,#94304,#94305))
REPRESENTATION_CONTEXT('','3D')
);
#94287=(
GEOMETRIC_REPRESENTATION_CONTEXT(3)
GLOBAL_UNCERTAINTY_ASSIGNED_CONTEXT((#94271))
GLOBAL_UNIT_ASSIGNED_CONTEXT((#94302,#94304,#94305))
REPRESENTATION_CONTEXT('','3D')
);
#94288=(
GEOMETRIC_REPRESENTATION_CONTEXT(3)
GLOBAL_UNCERTAINTY_ASSIGNED_CONTEXT((#94272))
GLOBAL_UNIT_ASSIGNED_CONTEXT((#94302,#94304,#94305))
REPRESENTATION_CONTEXT('','3D')
);
#94289=(
GEOMETRIC_REPRESENTATION_CONTEXT(3)
GLOBAL_UNCERTAINTY_ASSIGNED_CONTEXT((#94273))
GLOBAL_UNIT_ASSIGNED_CONTEXT((#94302,#94304,#94305))
REPRESENTATION_CONTEXT('','3D')
);
#94290=(
GEOMETRIC_REPRESENTATION_CONTEXT(3)
GLOBAL_UNCERTAINTY_ASSIGNED_CONTEXT((#94274))
GLOBAL_UNIT_ASSIGNED_CONTEXT((#94302,#94304,#94305))
REPRESENTATION_CONTEXT('','3D')
);
#94291=(
GEOMETRIC_REPRESENTATION_CONTEXT(3)
GLOBAL_UNCERTAINTY_ASSIGNED_CONTEXT((#94275))
GLOBAL_UNIT_ASSIGNED_CONTEXT((#94302,#94304,#94305))
REPRESENTATION_CONTEXT('','3D')
);
#94292=(
GEOMETRIC_REPRESENTATION_CONTEXT(3)
GLOBAL_UNCERTAINTY_ASSIGNED_CONTEXT((#94276))
GLOBAL_UNIT_ASSIGNED_CONTEXT((#94302,#94304,#94305))
REPRESENTATION_CONTEXT('','3D')
);
#94293=(
GEOMETRIC_REPRESENTATION_CONTEXT(3)
GLOBAL_UNCERTAINTY_ASSIGNED_CONTEXT((#94277))
GLOBAL_UNIT_ASSIGNED_CONTEXT((#94302,#94304,#94305))
REPRESENTATION_CONTEXT('','3D')
);
#94294=(
GEOMETRIC_REPRESENTATION_CONTEXT(3)
GLOBAL_UNCERTAINTY_ASSIGNED_CONTEXT((#94278))
GLOBAL_UNIT_ASSIGNED_CONTEXT((#94302,#94304,#94305))
REPRESENTATION_CONTEXT('','3D')
);
#94295=(
GEOMETRIC_REPRESENTATION_CONTEXT(3)
GLOBAL_UNCERTAINTY_ASSIGNED_CONTEXT((#94279))
GLOBAL_UNIT_ASSIGNED_CONTEXT((#94302,#94304,#94305))
REPRESENTATION_CONTEXT('','3D')
);
#94296=(
GEOMETRIC_REPRESENTATION_CONTEXT(3)
GLOBAL_UNCERTAINTY_ASSIGNED_CONTEXT((#94280))
GLOBAL_UNIT_ASSIGNED_CONTEXT((#94302,#94304,#94305))
REPRESENTATION_CONTEXT('','3D')
);
#94297=(
GEOMETRIC_REPRESENTATION_CONTEXT(3)
GLOBAL_UNCERTAINTY_ASSIGNED_CONTEXT((#94281))
GLOBAL_UNIT_ASSIGNED_CONTEXT((#94302,#94304,#94305))
REPRESENTATION_CONTEXT('','3D')
);
#94298=(
GEOMETRIC_REPRESENTATION_CONTEXT(3)
GLOBAL_UNCERTAINTY_ASSIGNED_CONTEXT((#94282))
GLOBAL_UNIT_ASSIGNED_CONTEXT((#94302,#94304,#94305))
REPRESENTATION_CONTEXT('','3D')
);
#94299=(
GEOMETRIC_REPRESENTATION_CONTEXT(3)
GLOBAL_UNCERTAINTY_ASSIGNED_CONTEXT((#94283))
GLOBAL_UNIT_ASSIGNED_CONTEXT((#94302,#94304,#94305))
REPRESENTATION_CONTEXT('','3D')
);
#94300=(
GEOMETRIC_REPRESENTATION_CONTEXT(3)
GLOBAL_UNCERTAINTY_ASSIGNED_CONTEXT((#94284))
GLOBAL_UNIT_ASSIGNED_CONTEXT((#94302,#94304,#94305))
REPRESENTATION_CONTEXT('','3D')
);
#94301=(
GEOMETRIC_REPRESENTATION_CONTEXT(3)
GLOBAL_UNCERTAINTY_ASSIGNED_CONTEXT((#94285))
GLOBAL_UNIT_ASSIGNED_CONTEXT((#94302,#94304,#94305))
REPRESENTATION_CONTEXT('','3D')
);
#94302=(
LENGTH_UNIT()
NAMED_UNIT(*)
SI_UNIT(.MILLI.,.METRE.)
);
#94303=(
LENGTH_UNIT()
NAMED_UNIT(*)
SI_UNIT($,.METRE.)
);
#94304=(
NAMED_UNIT(*)
PLANE_ANGLE_UNIT()
SI_UNIT($,.RADIAN.)
);
#94305=(
NAMED_UNIT(*)
SI_UNIT($,.STERADIAN.)
SOLID_ANGLE_UNIT()
);
#94306=SHAPE_DEFINITION_REPRESENTATION(#94321,#94370);
#94307=SHAPE_DEFINITION_REPRESENTATION(#94322,#94371);
#94308=SHAPE_DEFINITION_REPRESENTATION(#94323,#94372);
#94309=SHAPE_DEFINITION_REPRESENTATION(#94324,#94373);
#94310=SHAPE_DEFINITION_REPRESENTATION(#94325,#94374);
#94311=SHAPE_DEFINITION_REPRESENTATION(#94326,#94375);
#94312=SHAPE_DEFINITION_REPRESENTATION(#94327,#94376);
#94313=SHAPE_DEFINITION_REPRESENTATION(#94328,#94377);
#94314=SHAPE_DEFINITION_REPRESENTATION(#94329,#94378);
#94315=SHAPE_DEFINITION_REPRESENTATION(#94330,#94379);
#94316=SHAPE_DEFINITION_REPRESENTATION(#94331,#94380);
#94317=SHAPE_DEFINITION_REPRESENTATION(#94332,#94381);
#94318=SHAPE_DEFINITION_REPRESENTATION(#94333,#94382);
#94319=SHAPE_DEFINITION_REPRESENTATION(#94334,#94383);
#94320=SHAPE_DEFINITION_REPRESENTATION(#94335,#94384);
#94321=PRODUCT_DEFINITION_SHAPE('',$,#94386);
#94322=PRODUCT_DEFINITION_SHAPE('',$,#94387);
#94323=PRODUCT_DEFINITION_SHAPE('',$,#94388);
#94324=PRODUCT_DEFINITION_SHAPE('',$,#94389);
#94325=PRODUCT_DEFINITION_SHAPE('',$,#94390);
#94326=PRODUCT_DEFINITION_SHAPE('',$,#94391);
#94327=PRODUCT_DEFINITION_SHAPE('',$,#94392);
#94328=PRODUCT_DEFINITION_SHAPE('',$,#94393);
#94329=PRODUCT_DEFINITION_SHAPE('',$,#94394);
#94330=PRODUCT_DEFINITION_SHAPE('',$,#94395);
#94331=PRODUCT_DEFINITION_SHAPE('',$,#94396);
#94332=PRODUCT_DEFINITION_SHAPE('',$,#94397);
#94333=PRODUCT_DEFINITION_SHAPE('',$,#94398);
#94334=PRODUCT_DEFINITION_SHAPE('',$,#94399);
#94335=PRODUCT_DEFINITION_SHAPE('',$,#94400);
#94336=PRODUCT_DEFINITION_SHAPE($,$,#113);
#94337=PRODUCT_DEFINITION_SHAPE($,$,#114);
#94338=PRODUCT_DEFINITION_SHAPE($,$,#115);
#94339=PRODUCT_DEFINITION_SHAPE($,$,#116);
#94340=PRODUCT_DEFINITION_SHAPE($,$,#117);
#94341=PRODUCT_DEFINITION_SHAPE($,$,#118);
#94342=PRODUCT_DEFINITION_SHAPE($,$,#119);
#94343=PRODUCT_DEFINITION_SHAPE($,$,#120);
#94344=PRODUCT_DEFINITION_SHAPE($,$,#121);
#94345=PRODUCT_DEFINITION_SHAPE($,$,#122);
#94346=PRODUCT_DEFINITION_SHAPE($,$,#123);
#94347=PRODUCT_DEFINITION_SHAPE($,$,#124);
#94348=PRODUCT_DEFINITION_SHAPE($,$,#125);
#94349=PRODUCT_DEFINITION_SHAPE($,$,#126);
#94350=PRODUCT_DEFINITION_SHAPE($,$,#127);
#94351=PRODUCT_DEFINITION_SHAPE($,$,#128);
#94352=PRODUCT_DEFINITION_SHAPE($,$,#129);
#94353=PRODUCT_DEFINITION_SHAPE($,$,#130);
#94354=PRODUCT_DEFINITION_SHAPE($,$,#131);
#94355=PRODUCT_DEFINITION_SHAPE($,$,#132);
#94356=PRODUCT_DEFINITION_SHAPE($,$,#133);
#94357=PRODUCT_DEFINITION_SHAPE($,$,#134);
#94358=PRODUCT_DEFINITION_SHAPE($,$,#135);
#94359=PRODUCT_DEFINITION_SHAPE($,$,#136);
#94360=PRODUCT_DEFINITION_SHAPE($,$,#137);
#94361=PRODUCT_DEFINITION_SHAPE($,$,#138);
#94362=PRODUCT_DEFINITION_SHAPE($,$,#139);
#94363=PRODUCT_DEFINITION_SHAPE($,$,#140);
#94364=PRODUCT_DEFINITION_SHAPE($,$,#141);
#94365=PRODUCT_DEFINITION_SHAPE($,$,#142);
#94366=PRODUCT_DEFINITION_SHAPE($,$,#143);
#94367=PRODUCT_DEFINITION_SHAPE($,$,#144);
#94368=PRODUCT_DEFINITION_SHAPE($,$,#145);
#94369=PRODUCT_DEFINITION_SHAPE($,$,#146);
#94370=SHAPE_REPRESENTATION('',(#51187,#55334,#55335,#55336,#55337,#55338,
#55339,#55340,#55341,#55342,#55343,#55344,#55345,#55346,#55347,#55348,#55349,
#55350,#55351,#55352,#55353,#55354,#55355,#55356,#55357,#55358,#55359,#55360,
#55361,#55362,#55363,#55364,#55365,#55366,#55367),#94286);
#94371=SHAPE_REPRESENTATION('',(#51188),#94287);
#94372=SHAPE_REPRESENTATION('',(#53608),#94288);
#94373=SHAPE_REPRESENTATION('',(#54142),#94289);
#94374=SHAPE_REPRESENTATION('',(#54216),#94290);
#94375=SHAPE_REPRESENTATION('',(#54474),#94291);
#94376=SHAPE_REPRESENTATION('',(#54491),#94292);
#94377=SHAPE_REPRESENTATION('',(#54812),#94293);
#94378=SHAPE_REPRESENTATION('',(#54829),#94294);
#94379=SHAPE_REPRESENTATION('',(#54858),#94295);
#94380=SHAPE_REPRESENTATION('',(#55178),#94296);
#94381=SHAPE_REPRESENTATION('',(#55192),#94297);
#94382=SHAPE_REPRESENTATION('',(#55271),#94298);
#94383=SHAPE_REPRESENTATION('',(#55288),#94299);
#94384=SHAPE_REPRESENTATION('',(#55314),#94300);
#94385=PRODUCT_DEFINITION_CONTEXT('part definition',#94432,'design');
#94386=PRODUCT_DEFINITION('2026-10-11-08-26-30-919','MAS-367',#94401,
#94385);
#94387=PRODUCT_DEFINITION('2026-10-11-08-26-31-288',
'01_Synchro_Sleeve_Torque-Lock_T10-15_WT297-15',#94402,#94385);
#94388=PRODUCT_DEFINITION('2026-10-11-08-26-33-125',
'02_Splined_Display_Hub_36T',#94403,#94385);
#94389=PRODUCT_DEFINITION('2026-10-11-08-26-34-261',
'03_Display_Pedestal',#94404,#94385);
#94390=PRODUCT_DEFINITION('2026-10-11-08-26-34-988',
'04_Base_Plate_180x130x16',#94405,#94385);
#94391=PRODUCT_DEFINITION('2026-10-11-08-26-38-347',
'05_Hub_Retainer_Plate_D56x6',#94406,#94385);
#94392=PRODUCT_DEFINITION('2026-10-11-08-26-38-736',
'06_ISO_4762_M10x25_SHCS',#94407,#94385);
#94393=PRODUCT_DEFINITION('2026-10-11-08-26-40-364',
'07_ISO_7089_Washer_10',#94408,#94385);
#94394=PRODUCT_DEFINITION('2026-10-11-08-26-40-818',
'08_DIN_127_B10_Spring_Washer',#94409,#94385);
#94395=PRODUCT_DEFINITION('2026-10-11-08-26-41-539',
'09_ISO_4762_M6x16_SHCS',#94410,#94385);
#94396=PRODUCT_DEFINITION('2026-10-11-08-26-44-599',
'10_ISO_8734_Dowel_6x20',#94411,#94385);
#94397=PRODUCT_DEFINITION('2026-10-11-08-26-45-510',
'11_ISO_4017_M8x30_Hex_Bolt',#94412,#94385);
#94398=PRODUCT_DEFINITION('2026-10-11-08-26-48-006',
'12_ISO_7089_Washer_8',#94413,#94385);
#94399=PRODUCT_DEFINITION('2026-10-11-08-26-49-607',
'13_DIN_127_B8_Spring_Washer',#94414,#94385);
#94400=PRODUCT_DEFINITION('2026-10-11-08-26-51-541',
'14_ISO_4032_M8_Hex_Nut',#94415,#94385);
#94401=PRODUCT_DEFINITION_FORMATION('',$,#94434);
#94402=PRODUCT_DEFINITION_FORMATION('',$,#94435);
#94403=PRODUCT_DEFINITION_FORMATION('',$,#94436);
#94404=PRODUCT_DEFINITION_FORMATION('',$,#94437);
#94405=PRODUCT_DEFINITION_FORMATION('',$,#94438);
#94406=PRODUCT_DEFINITION_FORMATION('',$,#94439);
#94407=PRODUCT_DEFINITION_FORMATION('',$,#94440);
#94408=PRODUCT_DEFINITION_FORMATION('',$,#94441);
#94409=PRODUCT_DEFINITION_FORMATION('',$,#94442);
#94410=PRODUCT_DEFINITION_FORMATION('',$,#94443);
#94411=PRODUCT_DEFINITION_FORMATION('',$,#94444);
#94412=PRODUCT_DEFINITION_FORMATION('',$,#94445);
#94413=PRODUCT_DEFINITION_FORMATION('',$,#94446);
#94414=PRODUCT_DEFINITION_FORMATION('',$,#94447);
#94415=PRODUCT_DEFINITION_FORMATION('',$,#94448);
#94416=PRODUCT_RELATED_PRODUCT_CATEGORY('MAS-367','MAS-367',(#94434));
#94417=PRODUCT_RELATED_PRODUCT_CATEGORY(
'01_Synchro_Sleeve_Torque-Lock_T10-15_WT297-15',
'01_Synchro_Sleeve_Torque-Lock_T10-15_WT297-15',(#94435));
#94418=PRODUCT_RELATED_PRODUCT_CATEGORY('02_Splined_Display_Hub_36T',
'02_Splined_Display_Hub_36T',(#94436));
#94419=PRODUCT_RELATED_PRODUCT_CATEGORY('03_Display_Pedestal',
'03_Display_Pedestal',(#94437));
#94420=PRODUCT_RELATED_PRODUCT_CATEGORY('04_Base_Plate_180x130x16',
'04_Base_Plate_180x130x16',(#94438));
#94421=PRODUCT_RELATED_PRODUCT_CATEGORY('05_Hub_Retainer_Plate_D56x6',
'05_Hub_Retainer_Plate_D56x6',(#94439));
#94422=PRODUCT_RELATED_PRODUCT_CATEGORY('06_ISO_4762_M10x25_SHCS',
'06_ISO_4762_M10x25_SHCS',(#94440));
#94423=PRODUCT_RELATED_PRODUCT_CATEGORY('07_ISO_7089_Washer_10',
'07_ISO_7089_Washer_10',(#94441));
#94424=PRODUCT_RELATED_PRODUCT_CATEGORY('08_DIN_127_B10_Spring_Washer',
'08_DIN_127_B10_Spring_Washer',(#94442));
#94425=PRODUCT_RELATED_PRODUCT_CATEGORY('09_ISO_4762_M6x16_SHCS',
'09_ISO_4762_M6x16_SHCS',(#94443));
#94426=PRODUCT_RELATED_PRODUCT_CATEGORY('10_ISO_8734_Dowel_6x20',
'10_ISO_8734_Dowel_6x20',(#94444));
#94427=PRODUCT_RELATED_PRODUCT_CATEGORY('11_ISO_4017_M8x30_Hex_Bolt',
'11_ISO_4017_M8x30_Hex_Bolt',(#94445));
#94428=PRODUCT_RELATED_PRODUCT_CATEGORY('12_ISO_7089_Washer_8',
'12_ISO_7089_Washer_8',(#94446));
#94429=PRODUCT_RELATED_PRODUCT_CATEGORY('13_DIN_127_B8_Spring_Washer',
'13_DIN_127_B8_Spring_Washer',(#94447));
#94430=PRODUCT_RELATED_PRODUCT_CATEGORY('14_ISO_4032_M8_Hex_Nut',
'14_ISO_4032_M8_Hex_Nut',(#94448));
#94431=APPLICATION_PROTOCOL_DEFINITION('international standard',
'automotive_design',2009,#94432);
#94432=APPLICATION_CONTEXT(
'Core Data for Automotive Mechanical Design Process');
#94433=PRODUCT_CONTEXT('part definition',#94432,'mechanical');
#94434=PRODUCT('2026-10-11-08-26-30-919','MAS-367',$,(#94433));
#94435=PRODUCT('2026-10-11-08-26-31-288',
'01_Synchro_Sleeve_Torque-Lock_T10-15_WT297-15',$,(#94433));
#94436=PRODUCT('2026-10-11-08-26-33-125','02_Splined_Display_Hub_36T',$,
(#94433));
#94437=PRODUCT('2026-10-11-08-26-34-261','03_Display_Pedestal',$,(#94433));
#94438=PRODUCT('2026-10-11-08-26-34-988','04_Base_Plate_180x130x16',$,(#94433));
#94439=PRODUCT('2026-10-11-08-26-38-347','05_Hub_Retainer_Plate_D56x6',
$,(#94433));
#94440=PRODUCT('2026-10-11-08-26-38-736','06_ISO_4762_M10x25_SHCS',$,(#94433));
#94441=PRODUCT('2026-10-11-08-26-40-364','07_ISO_7089_Washer_10',$,(#94433));
#94442=PRODUCT('2026-10-11-08-26-40-818','08_DIN_127_B10_Spring_Washer',
$,(#94433));
#94443=PRODUCT('2026-10-11-08-26-41-539','09_ISO_4762_M6x16_SHCS',$,(#94433));
#94444=PRODUCT('2026-10-11-08-26-44-599','10_ISO_8734_Dowel_6x20',$,(#94433));
#94445=PRODUCT('2026-10-11-08-26-45-510','11_ISO_4017_M8x30_Hex_Bolt',$,
(#94433));
#94446=PRODUCT('2026-10-11-08-26-48-006','12_ISO_7089_Washer_8',$,(#94433));
#94447=PRODUCT('2026-10-11-08-26-49-607','13_DIN_127_B8_Spring_Washer',
$,(#94433));
#94448=PRODUCT('2026-10-11-08-26-51-541','14_ISO_4032_M8_Hex_Nut',$,(#94433));
#94449=PRESENTATION_STYLE_ASSIGNMENT((#94464));
#94450=PRESENTATION_STYLE_ASSIGNMENT((#94465));
#94451=PRESENTATION_STYLE_ASSIGNMENT((#94466));
#94452=PRESENTATION_STYLE_ASSIGNMENT((#94467));
#94453=PRESENTATION_STYLE_ASSIGNMENT((#94468));
#94454=PRESENTATION_STYLE_ASSIGNMENT((#94469));
#94455=PRESENTATION_STYLE_ASSIGNMENT((#94470));
#94456=PRESENTATION_STYLE_ASSIGNMENT((#94471));
#94457=PRESENTATION_STYLE_ASSIGNMENT((#94472));
#94458=PRESENTATION_STYLE_ASSIGNMENT((#94473));
#94459=PRESENTATION_STYLE_ASSIGNMENT((#94474));
#94460=PRESENTATION_STYLE_ASSIGNMENT((#94475));
#94461=PRESENTATION_STYLE_ASSIGNMENT((#94476));
#94462=PRESENTATION_STYLE_ASSIGNMENT((#94477));
#94463=PRESENTATION_STYLE_ASSIGNMENT((#94478));
#94464=SURFACE_STYLE_USAGE(.BOTH.,#94479);
#94465=SURFACE_STYLE_USAGE(.BOTH.,#94480);
#94466=SURFACE_STYLE_USAGE(.BOTH.,#94481);
#94467=SURFACE_STYLE_USAGE(.BOTH.,#94482);
#94468=SURFACE_STYLE_USAGE(.BOTH.,#94483);
#94469=SURFACE_STYLE_USAGE(.BOTH.,#94484);
#94470=SURFACE_STYLE_USAGE(.BOTH.,#94485);
#94471=SURFACE_STYLE_USAGE(.BOTH.,#94486);
#94472=SURFACE_STYLE_USAGE(.BOTH.,#94487);
#94473=SURFACE_STYLE_USAGE(.BOTH.,#94488);
#94474=SURFACE_STYLE_USAGE(.BOTH.,#94489);
#94475=SURFACE_STYLE_USAGE(.BOTH.,#94490);
#94476=SURFACE_STYLE_USAGE(.BOTH.,#94491);
#94477=SURFACE_STYLE_USAGE(.BOTH.,#94492);
#94478=SURFACE_STYLE_USAGE(.BOTH.,#94493);
#94479=SURFACE_SIDE_STYLE('',(#94494));
#94480=SURFACE_SIDE_STYLE('',(#94495));
#94481=SURFACE_SIDE_STYLE('',(#94496));
#94482=SURFACE_SIDE_STYLE('',(#94497));
#94483=SURFACE_SIDE_STYLE('',(#94498));
#94484=SURFACE_SIDE_STYLE('',(#94499));
#94485=SURFACE_SIDE_STYLE('',(#94500));
#94486=SURFACE_SIDE_STYLE('',(#94501));
#94487=SURFACE_SIDE_STYLE('',(#94502));
#94488=SURFACE_SIDE_STYLE('',(#94503));
#94489=SURFACE_SIDE_STYLE('',(#94504));
#94490=SURFACE_SIDE_STYLE('',(#94505));
#94491=SURFACE_SIDE_STYLE('',(#94506));
#94492=SURFACE_SIDE_STYLE('',(#94507));
#94493=SURFACE_SIDE_STYLE('',(#94508));
#94494=SURFACE_STYLE_FILL_AREA(#94509);
#94495=SURFACE_STYLE_FILL_AREA(#94510);
#94496=SURFACE_STYLE_FILL_AREA(#94511);
#94497=SURFACE_STYLE_FILL_AREA(#94512);
#94498=SURFACE_STYLE_FILL_AREA(#94513);
#94499=SURFACE_STYLE_FILL_AREA(#94514);
#94500=SURFACE_STYLE_FILL_AREA(#94515);
#94501=SURFACE_STYLE_FILL_AREA(#94516);
#94502=SURFACE_STYLE_FILL_AREA(#94517);
#94503=SURFACE_STYLE_FILL_AREA(#94518);
#94504=SURFACE_STYLE_FILL_AREA(#94519);
#94505=SURFACE_STYLE_FILL_AREA(#94520);
#94506=SURFACE_STYLE_FILL_AREA(#94521);
#94507=SURFACE_STYLE_FILL_AREA(#94522);
#94508=SURFACE_STYLE_FILL_AREA(#94523);
#94509=FILL_AREA_STYLE('Steel - Satin',(#94524));
#94510=FILL_AREA_STYLE('MAS367_sleeve',(#94525));
#94511=FILL_AREA_STYLE('MAS367_hub',(#94526));
#94512=FILL_AREA_STYLE('MAS367_ped',(#94527));
#94513=FILL_AREA_STYLE('MAS367_base',(#94528));
#94514=FILL_AREA_STYLE('MAS367_ret',(#94529));
#94515=FILL_AREA_STYLE('MAS367_m10',(#94530));
#94516=FILL_AREA_STYLE('MAS367_w10',(#94531));
#94517=FILL_AREA_STYLE('MAS367_s10',(#94532));
#94518=FILL_AREA_STYLE('MAS367_m6',(#94533));
#94519=FILL_AREA_STYLE('MAS367_dow',(#94534));
#94520=FILL_AREA_STYLE('MAS367_bolt',(#94535));
#94521=FILL_AREA_STYLE('MAS367_w8',(#94536));
#94522=FILL_AREA_STYLE('MAS367_s8',(#94537));
#94523=FILL_AREA_STYLE('MAS367_nut',(#94538));
#94524=FILL_AREA_STYLE_COLOUR('Steel - Satin',#94539);
#94525=FILL_AREA_STYLE_COLOUR('MAS367_sleeve',#94540);
#94526=FILL_AREA_STYLE_COLOUR('MAS367_hub',#94541);
#94527=FILL_AREA_STYLE_COLOUR('MAS367_ped',#94542);
#94528=FILL_AREA_STYLE_COLOUR('MAS367_base',#94543);
#94529=FILL_AREA_STYLE_COLOUR('MAS367_ret',#94544);
#94530=FILL_AREA_STYLE_COLOUR('MAS367_m10',#94545);
#94531=FILL_AREA_STYLE_COLOUR('MAS367_w10',#94546);
#94532=FILL_AREA_STYLE_COLOUR('MAS367_s10',#94547);
#94533=FILL_AREA_STYLE_COLOUR('MAS367_m6',#94548);
#94534=FILL_AREA_STYLE_COLOUR('MAS367_dow',#94549);
#94535=FILL_AREA_STYLE_COLOUR('MAS367_bolt',#94550);
#94536=FILL_AREA_STYLE_COLOUR('MAS367_w8',#94551);
#94537=FILL_AREA_STYLE_COLOUR('MAS367_s8',#94552);
#94538=FILL_AREA_STYLE_COLOUR('MAS367_nut',#94553);
#94539=COLOUR_RGB('Steel - Satin',0.627450980392157,0.627450980392157,0.627450980392157);
#94540=COLOUR_RGB('MAS367_sleeve',0.470588235294118,0.462745098039216,0.431372549019608);
#94541=COLOUR_RGB('MAS367_hub',0.588235294117647,0.588235294117647,0.576470588235294);
#94542=COLOUR_RGB('MAS367_ped',0.8,0.807843137254902,0.823529411764706);
#94543=COLOUR_RGB('MAS367_base',0.588235294117647,0.6,0.619607843137255);
#94544=COLOUR_RGB('MAS367_ret',0.698039215686274,0.705882352941177,0.72156862745098);
#94545=COLOUR_RGB('MAS367_m10',0.784313725490196,0.792156862745098,0.807843137254902);
#94546=COLOUR_RGB('MAS367_w10',0.807843137254902,0.815686274509804,0.831372549019608);
#94547=COLOUR_RGB('MAS367_s10',0.768627450980392,0.776470588235294,0.792156862745098);
#94548=COLOUR_RGB('MAS367_m6',0.784313725490196,0.792156862745098,0.807843137254902);
#94549=COLOUR_RGB('MAS367_dow',0.83921568627451,0.847058823529412,0.862745098039216);
#94550=COLOUR_RGB('MAS367_bolt',0.792156862745098,0.8,0.811764705882353);
#94551=COLOUR_RGB('MAS367_w8',0.807843137254902,0.815686274509804,0.831372549019608);
#94552=COLOUR_RGB('MAS367_s8',0.768627450980392,0.776470588235294,0.792156862745098);
#94553=COLOUR_RGB('MAS367_nut',0.803921568627451,0.811764705882353,0.823529411764706);
#94554=COLOUR_RGB('Dark Blue',0.08,0.2,0.34);
#94555=FILL_AREA_STYLE_COLOUR('',#94554);
#94556=FILL_AREA_STYLE('',(#94555));
#94557=SURFACE_STYLE_FILL_AREA(#94556);
#94558=SURFACE_SIDE_STYLE('',(#94557));
#94559=SURFACE_STYLE_USAGE(.BOTH.,#94558);
#94560=PRESENTATION_STYLE_ASSIGNMENT((#94559));
#94561=COLOUR_RGB('Light Blue',0.38,0.62,0.78);
#94562=FILL_AREA_STYLE_COLOUR('',#94561);
#94563=FILL_AREA_STYLE('',(#94562));
#94564=SURFACE_STYLE_FILL_AREA(#94563);
#94565=SURFACE_SIDE_STYLE('',(#94564));
#94566=SURFACE_STYLE_USAGE(.BOTH.,#94565);
#94567=PRESENTATION_STYLE_ASSIGNMENT((#94566));
#94568=COLOUR_RGB('Sky Blue',0.24,0.69,0.87);
#94569=FILL_AREA_STYLE_COLOUR('',#94568);
#94570=FILL_AREA_STYLE('',(#94569));
#94571=SURFACE_STYLE_FILL_AREA(#94570);
#94572=SURFACE_SIDE_STYLE('',(#94571));
#94573=SURFACE_STYLE_USAGE(.BOTH.,#94572);
#94574=PRESENTATION_STYLE_ASSIGNMENT((#94573));
#94575=COLOUR_RGB('Grey',0.48,0.52,0.57);
#94576=FILL_AREA_STYLE_COLOUR('',#94575);
#94577=FILL_AREA_STYLE('',(#94576));
#94578=SURFACE_STYLE_FILL_AREA(#94577);
#94579=SURFACE_SIDE_STYLE('',(#94578));
#94580=SURFACE_STYLE_USAGE(.BOTH.,#94579);
#94581=PRESENTATION_STYLE_ASSIGNMENT((#94580));
#94582=COLOUR_RGB('Black',0.12,0.14,0.17);
#94583=FILL_AREA_STYLE_COLOUR('',#94582);
#94584=FILL_AREA_STYLE('',(#94583));
#94585=SURFACE_STYLE_FILL_AREA(#94584);
#94586=SURFACE_SIDE_STYLE('',(#94585));
#94587=SURFACE_STYLE_USAGE(.BOTH.,#94586);
#94588=PRESENTATION_STYLE_ASSIGNMENT((#94587));
#94589=COLOUR_RGB('Off White',0.89,0.88,0.83);
#94590=FILL_AREA_STYLE_COLOUR('',#94589);
#94591=FILL_AREA_STYLE('',(#94590));
#94592=SURFACE_STYLE_FILL_AREA(#94591);
#94593=SURFACE_SIDE_STYLE('',(#94592));
#94594=SURFACE_STYLE_USAGE(.BOTH.,#94593);
#94595=PRESENTATION_STYLE_ASSIGNMENT((#94594));
ENDSEC;
END-ISO-10303-21;
